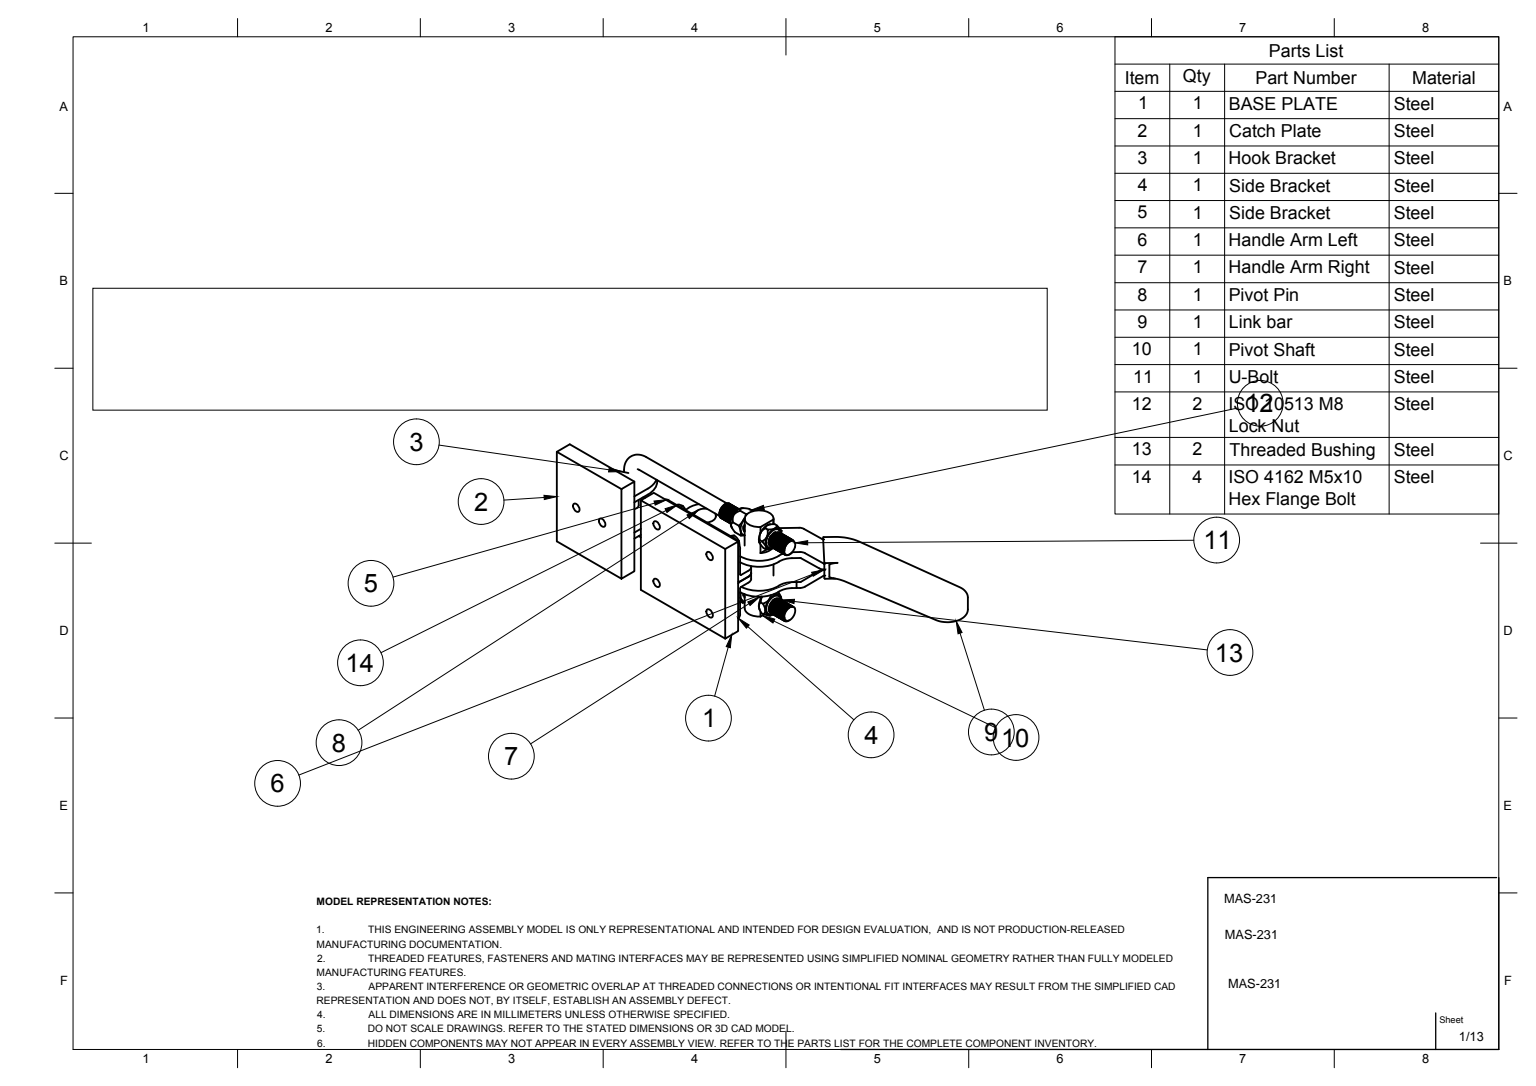
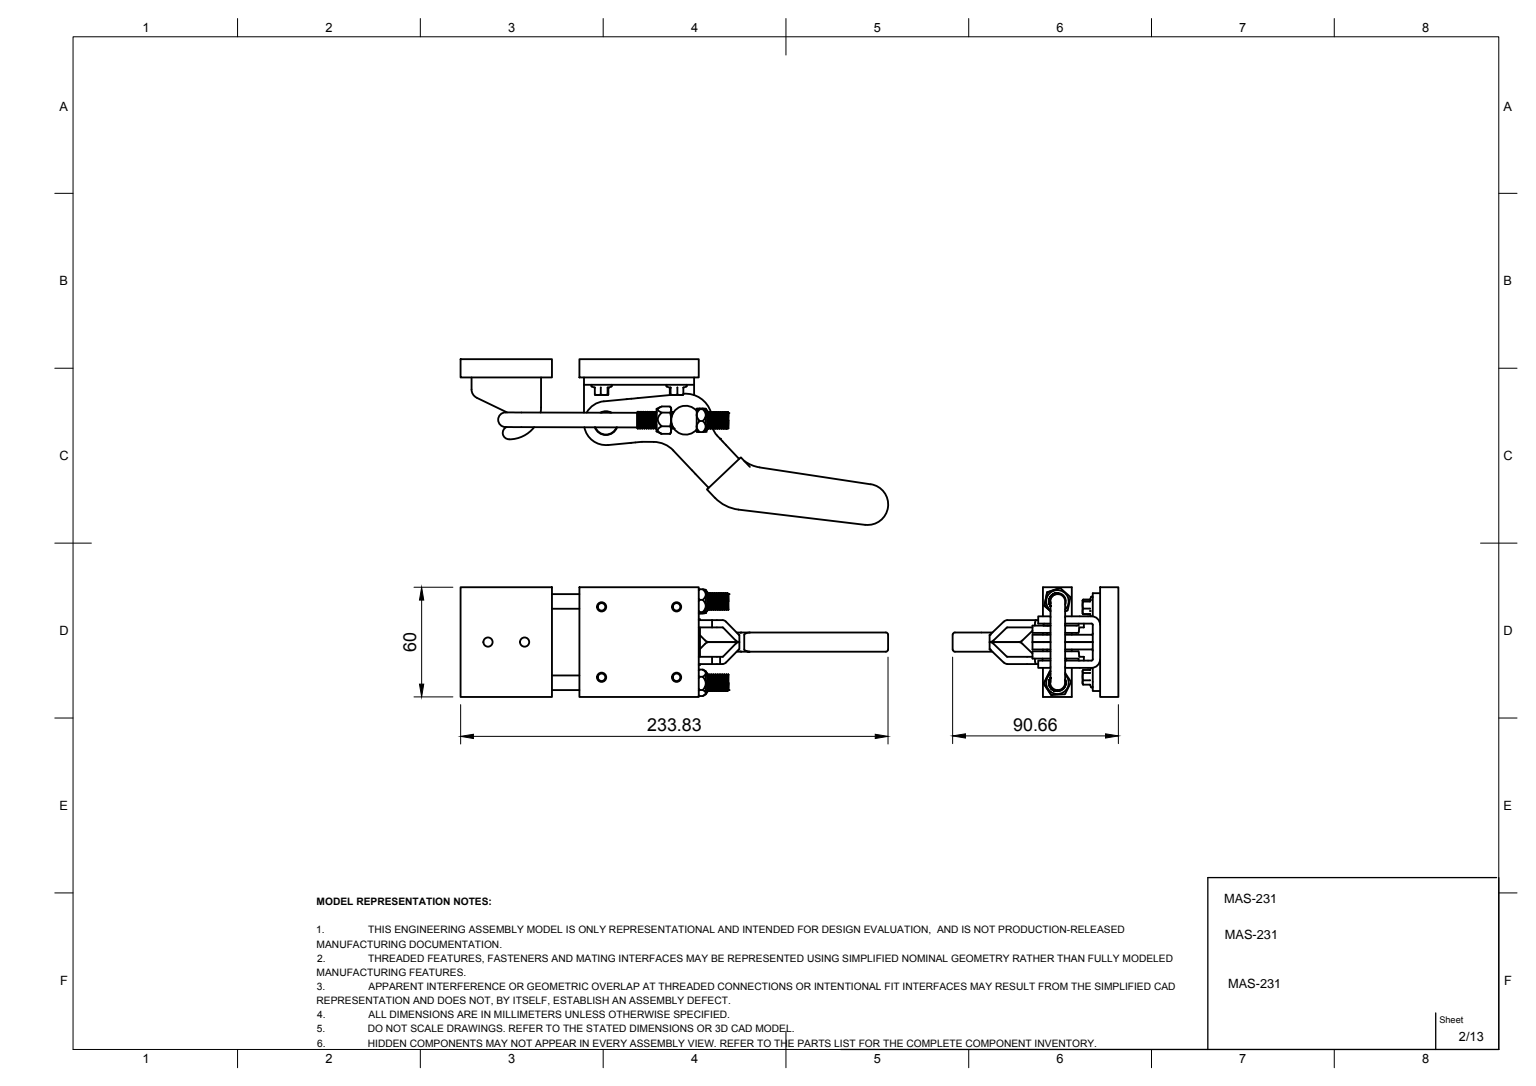
ISO-10303-21;
HEADER;
FILE_DESCRIPTION (('STEP AP214'),
    '1' );
FILE_NAME ( 'MAS-231', '2026-10-04T02:08:54', ( '' ), ( '' ), 'STEP AP214', 'Unspecified', '' );
FILE_SCHEMA (( 'AUTOMOTIVE_DESIGN' ));
ENDSEC;
DATA;
#1 = ORIENTED_EDGE ( 'NONE', *, *, #31259, .T. ) ;
#2 = VERTEX_POINT ( 'NONE', #9971 ) ;
#3 = CARTESIAN_POINT ( 'NONE',  ( -0.7646288533564489232, -0.1113553986120547346, 1.136811023622047223 ) ) ;
#4 = CARTESIAN_POINT ( 'NONE',  ( 0.07405724077823318263, -0.4114173227808823330, -0.1787899950787401604 ) ) ;
#5 = CARTESIAN_POINT ( 'NONE',  ( -1.094772975963752103E-17, -0.9552165353793071745, -0.1787899950787401882 ) ) ;
#6 = CONICAL_SURFACE ( 'NONE', #32970, 0.2471922904502826812, 0.5235987755982992597 ) ;
#7 = CARTESIAN_POINT ( 'NONE',  ( -0.2471922332845153669, -0.07944658092495102131, -0.07441910580874835923 ) ) ;
#8 = FACE_OUTER_BOUND ( 'NONE', #9994, .T. ) ;
#9 = CARTESIAN_POINT ( 'NONE',  ( 0.8019270111902717657, 0.1787899950787401604, 1.727362204670645385 ) ) ;
#10 = CARTESIAN_POINT ( 'NONE',  ( 0.7495606340400177148, 0.1264236179284866091, 0.3518700786863940833 ) ) ;
#11 = CARTESIAN_POINT ( 'NONE',  ( 0.7185039370078746268, -0.06523048226347956391, 0.3075787401574804347 ) ) ;
#12 = CARTESIAN_POINT ( 'NONE',  ( -0.07444174185955065859, -0.2446304237562738071, -0.1797182628040039087 ) ) ;
#13 = CARTESIAN_POINT ( 'NONE',  ( -1.094772975963752103E-17, -0.1049468028749080684, -0.1787899950787401882 ) ) ;
#14 = CARTESIAN_POINT ( 'NONE',  ( -1.094772975963752103E-17, -0.2465551180564728440, -0.1787899950787401882 ) ) ;
#15 = CARTESIAN_POINT ( 'NONE',  ( 0.1787899950787401604, -0.1013779527021420185, -0.07405724077823318263 ) ) ;
#16 = CARTESIAN_POINT ( 'NONE',  ( 0.2471913174570561644, -0.07307272215611475275, -0.08638584879597815958 ) ) ;
#17 = CARTESIAN_POINT ( 'NONE',  ( 0.8019270111902717657, -0.1787899950787401604, 0.6791338582139527791 ) ) ;
#18 = AXIS2_PLACEMENT_3D ( 'NONE', #45673, #23902, #16014 ) ;
#19 = DIRECTION ( 'NONE',  ( 0.000000000000000000, 0.000000000000000000, -1.000000000000000000 ) ) ;
#20 = DIRECTION ( 'NONE',  ( 0.000000000000000000, 0.000000000000000000, 1.000000000000000000 ) ) ;
#21 = CARTESIAN_POINT ( 'NONE',  ( 0.1264236179284866091, -0.4581692912848189247, 0.1264236179284866091 ) ) ;
#22 = EDGE_CURVE ( 'NONE', #36685, #42555, #8791, .T. ) ;
#23 = CARTESIAN_POINT ( 'NONE',  ( -0.8759842519685039353, 0.1574803149606299191, 1.309055118002708573 ) ) ;
#24 = CARTESIAN_POINT ( 'NONE',  ( 0.6971942568897637749, 2.189545951927499583E-17, 1.739665354276945131 ) ) ;
#26 = DIRECTION ( 'NONE',  ( 0.000000000000000000, 0.000000000000000000, -1.000000000000000000 ) ) ;
#25 = CARTESIAN_POINT ( 'NONE',  ( -0.1632645169450111788, -0.09126532511120305502, 0.1911722030494052427 ) ) ;
#27 = CARTESIAN_POINT ( 'NONE',  ( 0.8759842519685039353, 0.1787899950787401882, 0.5044291338045039375 ) ) ;
#28 = CARTESIAN_POINT ( 'NONE',  ( 0.000000000000000000, 0.09842519685039370636, 0.000000000000000000 ) ) ;
#29 = CARTESIAN_POINT ( 'NONE',  ( 0.1527640389977631963, -0.1337207259432456607, 0.04397945982240732826 ) ) ;
#31 = CARTESIAN_POINT ( 'NONE',  ( 0.1787899950787401604, -0.3425196849856064762, 0.07405724077823318263 ) ) ;
#30 = CARTESIAN_POINT ( 'NONE',  ( -0.06523048226347956391, -0.9306102361129453548, -0.1574803149606300301 ) ) ;
#33 = CARTESIAN_POINT ( 'NONE',  ( 0.1619907858920772714, 0.1553500912766716535, 0.01195870310704324514 ) ) ;
#32 = CARTESIAN_POINT ( 'NONE',  ( -0.8759842519685039353, 0.1787899950787401882, 0.4699803149068661479 ) ) ;
#34 = CARTESIAN_POINT ( 'NONE',  ( -0.07405724077823318263, -1.016732283410803905, 0.1787899950787401604 ) ) ;
#35 = FACE_OUTER_BOUND ( 'NONE', #16706, .T. ) ;
#36 = ADVANCED_FACE ( 'NONE', ( #44420 ), #33931, .T. ) ;
#37 = CARTESIAN_POINT ( 'NONE',  ( 0.1602931993194442739, 0.07955613945526338049, -0.1377952755905511861 ) ) ;
#38 = CARTESIAN_POINT ( 'NONE',  ( -0.8759842519685039353, -0.1787899950787401882, 1.587106299158834721 ) ) ;
#39 = VERTEX_POINT ( 'NONE', #1053 ) ;
#40 = CARTESIAN_POINT ( 'NONE',  ( -0.6971942568897648851, 0.07405724077823318263, 1.186023621993481658 ) ) ;
#41 = CYLINDRICAL_SURFACE ( 'NONE', #813, 0.1574803149606299191 ) ;
#42 = CARTESIAN_POINT ( 'NONE',  ( 0.6971942568897648851, -0.07405724077823297447, 1.112204724355684959 ) ) ;
#43 = CARTESIAN_POINT ( 'NONE',  ( 0.1574803149606299191, -1.139763779420031486, -1.928577636452523993E-17 ) ) ;
#44 = CARTESIAN_POINT ( 'NONE',  ( 0.6971942568897637749, 2.189545951927499583E-17, 1.813484251914740053 ) ) ;
#45 = CARTESIAN_POINT ( 'NONE',  ( -1.033464566929133799, 0.000000000000000000, 0.5610236220472440971 ) ) ;
#46 = CARTESIAN_POINT ( 'NONE',  ( -0.8019270111902717657, -0.1787899950787401604, 0.9940944881352130613 ) ) ;
#47 = EDGE_CURVE ( 'NONE', #46518, #3252, #13426, .T. ) ;
#48 = CARTESIAN_POINT ( 'NONE',  ( 0.1588779435336318824, 0.09971251034084034626, -0.1082054717952101869 ) ) ;
#49 = DIRECTION ( 'NONE',  ( 1.822029033848725028E-16, 0.000000000000000000, 1.000000000000000000 ) ) ;
#50 = CARTESIAN_POINT ( 'NONE',  ( 1.002407869896990045, 0.1264236179284866091, 0.3469488188438744070 ) ) ;
#51 = CARTESIAN_POINT ( 'NONE',  ( -0.6971942568897637749, 2.189545951927499583E-17, 0.2780511810485988278 ) ) ;
#52 = CARTESIAN_POINT ( 'NONE',  ( 0.7646288533564489232, -0.1113553986120547346, 1.678149606191684962 ) ) ;
#53 = ORIENTED_EDGE ( 'NONE', *, *, #45978, .F. ) ;
#54 = VECTOR ( 'NONE', #41568, 39.37007874015748143 ) ;
#55 = CARTESIAN_POINT ( 'NONE',  ( 0.1787899950787401604, 0.01181102367581077228, 0.07405724077823318263 ) ) ;
#56 = CARTESIAN_POINT ( 'NONE',  ( 0.7495606340400177148, 0.1264236179284866091, 0.7898622046706456068 ) ) ;
#57 = CARTESIAN_POINT ( 'NONE',  ( 0.8759842519685039353, -0.1787899950787401882, 1.040846456639149764 ) ) ;
#58 = CARTESIAN_POINT ( 'NONE',  ( -0.9500414927467377701, -0.1787899950787401604, 1.825787401521040243 ) ) ;
#59 = ORIENTED_EDGE ( 'NONE', *, *, #22403, .F. ) ;
#60 = VECTOR ( 'NONE', #5427, 39.37007874015748143 ) ;
#61 = AXIS2_PLACEMENT_3D ( 'NONE', #5298, #38366, #19916 ) ;
#62 = ( BOUNDED_CURVE ( )  B_SPLINE_CURVE ( 2, ( #7459, #22081, #47251, #3868, #22310, #18713, #36940, #14196, #13878 ),
 .UNSPECIFIED., .F., .F. ) 
 B_SPLINE_CURVE_WITH_KNOTS ( ( 3, 2, 2, 2, 3 ),
 ( 0.05000000000000000278, 0.05249999999999999806, 0.05500000000000000028, 0.05750000000000000250, 0.05999999999999999778 ),
 .UNSPECIFIED. ) 
 CURVE ( )  GEOMETRIC_REPRESENTATION_ITEM ( )  RATIONAL_B_SPLINE_CURVE ( ( 1.000000000000000000, 0.9238795325112869605, 1.000000000000000000, 0.9238795325112869605, 1.000000000000000000, 0.9238795325112869605, 1.000000000000000000, 0.9238795325112869605, 1.000000000000000000 ) ) 
 REPRESENTATION_ITEM ( '' )  ) ;
#63 = DIRECTION ( 'NONE',  ( 1.822029033848725028E-16, 0.000000000000000000, 1.000000000000000000 ) ) ;
#64 = CARTESIAN_POINT ( 'NONE',  ( 0.1264236179284866091, -1.340183023347348623, 0.1264236179284866091 ) ) ;
#65 = VERTEX_POINT ( 'NONE', #33456 ) ;
#66 = CARTESIAN_POINT ( 'NONE',  ( 0.1264236179284866091, -0.3006889763241893943, 0.1264236179284866091 ) ) ;
#67 = ORIENTED_EDGE ( 'NONE', *, *, #18348, .F. ) ;
#68 = CARTESIAN_POINT ( 'NONE',  ( 1.002407869896990045, 0.1264236179284866091, 1.208169291284818980 ) ) ;
#69 = LINE ( 'NONE', #40323, #2616 ) ;
#70 = EDGE_CURVE ( 'NONE', #32405, #30831, #8652, .T. ) ;
#71 = CARTESIAN_POINT ( 'NONE',  ( -0.7646288533564489232, 0.1113553986120547346, 0.9990157479239685223 ) ) ;
#72 = CARTESIAN_POINT ( 'NONE',  ( 0.8759842519685039353, 0.1787899950787401882, 1.488681102308440751 ) ) ;
#73 = CARTESIAN_POINT ( 'NONE',  ( 0.7646288533564489232, 0.1113553986120547346, 1.914370078740157632 ) ) ;
#74 = CARTESIAN_POINT ( 'NONE',  ( -0.1264236179284866091, -1.693405511757259951, 0.1264236179284866091 ) ) ;
#75 = CIRCLE ( 'NONE', #20007, 0.1787899950787401049 ) ;
#76 = CARTESIAN_POINT ( 'NONE',  ( -0.6971942568897637749, 2.189545951927499583E-17, 0.4404527558517480901 ) ) ;
#77 = CARTESIAN_POINT ( 'NONE',  ( -0.1540809957184832990, -0.09842519685039370636, 0.06850209239233011338 ) ) ;
#79 = CARTESIAN_POINT ( 'NONE',  ( -0.7240989362502219251, -0.07281704346119359517, 1.984672674023657102 ) ) ;
#78 = CARTESIAN_POINT ( 'NONE',  ( 0.1797182628040039087, -1.440496565488557978, 0.07444174185955046430 ) ) ;
#80 = DIRECTION ( 'NONE',  ( 0.000000000000000000, 0.000000000000000000, 1.000000000000000000 ) ) ;
#81 = CARTESIAN_POINT ( 'NONE',  ( 1.054774247047244540, 0.07405724077823318263, 1.249999999946235896 ) ) ;
#82 = CARTESIAN_POINT ( 'NONE',  ( 1.054774247047244540, -0.07405724077823318263, 1.712598425143087466 ) ) ;
#83 = AXIS2_PLACEMENT_3D ( 'NONE', #20865, #3610, #25184 ) ;
#84 = CARTESIAN_POINT ( 'NONE',  ( 0.7646288533564489232, 0.1113553986120547346, 1.510826771546015523 ) ) ;
#85 = CARTESIAN_POINT ( 'NONE',  ( 0.1574803149606300023, 0.3648440108500937140, -3.619166627704267558 ) ) ;
#86 = CIRCLE ( 'NONE', #1647, 0.09842519685039370636 ) ;
#87 = CARTESIAN_POINT ( 'NONE',  ( -0.1574803149606299191, 0.7443365962042343131, -3.964450923140766303 ) ) ;
#89 = CARTESIAN_POINT ( 'NONE',  ( 3.284318927891251994E-17, 0.1225393701325037388, 0.1787899950787401882 ) ) ;
#88 = CARTESIAN_POINT ( 'NONE',  ( -0.1574803149606297803, -0.7632874014672766938, 0.06523048226347956391 ) ) ;
#90 = CARTESIAN_POINT ( 'NONE',  ( 0.7646288533564489232, 0.1113553986120547346, 0.7627952754830236159 ) ) ;
#91 = CARTESIAN_POINT ( 'NONE',  ( 0.7013496418058506876, 0.02137559083948704225, 0.03937007727944009938 ) ) ;
#92 = EDGE_CURVE ( 'NONE', #27712, #6075, #1837, .T. ) ;
#94 = LINE ( 'NONE', #8474, #24641 ) ;
#93 = CARTESIAN_POINT ( 'NONE',  ( 0.8019270111902716547, -0.1787899950787401604, 1.269685039316314601 ) ) ;
#95 = DIRECTION ( 'NONE',  ( 1.000000000000000000, -0.000000000000000000, -1.144917494144692682E-16 ) ) ;
#96 = CARTESIAN_POINT ( 'NONE',  ( 0.3108999017613323090, 0.9251089822459528378, -1.060267534067256046 ) ) ;
#97 = CARTESIAN_POINT ( 'NONE',  ( 0.9412147342319837628, -0.1574803149606297803, 0.5831692912310553201 ) ) ;
#98 = ORIENTED_EDGE ( 'NONE', *, *, #40284, .T. ) ;
#99 = DIRECTION ( 'NONE',  ( 1.822029033848725028E-16, 0.000000000000000000, 1.000000000000000000 ) ) ;
#100 = CARTESIAN_POINT ( 'NONE',  ( 0.9656857656210602325, 0.1425117190157106917, 0.03937007042889534292 ) ) ;
#101 = CARTESIAN_POINT ( 'NONE',  ( -1.033464566929134687, -0.06523048226347956391, 0.3124999998924728462 ) ) ;
#102 = CARTESIAN_POINT ( 'NONE',  ( -0.7185039370078746268, -0.06523048226347956391, 0.4158464565853862704 ) ) ;
#103 = CARTESIAN_POINT ( 'NONE',  ( 0.005425426062181716927, 0.05318853600681028998, 0.1377950977353498141 ) ) ;
#104 = CARTESIAN_POINT ( 'NONE',  ( 0.9500414927467378812, -0.1787899950787401604, 1.432086614119464141 ) ) ;
#105 = CARTESIAN_POINT ( 'NONE',  ( -0.8107537697050253289, 0.1574803149606300301, 1.163877952755904666 ) ) ;
#106 = EDGE_CURVE ( 'NONE', #13083, #24265, #27060, .T. ) ;
#108 = CARTESIAN_POINT ( 'NONE',  ( 0.7185039370078739607, 1.928577636452523993E-17, 1.683070866141732402 ) ) ;
#107 = CARTESIAN_POINT ( 'NONE',  ( -1.033464566929133355, 0.06523048226348168721, 1.626476377952755570 ) ) ;
#109 = CARTESIAN_POINT ( 'NONE',  ( 0.1264236179284866091, -0.1038385826234017734, 0.1264236179284866091 ) ) ;
#110 = VERTEX_POINT ( 'NONE', #36790 ) ;
#111 = CARTESIAN_POINT ( 'NONE',  ( 0.7185039370078746268, -0.06523048226347956391, 0.6520669290263312323 ) ) ;
#112 = DIRECTION ( 'NONE',  ( 1.822029033848725028E-16, 0.000000000000000000, 1.000000000000000000 ) ) ;
#113 = CARTESIAN_POINT ( 'NONE',  ( -0.6195511811023656223, 0.6102362204724407491, 1.186023622047243986 ) ) ;
#114 = CARTESIAN_POINT ( 'NONE',  ( 0.6971942568897626646, 0.07405724077823318263, 0.5954724408911187261 ) ) ;
#115 = ORIENTED_EDGE ( 'NONE', *, *, #9426, .T. ) ;
#116 = CARTESIAN_POINT ( 'NONE',  ( -0.8019270111902716547, 0.1787899950787401604, 1.451771653489543290 ) ) ;
#117 = CARTESIAN_POINT ( 'NONE',  ( 0.1113553986120547346, 0.1250000001075269596, -0.1113553986120547346 ) ) ;
#118 = CARTESIAN_POINT ( 'NONE',  ( -1.002407869896990045, -0.1264236179284866091, 1.163877952702141672 ) ) ;
#119 = EDGE_LOOP ( 'NONE', ( #9384, #25327, #26730, #11644 ) ) ;
#120 = CARTESIAN_POINT ( 'NONE',  ( -0.2559055118110235560, -0.04581480775486102691, -0.03611822492271276469 ) ) ;
#121 = CARTESIAN_POINT ( 'NONE',  ( -0.8019270111902717657, 0.1787899950787401604, 0.8661417322297003674 ) ) ;
#122 = AXIS2_PLACEMENT_3D ( 'NONE', #43059, #39470, #7131 ) ;
#123 = CARTESIAN_POINT ( 'NONE',  ( 0.8107537697050254399, -0.1574803149606297803, 0.6668307086614162493 ) ) ;
#124 = DIRECTION ( 'NONE',  ( -1.000000000000000000, -6.679788269418529283E-17, 0.000000000000000000 ) ) ;
#125 = CARTESIAN_POINT ( 'NONE',  ( -0.1787899950787401604, -0.7668562516938051132, -0.07405724077823318263 ) ) ;
#126 = EDGE_LOOP ( 'NONE', ( #4193, #39037, #39203, #47364, #17831, #33692, #29299, #33986, #26594 ) ) ;
#127 = ORIENTED_EDGE ( 'NONE', *, *, #14895, .F. ) ;
#128 = VECTOR ( 'NONE', #18538, 39.37007874015748143 ) ;
#129 = CARTESIAN_POINT ( 'NONE',  ( 0.7185039370078739607, 1.928577636452523993E-17, 0.9645669290263307882 ) ) ;
#130 = ADVANCED_FACE ( 'NONE', ( #15231 ), #18799, .T. ) ;
#131 = CARTESIAN_POINT ( 'NONE',  ( -0.9500414927467378812, -0.1787899950787401604, 0.8021653542769460188 ) ) ;
#132 = FACE_OUTER_BOUND ( 'NONE', #21236, .T. ) ;
#133 = ORIENTED_EDGE ( 'NONE', *, *, #14771, .F. ) ;
#134 = CARTESIAN_POINT ( 'NONE',  ( -0.8019270111902716547, -0.1787899950787401604, 1.865157480261198097 ) ) ;
#135 = CARTESIAN_POINT ( 'NONE',  ( 0.07405724077823318263, -0.4901574802611972093, -0.1787899950787401604 ) ) ;
#136 = DIRECTION ( 'NONE',  ( -1.000000000000000000, 0.000000000000000000, 0.000000000000000000 ) ) ;
#137 = CARTESIAN_POINT ( 'NONE',  ( 0.7185039370078746268, -0.06523048226347956391, 0.6225393700787401619 ) ) ;
#138 = CARTESIAN_POINT ( 'NONE',  ( 3.301370929368692659E-17, -0.8573272741499744498, 0.1797182628040039365 ) ) ;
#139 = FACE_OUTER_BOUND ( 'NONE', #32124, .T. ) ;
#140 = CARTESIAN_POINT ( 'NONE',  ( -0.8759842519685039353, 0.1574803149606299191, 1.466535432963338437 ) ) ;
#141 = EDGE_CURVE ( 'NONE', #480, #43073, #20129, .T. ) ;
#142 = CARTESIAN_POINT ( 'NONE',  ( 0.9500414927467378812, -0.1787899950787401604, 0.7283464566391493200 ) ) ;
#143 = DIRECTION ( 'NONE',  ( -0.000000000000000000, -0.000000000000000000, 1.000000000000000000 ) ) ;
#144 = CARTESIAN_POINT ( 'NONE',  ( 0.9873396505805591694, -0.1113553986120547346, 1.343503937007874072 ) ) ;
#145 = DIRECTION ( 'NONE',  ( 0.000000000000000000, -0.6156614753256641759, -0.7880107536067173513 ) ) ;
#147 = FACE_OUTER_BOUND ( 'NONE', #21139, .T. ) ;
#146 = CARTESIAN_POINT ( 'NONE',  ( 0.9356431618536311667, -0.1660064224309732994, 1.989266148032244885 ) ) ;
#148 = DIRECTION ( 'NONE',  ( -1.000000000000000000, 0.000000000000000000, 0.000000000000000000 ) ) ;
#149 = CARTESIAN_POINT ( 'NONE',  ( 0.1113553986120547346, -0.6328740156405040507, 0.1113553986120547346 ) ) ;
#150 = ORIENTED_EDGE ( 'NONE', *, *, #2837, .F. ) ;
#151 = CIRCLE ( 'NONE', #10128, 0.1787899950787401049 ) ;
#152 = EDGE_CURVE ( 'NONE', #35410, #47206, #15470, .T. ) ;
#154 = DIRECTION ( 'NONE',  ( -1.000000000000000000, -1.802250327717385127E-14, 1.473544972410982106E-14 ) ) ;
#153 = CARTESIAN_POINT ( 'NONE',  ( 0.7495606340400177148, -0.1264236179284866091, 0.8341535432533228045 ) ) ;
#155 = CARTESIAN_POINT ( 'NONE',  ( 0.1787899950787401882, -0.7288385826234015097, -2.189545951927503898E-17 ) ) ;
#156 = DIRECTION ( 'NONE',  ( 0.000000000000000000, 0.6156614753256598460, 0.7880107536067207930 ) ) ;
#157 = VERTEX_POINT ( 'NONE', #7543 ) ;
#158 = CARTESIAN_POINT ( 'NONE',  ( -0.7646288533564489232, 0.1113553986120547346, 1.166338582677165281 ) ) ;
#159 = TOROIDAL_SURFACE ( 'NONE', #46862, 0.3814023619577306956, 0.009842519685039369942 ) ;
#160 = DIRECTION ( 'NONE',  ( 0.8191520442889949072, -0.4519843998600416302, 0.3531289150159167556 ) ) ;
#161 = CARTESIAN_POINT ( 'NONE',  ( 0.6971942568897637749, 2.189545951927499583E-17, 0.9867125983714331028 ) ) ;
#162 = EDGE_CURVE ( 'NONE', #28497, #15222, #36387, .T. ) ;
#163 = CARTESIAN_POINT ( 'NONE',  ( 0.000000000000000000, 0.000000000000000000, 1.181102362204724310 ) ) ;
#164 = CARTESIAN_POINT ( 'NONE',  ( 0.1113553986120547346, -1.617125984251968518, -0.1113553986120547346 ) ) ;
#165 = CARTESIAN_POINT ( 'NONE',  ( -0.8107537697050254399, -0.1574803149606297803, 0.5093503937007877180 ) ) ;
#166 = ORIENTED_EDGE ( 'NONE', *, *, #15392, .T. ) ;
#167 = FACE_BOUND ( 'NONE', #12224, .T. ) ;
#168 = CARTESIAN_POINT ( 'NONE',  ( -0.8019270111902717657, 0.1787899950787401604, 0.1131889763241894359 ) ) ;
#169 = ORIENTED_EDGE ( 'NONE', *, *, #21607, .F. ) ;
#170 = CARTESIAN_POINT ( 'NONE',  ( -0.9873396505805591694, -0.1113553986120547346, 0.7135826771653542844 ) ) ;
#171 = CARTESIAN_POINT ( 'NONE',  ( 0.07405724077823318263, -1.435039370024976391, -0.1787899950787401604 ) ) ;
#172 = CARTESIAN_POINT ( 'NONE',  ( -0.9873396505805591694, -0.1113553986120547346, 1.855314960629921295 ) ) ;
#173 = CARTESIAN_POINT ( 'NONE',  ( -1.002407869896990045, -0.1264236179284866091, 1.631397637741511808 ) ) ;
#174 = CARTESIAN_POINT ( 'NONE',  ( -1.033464566929133799, 0.000000000000000000, 0.1181102361129454797 ) ) ;
#175 = CARTESIAN_POINT ( 'NONE',  ( 0.1619971594100712287, 0.06735705997075436269, 0.1405166210180776309 ) ) ;
#176 = CARTESIAN_POINT ( 'NONE',  ( 0.9500414927467378812, 0.1787899950787401604, 0.02952755900135462311 ) ) ;
#177 = CYLINDRICAL_SURFACE ( 'NONE', #43516, 0.1574803149606299191 ) ;
#178 = CARTESIAN_POINT ( 'NONE',  ( -1.094772975963752103E-17, -0.3411672753158531690, -0.1787899950787401882 ) ) ;
#179 = CARTESIAN_POINT ( 'NONE',  ( 0.8759842519685039353, 0.000000000000000000, 4.498031496062992574 ) ) ;
#180 = DIRECTION ( 'NONE',  ( 1.822029033848725028E-16, 0.000000000000000000, 1.000000000000000000 ) ) ;
#181 = CARTESIAN_POINT ( 'NONE',  ( -0.9500414927467378812, 0.1787899950787401604, 0.3051181101824569919 ) ) ;
#182 = CIRCLE ( 'NONE', #27018, 0.1574803149606299191 ) ;
#183 = VERTEX_POINT ( 'NONE', #42256 ) ;
#184 = ORIENTED_EDGE ( 'NONE', *, *, #3239, .T. ) ;
#185 = CARTESIAN_POINT ( 'NONE',  ( -0.8019270111902716547, -0.1787899950787401604, 1.313976377898992132 ) ) ;
#186 = ORIENTED_EDGE ( 'NONE', *, *, #26981, .F. ) ;
#187 = ( GEOMETRIC_REPRESENTATION_CONTEXT ( 3 ) GLOBAL_UNCERTAINTY_ASSIGNED_CONTEXT ( ( #19281 ) ) GLOBAL_UNIT_ASSIGNED_CONTEXT ( ( #14903, #26165, #18708 ) ) REPRESENTATION_CONTEXT ( 'NONE', 'WORKASPACE' ) ) ;
#188 = VECTOR ( 'NONE', #38666, 39.37007874015748143 ) ;
#189 = ADVANCED_FACE ( 'NONE', ( #38682 ), #13369, .T. ) ;
#190 = CARTESIAN_POINT ( 'NONE',  ( -0.1787899950787401604, -1.262795275536788386, 0.07405724077823318263 ) ) ;
#191 = CARTESIAN_POINT ( 'NONE',  ( 0.1264236179284866091, -1.403051181048598384, 0.1264236179284866091 ) ) ;
#192 = CARTESIAN_POINT ( 'NONE',  ( 0.000000000000000000, 0.000000000000000000, 0.000000000000000000 ) ) ;
#193 = ADVANCED_FACE ( 'NONE', ( #1523 ), #30571, .F. ) ;
#194 = CARTESIAN_POINT ( 'NONE',  ( 0.8759842519685039353, 0.1574803149606299191, 0.3346456692913385988 ) ) ;
#195 = CARTESIAN_POINT ( 'NONE',  ( -1.181102362204724310, 0.000000000000000000, 0.9842519685039370358 ) ) ;
#196 = CARTESIAN_POINT ( 'NONE',  ( -0.8107537697050253289, -0.1574803149606297803, 1.011318897530268712 ) ) ;
#197 = VECTOR ( 'NONE', #24397, 39.37007874015748143 ) ;
#198 = ADVANCED_FACE ( 'NONE', ( #20458 ), #16639, .T. ) ;
#199 = CARTESIAN_POINT ( 'NONE',  ( 0.6971942568897637749, 2.189545951927499583E-17, 0.4010826771115905687 ) ) ;
#200 = CARTESIAN_POINT ( 'NONE',  ( 0.1113553986120547346, -0.3277559055118110520, 0.1113553986120547346 ) ) ;
#201 = CARTESIAN_POINT ( 'NONE',  ( 0.7185039370078746268, 0.06523048226347956391, 1.906988188868851797 ) ) ;
#202 = EDGE_LOOP ( 'NONE', ( #15956, #3484, #38224, #16323 ) ) ;
#203 = DIRECTION ( 'NONE',  ( 0.000000000000000000, 0.000000000000000000, -1.000000000000000000 ) ) ;
#204 = CARTESIAN_POINT ( 'NONE',  ( 0.7185039370078746268, -0.06523048226347956391, 0.9374999999999991118 ) ) ;
#205 = CARTESIAN_POINT ( 'NONE',  ( -1.033464566929133799, 0.000000000000000000, 0.6692913384751496553 ) ) ;
#206 = CARTESIAN_POINT ( 'NONE',  ( -0.1113553986120547346, -0.4950787400499527813, -0.1113553986120547346 ) ) ;
#208 = CARTESIAN_POINT ( 'NONE',  ( 0.7185039370078746268, -0.06523048226347956391, 0.7406496062992133922 ) ) ;
#207 = CARTESIAN_POINT ( 'NONE',  ( 0.8759842519685039353, 0.000000000000000000, 4.498031496062992574 ) ) ;
#209 = CARTESIAN_POINT ( 'NONE',  ( -0.7185039370078739607, 1.928577636452523993E-17, 0.7677165353255432922 ) ) ;
#210 = EDGE_LOOP ( 'NONE', ( #1234, #31218, #6999, #28687 ) ) ;
#211 = CARTESIAN_POINT ( 'NONE',  ( -0.1574803149606297803, 0.1028543308161884995, 0.06523048226347956391 ) ) ;
#212 = CARTESIAN_POINT ( 'NONE',  ( 0.4330708661417322913, 0.08090551181102362266, 0.000000000000000000 ) ) ;
#213 = CARTESIAN_POINT ( 'NONE',  ( 0.07405724077823318263, -1.508858267662772867, -0.1787899950787401604 ) ) ;
#214 = CARTESIAN_POINT ( 'NONE',  ( -0.1574803149606297803, -1.511318897530268712, 0.06523048226347956391 ) ) ;
#215 = CARTESIAN_POINT ( 'NONE',  ( 0.1264236179284866091, -0.7780511810485984947, 0.1264236179284866091 ) ) ;
#216 = CARTESIAN_POINT ( 'NONE',  ( -0.06523048226347956391, -1.097933070866141225, -0.1574803149606300301 ) ) ;
#217 = CARTESIAN_POINT ( 'NONE',  ( 1.033464566929134687, -0.06523048226347956391, 0.9424212597349932441 ) ) ;
#218 = CARTESIAN_POINT ( 'NONE',  ( 0.7185039370078746268, 0.06523048226347956391, 0.5388779527559055538 ) ) ;
#219 = VECTOR ( 'NONE', #41742, 39.37007874015748143 ) ;
#220 = EDGE_CURVE ( 'NONE', #8537, #45765, #3616, .T. ) ;
#221 = ORIENTED_EDGE ( 'NONE', *, *, #44499, .F. ) ;
#222 = ORIENTED_EDGE ( 'NONE', *, *, #18590, .F. ) ;
#223 = EDGE_LOOP ( 'NONE', ( #32593, #34812, #29678, #45510 ) ) ;
#224 = CARTESIAN_POINT ( 'NONE',  ( -1.054774247047244096, 0.000000000000000000, 1.562499999946236118 ) ) ;
#225 = CARTESIAN_POINT ( 'NONE',  ( 0.6971942568897648851, 0.07405724077823318263, 1.697834645615527771 ) ) ;
#226 = CARTESIAN_POINT ( 'NONE',  ( 0.1574803149606300301, -1.339074803042078932, 0.06523048226347956391 ) ) ;
#227 = CARTESIAN_POINT ( 'NONE',  ( -0.9500414927467378812, -0.1787899950787401604, 0.7283464566391493200 ) ) ;
#228 = AXIS2_PLACEMENT_3D ( 'NONE', #14600, #36183, #18649 ) ;
#230 = FACE_OUTER_BOUND ( 'NONE', #13816, .T. ) ;
#229 = AXIS2_PLACEMENT_3D ( 'NONE', #33997, #1125, #15784 ) ;
#231 = CARTESIAN_POINT ( 'NONE',  ( 1.054774247047244096, 0.000000000000000000, 0.3420275590013546751 ) ) ;
#232 = CARTESIAN_POINT ( 'NONE',  ( 0.3161444924769701292, 2.177585298233984279, -3.731703755406948986 ) ) ;
#233 = CARTESIAN_POINT ( 'NONE',  ( -0.6971942568897648851, 0.07405724077823318263, 1.220472440891118504 ) ) ;
#234 = CARTESIAN_POINT ( 'NONE',  ( -0.7495606340400177148, -0.1264236179284866091, 0.6373031495525354195 ) ) ;
#235 = DIRECTION ( 'NONE',  ( 1.000000000000000000, 0.000000000000000000, -1.822029033848725275E-16 ) ) ;
#236 = ( BOUNDED_CURVE ( )  B_SPLINE_CURVE ( 2, ( #18764, #29842, #25754, #33895, #32949, #1015, #4363, #41246, #25970 ),
 .UNSPECIFIED., .F., .T. ) 
 B_SPLINE_CURVE_WITH_KNOTS ( ( 3, 2, 2, 2, 3 ),
 ( 0.4000000000000000222, 0.4025000000000000244, 0.4050000000000000266, 0.4074999999999999734, 0.4099999999999999756 ),
 .UNSPECIFIED. ) 
 CURVE ( )  GEOMETRIC_REPRESENTATION_ITEM ( )  RATIONAL_B_SPLINE_CURVE ( ( 1.000000000000000000, 0.9238795325112869605, 1.000000000000000000, 0.9238795325112869605, 1.000000000000000000, 0.9238795325112869605, 1.000000000000000000, 0.9238795325112849621, 1.000000000000000000 ) ) 
 REPRESENTATION_ITEM ( '' )  ) ;
#237 = AXIS2_PLACEMENT_3D ( 'NONE', #26256, #7319, #29176 ) ;
#238 = DIRECTION ( 'NONE',  ( -1.000000000000000000, 0.000000000000000000, 0.000000000000000000 ) ) ;
#239 = CARTESIAN_POINT ( 'NONE',  ( -0.8759842519685039353, 0.1787899950787401882, 1.572342519631275692 ) ) ;
#240 = CARTESIAN_POINT ( 'NONE',  ( -0.7185039370078739607, 1.928577636452523993E-17, 1.948818897530267602 ) ) ;
#241 = ORIENTED_EDGE ( 'NONE', *, *, #39973, .T. ) ;
#243 = ( BOUNDED_CURVE ( )  B_SPLINE_CURVE ( 2, ( #38368, #35271, #35028, #17505, #31910, #27861, #39299, #28309, #42180 ),
 .UNSPECIFIED., .F., .F. ) 
 B_SPLINE_CURVE_WITH_KNOTS ( ( 3, 2, 2, 2, 3 ),
 ( 0.4500000000000000111, 0.4525000000000000133, 0.4550000000000000155, 0.4575000000000000178, 0.4600000000000000200 ),
 .UNSPECIFIED. ) 
 CURVE ( )  GEOMETRIC_REPRESENTATION_ITEM ( )  RATIONAL_B_SPLINE_CURVE ( ( 1.000000000000000000, 0.9238795325112869605, 1.000000000000000000, 0.9238795325112869605, 1.000000000000000000, 0.9238795325112869605, 1.000000000000000000, 0.9238795325112869605, 1.000000000000000000 ) ) 
 REPRESENTATION_ITEM ( '' )  ) ;
#242 = CARTESIAN_POINT ( 'NONE',  ( -0.9412147342319837628, -0.1574803149606297803, 1.656003937007873406 ) ) ;
#244 = DIRECTION ( 'NONE',  ( 0.000000000000000000, 0.000000000000000000, 1.000000000000000000 ) ) ;
#245 = CARTESIAN_POINT ( 'NONE',  ( 0.8019270111902716547, -0.1787899950787401604, 1.471456692859622217 ) ) ;
#246 = CARTESIAN_POINT ( 'NONE',  ( 0.2698848154395015464, -3.032960542342102697E-32, 0.09842519685039370636 ) ) ;
#247 = ORIENTED_EDGE ( 'NONE', *, *, #10180, .F. ) ;
#248 = CARTESIAN_POINT ( 'NONE',  ( -0.3161444924769509779, 1.495705267341512767, -0.3569552279982057819 ) ) ;
#249 = ORIENTED_EDGE ( 'NONE', *, *, #21041, .T. ) ;
#250 = ORIENTED_EDGE ( 'NONE', *, *, #34224, .F. ) ;
#251 = EDGE_CURVE ( 'NONE', #13767, #23712, #510, .T. ) ;
#252 = CARTESIAN_POINT ( 'NONE',  ( -0.4338976377952755703, 0.1574803149606299191, 1.928577636452523993E-17 ) ) ;
#253 = CARTESIAN_POINT ( 'NONE',  ( -0.1787899950787401604, -0.4360236219934807145, 0.07405724077823318263 ) ) ;
#254 = EDGE_CURVE ( 'NONE', #18975, #21109, #11079, .T. ) ;
#255 = CARTESIAN_POINT ( 'NONE',  ( 0.1787899950787401604, -0.8494094487651332459, 0.07405724077823318263 ) ) ;
#256 = CARTESIAN_POINT ( 'NONE',  ( 0.7185039370078739607, 0.000000000000000000, 4.498031496062992574 ) ) ;
#257 = CARTESIAN_POINT ( 'NONE',  ( 0.7495606340400177148, 0.1264236179284866091, 1.729822834591905556 ) ) ;
#258 = CARTESIAN_POINT ( 'NONE',  ( -0.1797182628040039087, -0.2003390851735964984, -0.07444174185955065859 ) ) ;
#259 = EDGE_CURVE ( 'NONE', #25443, #30394, #12521, .T. ) ;
#260 = VECTOR ( 'NONE', #32837, 39.37007874015748143 ) ;
#261 = CARTESIAN_POINT ( 'NONE',  ( 0.1787899950787401604, -0.1172499524812071620, 0.07405724077823318263 ) ) ;
#262 = CARTESIAN_POINT ( 'NONE',  ( -0.1264236179284866091, -0.1186023621509608300, 0.1264236179284866091 ) ) ;
#263 = CARTESIAN_POINT ( 'NONE',  ( 0.2471920270787851259, -0.07566776403336712697, -0.08167830084036972749 ) ) ;
#264 = EDGE_CURVE ( 'NONE', #24192, #11278, #27216, .T. ) ;
#265 = CARTESIAN_POINT ( 'NONE',  ( 1.054774247047244540, -0.07405724077823318263, 0.7283464566391493200 ) ) ;
#266 = CARTESIAN_POINT ( 'NONE',  ( 0.1673228346456693549, 0.05639690512153990726, -0.1570009270184611616 ) ) ;
#267 = VECTOR ( 'NONE', #18707, 39.37007874015748143 ) ;
#268 = CARTESIAN_POINT ( 'NONE',  ( -0.1787899950787401604, -0.4311023621509605386, 0.07405724077823318263 ) ) ;
#269 = LINE ( 'NONE', #3642, #3920 ) ;
#270 = CARTESIAN_POINT ( 'NONE',  ( 0.8019270111902717657, -0.1787899950787401604, 1.786417322780882388 ) ) ;
#271 = CYLINDRICAL_SURFACE ( 'NONE', #38342, 0.1574803149606299191 ) ;
#272 = CARTESIAN_POINT ( 'NONE',  ( 0.6971942568897637749, 2.189545951927499583E-17, 0.5142716534895434011 ) ) ;
#273 = ORIENTED_EDGE ( 'NONE', *, *, #35074, .F. ) ;
#274 = CARTESIAN_POINT ( 'NONE',  ( 1.033464566929134687, -0.06523048226347956391, 0.08612204724409450174 ) ) ;
#276 = CARTESIAN_POINT ( 'NONE',  ( 0.1264236179284866091, -0.2170275590013547307, -0.1264236179284866091 ) ) ;
#275 = CARTESIAN_POINT ( 'NONE',  ( 0.1574803149606299191, -0.9429133857192442125, -1.928577636452523993E-17 ) ) ;
#278 = CARTESIAN_POINT ( 'NONE',  ( 0.1571385178022428053, 0.1097099440836636214, 0.09077329659527381966 ) ) ;
#277 = CARTESIAN_POINT ( 'NONE',  ( -0.8759842519685039353, -0.1787899950787401882, 0.4502952755367874427 ) ) ;
#279 = CARTESIAN_POINT ( 'NONE',  ( 0.1787899950787401604, -1.041338582623402287, -0.07405724077823318263 ) ) ;
#280 = CARTESIAN_POINT ( 'NONE',  ( 0.6971942568897626646, -0.07405724077823297447, 0.2460629920722207375 ) ) ;
#281 = CARTESIAN_POINT ( 'NONE',  ( 0.1640397255812384159, 0.08076041531236369253, -0.1398787134456308257 ) ) ;
#282 = CARTESIAN_POINT ( 'NONE',  ( -0.6971942568897648851, 0.07405724077823318263, 1.535433070812378675 ) ) ;
#283 = ORIENTED_EDGE ( 'NONE', *, *, #46313, .T. ) ;
#284 = CARTESIAN_POINT ( 'NONE',  ( -0.8759842519685039353, 0.1787899950787401882, 1.218011810969858111 ) ) ;
#285 = CARTESIAN_POINT ( 'NONE',  ( -0.8107537697050254399, 0.1574803149606300301, 0.3371062992125987146 ) ) ;
#286 = CARTESIAN_POINT ( 'NONE',  ( 0.9500414927467378812, 0.1787899950787401604, 1.254921259788757348 ) ) ;
#287 = CARTESIAN_POINT ( 'NONE',  ( -0.06523048226347956391, -1.206200787294047228, -0.1574803149606300301 ) ) ;
#288 = CARTESIAN_POINT ( 'NONE',  ( 1.054774247047244096, 0.000000000000000000, 1.951279527505291433 ) ) ;
#289 = CARTESIAN_POINT ( 'NONE',  ( -0.8759842519685039353, 0.1574803149606299191, 0.6496062992125984925 ) ) ;
#290 = CARTESIAN_POINT ( 'NONE',  ( -0.6971942568897648851, -0.07405724077823297447, 1.028543307032851795 ) ) ;
#291 = CARTESIAN_POINT ( 'NONE',  ( -0.7185039370078739607, 1.928577636452523993E-17, 1.604330708661417360 ) ) ;
#292 = CARTESIAN_POINT ( 'NONE',  ( -0.1706040688522822979, -0.1969959271856973060, -0.03730110279448183019 ) ) ;
#293 = CARTESIAN_POINT ( 'NONE',  ( 0.8759842519685039353, -0.1787899950787401882, 0.3715551180564728440 ) ) ;
#294 = CARTESIAN_POINT ( 'NONE',  ( -1.002407869896990045, -0.1264236179284866091, 0.1747047243556852092 ) ) ;
#295 = CARTESIAN_POINT ( 'NONE',  ( 0.7185039370078746268, 0.06523048226347956391, 1.670767716427906002 ) ) ;
#296 = ORIENTED_EDGE ( 'NONE', *, *, #20298, .F. ) ;
#297 = CARTESIAN_POINT ( 'NONE',  ( -0.1787899950787401604, 0.03149606304588949135, -0.07405724077823318263 ) ) ;
#298 = ORIENTED_EDGE ( 'NONE', *, *, #27985, .F. ) ;
#299 = CARTESIAN_POINT ( 'NONE',  ( 1.002407869896990045, 0.1264236179284866091, 0.8981299212060788184 ) ) ;
#300 = CARTESIAN_POINT ( 'NONE',  ( 0.9500414927467377701, -0.1787899950787401604, 1.082677165300567346 ) ) ;
#301 = CARTESIAN_POINT ( 'NONE',  ( -0.8759842519685039353, -0.1787899950787401882, 1.823326771599779406 ) ) ;
#302 = AXIS2_PLACEMENT_3D ( 'NONE', #11967, #8576, #23214 ) ;
#303 = EDGE_LOOP ( 'NONE', ( #910, #27362, #9795, #24309 ) ) ;
#304 = CARTESIAN_POINT ( 'NONE',  ( 1.054774247047244540, 0.07405724077823318263, 1.953740157426552715 ) ) ;
#305 = CARTESIAN_POINT ( 'NONE',  ( 0.1574803149606299191, 0.5360961046428496246, -0.7563373642699310340 ) ) ;
#306 = CARTESIAN_POINT ( 'NONE',  ( 0.1787899950787401604, -1.258982235945774075, 0.07405724077823318263 ) ) ;
#307 = AXIS2_PLACEMENT_3D ( 'NONE', #8881, #45755, #23738 ) ;
#308 = ORIENTED_EDGE ( 'NONE', *, *, #11008, .T. ) ;
#309 = CARTESIAN_POINT ( 'NONE',  ( -0.07405724077823318263, -0.2047244093950554844, -0.1787899950787401604 ) ) ;
#310 = DIRECTION ( 'NONE',  ( 0.000000000000000000, 0.000000000000000000, 1.000000000000000000 ) ) ;
#311 = ORIENTED_EDGE ( 'NONE', *, *, #11167, .T. ) ;
#312 = CARTESIAN_POINT ( 'NONE',  ( 0.8019270111902717657, 0.1787899950787401604, 1.136811023568283119 ) ) ;
#313 = CARTESIAN_POINT ( 'NONE',  ( 0.000000000000000000, -0.09842519685039370636, 0.000000000000000000 ) ) ;
#314 = CARTESIAN_POINT ( 'NONE',  ( -0.8759842519685039353, 0.1574803149606299191, 0.9940944880814488460 ) ) ;
#315 = EDGE_CURVE ( 'NONE', #5716, #5360, #10980, .T. ) ;
#316 = CARTESIAN_POINT ( 'NONE',  ( 0.9500414927467378812, 0.1787899950787401604, 0.1870078739619845387 ) ) ;
#317 = CARTESIAN_POINT ( 'NONE',  ( -0.1787899950787401604, -1.656496062938362268, 0.07405724077823318263 ) ) ;
#318 = CARTESIAN_POINT ( 'NONE',  ( 0.1787899950787401604, -1.715551181048599716, 0.07405724077823318263 ) ) ;
#319 = APPLICATION_PROTOCOL_DEFINITION ( 'draft international standard', 'automotive_design', 1998, #20485 ) ;
#320 = APPLICATION_CONTEXT ( 'automotive_design' ) ;
#321 = EDGE_CURVE ( 'NONE', #8150, #39441, #13683, .T. ) ;
#322 = CARTESIAN_POINT ( 'NONE',  ( -0.8759842519685039353, -0.1787899950787401882, 0.5290354330171024300 ) ) ;
#323 = DIRECTION ( 'NONE',  ( -2.602085213965207486E-14, -0.6156614753256566264, -0.7880107536067233465 ) ) ;
#324 = CARTESIAN_POINT ( 'NONE',  ( 3.301370929368692659E-17, -1.369138297772021673, 0.1797182628040039365 ) ) ;
#325 = CARTESIAN_POINT ( 'NONE',  ( 1.033464566929134687, 0.06523048226347956391, 1.429625984251967852 ) ) ;
#326 = AXIS2_PLACEMENT_3D ( 'NONE', #47306, #10657, #25265 ) ;
#327 = CARTESIAN_POINT ( 'NONE',  ( 1.002407869896990045, 0.1264236179284866091, 1.409940944828126153 ) ) ;
#328 = CARTESIAN_POINT ( 'NONE',  ( 0.6971942568897648851, 0.07405724077823318263, 1.732283464513166615 ) ) ;
#329 = B_SPLINE_CURVE_WITH_KNOTS ( 'NONE', 3,
 ( #40653, #8085, #22708, #37314, #20055, #46161, #9758, #34449, #45674, #2308, #13357, #45919, #24148, #16938, #24370, #42328, #41837, #20757 ),
 .UNSPECIFIED., .F., .F.,
 ( 4, 2, 2, 2, 1, 1, 2, 2, 2, 4 ),
 ( 0.000000000000000000, 0.2499999999999993894, 0.3749999999999990008, 0.4374999999999987788, 0.4687499999999986122, 0.4843749999999986122, 0.4921874999999985567, 0.4999999999999985567, 0.7499999999999992228, 1.000000000000000000 ),
 .UNSPECIFIED. ) ;
#330 = AXIS2_PLACEMENT_3D ( 'NONE', #15898, #1005, #37686 ) ;
#331 = CIRCLE ( 'NONE', #19461, 0.1870078740157480324 ) ;
#332 = CARTESIAN_POINT ( 'NONE',  ( 0.7185039370078714072, 0.06523048226347728795, 1.513287401467276583 ) ) ;
#333 = DIRECTION ( 'NONE',  ( 1.000000000000000000, 2.891205793294678326E-16, 0.000000000000000000 ) ) ;
#334 = CARTESIAN_POINT ( 'NONE',  ( 0.7185039370078746268, -0.06523048226347956391, 0.8095472439869610959 ) ) ;
#336 = CARTESIAN_POINT ( 'NONE',  ( 0.5358894627757212481, 4.766607801171850497E-17, 0.000000000000000000 ) ) ;
#335 = CARTESIAN_POINT ( 'NONE',  ( 0.1113553986120547346, -0.8198818896562519720, -0.1113553986120547346 ) ) ;
#337 = CARTESIAN_POINT ( 'NONE',  ( 0.7185039370078739607, 1.928577636452523993E-17, 0.7677165353255432922 ) ) ;
#339 = DIRECTION ( 'NONE',  ( 0.000000000000000000, 1.000000000000000000, 0.000000000000000000 ) ) ;
#338 = CARTESIAN_POINT ( 'NONE',  ( 1.002407869896990045, 0.1264236179284866091, 1.286909448765133801 ) ) ;
#340 = DIRECTION ( 'NONE',  ( 1.000000000000000000, 0.000000000000000000, 0.000000000000000000 ) ) ;
#341 = CARTESIAN_POINT ( 'NONE',  ( 0.7185039370078739607, 0.000000000000000000, 4.498031496062992574 ) ) ;
#342 = CARTESIAN_POINT ( 'NONE',  ( -0.7495606340400177148, -0.1264236179284866091, 1.267224409395055096 ) ) ;
#343 = CARTESIAN_POINT ( 'NONE',  ( 0.7646288533564489232, -0.1113553986120547346, 0.6545275589475906264 ) ) ;
#344 = ORIENTED_EDGE ( 'NONE', *, *, #39545, .F. ) ;
#345 = CARTESIAN_POINT ( 'NONE',  ( -0.7185039370078739607, 1.928577636452523993E-17, 1.761811023622047223 ) ) ;
#346 = CARTESIAN_POINT ( 'NONE',  ( -0.1992661408232795639, -0.3637244504922588773, -1.027838479691305595 ) ) ;
#347 = EDGE_LOOP ( 'NONE', ( #1174, #678, #18238, #19385 ) ) ;
#348 = CARTESIAN_POINT ( 'NONE',  ( 0.9412147342319837628, -0.1574803149606297803, 0.2780511811023620439 ) ) ;
#349 = CARTESIAN_POINT ( 'NONE',  ( -0.1270800023317771588, 0.1515309935665608287, -0.1270800023317771588 ) ) ;
#350 = CARTESIAN_POINT ( 'NONE',  ( 0.1574803149606300301, -1.063484251860977059, 0.06523048226347956391 ) ) ;
#351 = DIRECTION ( 'NONE',  ( 0.000000000000000000, -0.6220299971367094782, 0.7829934116339071215 ) ) ;
#352 = CARTESIAN_POINT ( 'NONE',  ( 0.9500414927467378812, 0.1787899950787401604, 1.643700787347811998 ) ) ;
#354 = CARTESIAN_POINT ( 'NONE',  ( -0.7185039370078732945, -0.06523048226347920309, 0.1107283464566930498 ) ) ;
#353 = CARTESIAN_POINT ( 'NONE',  ( -0.8759842519685039353, 0.1574803149606299191, 0.9251968503937008093 ) ) ;
#355 = CARTESIAN_POINT ( 'NONE',  ( 0.7646288533564489232, -0.1113553986120547346, 1.176181102362204633 ) ) ;
#356 = CARTESIAN_POINT ( 'NONE',  ( 0.07405724077823318263, -0.2244094487651340231, 0.1787899950787401604 ) ) ;
#357 = ORIENTED_EDGE ( 'NONE', *, *, #35134, .F. ) ;
#358 = ( BOUNDED_CURVE ( )  B_SPLINE_CURVE ( 2, ( #11263, #3350, #25876, #28789, #17960, #43354, #17490, #32615, #32121 ),
 .UNSPECIFIED., .F., .T. ) 
 B_SPLINE_CURVE_WITH_KNOTS ( ( 3, 2, 2, 2, 3 ),
 ( 0.2300000000000000100, 0.2325000000000000122, 0.2349999999999999867, 0.2374999999999999889, 0.2399999999999999911 ),
 .UNSPECIFIED. ) 
 CURVE ( )  GEOMETRIC_REPRESENTATION_ITEM ( )  RATIONAL_B_SPLINE_CURVE ( ( 1.000000000000000000, 0.9238795325112869605, 1.000000000000000000, 0.9238795325112869605, 1.000000000000000000, 0.9238795325112869605, 1.000000000000000000, 0.9238795325112869605, 1.000000000000000000 ) ) 
 REPRESENTATION_ITEM ( '' )  ) ;
#359 = DIRECTION ( 'NONE',  ( 1.822029033848725028E-16, 0.000000000000000000, 1.000000000000000000 ) ) ;
#360 = CARTESIAN_POINT ( 'NONE',  ( -0.009745153983727199848, -0.04193537623276894638, 0.2798067035903421540 ) ) ;
#361 = CARTESIAN_POINT ( 'NONE',  ( 1.054774247047244540, -0.07405724077823318263, 0.6545275590013545086 ) ) ;
#362 = ORIENTED_EDGE ( 'NONE', *, *, #11409, .F. ) ;
#363 = CARTESIAN_POINT ( 'NONE',  ( 0.8759842519685039353, 0.1787899950787401882, 0.8243110235682834519 ) ) ;
#364 = CARTESIAN_POINT ( 'NONE',  ( -9.642888182262618425E-18, 0.09055118120988918384, -0.1574803149606299191 ) ) ;
#365 = CARTESIAN_POINT ( 'NONE',  ( -0.8759842519685039353, -0.1787899950787401882, 1.277066929080094448 ) ) ;
#366 = CARTESIAN_POINT ( 'NONE',  ( -0.7495606340400177148, 0.1264236179284866091, 0.1599409448281264023 ) ) ;
#367 = LINE ( 'NONE', #8269, #13455 ) ;
#368 = VECTOR ( 'NONE', #12553, 39.37007874015748143 ) ;
#369 = CARTESIAN_POINT ( 'NONE',  ( 0.1787899950787401882, -0.9021908973630964335, -2.189545951927503898E-17 ) ) ;
#370 = VERTEX_POINT ( 'NONE', #31969 ) ;
#371 = DIRECTION ( 'NONE',  ( 0.000000000000000000, 0.000000000000000000, 1.000000000000000000 ) ) ;
#372 = AXIS2_PLACEMENT_3D ( 'NONE', #5692, #17413, #32052 ) ;
#373 = ORIENTED_EDGE ( 'NONE', *, *, #26554, .F. ) ;
#374 = CARTESIAN_POINT ( 'NONE',  ( 1.054774247047244096, 0.000000000000000000, 1.006397637741511808 ) ) ;
#375 = CARTESIAN_POINT ( 'NONE',  ( 0.003837171311379782533, -0.04331820873536343375, 0.1377949924024825246 ) ) ;
#376 = ( BOUNDED_CURVE ( )  B_SPLINE_CURVE ( 2, ( #44031, #36857, #22706, #4461, #11233, #44728, #15066, #25618, #15540 ),
 .UNSPECIFIED., .F., .T. ) 
 B_SPLINE_CURVE_WITH_KNOTS ( ( 3, 2, 2, 2, 3 ),
 ( 0.07000000000000000666, 0.07249999999999999500, 0.07499999999999999722, 0.07749999999999999944, 0.08000000000000000167 ),
 .UNSPECIFIED. ) 
 CURVE ( )  GEOMETRIC_REPRESENTATION_ITEM ( )  RATIONAL_B_SPLINE_CURVE ( ( 1.000000000000000000, 0.9238795325112859613, 1.000000000000000000, 0.9238795325112869605, 1.000000000000000000, 0.9238795325112869605, 1.000000000000000000, 0.9238795325112869605, 1.000000000000000000 ) ) 
 REPRESENTATION_ITEM ( '' )  ) ;
#377 = CARTESIAN_POINT ( 'NONE',  ( -1.054774247047244540, -0.07405724077823318263, 0.7283464566391493200 ) ) ;
#378 = EDGE_CURVE ( 'NONE', #9213, #13081, #13737, .T. ) ;
#379 = CARTESIAN_POINT ( 'NONE',  ( -0.1787899950787401604, -0.4753937007336378473, 0.07405724077823318263 ) ) ;
#380 = EDGE_CURVE ( 'NONE', #22666, #46167, #21394, .T. ) ;
#381 = CARTESIAN_POINT ( 'NONE',  ( -1.002407869896990045, 0.1264236179284866091, 0.07135826766277185429 ) ) ;
#382 = CARTESIAN_POINT ( 'NONE',  ( -0.8759842519685039353, 0.1574803149606299191, 0.9251968503937008093 ) ) ;
#383 = CARTESIAN_POINT ( 'NONE',  ( -0.1270800023317771588, -1.059098927693281622, 0.1270800023317771588 ) ) ;
#384 = CARTESIAN_POINT ( 'NONE',  ( 0.6195511811023588500, -5.463695987328330208E-16, -1.186023622047243986 ) ) ;
#385 = CARTESIAN_POINT ( 'NONE',  ( -0.7185039370078739607, 1.928577636452523993E-17, 1.594488188868850242 ) ) ;
#386 = CARTESIAN_POINT ( 'NONE',  ( 0.8019270111902717657, -0.1787899950787401604, 0.7234251967966300878 ) ) ;
#387 = CARTESIAN_POINT ( 'NONE',  ( 0.7495606340400177148, -0.1264236179284866091, 1.345964566875370139 ) ) ;
#388 = B_SPLINE_CURVE_WITH_KNOTS ( 'NONE', 3,
 ( #34639, #1791, #24318, #31755 ),
 .UNSPECIFIED., .F., .F.,
 ( 4, 4 ),
 ( 0.000000000000000000, 1.000000000000000000 ),
 .UNSPECIFIED. ) ;
#389 = CARTESIAN_POINT ( 'NONE',  ( -0.1673228346456692994, -0.4812165006432425063, -0.8611016091043821596 ) ) ;
#391 = FACE_OUTER_BOUND ( 'NONE', #347, .T. ) ;
#390 = CARTESIAN_POINT ( 'NONE',  ( 0.7125413026092556334, -0.03488858553940781676, 1.983914878791770864 ) ) ;
#392 = CARTESIAN_POINT ( 'NONE',  ( -0.1235961452251413406, -0.09842519685039370636, 0.2140748031496062798 ) ) ;
#394 = CARTESIAN_POINT ( 'NONE',  ( 0.1637325577037128943, 0.07820587237429499350, 0.1401340067785760701 ) ) ;
#393 = CARTESIAN_POINT ( 'NONE',  ( 1.054774247047244096, 0.000000000000000000, 0.8095472440407244230 ) ) ;
#395 = AXIS2_PLACEMENT_3D ( 'NONE', #5918, #35170, #24842 ) ;
#396 = CARTESIAN_POINT ( 'NONE',  ( -0.1787899950787401604, -0.8248031495525351975, 0.07405724077823318263 ) ) ;
#397 = CARTESIAN_POINT ( 'NONE',  ( -0.5555748031496061667, 0.1864803149606364951, -0.7480314960629921295 ) ) ;
#398 = VERTEX_POINT ( 'NONE', #6064 ) ;
#399 = FACE_OUTER_BOUND ( 'NONE', #15103, .T. ) ;
#400 = CONICAL_SURFACE ( 'NONE', #29553, 0.09842519685039310962, 0.7853981633972314524 ) ;
#401 = DIRECTION ( 'NONE',  ( 1.822029033848725028E-16, 0.000000000000000000, 1.000000000000000000 ) ) ;
#402 = CARTESIAN_POINT ( 'NONE',  ( 0.8019270111902717657, 0.1787899950787401604, 0.9399606298674970661 ) ) ;
#403 = DIRECTION ( 'NONE',  ( 1.000000000000000000, 0.000000000000000000, -1.822029033848725275E-16 ) ) ;
#404 = CARTESIAN_POINT ( 'NONE',  ( -0.06523048226347956391, -1.727854330708660902, -0.1574803149606300301 ) ) ;
#405 = EDGE_CURVE ( 'NONE', #45750, #40086, #43961, .T. ) ;
#406 = DIRECTION ( 'NONE',  ( 0.000000000000000000, -0.2126700594527834443, 0.9771240687918547607 ) ) ;
#407 = ORIENTED_EDGE ( 'NONE', *, *, #24032, .F. ) ;
#408 = DIRECTION ( 'NONE',  ( -1.000000000000000000, 0.000000000000000000, 0.000000000000000000 ) ) ;
#409 = CARTESIAN_POINT ( 'NONE',  ( -0.8019270111902717657, 0.1787899950787401604, 0.2706692912848194243 ) ) ;
#410 = CARTESIAN_POINT ( 'NONE',  ( 0.9873396505805591694, 0.1113553986120547346, 0.3297244094488189226 ) ) ;
#411 = CARTESIAN_POINT ( 'NONE',  ( -0.7495606340400177148, 0.1264236179284866091, 1.611712598371433103 ) ) ;
#412 = CARTESIAN_POINT ( 'NONE',  ( -0.6971942568897648851, 0.07405724077823318263, 0.9055118109698584439 ) ) ;
#413 = CARTESIAN_POINT ( 'NONE',  ( -0.9500414927467378812, -0.1787899950787401604, 0.3346456692375748831 ) ) ;
#414 = CARTESIAN_POINT ( 'NONE',  ( -0.4330708661417322913, 0.1574803149606299191, 1.186023622047243986 ) ) ;
#415 = FACE_OUTER_BOUND ( 'NONE', #12654, .T. ) ;
#416 = CARTESIAN_POINT ( 'NONE',  ( 0.6971942568897626646, 0.07405724077823318263, 0.03937007868639404856 ) ) ;
#417 = DIRECTION ( 'NONE',  ( -1.000000000000000000, 0.000000000000000000, 0.000000000000000000 ) ) ;
#418 = CARTESIAN_POINT ( 'NONE',  ( 0.07405724077823318263, -0.3436279052371127296, -0.1787899950787401604 ) ) ;
#419 = CARTESIAN_POINT ( 'NONE',  ( 0.08603670706143877467, -0.09842519685039370636, 0.1221131442762555253 ) ) ;
#420 = CARTESIAN_POINT ( 'NONE',  ( -0.8107537697050254399, 0.1574803149606300301, 1.902066929026330566 ) ) ;
#421 = PLANE ( 'NONE',  #8031 ) ;
#422 = VECTOR ( 'NONE', #8785, 39.37007874015748143 ) ;
#423 = CARTESIAN_POINT ( 'NONE',  ( -0.8019270111902717657, 0.1787899950787401604, 0.3100393700249766682 ) ) ;
#424 = EDGE_CURVE ( 'NONE', #18854, #1825, #37750, .T. ) ;
#425 = CARTESIAN_POINT ( 'NONE',  ( -1.054774247047244540, -0.07405724077823318263, 1.323818897584032594 ) ) ;
#426 = VERTEX_POINT ( 'NONE', #25002 ) ;
#427 = AXIS2_PLACEMENT_3D ( 'NONE', #21003, #3022, #14070 ) ;
#428 = AXIS2_PLACEMENT_3D ( 'NONE', #42726, #2726, #24548 ) ;
#429 = EDGE_CURVE ( 'NONE', #8074, #10105, #18584, .T. ) ;
#430 = CARTESIAN_POINT ( 'NONE',  ( 0.1787899950787401882, -1.284940944828125930, -2.189545951927503898E-17 ) ) ;
#431 = CARTESIAN_POINT ( 'NONE',  ( 0.1264236179284866091, -1.481791338528913426, 0.1264236179284866091 ) ) ;
#432 = FILL_AREA_STYLE_COLOUR ( '', #44690 ) ;
#433 = DIRECTION ( 'NONE',  ( 0.000000000000000000, 0.000000000000000000, 1.000000000000000000 ) ) ;
#434 = CARTESIAN_POINT ( 'NONE',  ( 0.9412147342319837628, -0.1574803149606297803, 0.3567913385826772532 ) ) ;
#435 = LINE ( 'NONE', #44275, #37021 ) ;
#436 = CARTESIAN_POINT ( 'NONE',  ( -0.7646288533564489232, -0.1113553986120547346, 1.048228346349165507 ) ) ;
#437 = CARTESIAN_POINT ( 'NONE',  ( 0.7495606340400177148, -0.1264236179284866091, 0.4453740156942677664 ) ) ;
#438 = CARTESIAN_POINT ( 'NONE',  ( -0.1113553986120547346, -0.2194881889763779514, 0.1113553986120547346 ) ) ;
#439 = DIRECTION ( 'NONE',  ( 0.000000000000000000, 0.000000000000000000, -1.000000000000000000 ) ) ;
#440 = ORIENTED_EDGE ( 'NONE', *, *, #40777, .T. ) ;
#441 = CARTESIAN_POINT ( 'NONE',  ( -0.1787899950787401604, -0.2047244093950554844, -0.07405724077823318263 ) ) ;
#442 = DIRECTION ( 'NONE',  ( 0.000000000000000000, -0.6156614753256597350, -0.7880107536067206819 ) ) ;
#443 = CARTESIAN_POINT ( 'NONE',  ( 0.8759842519685039353, 0.1574803149606299191, 0.9645669291338583307 ) ) ;
#444 = CARTESIAN_POINT ( 'NONE',  ( 1.033464566929133799, 0.000000000000000000, 1.348425196850393748 ) ) ;
#445 = LINE ( 'NONE', #14857, #29310 ) ;
#446 = CARTESIAN_POINT ( 'NONE',  ( 0.01230737760510395781, 0.07955613945526338049, -0.1377952755905511861 ) ) ;
#447 = CARTESIAN_POINT ( 'NONE',  ( 0.1645760670519675339, 0.08210188079435769282, -0.1405695449895551230 ) ) ;
#448 = CARTESIAN_POINT ( 'NONE',  ( -0.3100393700787401619, -2.714815113292586694E-26, 1.043307086614172707 ) ) ;
#449 = CIRCLE ( 'NONE', #39490, 0.02900000000000001882 ) ;
#450 = ORIENTED_EDGE ( 'NONE', *, *, #1798, .T. ) ;
#451 = CARTESIAN_POINT ( 'NONE',  ( 0.000000000000000000, 0.000000000000000000, -0.1574803149606298636 ) ) ;
#452 = DIRECTION ( 'NONE',  ( 0.000000000000000000, -1.000000000000000000, 0.000000000000000000 ) ) ;
#453 = CARTESIAN_POINT ( 'NONE',  ( -0.1264236179284866091, -1.531003936954110189, 0.1264236179284866091 ) ) ;
#454 = CARTESIAN_POINT ( 'NONE',  ( 0.07405724077823318263, -0.8198818897100156322, 0.1787899950787401604 ) ) ;
#455 = CARTESIAN_POINT ( 'NONE',  ( -0.06523048226347956391, -1.240649606299213614, 0.1574803149606297803 ) ) ;
#456 = CARTESIAN_POINT ( 'NONE',  ( 0.7646288533564489232, -0.1113553986120547346, 0.9301181101286929431 ) ) ;
#457 = CARTESIAN_POINT ( 'NONE',  ( 0.2759478392031653460, -0.09842519685039370636, 2.185526306663015728 ) ) ;
#458 = UNCERTAINTY_MEASURE_WITH_UNIT (LENGTH_MEASURE( 1.000000000000000082E-05 ), #21946, 'distance_accuracy_value', 'NONE') ;
#459 = ORIENTED_EDGE ( 'NONE', *, *, #45696, .T. ) ;
#460 = VERTEX_POINT ( 'NONE', #6542 ) ;
#461 = VERTEX_POINT ( 'NONE', #43426 ) ;
#462 = CARTESIAN_POINT ( 'NONE',  ( -1.002407869896990045, -0.1264236179284866091, 1.557578740103716441 ) ) ;
#463 = CARTESIAN_POINT ( 'NONE',  ( 1.054774247047244540, -0.07405724077823318263, 1.638779527505292988 ) ) ;
#464 = CARTESIAN_POINT ( 'NONE',  ( -1.002407869896990045, -0.1264236179284866091, 0.8095472440407244230 ) ) ;
#465 = DIRECTION ( 'NONE',  ( 0.000000000000000000, -1.000000000000000000, -0.000000000000000000 ) ) ;
#466 = CARTESIAN_POINT ( 'NONE',  ( 0.8759842519685039353, 0.1787899950787401882, 0.2731299212060791515 ) ) ;
#467 = CARTESIAN_POINT ( 'NONE',  ( -0.07874015748031489015, -0.5708661417322835607, 0.9783464566929127582 ) ) ;
#468 = CARTESIAN_POINT ( 'NONE',  ( -0.7495606340400177148, 0.1264236179284866091, 1.296751968450173154 ) ) ;
#469 = DIRECTION ( 'NONE',  ( 1.822029033848725028E-16, 0.000000000000000000, 1.000000000000000000 ) ) ;
#470 = CARTESIAN_POINT ( 'NONE',  ( 0.3604359965418638123, 4.466152701071653354E-17, 0.000000000000000000 ) ) ;
#471 = CARTESIAN_POINT ( 'NONE',  ( -0.7495606340400177148, -0.1264236179284866091, 1.626476377898992132 ) ) ;
#472 = CARTESIAN_POINT ( 'NONE',  ( -0.9873396505805591694, -0.1113553986120547346, 1.884842519577511810 ) ) ;
#473 = ORIENTED_EDGE ( 'NONE', *, *, #10794, .F. ) ;
#474 = CARTESIAN_POINT ( 'NONE',  ( -1.033464566929133799, 0.000000000000000000, 1.663385826771653697 ) ) ;
#475 = DIRECTION ( 'NONE',  ( 0.5735764363510417185, 0.6455006197386566891, -0.5043203561029927506 ) ) ;
#476 = EDGE_CURVE ( 'NONE', #44070, #30751, #10635, .T. ) ;
#477 = CARTESIAN_POINT ( 'NONE',  ( 0.7495606340400177148, -0.1264236179284866091, 1.468996062938362046 ) ) ;
#478 = CARTESIAN_POINT ( 'NONE',  ( -0.2009290272083082973, -0.09842519685039370636, 0.1224581209280712624 ) ) ;
#479 = CARTESIAN_POINT ( 'NONE',  ( 1.033464566929133799, 1.928577636452524610E-17, 4.498031496062992574 ) ) ;
#480 = VERTEX_POINT ( 'NONE', #32205 ) ;
#481 = ORIENTED_EDGE ( 'NONE', *, *, #44567, .F. ) ;
#482 = EDGE_LOOP ( 'NONE', ( #14896, #4355, #6135, #13847 ) ) ;
#483 = EDGE_CURVE ( 'NONE', #12524, #45117, #9920, .T. ) ;
#484 = CARTESIAN_POINT ( 'NONE',  ( 0.1787899950787401604, -0.8937007873478103326, 0.07405724077823318263 ) ) ;
#485 = CARTESIAN_POINT ( 'NONE',  ( -0.1264236179284866091, -0.9010826771115905132, 0.1264236179284866091 ) ) ;
#486 = LINE ( 'NONE', #44113, #7940 ) ;
#487 = CARTESIAN_POINT ( 'NONE',  ( 0.6971942568897648851, 0.07405724077823318263, 1.732283464513166615 ) ) ;
#488 = CARTESIAN_POINT ( 'NONE',  ( 0.1797182628040039087, -0.2544729434413131597, -0.07444174185955065859 ) ) ;
#489 = FACE_OUTER_BOUND ( 'NONE', #28194, .T. ) ;
#490 = CARTESIAN_POINT ( 'NONE',  ( 0.07405724077823318263, -0.03248031490686641154, 0.1787899950787401604 ) ) ;
#491 = CARTESIAN_POINT ( 'NONE',  ( -0.9873396505805591694, -0.1113553986120547346, 0.9005905510735748853 ) ) ;
#492 = CARTESIAN_POINT ( 'NONE',  ( 0.6971942568897626646, -0.07405724077823297447, 0.7923228345919055560 ) ) ;
#493 = CARTESIAN_POINT ( 'NONE',  ( 0.3849708276051176936, 1.205361022782824954E-17, -0.09842519685039370636 ) ) ;
#495 = FACE_OUTER_BOUND ( 'NONE', #27170, .T. ) ;
#494 = LINE ( 'NONE', #33851, #14264 ) ;
#496 = CARTESIAN_POINT ( 'NONE',  ( 0.6195511811023624027, 0.9842519685039370358, -0.8759842519685050455 ) ) ;
#497 = CARTESIAN_POINT ( 'NONE',  ( 1.054774247047244540, -0.07405724077823318263, 1.874999999946236784 ) ) ;
#498 = CARTESIAN_POINT ( 'NONE',  ( 0.5555748031496077211, 2.215965818540671970E-15, 0.7480314960629921295 ) ) ;
#499 = CARTESIAN_POINT ( 'NONE',  ( 1.033464566929134687, 0.06523048226347956391, 0.05167322834645668439 ) ) ;
#500 = CARTESIAN_POINT ( 'NONE',  ( 0.4330708661417322913, 4.616380251121755931E-17, 0.000000000000000000 ) ) ;
#501 = CARTESIAN_POINT ( 'NONE',  ( -0.1787899950787401882, -0.3203740156942680994, 0.000000000000000000 ) ) ;
#502 = DIRECTION ( 'NONE',  ( 0.000000000000000000, -1.000000000000000000, 0.000000000000000000 ) ) ;
#504 = CIRCLE ( 'NONE', #41823, 0.1003937007874011050 ) ;
#503 = CARTESIAN_POINT ( 'NONE',  ( 0.1787899950787401604, -1.164370078686393306, 0.07405724077823318263 ) ) ;
#505 = ( BOUNDED_CURVE ( )  B_SPLINE_CURVE ( 2, ( #37995, #45404, #8993, #34647, #17355, #14004, #10901, #46347, #35584 ),
 .UNSPECIFIED., .F., .F. ) 
 B_SPLINE_CURVE_WITH_KNOTS ( ( 3, 2, 2, 2, 3 ),
 ( 0.5899999999999999689, 0.5925000000000000266, 0.5949999999999999734, 0.5975000000000000311, 0.5999999999999999778 ),
 .UNSPECIFIED. ) 
 CURVE ( )  GEOMETRIC_REPRESENTATION_ITEM ( )  RATIONAL_B_SPLINE_CURVE ( ( 1.000000000000000000, 0.9238795325112869605, 1.000000000000000000, 0.9238795325112869605, 1.000000000000000000, 0.9238795325112869605, 1.000000000000000000, 0.9238795325112869605, 1.000000000000000000 ) ) 
 REPRESENTATION_ITEM ( '' )  ) ;
#506 = CARTESIAN_POINT ( 'NONE',  ( 0.6971942568897626646, 0.07405724077823318263, 0.2017716534895435399 ) ) ;
#507 = CARTESIAN_POINT ( 'NONE',  ( 0.1574803149606300023, -1.308580299410598613, -1.920078980116132872 ) ) ;
#508 = CARTESIAN_POINT ( 'NONE',  ( -0.6971942568897637749, 2.189545951927499583E-17, 1.577263779473795369 ) ) ;
#509 = ORIENTED_EDGE ( 'NONE', *, *, #3081, .F. ) ;
#510 = ( BOUNDED_CURVE ( )  B_SPLINE_CURVE ( 2, ( #44895, #41286, #45377, #26733, #8969, #4890, #8486, #9205, #45132 ),
 .UNSPECIFIED., .F., .T. ) 
 B_SPLINE_CURVE_WITH_KNOTS ( ( 3, 2, 2, 2, 3 ),
 ( 0.6099999999999999867, 0.6125000000000000444, 0.6149999999999999911, 0.6175000000000000488, 0.6199999999999999956 ),
 .UNSPECIFIED. ) 
 CURVE ( )  GEOMETRIC_REPRESENTATION_ITEM ( )  RATIONAL_B_SPLINE_CURVE ( ( 1.000000000000000000, 0.9238795325112869605, 1.000000000000000000, 0.9238795325112869605, 1.000000000000000000, 0.9238795325112869605, 1.000000000000000000, 0.9238795325112869605, 1.000000000000000000 ) ) 
 REPRESENTATION_ITEM ( '' )  ) ;
#511 = CARTESIAN_POINT ( 'NONE',  ( -0.9500414927467378812, 0.1787899950787401604, 1.176181102308441417 ) ) ;
#512 = CARTESIAN_POINT ( 'NONE',  ( 0.1377952755905511861, -1.365923996832131609E-16, 0.9074803149606294195 ) ) ;
#513 = CARTESIAN_POINT ( 'NONE',  ( 0.6971942568897648851, 0.07405724077823318263, 1.304133858213953667 ) ) ;
#514 = CARTESIAN_POINT ( 'NONE',  ( 0.8759842519685039353, -0.1787899950787401882, 1.980807086560409491 ) ) ;
#515 = CARTESIAN_POINT ( 'NONE',  ( -0.6971942568897648851, 0.07405724077823318263, 1.102362204670646495 ) ) ;
#516 = ADVANCED_FACE ( 'NONE', ( #27279 ), #1832, .T. ) ;
#517 = CARTESIAN_POINT ( 'NONE',  ( 0.1577586585109271855, 0.1377137394884521138, -0.04231661445875282285 ) ) ;
#518 = CYLINDRICAL_SURFACE ( 'NONE', #9417, 0.5708661417322833387 ) ;
#519 = CARTESIAN_POINT ( 'NONE',  ( 1.054774247047244540, -0.07405724077823318263, 0.4183070865604096578 ) ) ;
#520 = CARTESIAN_POINT ( 'NONE',  ( -0.7495606340400177148, 0.1264236179284866091, 0.1550196849856066983 ) ) ;
#521 = CARTESIAN_POINT ( 'NONE',  ( -0.9500414927467378812, -0.1787899950787401604, 0.7234251967966300878 ) ) ;
#522 = ORIENTED_EDGE ( 'NONE', *, *, #12247, .F. ) ;
#523 = ADVANCED_FACE ( 'NONE', ( #24362 ), #19359, .F. ) ;
#524 = CARTESIAN_POINT ( 'NONE',  ( -0.1264236179284866091, -0.08907480309584270284, -0.1264236179284866091 ) ) ;
#525 = ORIENTED_EDGE ( 'NONE', *, *, #11840, .F. ) ;
#526 = CARTESIAN_POINT ( 'NONE',  ( -0.9412147342319837628, -0.1574803149606297803, 0.1205708661417322497 ) ) ;
#527 = ADVANCED_FACE ( 'NONE', ( #9030 ), #27517, .T. ) ;
#528 = CARTESIAN_POINT ( 'NONE',  ( -0.1750152858685271595, -0.09851385417196180383, -0.1786646369836015769 ) ) ;
#529 = VERTEX_POINT ( 'NONE', #25560 ) ;
#530 = CARTESIAN_POINT ( 'NONE',  ( 0.8759842519685039353, 0.1787899950787401882, 1.921751968450173376 ) ) ;
#531 = CARTESIAN_POINT ( 'NONE',  ( -1.002407869896990045, -0.1264236179284866091, 0.05659448813521283234 ) ) ;
#532 = CARTESIAN_POINT ( 'NONE',  ( 0.1787899950787401604, -1.455832629646562015, 0.07405724077823318263 ) ) ;
#533 = EDGE_LOOP ( 'NONE', ( #23473, #14540, #33151, #19710 ) ) ;
#534 = CARTESIAN_POINT ( 'NONE',  ( 0.07405724077823318263, -0.4212598424659216856, 0.1787899950787401604 ) ) ;
#535 = DIRECTION ( 'NONE',  ( 1.000000000000000000, -0.000000000000000000, -0.000000000000000000 ) ) ;
#536 = ORIENTED_EDGE ( 'NONE', *, *, #44389, .T. ) ;
#537 = CARTESIAN_POINT ( 'NONE',  ( 0.8759842519685039353, -0.1787899950787401882, 1.232775590497417362 ) ) ;
#538 = CARTESIAN_POINT ( 'NONE',  ( -0.5555748031496058337, 0.2597269656108975311, 0.7480314960629921295 ) ) ;
#539 = CARTESIAN_POINT ( 'NONE',  ( -0.1586641775163213364, 1.209494567139720367, -1.479906699140297599 ) ) ;
#540 = CARTESIAN_POINT ( 'NONE',  ( -0.9873396505805591694, 0.1113553986120547346, 1.432086614173228245 ) ) ;
#541 = CARTESIAN_POINT ( 'NONE',  ( 1.002407869896990045, 0.1264236179284866091, 0.2239173227808822775 ) ) ;
#542 = CARTESIAN_POINT ( 'NONE',  ( 0.07405724077823318263, -1.646653543253324026, 0.1787899950787401604 ) ) ;
#543 = CARTESIAN_POINT ( 'NONE',  ( -0.1787899950787401604, -1.651574803095843258, 0.07405724077823318263 ) ) ;
#544 = APPLICATION_PROTOCOL_DEFINITION ( 'draft international standard', 'automotive_design', 1998, #320 ) ;
#545 = DIRECTION ( 'NONE',  ( 0.000000000000000000, -8.673617379884043361E-16, 1.000000000000000000 ) ) ;
#546 = ORIENTED_EDGE ( 'NONE', *, *, #8764, .F. ) ;
#547 = CARTESIAN_POINT ( 'NONE',  ( -0.6971942568897648851, 0.07405724077823318263, 0.7135826771115916234 ) ) ;
#548 = CARTESIAN_POINT ( 'NONE',  ( -1.100456976456230270E-17, -1.349453258401942746, -0.1797182628040039365 ) ) ;
#549 = CARTESIAN_POINT ( 'NONE',  ( 0.6195511811023604043, 0.4133858267716528090, 0.9891732283464566011 ) ) ;
#550 = CARTESIAN_POINT ( 'NONE',  ( 1.054774247047244540, -0.07405724077823318263, 1.323818897584032817 ) ) ;
#551 = CARTESIAN_POINT ( 'NONE',  ( 1.054774247047244540, -0.07405724077823318263, 1.633858267662771091 ) ) ;
#552 = CARTESIAN_POINT ( 'NONE',  ( 0.8759842519685039353, -0.1787899950787401882, 0.2485236219934806867 ) ) ;
#553 = DIRECTION ( 'NONE',  ( 1.000000000000000000, 0.000000000000000000, -1.822029033848725275E-16 ) ) ;
#554 = EDGE_CURVE ( 'NONE', #37817, #25198, #47100, .T. ) ;
#555 = DIRECTION ( 'NONE',  ( 1.000000000000000000, 0.000000000000000000, 0.000000000000000000 ) ) ;
#556 = DIRECTION ( 'NONE',  ( 0.000000000000000000, 0.9699617890481115889, 0.2432573283306930789 ) ) ;
#557 = CARTESIAN_POINT ( 'NONE',  ( -1.094772975963752103E-17, 0.1422244095025824717, -0.1787899950787401882 ) ) ;
#558 = CARTESIAN_POINT ( 'NONE',  ( -0.1586641775163213364, 1.205832402325951680, -1.129708666049261900 ) ) ;
#559 = CARTESIAN_POINT ( 'NONE',  ( 0.6971942568897637749, 2.189545951927499583E-17, 0.2780511810485988278 ) ) ;
#560 = CARTESIAN_POINT ( 'NONE',  ( -0.9412147342319837628, 0.1574803149606300301, 1.710137795275591843 ) ) ;
#561 = DIRECTION ( 'NONE',  ( 1.144917494144692682E-16, -3.972230510298676574E-31, 1.000000000000000000 ) ) ;
#562 = AXIS2_PLACEMENT_3D ( 'NONE', #23103, #45118, #555 ) ;
#563 = CARTESIAN_POINT ( 'NONE',  ( 0.2759478392031586291, -3.539702385322740129E-16, 1.224299699984019663 ) ) ;
#564 = CARTESIAN_POINT ( 'NONE',  ( -0.8019270111902717657, 0.1787899950787401604, 1.215551181048599272 ) ) ;
#565 = CARTESIAN_POINT ( 'NONE',  ( 0.8107537697050253289, -0.1574803149606297803, 0.6963582676090082080 ) ) ;
#566 = ORIENTED_EDGE ( 'NONE', *, *, #42957, .T. ) ;
#567 = CARTESIAN_POINT ( 'NONE',  ( 0.7185039370078746268, 0.06523048226347956391, 1.405019685039369914 ) ) ;
#568 = CARTESIAN_POINT ( 'NONE',  ( -0.2066929133858267931, -0.3022687907404924545, -1.075852903322848331 ) ) ;
#569 = ORIENTED_EDGE ( 'NONE', *, *, #21974, .T. ) ;
#570 = CARTESIAN_POINT ( 'NONE',  ( 0.1797182628040039365, -0.06008317966178563369, -2.200913952912460540E-17 ) ) ;
#571 = CARTESIAN_POINT ( 'NONE',  ( -0.7185039370078746268, -0.06523048226347956391, 0.2977362203649139283 ) ) ;
#572 = CARTESIAN_POINT ( 'NONE',  ( -0.1787899950787401604, -1.188976377898991688, -0.07405724077823318263 ) ) ;
#573 = CARTESIAN_POINT ( 'NONE',  ( 3.334775382890951728E-20, 0.003375231709989810237, 0.1377952755905512139 ) ) ;
#574 = CARTESIAN_POINT ( 'NONE',  ( 0.8759842519685039353, -0.1787899950787401882, 1.626476377898992132 ) ) ;
#575 = EDGE_CURVE ( 'NONE', #3281, #35903, #38693, .T. ) ;
#576 = FACE_OUTER_BOUND ( 'NONE', #27675, .T. ) ;
#577 = CARTESIAN_POINT ( 'NONE',  ( -1.033464566929134687, 0.06523048226347956391, 0.9178149606299221830 ) ) ;
#578 = CARTESIAN_POINT ( 'NONE',  ( 0.7646288533564489232, -0.1113553986120547346, 1.914370078632629868 ) ) ;
#579 = CARTESIAN_POINT ( 'NONE',  ( 3.284318927891251994E-17, -0.2268700786863941110, 0.1787899950787401882 ) ) ;
#580 = VERTEX_POINT ( 'NONE', #5172 ) ;
#581 = AXIS2_PLACEMENT_3D ( 'NONE', #37868, #23494, #19160 ) ;
#582 = EDGE_CURVE ( 'NONE', #35894, #1072, #33031, .T. ) ;
#583 = CARTESIAN_POINT ( 'NONE',  ( -0.06523048226347935574, 0.09793307086614168322, 0.1574803149606300301 ) ) ;
#584 = CARTESIAN_POINT ( 'NONE',  ( 0.000000000000000000, 0.000000000000000000, -0.3149606299212598381 ) ) ;
#585 = ORIENTED_EDGE ( 'NONE', *, *, #39318, .F. ) ;
#586 = EDGE_CURVE ( 'NONE', #31109, #36213, #45187, .T. ) ;
#587 = CARTESIAN_POINT ( 'NONE',  ( -0.7495606340400177148, -0.1264236179284866091, 1.464074803095842370 ) ) ;
#588 = CARTESIAN_POINT ( 'NONE',  ( -0.1113553986120547346, 0.1348425197925665342, -0.1113553986120547346 ) ) ;
#589 = CARTESIAN_POINT ( 'NONE',  ( -0.7495606340400177148, -0.1264236179284866091, 1.311515747977732405 ) ) ;
#590 = ADVANCED_FACE ( 'NONE', ( #4944 ), #41819, .T. ) ;
#591 = CARTESIAN_POINT ( 'NONE',  ( -0.8019270111902717657, -0.1787899950787401604, 0.3690944881352128393 ) ) ;
#592 = CARTESIAN_POINT ( 'NONE',  ( 0.004734662961546367427, 0.1434636420620040986, -0.02711672434608614068 ) ) ;
#593 = CARTESIAN_POINT ( 'NONE',  ( -0.4620708661417322616, 0.6102362204724408601, 0.5854071585544579071 ) ) ;
#594 = CARTESIAN_POINT ( 'NONE',  ( 0.07405724077823318263, -0.9883129446071914348, 0.1787899950787401604 ) ) ;
#595 = ORIENTED_EDGE ( 'NONE', *, *, #3073, .T. ) ;
#596 = CARTESIAN_POINT ( 'NONE',  ( 0.1787899950787401604, 0.1348425197388028463, 0.07405724077823318263 ) ) ;
#597 = EDGE_LOOP ( 'NONE', ( #36228, #9549, #2235, #27768 ) ) ;
#598 = CARTESIAN_POINT ( 'NONE',  ( 0.6971942568897648851, -0.07405724077823297447, 1.028543307032851795 ) ) ;
#599 = CARTESIAN_POINT ( 'NONE',  ( 0.7185039370078739607, 1.928577636452523993E-17, 1.200787401467275695 ) ) ;
#600 = CARTESIAN_POINT ( 'NONE',  ( -0.8759842519685039353, -0.1574803149606299191, 0.5807086613097960370 ) ) ;
#601 = VECTOR ( 'NONE', #24176, 39.37007874015748143 ) ;
#602 = AXIS2_PLACEMENT_3D ( 'NONE', #9099, #23721, #38801 ) ;
#603 = CARTESIAN_POINT ( 'NONE',  ( -0.7646288533564489232, 0.1113553986120547346, 0.8907480314960629642 ) ) ;
#604 = CYLINDRICAL_SURFACE ( 'NONE', #44721, 0.1574803149606299191 ) ;
#605 = CARTESIAN_POINT ( 'NONE',  ( -0.07444174185955065859, -1.071402077299582034, -0.1797182628040039087 ) ) ;
#606 = CARTESIAN_POINT ( 'NONE',  ( 0.1574803149606299191, 0.6241017553149685870, 0.3240160679609070948 ) ) ;
#607 = CARTESIAN_POINT ( 'NONE',  ( -0.7185039370078746268, -0.06523048226347956391, 1.518208661309795149 ) ) ;
#608 = CARTESIAN_POINT ( 'NONE',  ( 1.054774247047244540, 0.07405724077823318263, 0.9350393700249758355 ) ) ;
#609 = CARTESIAN_POINT ( 'NONE',  ( 0.7495606340400177148, 0.1264236179284866091, 1.375492125930488196 ) ) ;
#610 = CARTESIAN_POINT ( 'NONE',  ( -0.9412147342319837628, 0.1574803149606300301, 0.4502952755905510474 ) ) ;
#611 = CARTESIAN_POINT ( 'NONE',  ( 0.8759842519685039353, -0.1574803149606299191, 1.456692913385826849 ) ) ;
#612 = CARTESIAN_POINT ( 'NONE',  ( 0.000000000000000000, -0.09842519685039370636, 0.000000000000000000 ) ) ;
#613 = ( BOUNDED_CURVE ( )  B_SPLINE_CURVE ( 2, ( #7881, #44290, #26361, #32849, #7413, #29979, #15326, #47443, #39990 ),
 .UNSPECIFIED., .F., .T. ) 
 B_SPLINE_CURVE_WITH_KNOTS ( ( 3, 2, 2, 2, 3 ),
 ( 0.4099999999999999756, 0.4124999999999999778, 0.4149999999999999800, 0.4174999999999999822, 0.4199999999999999845 ),
 .UNSPECIFIED. ) 
 CURVE ( )  GEOMETRIC_REPRESENTATION_ITEM ( )  RATIONAL_B_SPLINE_CURVE ( ( 1.000000000000000000, 0.9238795325112879597, 1.000000000000000000, 0.9238795325112869605, 1.000000000000000000, 0.9238795325112869605, 1.000000000000000000, 0.9238795325112869605, 1.000000000000000000 ) ) 
 REPRESENTATION_ITEM ( '' )  ) ;
#614 = CARTESIAN_POINT ( 'NONE',  ( 0.8019270111902716547, 0.1787899950787401604, 0.8218503936470251681 ) ) ;
#615 = CARTESIAN_POINT ( 'NONE',  ( -0.07405724077823318263, -0.7411417322297018107, 0.1787899950787401604 ) ) ;
#616 = ORIENTED_EDGE ( 'NONE', *, *, #20566, .T. ) ;
#617 = CARTESIAN_POINT ( 'NONE',  ( 0.7646288533564489232, -0.1113553986120547346, 0.4183070865066456645 ) ) ;
#618 = DIRECTION ( 'NONE',  ( -0.000000000000000000, 0.7880107536067184615, -0.6156614753256628436 ) ) ;
#619 = CARTESIAN_POINT ( 'NONE',  ( 0.7495606340400177148, -0.1264236179284866091, 1.070374015694267600 ) ) ;
#620 = LINE ( 'NONE', #7837, #8860 ) ;
#621 = CARTESIAN_POINT ( 'NONE',  ( -0.1574803149606300301, -1.644192913385826404, -0.06523048226347956391 ) ) ;
#622 = CYLINDRICAL_SURFACE ( 'NONE', #2285, 0.1574803149606297803 ) ;
#623 = EDGE_CURVE ( 'NONE', #39641, #16593, #45079, .T. ) ;
#624 = AXIS2_PLACEMENT_3D ( 'NONE', #17137, #13103, #2740 ) ;
#625 = ORIENTED_EDGE ( 'NONE', *, *, #36161, .F. ) ;
#626 = PLANE ( 'NONE',  #7602 ) ;
#627 = CARTESIAN_POINT ( 'NONE',  ( -0.6971942568897637749, 2.189545951927499583E-17, 0.2386811023084413619 ) ) ;
#628 = ORIENTED_EDGE ( 'NONE', *, *, #34521, .T. ) ;
#629 = CARTESIAN_POINT ( 'NONE',  ( -0.06523048226347956391, 0.05364173239099160467, -0.1574803149606300301 ) ) ;
#630 = CARTESIAN_POINT ( 'NONE',  ( -0.9500414927467378812, 0.1787899950787401604, 1.643700787347811998 ) ) ;
#631 = CARTESIAN_POINT ( 'NONE',  ( -1.054774247047244540, -0.07405724077823318263, 0.8858267715997791836 ) ) ;
#632 = ADVANCED_FACE ( 'NONE', ( #9505 ), #7574, .F. ) ;
#633 = CARTESIAN_POINT ( 'NONE',  ( -1.054774247047244096, 0.000000000000000000, 1.124507873961984261 ) ) ;
#634 = CONICAL_SURFACE ( 'NONE', #29824, 0.09842519685039370636, 0.9599310885968824758 ) ;
#635 = CARTESIAN_POINT ( 'NONE',  ( -0.6971942568897637749, 2.189545951927499583E-17, 0.4798228345919055560 ) ) ;
#636 = ( BOUNDED_CURVE ( )  B_SPLINE_CURVE ( 2, ( #787, #43949, #8233, #4159, #30330, #26237, #30102, #40335, #15451 ),
 .UNSPECIFIED., .F., .T. ) 
 B_SPLINE_CURVE_WITH_KNOTS ( ( 3, 2, 2, 2, 3 ),
 ( 0.8100000000000000533, 0.8125000000000000000, 0.8149999999999999467, 0.8175000000000000044, 0.8199999999999999512 ),
 .UNSPECIFIED. ) 
 CURVE ( )  GEOMETRIC_REPRESENTATION_ITEM ( )  RATIONAL_B_SPLINE_CURVE ( ( 1.000000000000000000, 0.9238795325112899581, 1.000000000000000000, 0.9238795325112869605, 1.000000000000000000, 0.9238795325112869605, 1.000000000000000000, 0.9238795325112829637, 1.000000000000000000 ) ) 
 REPRESENTATION_ITEM ( '' )  ) ;
#637 = CARTESIAN_POINT ( 'NONE',  ( 0.1377952755905511861, 0.1574803149606299191, -0.7057086614173228023 ) ) ;
#638 = CARTESIAN_POINT ( 'NONE',  ( -0.6971942568897648851, -0.07405724077823297447, 1.978346456639149320 ) ) ;
#639 = CARTESIAN_POINT ( 'NONE',  ( 0.8759842519685039353, 0.000000000000000000, 4.498031496062992574 ) ) ;
#640 = CARTESIAN_POINT ( 'NONE',  ( 1.054774247047244540, 0.07405724077823318263, 0.06397637789899228433 ) ) ;
#641 = CARTESIAN_POINT ( 'NONE',  ( -0.3094175599200251203, 0.02245875686878780197, -0.7098059324661201153 ) ) ;
#642 = CARTESIAN_POINT ( 'NONE',  ( -0.07405724077823318263, -0.5995334170481365632, 0.1787899950787401604 ) ) ;
#643 = FACE_OUTER_BOUND ( 'NONE', #21090, .T. ) ;
#644 = CARTESIAN_POINT ( 'NONE',  ( -1.033464566929133799, 0.000000000000000000, 1.781496062992125928 ) ) ;
#645 = DIRECTION ( 'NONE',  ( 0.000000000000000000, 1.000000000000000000, 0.000000000000000000 ) ) ;
#646 = CARTESIAN_POINT ( 'NONE',  ( -0.6971942568897626646, 0.07405724077823318263, 0.3149606298674962890 ) ) ;
#647 = CARTESIAN_POINT ( 'NONE',  ( -0.1264236179284866091, -1.743726330433962524, 0.1264236179284866091 ) ) ;
#648 = ORIENTED_EDGE ( 'NONE', *, *, #45925, .T. ) ;
#649 = VERTEX_POINT ( 'NONE', #2063 ) ;
#650 = CARTESIAN_POINT ( 'NONE',  ( -0.8759842519685039353, 0.1787899950787401882, 1.375492125930488196 ) ) ;
#651 = ORIENTED_EDGE ( 'NONE', *, *, #28716, .F. ) ;
#652 = CARTESIAN_POINT ( 'NONE',  ( 0.1264236179284866091, -1.289862204670645607, 0.1264236179284866091 ) ) ;
#653 = ADVANCED_FACE ( 'NONE', ( #8542 ), #25959, .T. ) ;
#654 = CARTESIAN_POINT ( 'NONE',  ( 0.07405724077823318263, -1.587598425143086800, -0.1787899950787401604 ) ) ;
#655 = AXIS2_PLACEMENT_3D ( 'NONE', #20910, #35078, #2226 ) ;
#656 = DIRECTION ( 'NONE',  ( -1.000000000000000000, 0.000000000000000000, 7.051687499798870116E-15 ) ) ;
#657 = DIRECTION ( 'NONE',  ( 0.000000000000000000, 0.000000000000000000, -1.000000000000000000 ) ) ;
#658 = CARTESIAN_POINT ( 'NONE',  ( 1.033464566929133799, 0.000000000000000000, 0.4330708660342047489 ) ) ;
#659 = CARTESIAN_POINT ( 'NONE',  ( -0.7646288533564489232, 0.1113553986120547346, 1.038385826664126155 ) ) ;
#660 = AXIS2_PLACEMENT_3D ( 'NONE', #17202, #46421, #20086 ) ;
#661 = CARTESIAN_POINT ( 'NONE',  ( 1.054774247047244540, 0.07405724077823318263, 0.6200787401037165525 ) ) ;
#662 = CARTESIAN_POINT ( 'NONE',  ( -0.8107537697050254399, -0.1574803149606297803, 1.483759842412158747 ) ) ;
#663 = CARTESIAN_POINT ( 'NONE',  ( -0.1113553986120547346, -0.2293307086614173318, -0.1113553986120547346 ) ) ;
#664 = DIRECTION ( 'NONE',  ( 0.000000000000000000, 0.000000000000000000, 1.000000000000000000 ) ) ;
#665 = ORIENTED_EDGE ( 'NONE', *, *, #6692, .F. ) ;
#666 = CARTESIAN_POINT ( 'NONE',  ( -0.1427036564498907201, -0.09517011092317628762, -0.1080556551396093801 ) ) ;
#667 = CARTESIAN_POINT ( 'NONE',  ( -0.6971942568897637749, 2.189545951927499583E-17, 0.9522637794737952577 ) ) ;
#668 = CARTESIAN_POINT ( 'NONE',  ( 0.7185039370078746268, 0.06523048226347956391, 0.9325787401574799906 ) ) ;
#669 = VECTOR ( 'NONE', #5870, 39.37007874015748143 ) ;
#670 = DIRECTION ( 'NONE',  ( 1.000000000000000000, 0.000000000000000000, -0.000000000000000000 ) ) ;
#671 = CARTESIAN_POINT ( 'NONE',  ( 0.3425196850393700809, 4.616380251121755931E-17, 0.000000000000000000 ) ) ;
#672 = CARTESIAN_POINT ( 'NONE',  ( -0.1690815567638284667, -0.08955967048287666321, -0.02567216645670302583 ) ) ;
#673 = ORIENTED_EDGE ( 'NONE', *, *, #33785, .F. ) ;
#674 = AXIS2_PLACEMENT_3D ( 'NONE', #44945, #41576, #5660 ) ;
#675 = DIRECTION ( 'NONE',  ( 0.000000000000000000, 1.000000000000000000, 0.000000000000000000 ) ) ;
#676 = CARTESIAN_POINT ( 'NONE',  ( -0.2802144182493691016, 0.1328525842424023995, 0.9782784368059546098 ) ) ;
#677 = CARTESIAN_POINT ( 'NONE',  ( 1.002407869896990045, 0.1264236179284866091, 0.6963582676627716461 ) ) ;
#678 = ORIENTED_EDGE ( 'NONE', *, *, #20325, .T. ) ;
#679 = FACE_OUTER_BOUND ( 'NONE', #47350, .T. ) ;
#680 = CARTESIAN_POINT ( 'NONE',  ( 1.033464566929136907, -0.06523048226347749612, 1.385334645669292541 ) ) ;
#681 = CARTESIAN_POINT ( 'NONE',  ( -0.07405724077823318263, -1.607283464513165949, 0.1787899950787401604 ) ) ;
#682 = CARTESIAN_POINT ( 'NONE',  ( -0.1787899950787401604, -0.7952755904974174728, -0.07405724077823318263 ) ) ;
#683 = CARTESIAN_POINT ( 'NONE',  ( -0.1113553986120547346, -1.252952755905511806, -0.1113553986120547346 ) ) ;
#684 = CARTESIAN_POINT ( 'NONE',  ( 0.8759842519685039353, -0.1574803149606299191, 1.131889763672000004 ) ) ;
#685 = CARTESIAN_POINT ( 'NONE',  ( 0.2395294000716133853, 0.1968503937007874127, -1.181102362204724310 ) ) ;
#686 = EDGE_CURVE ( 'NONE', #23816, #39475, #34433, .T. ) ;
#687 = CARTESIAN_POINT ( 'NONE',  ( -0.9500414927467378812, -0.1787899950787401604, 0.4872047243556847929 ) ) ;
#688 = ORIENTED_EDGE ( 'NONE', *, *, #3021, .T. ) ;
#689 = ORIENTED_EDGE ( 'NONE', *, *, #1840, .T. ) ;
#690 = CARTESIAN_POINT ( 'NONE',  ( -0.8019270111902717657, -0.1787899950787401604, 1.825787401521040243 ) ) ;
#691 = CARTESIAN_POINT ( 'NONE',  ( 0.9500414927467378812, -0.1787899950787401604, 1.673228346402929834 ) ) ;
#692 = CARTESIAN_POINT ( 'NONE',  ( 0.8759842519685039353, 0.000000000000000000, 4.498031496062992574 ) ) ;
#693 = CARTESIAN_POINT ( 'NONE',  ( 0.8019270111902717657, 0.1787899950787401604, 0.2362204723871814960 ) ) ;
#694 = CARTESIAN_POINT ( 'NONE',  ( -1.054774247047244540, -0.07405724077823318263, 1.200787401521039355 ) ) ;
#695 = CARTESIAN_POINT ( 'NONE',  ( -0.9500414927467378812, -0.1787899950787401604, 0.05905511805647267048 ) ) ;
#696 = AXIS2_PLACEMENT_3D ( 'NONE', #10327, #39534, #28800 ) ;
#697 = CARTESIAN_POINT ( 'NONE',  ( 0.1377952755905511861, 0.000000000000000000, -0.1712639279175142137 ) ) ;
#698 = CARTESIAN_POINT ( 'NONE',  ( -1.054774247047244540, 0.07405724077823318263, 1.604330708607653921 ) ) ;
#699 = CARTESIAN_POINT ( 'NONE',  ( -0.9412147342319837628, -0.1574803149606297803, 1.843011810916095561 ) ) ;
#700 = ORIENTED_EDGE ( 'NONE', *, *, #15382, .F. ) ;
#701 = CARTESIAN_POINT ( 'NONE',  ( -0.7646288533564489232, -0.1113553986120547346, 1.609251968503937036 ) ) ;
#702 = CARTESIAN_POINT ( 'NONE',  ( 0.1925235483212767162, -0.3878655561654137385, -1.008977380820889946 ) ) ;
#703 = CARTESIAN_POINT ( 'NONE',  ( 0.6971942568897648851, 0.07405724077823318263, 1.579724409395055318 ) ) ;
#704 = CARTESIAN_POINT ( 'NONE',  ( -0.1919739359782932919, -0.09842519685039370636, 0.1351110688617698785 ) ) ;
#705 = DIRECTION ( 'NONE',  ( 0.000000000000000000, -1.000000000000000000, 0.000000000000000000 ) ) ;
#706 = CARTESIAN_POINT ( 'NONE',  ( 1.033464566929134687, 0.06523048226347956391, 0.2780511809948353341 ) ) ;
#707 = EDGE_LOOP ( 'NONE', ( #31570, #13137, #36634, #7165 ) ) ;
#708 = B_SPLINE_CURVE_WITH_KNOTS ( 'NONE', 3,
 ( #28141, #32202, #2466, #28627, #9914, #21640, #28865, #17093, #7013, #18040, #32685, #28374, #6538, #32454, #24524, #2926, #25235, #7260, #47275, #6296, #31966, #42943, #39824, #46788, #14454, #29112, #43665, #35327, #13976, #46551, #21152, #25494, #20919, #10153, #47031, #17804, #35559, #10873 ),
 .UNSPECIFIED., .F., .F.,
 ( 4, 2, 2, 2, 2, 2, 2, 2, 2, 2, 2, 2, 2, 2, 2, 2, 2, 2, 4 ),
 ( 0.000000000000000000, 0.0008476847199669468704, 0.001695369439933893741, 0.002543054159900840286, 0.003390738879867787482, 0.004238423599834733810, 0.005086108319801680572, 0.005933793039768628201, 0.006781477759735574963, 0.007205320119719049211, 0.007629162479702521725, 0.008476847199669457211, 0.009324531919636393565, 0.01017221663960332992, 0.01101990135957026627, 0.01186758607953720263, 0.01229142843952067167, 0.01271527079950414071, 0.01356295551947107707 ),
 .UNSPECIFIED. ) ;
#709 = CIRCLE ( 'NONE', #12248, 0.1968503937007874127 ) ;
#710 = ORIENTED_EDGE ( 'NONE', *, *, #12023, .T. ) ;
#711 = AXIS2_PLACEMENT_3D ( 'NONE', #7841, #43130, #8307 ) ;
#712 = VERTEX_POINT ( 'NONE', #45900 ) ;
#713 = B_SPLINE_CURVE_WITH_KNOTS ( 'NONE', 3,
 ( #38757, #41598, #38277, #27534 ),
 .UNSPECIFIED., .F., .F.,
 ( 4, 4 ),
 ( 0.000000000000000000, 1.000000000000000000 ),
 .UNSPECIFIED. ) ;
#714 = CARTESIAN_POINT ( 'NONE',  ( 0.1264236179284866091, -0.9256889763241890057, -0.1264236179284866091 ) ) ;
#715 = CARTESIAN_POINT ( 'NONE',  ( -0.07405724077823318263, -0.9921259841982054128, -0.1787899950787401604 ) ) ;
#716 = DIRECTION ( 'NONE',  ( 1.000000000000000000, -3.469446951953614978E-15, -1.144917494144692929E-16 ) ) ;
#717 = CARTESIAN_POINT ( 'NONE',  ( 0.8759842519685039353, 0.1787899950787401882, 1.803641732229700700 ) ) ;
#718 = CARTESIAN_POINT ( 'NONE',  ( 0.07444174185955065859, -0.3824256993468252430, 0.1797182628040039087 ) ) ;
#719 = CARTESIAN_POINT ( 'NONE',  ( -0.1574803149606297803, 0.09301181102362203468, 0.06523048226347956391 ) ) ;
#720 = CARTESIAN_POINT ( 'NONE',  ( 0.1787899950787401604, -0.02755905506434671789, 0.07405724077823318263 ) ) ;
#721 = CARTESIAN_POINT ( 'NONE',  ( -1.033464566929133799, 0.000000000000000000, 1.062992125876724314 ) ) ;
#722 = CARTESIAN_POINT ( 'NONE',  ( 0.6971942568897637749, 2.189545951927499583E-17, 0.7898622046706456068 ) ) ;
#723 = AXIS2_PLACEMENT_3D ( 'NONE', #34044, #1169, #31627 ) ;
#725 = CARTESIAN_POINT ( 'NONE',  ( 0.4934383202099732468, 0.08090551181102362266, 9.908067607274841931E-18 ) ) ;
#724 = DIRECTION ( 'NONE',  ( 0.000000000000000000, -1.000000000000000000, 0.000000000000000000 ) ) ;
#726 = CARTESIAN_POINT ( 'NONE',  ( 1.033464566929133799, 1.928577636452524610E-17, 4.498031496062992574 ) ) ;
#727 = CARTESIAN_POINT ( 'NONE',  ( 0.6971942568897648851, 0.07405724077823318263, 1.815944881835999558 ) ) ;
#728 = CARTESIAN_POINT ( 'NONE',  ( 0.8759842519685039353, -0.1574803149606299191, 1.879921259734992134 ) ) ;
#729 = EDGE_CURVE ( 'NONE', #7655, #31223, #13710, .T. ) ;
#730 = ADVANCED_FACE ( 'NONE', ( #7834 ), #25829, .F. ) ;
#731 = CARTESIAN_POINT ( 'NONE',  ( 0.8759842519685039353, -0.1574803149606299191, 0.1181102362204724532 ) ) ;
#732 = DIRECTION ( 'NONE',  ( 0.000000000000000000, -0.7880107536067199048, 0.6156614753256609562 ) ) ;
#733 = CARTESIAN_POINT ( 'NONE',  ( -0.07405724077823318263, -0.2342519684501733479, 0.1787899950787401604 ) ) ;
#734 = AXIS2_PLACEMENT_3D ( 'NONE', #37549, #13067, #42266 ) ;
#735 = CARTESIAN_POINT ( 'NONE',  ( -1.094772975963752103E-17, -1.270177165300566902, -0.1787899950787401882 ) ) ;
#736 = CARTESIAN_POINT ( 'NONE',  ( 1.002407869896990045, -0.1264236179284866091, 0.1796259841982051075 ) ) ;
#737 = CARTESIAN_POINT ( 'NONE',  ( 0.1642211665453957858, 0.08093770371294724264, -0.1401839329144623780 ) ) ;
#738 = ADVANCED_FACE ( 'NONE', ( #36391 ), #37067, .F. ) ;
#739 = CARTESIAN_POINT ( 'NONE',  ( -0.8759842519685039353, 0.1787899950787401882, 1.724901574749385880 ) ) ;
#740 = VERTEX_POINT ( 'NONE', #18615 ) ;
#741 = CARTESIAN_POINT ( 'NONE',  ( -0.9500414927467378812, 0.1787899950787401604, 1.333661417269071059 ) ) ;
#742 = FACE_OUTER_BOUND ( 'NONE', #45156, .T. ) ;
#743 = CARTESIAN_POINT ( 'NONE',  ( 1.054774247047244540, -0.07405724077823318263, 1.284448818843874740 ) ) ;
#744 = CARTESIAN_POINT ( 'NONE',  ( 0.1574803149606299191, -1.218503936900346529, -1.928577636452523993E-17 ) ) ;
#745 = CARTESIAN_POINT ( 'NONE',  ( -0.6971942568897648851, 0.07405724077823318263, 1.023622047190330342 ) ) ;
#746 = CARTESIAN_POINT ( 'NONE',  ( 0.01529509707327361516, -0.09839281432029055308, -0.1781982434423184380 ) ) ;
#747 = CARTESIAN_POINT ( 'NONE',  ( -1.181162989532618060E-16, -0.0009842519685041700977, -0.3937007874015748254 ) ) ;
#748 = CARTESIAN_POINT ( 'NONE',  ( 0.6971942568897637749, 2.189545951927499583E-17, 0.4010826771115905687 ) ) ;
#749 = CARTESIAN_POINT ( 'NONE',  ( -0.9500414927467377701, -0.1787899950787401604, 0.3690944881352128393 ) ) ;
#750 = CARTESIAN_POINT ( 'NONE',  ( -1.054774247047244540, -0.07405724077823318263, 0.8464566928596233275 ) ) ;
#751 = ORIENTED_EDGE ( 'NONE', *, *, #17520, .F. ) ;
#752 = VERTEX_POINT ( 'NONE', #29469 ) ;
#753 = EDGE_CURVE ( 'NONE', #41392, #4833, #15522, .T. ) ;
#754 = PRODUCT_DEFINITION ( 'UNKNOWN', '', #15557, #11115 ) ;
#755 = ORIENTED_EDGE ( 'NONE', *, *, #13172, .T. ) ;
#756 = CARTESIAN_POINT ( 'NONE',  ( -0.7646288533564489232, 0.1113553986120547346, 0.1033464566929133965 ) ) ;
#757 = FACE_OUTER_BOUND ( 'NONE', #34050, .T. ) ;
#758 = VERTEX_POINT ( 'NONE', #19081 ) ;
#759 = CARTESIAN_POINT ( 'NONE',  ( -0.9500414927467378812, -0.1787899950787401604, 0.8858267715997791836 ) ) ;
#760 = CARTESIAN_POINT ( 'NONE',  ( 0.5962569168439626477, -3.032960542342102697E-32, 0.09842519685039370636 ) ) ;
#761 = CARTESIAN_POINT ( 'NONE',  ( 1.033464566929133799, 0.000000000000000000, 0.3248031496062992463 ) ) ;
#762 = CARTESIAN_POINT ( 'NONE',  ( 0.1264236179284866091, -1.379553102087506256, 0.1264236179284866091 ) ) ;
#763 = VERTEX_POINT ( 'NONE', #18849 ) ;
#764 = PLANE ( 'NONE',  #10375 ) ;
#765 = CARTESIAN_POINT ( 'NONE',  ( -0.07405724077823318263, -0.4655511810485986057, 0.1787899950787401604 ) ) ;
#766 = DIRECTION ( 'NONE',  ( -1.000000000000000000, -0.000000000000000000, 0.000000000000000000 ) ) ;
#767 = ORIENTED_EDGE ( 'NONE', *, *, #22825, .T. ) ;
#768 = CARTESIAN_POINT ( 'NONE',  ( 0.8019270111902717657, -0.1787899950787401604, 1.269685039316314601 ) ) ;
#769 = AXIS2_PLACEMENT_3D ( 'NONE', #1035, #36541, #36769 ) ;
#770 = CARTESIAN_POINT ( 'NONE',  ( 1.033464566929134687, 0.06523048226347956391, 1.587106299212598604 ) ) ;
#771 = AXIS2_PLACEMENT_3D ( 'NONE', #44550, #8619, #18463 ) ;
#772 = CARTESIAN_POINT ( 'NONE',  ( -0.1574803149606299191, 1.928577636452524610E-17, -0.1966003937007873570 ) ) ;
#773 = CARTESIAN_POINT ( 'NONE',  ( 0.6971942568897626646, -0.07405724077823297447, 0.1230314960092287191 ) ) ;
#774 = CARTESIAN_POINT ( 'NONE',  ( -0.1787899950787401604, -1.740157480261197875, -0.07405724077823318263 ) ) ;
#775 = CARTESIAN_POINT ( 'NONE',  ( 0.1787899950787401604, -1.710629921206078041, -0.07405724077823318263 ) ) ;
#776 = DIRECTION ( 'NONE',  ( -0.5506710774114468299, 0.000000000000000000, 0.8347223277848248024 ) ) ;
#777 = EDGE_CURVE ( 'NONE', #24545, #4083, #7595, .T. ) ;
#778 = CARTESIAN_POINT ( 'NONE',  ( -0.1476377952755905387, -0.2274162997038010614, -0.9219983537151217323 ) ) ;
#779 = CARTESIAN_POINT ( 'NONE',  ( -1.054774247047244096, 0.000000000000000000, 0.6176181101824566033 ) ) ;
#780 = CARTESIAN_POINT ( 'NONE',  ( 0.7185039370078746268, -0.06523048226347956391, 0.2977362203649139283 ) ) ;
#781 = CARTESIAN_POINT ( 'NONE',  ( 3.301370929368692659E-17, -1.447878455252336716, 0.1797182628040039365 ) ) ;
#782 = CARTESIAN_POINT ( 'NONE',  ( -0.3551574803149606385, -0.2559055118110236116, 0.000000000000000000 ) ) ;
#783 = CARTESIAN_POINT ( 'NONE',  ( 0.5839895013123354017, 4.616380251121755931E-17, 0.000000000000000000 ) ) ;
#784 = CARTESIAN_POINT ( 'NONE',  ( 0.6971942568897648851, 0.07405724077823318263, 1.422244094434426120 ) ) ;
#785 = CARTESIAN_POINT ( 'NONE',  ( 0.9500414927467377701, 0.1787899950787401604, 1.761811023568284229 ) ) ;
#786 = EDGE_CURVE ( 'NONE', #42479, #21227, #41230, .T. ) ;
#787 = CARTESIAN_POINT ( 'NONE',  ( -0.7185039370078739607, 1.928577636452523993E-17, 1.633858267609007875 ) ) ;
#788 = CARTESIAN_POINT ( 'NONE',  ( -0.8107537697050254399, 0.1574803149606300301, 1.518208661417322913 ) ) ;
#789 = DIRECTION ( 'NONE',  ( -0.000000000000000000, 1.000000000000000000, -0.000000000000000000 ) ) ;
#791 = CARTESIAN_POINT ( 'NONE',  ( 0.1264236179284866091, 0.1274606299750234428, 0.1264236179284866091 ) ) ;
#790 = CARTESIAN_POINT ( 'NONE',  ( -0.1574803149606297803, -0.8026574802074324388, 0.06523048226347956391 ) ) ;
#792 = CARTESIAN_POINT ( 'NONE',  ( -1.033464566929133799, 0.000000000000000000, 1.220472440837354400 ) ) ;
#793 = CARTESIAN_POINT ( 'NONE',  ( 0.7495606340400177148, 0.1264236179284866091, 0.3518700786863940833 ) ) ;
#794 = CARTESIAN_POINT ( 'NONE',  ( -0.8107537697050254399, -0.1574803149606297803, 1.719980314853102321 ) ) ;
#795 = LINE ( 'NONE', #37964, #37288 ) ;
#796 = CARTESIAN_POINT ( 'NONE',  ( -0.8107537697050254399, 0.1574803149606300301, 0.7701771653543307838 ) ) ;
#797 = CARTESIAN_POINT ( 'NONE',  ( -0.8019270111902717657, 0.1787899950787401604, 1.373031496009229135 ) ) ;
#798 = CARTESIAN_POINT ( 'NONE',  ( 1.033464566929134687, 0.06523048226347956391, 0.7111220471365681250 ) ) ;
#799 = VERTEX_POINT ( 'NONE', #25603 ) ;
#800 = CARTESIAN_POINT ( 'NONE',  ( -0.7646288533564489232, 0.1113553986120547346, 1.756889763779527547 ) ) ;
#801 = CARTESIAN_POINT ( 'NONE',  ( 0.1627249056762492263, 1.099487083487564965, -0.04739565599252298922 ) ) ;
#802 = VERTEX_POINT ( 'NONE', #40870 ) ;
#803 = CARTESIAN_POINT ( 'NONE',  ( 0.1797182628040039365, -0.02071310092162823024, -2.200913952912460540E-17 ) ) ;
#804 = CARTESIAN_POINT ( 'NONE',  ( 0.1264236179284866091, -1.289862204670645607, 0.1264236179284866091 ) ) ;
#805 = AXIS2_PLACEMENT_3D ( 'NONE', #34915, #9017, #31319 ) ;
#806 = CARTESIAN_POINT ( 'NONE',  ( -1.033464566929134687, 0.06523048226347956391, 1.104822834538142340 ) ) ;
#807 = CARTESIAN_POINT ( 'NONE',  ( 0.8019270111902717657, 0.1787899950787401604, 1.530511810969859443 ) ) ;
#808 = FACE_OUTER_BOUND ( 'NONE', #31107, .T. ) ;
#810 = CARTESIAN_POINT ( 'NONE',  ( 0.9873396505805591694, 0.1113553986120547346, 1.904527559055118280 ) ) ;
#809 = CARTESIAN_POINT ( 'NONE',  ( 0.1574803149606300023, 0.06415291647593675262, -0.1630605872086743346 ) ) ;
#811 = CARTESIAN_POINT ( 'NONE',  ( -1.033464566929134687, -0.06523048226347956391, 0.5093503935932608417 ) ) ;
#813 = AXIS2_PLACEMENT_3D ( 'NONE', #15403, #44359, #29363 ) ;
#812 = CARTESIAN_POINT ( 'NONE',  ( -1.094772975963752103E-17, -0.1678149605761578844, -0.1787899950787401882 ) ) ;
#814 = CARTESIAN_POINT ( 'NONE',  ( 0.8759842519685039353, 0.1574803149606299191, 1.309055118002708573 ) ) ;
#815 = VERTEX_POINT ( 'NONE', #4446 ) ;
#816 = CARTESIAN_POINT ( 'NONE',  ( -0.1574803149606299191, 0.06415291647593700242, -0.1630605872086743624 ) ) ;
#817 = CIRCLE ( 'NONE', #6954, 0.1624015748031501782 ) ;
#818 = CARTESIAN_POINT ( 'NONE',  ( 0.9500414927467377701, -0.1787899950787401604, 0.9251968503399373711 ) ) ;
#819 = CARTESIAN_POINT ( 'NONE',  ( -0.8759842519685039353, 0.1787899950787401882, 1.528051181048598384 ) ) ;
#820 = CARTESIAN_POINT ( 'NONE',  ( -0.06523048226347956391, -0.08907480304207930633, 0.1574803149606297803 ) ) ;
#821 = CARTESIAN_POINT ( 'NONE',  ( -0.8759842519685039353, -0.1787899950787401882, 1.237696850339937038 ) ) ;
#822 = ORIENTED_EDGE ( 'NONE', *, *, #16650, .T. ) ;
#823 = CARTESIAN_POINT ( 'NONE',  ( -1.054774247047244540, 0.07405724077823318263, 0.3444881889226146243 ) ) ;
#824 = CARTESIAN_POINT ( 'NONE',  ( 1.033464566929133799, 1.928577636452524610E-17, 4.498031496062992574 ) ) ;
#825 = DIRECTION ( 'NONE',  ( 1.822029033848725028E-16, 0.000000000000000000, 1.000000000000000000 ) ) ;
#826 = CARTESIAN_POINT ( 'NONE',  ( -0.1264236179284866091, -0.9267971965756948149, -0.1264236179284866091 ) ) ;
#827 = VERTEX_POINT ( 'NONE', #3995 ) ;
#828 = CARTESIAN_POINT ( 'NONE',  ( -0.07405724077823318263, 0.08562992131360593062, 0.1787899950787401604 ) ) ;
#829 = VERTEX_POINT ( 'NONE', #7135 ) ;
#830 = ORIENTED_EDGE ( 'NONE', *, *, #34012, .T. ) ;
#831 = DIRECTION ( 'NONE',  ( 1.000000000000000000, 0.000000000000000000, -1.822029033848725275E-16 ) ) ;
#832 = CYLINDRICAL_SURFACE ( 'NONE', #40644, 0.09842519685039370636 ) ;
#833 = CARTESIAN_POINT ( 'NONE',  ( 0.7185039370078714072, 0.06523048226347728795, 1.828248031388537198 ) ) ;
#834 = VECTOR ( 'NONE', #5877, 39.37007874015748143 ) ;
#835 = AXIS2_PLACEMENT_3D ( 'NONE', #29189, #20976, #40131 ) ;
#836 = CARTESIAN_POINT ( 'NONE',  ( 0.07405724077823318263, -0.5442913385289138706, 0.1787899950787401604 ) ) ;
#837 = EDGE_CURVE ( 'NONE', #23661, #38468, #18158, .T. ) ;
#838 = CIRCLE ( 'NONE', #29214, 0.09842519685039370636 ) ;
#839 = ADVANCED_FACE ( 'NONE', ( #47393 ), #6059, .T. ) ;
#840 = CARTESIAN_POINT ( 'NONE',  ( -0.7495606340400177148, 0.1264236179284866091, 0.1993110235682838682 ) ) ;
#841 = CARTESIAN_POINT ( 'NONE',  ( -1.033464566929134687, 0.06523048226347956391, 0.9571850393700783721 ) ) ;
#842 = DIRECTION ( 'NONE',  ( 0.7986355100472960489, 0.000000000000000000, -0.6018150231520441595 ) ) ;
#843 = CARTESIAN_POINT ( 'NONE',  ( 0.1270800023317771588, -1.039413888323202695, -0.1270800023317771588 ) ) ;
#844 = CARTESIAN_POINT ( 'NONE',  ( 0.1731942250296887864, 0.1299212598425197318, 0.03910837931845940335 ) ) ;
#845 = CARTESIAN_POINT ( 'NONE',  ( -1.033464566929134687, 0.06523048226347956391, 1.459153543199560144 ) ) ;
#846 = CARTESIAN_POINT ( 'NONE',  ( 0.9500414927467378812, -0.1787899950787401604, 0.8858267715997791836 ) ) ;
#847 = EDGE_CURVE ( 'NONE', #7195, #1272, #43787, .T. ) ;
#848 = ADVANCED_FACE ( 'NONE', ( #29928 ), #26313, .T. ) ;
#849 = CARTESIAN_POINT ( 'NONE',  ( 0.7185039370078737386, 0.06523048226348011902, 0.5290354329633389918 ) ) ;
#850 = CARTESIAN_POINT ( 'NONE',  ( 1.033464566929134687, 0.06523048226347956391, 1.350885826771654363 ) ) ;
#852 = DIRECTION ( 'NONE',  ( 1.822029033848725028E-16, 0.000000000000000000, 1.000000000000000000 ) ) ;
#851 = CARTESIAN_POINT ( 'NONE',  ( 0.7154772363482215791, 0.03734124201450598340, 1.982562885371508488 ) ) ;
#853 = CYLINDRICAL_SURFACE ( 'NONE', #4451, 0.1574803149606299191 ) ;
#854 = CARTESIAN_POINT ( 'NONE',  ( 0.1113553986120547346, -0.7017716534357795188, -0.1113553986120547346 ) ) ;
#856 = CARTESIAN_POINT ( 'NONE',  ( 0.1608809465420318885, 0.1607368455565694743, -0.002813831971227472289 ) ) ;
#855 = CARTESIAN_POINT ( 'NONE',  ( 0.8019270111902716547, -0.1787899950787401604, 0.8366141731745828647 ) ) ;
#857 = CARTESIAN_POINT ( 'NONE',  ( 1.054774247047244540, -0.07405724077823318263, 1.756889763725764553 ) ) ;
#858 = CARTESIAN_POINT ( 'NONE',  ( -0.1787899950787401882, -0.7091535432533228045, 0.000000000000000000 ) ) ;
#859 = CARTESIAN_POINT ( 'NONE',  ( -0.1673228346456692994, -0.9654866319674424435, -1.480939111413832610 ) ) ;
#860 = VERTEX_POINT ( 'NONE', #44704 ) ;
#861 = CARTESIAN_POINT ( 'NONE',  ( 1.033464566929134687, 0.06523048226347956391, 1.075295275590550048 ) ) ;
#862 = CARTESIAN_POINT ( 'NONE',  ( 0.2395294000716133853, 0.000000000000000000, 0.8759842519685039353 ) ) ;
#863 = CARTESIAN_POINT ( 'NONE',  ( -0.7185039370078746268, -0.06523048226347956391, 0.1008858266641264878 ) ) ;
#864 = CARTESIAN_POINT ( 'NONE',  ( 0.8019270111902717657, -0.1787899950787401604, 1.112204724355684959 ) ) ;
#865 = CARTESIAN_POINT ( 'NONE',  ( -0.1377952755905511861, 0.1574803149606320007, -0.8070866141732283561 ) ) ;
#866 = CARTESIAN_POINT ( 'NONE',  ( -0.06523048226347956391, -1.634350393700787496, 0.1574803149606297803 ) ) ;
#867 = CARTESIAN_POINT ( 'NONE',  ( 0.5555748031496089423, 0.3833307086614172743, 0.7480314960629921295 ) ) ;
#868 = CONICAL_SURFACE ( 'NONE', #23889, 0.08090551181102362266, 0.9599310885968742602 ) ;
#869 = EDGE_LOOP ( 'NONE', ( #32440, #31673, #26613, #9439 ) ) ;
#870 = DIRECTION ( 'NONE',  ( 1.000000000000000000, 0.000000000000000000, 0.000000000000000000 ) ) ;
#871 = CARTESIAN_POINT ( 'NONE',  ( -0.8759842519685039353, -0.1787899950787401882, 0.2485236219934806867 ) ) ;
#872 = CARTESIAN_POINT ( 'NONE',  ( -0.7185039370078739607, 1.928577636452523993E-17, 0.6200787401574803237 ) ) ;
#873 = VERTEX_POINT ( 'NONE', #29699 ) ;
#874 = CARTESIAN_POINT ( 'NONE',  ( -1.094772975963752103E-17, -1.471948818843874074, -0.1787899950787401882 ) ) ;
#875 = AXIS2_PLACEMENT_3D ( 'NONE', #18309, #25267, #40324 ) ;
#876 = VECTOR ( 'NONE', #10922, 39.37007874015748143 ) ;
#877 = CARTESIAN_POINT ( 'NONE',  ( -0.6971942568897637749, 2.189545951927499583E-17, 0.9473425196312755814 ) ) ;
#878 = CARTESIAN_POINT ( 'NONE',  ( -0.7495606340400177148, -0.1264236179284866091, 0.4847440944344252323 ) ) ;
#879 = DIRECTION ( 'NONE',  ( 1.822029033848725028E-16, 0.000000000000000000, 1.000000000000000000 ) ) ;
#880 = CARTESIAN_POINT ( 'NONE',  ( 0.1594617487093260011, 0.04893254358519821129, 0.1404675734346356175 ) ) ;
#881 = CARTESIAN_POINT ( 'NONE',  ( 0.1574803149606299746, 0.6241017553149654784, 0.3240160679609099259 ) ) ;
#882 = CARTESIAN_POINT ( 'NONE',  ( 0.5057057357416000487, 4.766607801171850497E-17, 0.000000000000000000 ) ) ;
#883 = CARTESIAN_POINT ( 'NONE',  ( 0.07405724077823318263, -0.5798483776780570809, -0.1787899950787401604 ) ) ;
#884 = CARTESIAN_POINT ( 'NONE',  ( 0.02785187604205846545, -0.08955996554169548540, 0.2176922158899677329 ) ) ;
#885 = CARTESIAN_POINT ( 'NONE',  ( 0.8759842519685039353, 0.000000000000000000, 4.498031496062992574 ) ) ;
#886 = CYLINDRICAL_SURFACE ( 'NONE', #39424, 0.1574803149606299191 ) ;
#887 = CARTESIAN_POINT ( 'NONE',  ( 0.2559052507921502073, -0.04868370062670082654, -0.03721911624063468926 ) ) ;
#888 = CARTESIAN_POINT ( 'NONE',  ( -0.6971942568897626646, -0.07405724077823297447, 0.3198818897100162983 ) ) ;
#889 = CARTESIAN_POINT ( 'NONE',  ( 0.8070866141732283561, -0.0009842519685049383633, 0.8559055118110230342 ) ) ;
#890 = ORIENTED_EDGE ( 'NONE', *, *, #19656, .T. ) ;
#891 = CARTESIAN_POINT ( 'NONE',  ( 0.2471922904502826812, -0.03219022224904106305, 0.1427165354330708902 ) ) ;
#892 = ORIENTED_EDGE ( 'NONE', *, *, #28438, .F. ) ;
#893 = CARTESIAN_POINT ( 'NONE',  ( -0.6971942568897637749, 2.189545951927499583E-17, 1.464074803095842370 ) ) ;
#894 = VERTEX_POINT ( 'NONE', #40177 ) ;
#895 = CIRCLE ( 'NONE', #27749, 0.4724409448818896462 ) ;
#896 = CARTESIAN_POINT ( 'NONE',  ( 0.1264236179284866091, -1.358759842465921297, -0.1264236179284866091 ) ) ;
#897 = CARTESIAN_POINT ( 'NONE',  ( 0.07405724077823318263, -1.523622047190330564, 0.1787899950787401604 ) ) ;
#898 = ( BOUNDED_CURVE ( )  B_SPLINE_CURVE ( 2, ( #25785, #18803, #810, #11640, #18103, #40125, #10697, #22157, #37254 ),
 .UNSPECIFIED., .F., .T. ) 
 B_SPLINE_CURVE_WITH_KNOTS ( ( 3, 2, 2, 2, 3 ),
 ( 0.9599999999999999645, 0.9625000000000000222, 0.9649999999999999689, 0.9675000000000000266, 0.9699999999999999734 ),
 .UNSPECIFIED. ) 
 CURVE ( )  GEOMETRIC_REPRESENTATION_ITEM ( )  RATIONAL_B_SPLINE_CURVE ( ( 1.000000000000000000, 0.9238795325112869605, 1.000000000000000000, 0.9238795325112869605, 1.000000000000000000, 0.9238795325112869605, 1.000000000000000000, 0.9238795325112869605, 1.000000000000000000 ) ) 
 REPRESENTATION_ITEM ( '' )  ) ;
#899 = EDGE_CURVE ( 'NONE', #2549, #11279, #11446, .T. ) ;
#900 = AXIS2_PLACEMENT_3D ( 'NONE', #38784, #2573, #27326 ) ;
#901 = CARTESIAN_POINT ( 'NONE',  ( 1.033464566929133799, 0.000000000000000000, 0.2066929133858267931 ) ) ;
#902 = CARTESIAN_POINT ( 'NONE',  ( 0.1555687797274980522, 0.09281549603114055969, 0.1148293963254592570 ) ) ;
#903 = DIRECTION ( 'NONE',  ( 1.822029033848725028E-16, 0.000000000000000000, 1.000000000000000000 ) ) ;
#904 = CARTESIAN_POINT ( 'NONE',  ( -0.9873396505805591694, 0.1113553986120547346, 1.107283464459401623 ) ) ;
#905 = CARTESIAN_POINT ( 'NONE',  ( 0.7495606340400177148, 0.1264236179284866091, 0.5142716534895434011 ) ) ;
#907 = DIRECTION ( 'NONE',  ( 0.8191520442889899112, -0.4519843998600478474, 0.3531289150159199197 ) ) ;
#906 = CARTESIAN_POINT ( 'NONE',  ( 0.1574803149606300301, -0.2416338582677168279, -0.06523048226347956391 ) ) ;
#908 = VECTOR ( 'NONE', #12308, 39.37007874015748143 ) ;
#909 = CARTESIAN_POINT ( 'NONE',  ( 0.7646288533564489232, -0.1113553986120547346, 1.953740157372787500 ) ) ;
#910 = ORIENTED_EDGE ( 'NONE', *, *, #13077, .T. ) ;
#911 = EDGE_CURVE ( 'NONE', #13663, #9851, #36610, .T. ) ;
#912 = CARTESIAN_POINT ( 'NONE',  ( 0.7185039370078739607, 1.928577636452523993E-17, 0.9744094488188976833 ) ) ;
#913 = CARTESIAN_POINT ( 'NONE',  ( -0.8759842519685039353, -0.1787899950787401882, 1.040846456639149764 ) ) ;
#914 = CARTESIAN_POINT ( 'NONE',  ( 0.9873396505805591694, 0.1113553986120547346, 0.9596456692913386544 ) ) ;
#915 = CARTESIAN_POINT ( 'NONE',  ( 0.1641609177537618758, -0.08086997970899940935, -0.1400748931816458154 ) ) ;
#916 = CARTESIAN_POINT ( 'NONE',  ( 0.5839895013123354017, 0.08090551181102362266, 9.908067607274841931E-18 ) ) ;
#917 = CARTESIAN_POINT ( 'NONE',  ( 0.1113553986120547346, -0.5442913384751496553, -0.1113553986120547346 ) ) ;
#918 = CARTESIAN_POINT ( 'NONE',  ( 1.351300519334104211E-16, 0.000000000000000000, 0.2942913385826777528 ) ) ;
#919 = CARTESIAN_POINT ( 'NONE',  ( -0.1547363509471673670, -0.08956143428533665241, 0.05872201630027999719 ) ) ;
#920 = ORIENTED_EDGE ( 'NONE', *, *, #33954, .T. ) ;
#921 = AXIS2_PLACEMENT_3D ( 'NONE', #33497, #29461, #21978 ) ;
#922 = CARTESIAN_POINT ( 'NONE',  ( 0.1645805171892397445, -0.08212597262126515585, -0.1405696315964612142 ) ) ;
#923 = ORIENTED_EDGE ( 'NONE', *, *, #43493, .T. ) ;
#924 = DIRECTION ( 'NONE',  ( 0.000000000000000000, -0.7880107536067184615, 0.6156614753256628436 ) ) ;
#925 = CARTESIAN_POINT ( 'NONE',  ( 2.892866454678787531E-17, -0.01771653543307086590, 0.1574803149606299191 ) ) ;
#926 = CARTESIAN_POINT ( 'NONE',  ( 0.1787899950787401604, -1.558070866087969630, 0.07405724077823318263 ) ) ;
#927 = CARTESIAN_POINT ( 'NONE',  ( -0.07405724077823318263, -0.9576771653005667906, -0.1787899950787401604 ) ) ;
#928 = CARTESIAN_POINT ( 'NONE',  ( 0.06523048226347956391, -1.142224409448818534, -0.1574803149606300301 ) ) ;
#930 = ( BOUNDED_CURVE ( )  B_SPLINE_CURVE ( 2, ( #28913, #10684, #25292, #39880, #29164, #18090, #14741, #32736, #25546 ),
 .UNSPECIFIED., .F., .T. ) 
 B_SPLINE_CURVE_WITH_KNOTS ( ( 3, 2, 2, 2, 3 ),
 ( 0.6099999999999999867, 0.6125000000000000444, 0.6149999999999999911, 0.6175000000000000488, 0.6199999999999999956 ),
 .UNSPECIFIED. ) 
 CURVE ( )  GEOMETRIC_REPRESENTATION_ITEM ( )  RATIONAL_B_SPLINE_CURVE ( ( 1.000000000000000000, 0.9238795325112869605, 1.000000000000000000, 0.9238795325112869605, 1.000000000000000000, 0.9238795325112869605, 1.000000000000000000, 0.9238795325112869605, 1.000000000000000000 ) ) 
 REPRESENTATION_ITEM ( '' )  ) ;
#929 = CARTESIAN_POINT ( 'NONE',  ( 1.033464566929134687, -0.06523048226347956391, 1.099901574695622886 ) ) ;
#931 = ORIENTED_EDGE ( 'NONE', *, *, #9551, .T. ) ;
#932 = ORIENTED_EDGE ( 'NONE', *, *, #10243, .T. ) ;
#933 = CARTESIAN_POINT ( 'NONE',  ( -0.6971942568897648851, 0.07405724077823318263, 1.815944881835999558 ) ) ;
#934 = CARTESIAN_POINT ( 'NONE',  ( 0.8759842519685039353, -0.1787899950787401882, 1.710137795221826851 ) ) ;
#935 = CARTESIAN_POINT ( 'NONE',  ( -0.7495606340400177148, -0.1264236179284866091, 0.9178149605761574126 ) ) ;
#936 = CARTESIAN_POINT ( 'NONE',  ( -0.05425864391566919548, -0.2641663005107283690, -0.3070225280280975411 ) ) ;
#937 = CARTESIAN_POINT ( 'NONE',  ( 0.7495606340400177148, 0.1264236179284866091, 0.2780511810485988278 ) ) ;
#938 = CARTESIAN_POINT ( 'NONE',  ( -1.054774247047244540, -0.07405724077823318263, 1.437007873961985371 ) ) ;
#939 = CARTESIAN_POINT ( 'NONE',  ( 1.229559056033039366E-16, -0.3937007874015746034, 0.3937007874015748254 ) ) ;
#940 = CARTESIAN_POINT ( 'NONE',  ( -0.8759842519685039353, -0.1787899950787401882, 1.311515747977732405 ) ) ;
#941 = CARTESIAN_POINT ( 'NONE',  ( -0.7495606340400177148, 0.1264236179284866091, 0.7849409448281259305 ) ) ;
#942 = CARTESIAN_POINT ( 'NONE',  ( -0.8019270111902717657, -0.1787899950787401604, 0.1328740156942679607 ) ) ;
#943 = DIRECTION ( 'NONE',  ( -0.8191520442889950182, 0.4519843998600410750, -0.3531289150159169776 ) ) ;
#944 = CARTESIAN_POINT ( 'NONE',  ( -0.6971942568897648851, -0.07405724077823297447, 1.624015747977732849 ) ) ;
#945 = CARTESIAN_POINT ( 'NONE',  ( -1.054774247047244540, 0.07405724077823318263, 0.06889763774151215492 ) ) ;
#946 = CARTESIAN_POINT ( 'NONE',  ( -1.033464566929134687, -0.06523048226347956391, 1.582185039370078927 ) ) ;
#947 = CARTESIAN_POINT ( 'NONE',  ( 1.033464566929133799, 0.000000000000000000, 0.7185039370078739607 ) ) ;
#948 = CARTESIAN_POINT ( 'NONE',  ( 0.8019270111902716547, 0.1787899950787401604, 1.574803149552536530 ) ) ;
#949 = CARTESIAN_POINT ( 'NONE',  ( -0.1522652282534474322, -0.09842519685039370636, -0.2000201865208625918 ) ) ;
#950 = LINE ( 'NONE', #23504, #21058 ) ;
#951 = CARTESIAN_POINT ( 'NONE',  ( -0.2559127773736598055, 0.03449262457614915567, -0.3136310232799333630 ) ) ;
#952 = ORIENTED_EDGE ( 'NONE', *, *, #13535, .F. ) ;
#953 = CIRCLE ( 'NONE', #27790, 0.1377952755905511861 ) ;
#954 = VERTEX_POINT ( 'NONE', #1342 ) ;
#955 = VERTEX_POINT ( 'NONE', #12405 ) ;
#956 = CARTESIAN_POINT ( 'NONE',  ( -1.054774247047244096, 0.000000000000000000, 1.168799212544661348 ) ) ;
#957 = ORIENTED_EDGE ( 'NONE', *, *, #27196, .F. ) ;
#958 = CARTESIAN_POINT ( 'NONE',  ( 0.1264236179284866091, -0.8174212597887557941, 0.1264236179284866091 ) ) ;
#959 = CARTESIAN_POINT ( 'NONE',  ( -0.1787899950787401882, -1.063484251914740275, 0.000000000000000000 ) ) ;
#960 = EDGE_CURVE ( 'NONE', #2888, #5683, #38491, .T. ) ;
#961 = CARTESIAN_POINT ( 'NONE',  ( 0.000000000000000000, 0.000000000000000000, 0.000000000000000000 ) ) ;
#962 = CARTESIAN_POINT ( 'NONE',  ( 0.7646288533564489232, -0.1113553986120547346, 0.3100393700787401619 ) ) ;
#963 = CARTESIAN_POINT ( 'NONE',  ( -0.1797182628040039087, -0.3922682190318645401, 0.07444174185955065859 ) ) ;
#964 = DIRECTION ( 'NONE',  ( -1.000000000000000000, 0.000000000000000000, 0.000000000000000000 ) ) ;
#965 = CARTESIAN_POINT ( 'NONE',  ( 0.1264236179284866091, -0.1382874015210397711, -0.1264236179284866091 ) ) ;
#966 = EDGE_CURVE ( 'NONE', #3817, #13566, #5414, .T. ) ;
#967 = CARTESIAN_POINT ( 'NONE',  ( 0.8019270111902717657, 0.1787899950787401604, 0.7824803149068669805 ) ) ;
#969 = CARTESIAN_POINT ( 'NONE',  ( 1.033464566929134687, -0.06523048226347956391, 1.139271653435781184 ) ) ;
#968 = CARTESIAN_POINT ( 'NONE',  ( 0.4632545931758527691, -0.08090551181102362266, 0.000000000000000000 ) ) ;
#970 = LINE ( 'NONE', #33143, #21182 ) ;
#971 = DIRECTION ( 'NONE',  ( -1.000000000000000000, 0.000000000000000000, 0.000000000000000000 ) ) ;
#972 = CARTESIAN_POINT ( 'NONE',  ( 0.6971942568897637749, 2.189545951927499583E-17, 1.818405511757259729 ) ) ;
#973 = AXIS2_PLACEMENT_3D ( 'NONE', #44511, #22847, #34131 ) ;
#974 = CIRCLE ( 'NONE', #3327, 0.5708661417322835607 ) ;
#975 = CARTESIAN_POINT ( 'NONE',  ( 0.7646288533564489232, -0.1113553986120547346, 0.1525590551181102428 ) ) ;
#976 = LINE ( 'NONE', #7946, #6077 ) ;
#977 = CARTESIAN_POINT ( 'NONE',  ( 0.1787899950787401604, -0.4557086613635593086, -0.07405724077823318263 ) ) ;
#978 = PLANE ( 'NONE',  #26301 ) ;
#979 = CARTESIAN_POINT ( 'NONE',  ( -0.1787899950787401882, -1.299704724355684959, 0.000000000000000000 ) ) ;
#980 = CARTESIAN_POINT ( 'NONE',  ( 0.6971942568897637749, 2.189545951927499583E-17, 0.2042322834108035723 ) ) ;
#981 = DIRECTION ( 'NONE',  ( 1.000000000000000000, 0.000000000000000000, -1.822029033848725275E-16 ) ) ;
#982 = CARTESIAN_POINT ( 'NONE',  ( -0.6971942568897648851, 0.07405724077823318263, 1.692913385773008539 ) ) ;
#983 = ORIENTED_EDGE ( 'NONE', *, *, #25046, .T. ) ;
#984 = CARTESIAN_POINT ( 'NONE',  ( -0.8019270111902717657, -0.1787899950787401604, 1.313976377898992132 ) ) ;
#985 = CARTESIAN_POINT ( 'NONE',  ( -0.9412147342319837628, 0.1574803149606300301, 0.3321850393700786497 ) ) ;
#986 = CARTESIAN_POINT ( 'NONE',  ( 1.002407869896990045, 0.1264236179284866091, 1.291830708607653477 ) ) ;
#987 = CARTESIAN_POINT ( 'NONE',  ( -0.06523048226347956391, -1.166830708553891371, -0.1574803149606300301 ) ) ;
#988 = CARTESIAN_POINT ( 'NONE',  ( -1.002407869896990045, -0.1264236179284866091, 0.5339566928596221063 ) ) ;
#989 = CARTESIAN_POINT ( 'NONE',  ( 1.054774247047244540, -0.07405724077823318263, 1.909448818843873186 ) ) ;
#990 = CARTESIAN_POINT ( 'NONE',  ( -1.002407869896990045, -0.1264236179284866091, 1.001476377898992132 ) ) ;
#991 = DIRECTION ( 'NONE',  ( 0.000000000000000000, 1.000000000000000000, 0.000000000000000000 ) ) ;
#992 = CARTESIAN_POINT ( 'NONE',  ( -0.05462378473120000494, -0.09842519705081047288, -0.1712222294880737516 ) ) ;
#993 = CARTESIAN_POINT ( 'NONE',  ( 0.7646288533564489232, 0.1113553986120547346, 1.205708661417322913 ) ) ;
#994 = CARTESIAN_POINT ( 'NONE',  ( 1.054774247047244096, 0.000000000000000000, 0.4995078739619842612 ) ) ;
#995 = CARTESIAN_POINT ( 'NONE',  ( -1.054774247047244540, 0.07405724077823318263, 0.3395669290800949480 ) ) ;
#996 = CARTESIAN_POINT ( 'NONE',  ( -0.9500414927467378812, -0.1787899950787401604, 0.8415354330171019859 ) ) ;
#997 = ORIENTED_EDGE ( 'NONE', *, *, #17149, .F. ) ;
#998 = EDGE_CURVE ( 'NONE', #41311, #3412, #6808, .T. ) ;
#999 = CYLINDRICAL_SURFACE ( 'NONE', #43573, 0.1574803149606299191 ) ;
#1000 = VERTEX_POINT ( 'NONE', #42057 ) ;
#1001 = CARTESIAN_POINT ( 'NONE',  ( 0.8759842519685039353, -0.1787899950787401882, 0.9227362204186770889 ) ) ;
#1002 = CARTESIAN_POINT ( 'NONE',  ( -0.9873396505805591694, -0.1113553986120547346, 0.1230314960629921295 ) ) ;
#1003 = DIRECTION ( 'NONE',  ( 1.000000000000000000, 0.000000000000000000, 0.000000000000000000 ) ) ;
#1004 = VERTEX_POINT ( 'NONE', #1577 ) ;
#1005 = DIRECTION ( 'NONE',  ( 0.000000000000000000, 1.000000000000000000, 0.000000000000000000 ) ) ;
#1006 = CARTESIAN_POINT ( 'NONE',  ( -0.9500414927467378812, 0.1787899950787401604, 0.9005905511273389896 ) ) ;
#1007 = CARTESIAN_POINT ( 'NONE',  ( 0.1637370714319413278, -0.1604746447930043285, 0.002359686926949007297 ) ) ;
#1008 = DIRECTION ( 'NONE',  ( 0.000000000000000000, 0.000000000000000000, -1.000000000000000000 ) ) ;
#1009 = CARTESIAN_POINT ( 'NONE',  ( -0.1787899950787401882, -1.473057039095379883, 0.000000000000000000 ) ) ;
#1010 = ORIENTED_EDGE ( 'NONE', *, *, #106, .T. ) ;
#1011 = CARTESIAN_POINT ( 'NONE',  ( 0.1264236179284866091, -0.3695866141194649179, -0.1264236179284866091 ) ) ;
#1012 = EDGE_CURVE ( 'NONE', #35936, #46714, #2060, .T. ) ;
#1013 = CYLINDRICAL_SURFACE ( 'NONE', #11687, 0.1574803149606297803 ) ;
#1014 = ORIENTED_EDGE ( 'NONE', *, *, #13181, .F. ) ;
#1015 = CARTESIAN_POINT ( 'NONE',  ( -0.8107537697050254399, 0.1574803149606300301, 0.8390748030420788206 ) ) ;
#1016 = CARTESIAN_POINT ( 'NONE',  ( 0.3161444924769291065, 1.914733266569315084, -0.6843357808987579061 ) ) ;
#1017 = EDGE_CURVE ( 'NONE', #32743, #28431, #42763, .T. ) ;
#1018 = CARTESIAN_POINT ( 'NONE',  ( 1.054774247047244540, 0.07405724077823318263, 1.638779527505292988 ) ) ;
#1019 = CARTESIAN_POINT ( 'NONE',  ( 0.9500414927467378812, 0.1787899950787401604, 0.2263779527021421711 ) ) ;
#1020 = AXIS2_PLACEMENT_3D ( 'NONE', #961, #29788, #33603 ) ;
#1021 = CARTESIAN_POINT ( 'NONE',  ( 0.1264236179284866091, -1.722933070812378009, 0.1264236179284866091 ) ) ;
#1022 = CARTESIAN_POINT ( 'NONE',  ( -0.1787899950787401882, -1.772145669237574994, 0.000000000000000000 ) ) ;
#1023 = CARTESIAN_POINT ( 'NONE',  ( -0.7185039370078714072, 0.06523048226347728795, 1.749507873908221045 ) ) ;
#1024 = ORIENTED_EDGE ( 'NONE', *, *, #5865, .T. ) ;
#1025 = ADVANCED_FACE ( 'NONE', ( #22928 ), #19568, .F. ) ;
#1026 = EDGE_CURVE ( 'NONE', #14442, #15222, #38252, .T. ) ;
#1027 = CARTESIAN_POINT ( 'NONE',  ( -1.002407869896990045, -0.1264236179284866091, 0.6520669290800944484 ) ) ;
#1029 = LENGTH_MEASURE_WITH_UNIT ( LENGTH_MEASURE( 0.02539999999999999897 ), #18778 ) ;
#1028 = CARTESIAN_POINT ( 'NONE',  ( -0.1113553986120547346, -0.7312992125984252301, 0.1113553986120547346 ) ) ;
#1030 = CARTESIAN_POINT ( 'NONE',  ( -0.1797182628040039087, -1.342071368638164675, -0.07444174185955065859 ) ) ;
#1031 = DIRECTION ( 'NONE',  ( 0.000000000000000000, -1.000000000000000000, 0.000000000000000000 ) ) ;
#1032 = CARTESIAN_POINT ( 'NONE',  ( 0.8759842519685039353, 0.1787899950787401882, 1.296751968450173154 ) ) ;
#1033 = CARTESIAN_POINT ( 'NONE',  ( 0.6971942568897648851, -0.07405724077823297447, 1.894685039316315489 ) ) ;
#1034 = CARTESIAN_POINT ( 'NONE',  ( 0.9500414927467377701, 0.1787899950787401604, 0.2657480314422993595 ) ) ;
#1035 = CARTESIAN_POINT ( 'NONE',  ( -0.8759842519685039353, 0.000000000000000000, 0.000000000000000000 ) ) ;
#1036 = AXIS2_PLACEMENT_3D ( 'NONE', #44067, #21807, #46957 ) ;
#1037 = CARTESIAN_POINT ( 'NONE',  ( -0.1184675242425147629, -0.09842519685039370636, 1.713085361781126803 ) ) ;
#1038 = CARTESIAN_POINT ( 'NONE',  ( 0.2362204724409448509, 0.000000000000000000, 0.9891732283464566011 ) ) ;
#1039 = CARTESIAN_POINT ( 'NONE',  ( -0.07405724077823318263, 0.1200787402112438867, 0.1787899950787401604 ) ) ;
#1040 = CARTESIAN_POINT ( 'NONE',  ( -0.8107537697050254399, 0.1574803149606300301, 1.232775590443654812 ) ) ;
#1041 = CARTESIAN_POINT ( 'NONE',  ( 0.8759842519685039353, -0.1787899950787401882, 0.3666338582139531677 ) ) ;
#1042 = SHAPE_REPRESENTATION ( 'ISO 10513 M8 Lock Nut', ( #20860 ), #17833 ) ;
#1043 = CARTESIAN_POINT ( 'NONE',  ( -0.7185039370078739607, 1.928577636452523993E-17, 1.250000000000000000 ) ) ;
#1044 = CARTESIAN_POINT ( 'NONE',  ( 1.739107093083948175E-16, 0.1574803149606340824, 0.2923228346456709370 ) ) ;
#1045 = CYLINDRICAL_SURFACE ( 'NONE', #11555, 0.009842519685039274532 ) ;
#1046 = CARTESIAN_POINT ( 'NONE',  ( -0.9500414927467378812, -0.1787899950787401604, 1.313976377898992132 ) ) ;
#1047 = CARTESIAN_POINT ( 'NONE',  ( 0.8759842519685039353, 0.1574803149606299191, 0.6791338581601890079 ) ) ;
#1048 = ORIENTED_EDGE ( 'NONE', *, *, #37438, .T. ) ;
#1049 = CARTESIAN_POINT ( 'NONE',  ( 0.4208034506101054895, 1.205361022782824954E-17, -0.09842519685039370636 ) ) ;
#1050 = ORIENTED_EDGE ( 'NONE', *, *, #18714, .T. ) ;
#1051 = CARTESIAN_POINT ( 'NONE',  ( 0.1797182628040039365, -0.09945325840194331468, -2.200913952912460540E-17 ) ) ;
#1052 = CARTESIAN_POINT ( 'NONE',  ( -0.1787899950787401604, -1.267716535379307619, -0.07405724077823318263 ) ) ;
#1053 = CARTESIAN_POINT ( 'NONE',  ( -1.181162989532618060E-16, 0.000000000000000000, -0.2942913385826778083 ) ) ;
#1054 = CARTESIAN_POINT ( 'NONE',  ( 0.9500414927467378812, 0.1787899950787401604, 1.604330708607653921 ) ) ;
#1055 = CARTESIAN_POINT ( 'NONE',  ( -1.033464566929133799, 0.000000000000000000, 1.190944881889763884 ) ) ;
#1056 = CARTESIAN_POINT ( 'NONE',  ( -0.7646288533564489232, 0.1113553986120547346, 1.156496062884598608 ) ) ;
#1058 = CARTESIAN_POINT ( 'NONE',  ( 0.8759842519685039353, 0.1574803149606299191, 1.948818897637795367 ) ) ;
#1057 = CARTESIAN_POINT ( 'NONE',  ( -0.9412147342319837628, 0.1574803149606300301, 0.9227362204724415262 ) ) ;
#1059 = CARTESIAN_POINT ( 'NONE',  ( 0.7185039370078760701, 0.06523048226348075740, 0.3715551180027094613 ) ) ;
#1060 = ORIENTED_EDGE ( 'NONE', *, *, #16668, .T. ) ;
#1061 = CARTESIAN_POINT ( 'NONE',  ( -0.06648378651140092466, -0.08350519546677943883, -0.2470477387548498660 ) ) ;
#1062 = CIRCLE ( 'NONE', #4901, 0.2471922904502826812 ) ;
#1063 = CARTESIAN_POINT ( 'NONE',  ( 0.7495606340400177148, -0.1264236179284866091, 0.6815944881352126172 ) ) ;
#1064 = CARTESIAN_POINT ( 'NONE',  ( -1.002407869896990045, 0.1264236179284866091, 1.523129921206078707 ) ) ;
#1065 = CARTESIAN_POINT ( 'NONE',  ( -0.06523048226347956391, 0.01427165365083412490, -0.1574803149606300301 ) ) ;
#1066 = CARTESIAN_POINT ( 'NONE',  ( -1.054774247047244540, -0.07405724077823318263, 1.323818897584032817 ) ) ;
#1067 = VERTEX_POINT ( 'NONE', #37789 ) ;
#1068 = DIRECTION ( 'NONE',  ( 1.541976423090495042E-15, 0.4344452574044150306, -0.9006982393225888561 ) ) ;
#1069 = CARTESIAN_POINT ( 'NONE',  ( -0.8019270111902717657, -0.1787899950787401604, 0.3297244093950552069 ) ) ;
#1070 = DIRECTION ( 'NONE',  ( 0.000000000000000000, 0.000000000000000000, -1.000000000000000000 ) ) ;
#1071 = CARTESIAN_POINT ( 'NONE',  ( -1.094772975963752103E-17, -0.9317184564182144912, -0.1787899950787401882 ) ) ;
#1072 = VERTEX_POINT ( 'NONE', #4941 ) ;
#1073 = CARTESIAN_POINT ( 'NONE',  ( -0.07405724077823318263, 0.006889763833291078637, 0.1787899950787401604 ) ) ;
#1074 = EDGE_LOOP ( 'NONE', ( #27931, #18471, #35975, #5562 ) ) ;
#1075 = EDGE_CURVE ( 'NONE', #17962, #28784, #34674, .T. ) ;
#1076 = ORIENTED_EDGE ( 'NONE', *, *, #45990, .T. ) ;
#1077 = CARTESIAN_POINT ( 'NONE',  ( 0.3649999999999999911, -0.1870078740157480324, 0.000000000000000000 ) ) ;
#1078 = DIRECTION ( 'NONE',  ( 0.000000000000000000, 0.000000000000000000, 1.000000000000000000 ) ) ;
#1079 = DIRECTION ( 'NONE',  ( 3.469446951953613794E-15, 1.000000000000000000, 1.020425574103997713E-16 ) ) ;
#1080 = CONICAL_SURFACE ( 'NONE', #330, 0.09842519685039310962, 0.7853981633972314524 ) ;
#1081 = CARTESIAN_POINT ( 'NONE',  ( 3.284318927891251994E-17, -0.5467519684501732646, 0.1787899950787401882 ) ) ;
#1082 = EDGE_CURVE ( 'NONE', #21217, #8391, #23509, .T. ) ;
#1083 = CARTESIAN_POINT ( 'NONE',  ( -1.033464566929134687, 0.06523048226347956391, 0.8390748031496061410 ) ) ;
#1084 = DIRECTION ( 'NONE',  ( 1.822029033848725028E-16, 0.000000000000000000, 1.000000000000000000 ) ) ;
#1085 = CARTESIAN_POINT ( 'NONE',  ( 0.1377952755905511861, 0.000000000000000000, -0.2886241641379866385 ) ) ;
#1086 = CARTESIAN_POINT ( 'NONE',  ( 3.301370929368692659E-17, -0.9360674316302894926, 0.1797182628040039365 ) ) ;
#1087 = CARTESIAN_POINT ( 'NONE',  ( 0.2397010884053811242, 4.466152701071653354E-17, 0.000000000000000000 ) ) ;
#1088 = CARTESIAN_POINT ( 'NONE',  ( -0.8759842519685039353, -0.1574803149606299191, 1.564960629813732185 ) ) ;
#1089 = AXIS2_PLACEMENT_3D ( 'NONE', #19982, #5124, #34384 ) ;
#1090 = CARTESIAN_POINT ( 'NONE',  ( 1.002407869896990045, 0.1264236179284866091, 0.8587598424659212970 ) ) ;
#1091 = CARTESIAN_POINT ( 'NONE',  ( 1.002407869896990045, 0.1264236179284866091, 1.405019684985606476 ) ) ;
#1092 = CARTESIAN_POINT ( 'NONE',  ( -0.7185039370078739607, 1.928577636452523993E-17, 0.4625984251968504046 ) ) ;
#1093 = CARTESIAN_POINT ( 'NONE',  ( 0.8107537697050253289, 0.1574803149606300301, 1.636318897637794700 ) ) ;
#1095 = CARTESIAN_POINT ( 'NONE',  ( -0.2341188618557034362, -0.1603256443476437643, -0.2993662881635553719 ) ) ;
#1094 = CARTESIAN_POINT ( 'NONE',  ( 0.7117081823007622710, -0.03022371456366571355, 1.983825291605011643 ) ) ;
#1096 = CARTESIAN_POINT ( 'NONE',  ( 0.1574803149606300023, -0.4008464425712924273, -0.9238935802775078976 ) ) ;
#1097 = CARTESIAN_POINT ( 'NONE',  ( -0.1787899950787401604, 0.08070866147108628208, 0.07405724077823318263 ) ) ;
#1098 = DIRECTION ( 'NONE',  ( 0.000000000000000000, -1.000000000000000000, 0.000000000000000000 ) ) ;
#1100 = CARTESIAN_POINT ( 'NONE',  ( -0.9873396505805591694, -0.1113553986120547346, 1.422244094488188892 ) ) ;
#1099 = CARTESIAN_POINT ( 'NONE',  ( 0.8759842519685039353, 0.1787899950787401882, 0.8981299212060788184 ) ) ;
#1101 = CARTESIAN_POINT ( 'NONE',  ( 1.054774247047244096, 0.000000000000000000, 1.838090551127338657 ) ) ;
#1102 = CARTESIAN_POINT ( 'NONE',  ( 3.284318927891251994E-17, -0.7780511810485984947, 0.1787899950787401882 ) ) ;
#1103 = DIRECTION ( 'NONE',  ( -0.8191520442889914655, 0.000000000000000000, -0.5735764363510464925 ) ) ;
#1104 = ORIENTED_EDGE ( 'NONE', *, *, #45815, .T. ) ;
#1105 = CARTESIAN_POINT ( 'NONE',  ( 0.7646288533564489232, 0.1113553986120547346, 1.087598425196850460 ) ) ;
#1106 = CARTESIAN_POINT ( 'NONE',  ( -0.1113553986120547346, -1.715551180994834723, -0.1113553986120547346 ) ) ;
#1107 = CARTESIAN_POINT ( 'NONE',  ( -0.9873396505805591694, -0.1113553986120547346, 0.07381889753026830980 ) ) ;
#1108 = CARTESIAN_POINT ( 'NONE',  ( 0.6971942568897637749, 2.189545951927499583E-17, 1.065452755851747924 ) ) ;
#1109 = CARTESIAN_POINT ( 'NONE',  ( 0.06523048226347956391, -1.654035433070866423, -0.1574803149606300301 ) ) ;
#1110 = DIRECTION ( 'NONE',  ( -1.144917494144692682E-16, -2.347476851301873745E-33, -1.000000000000000000 ) ) ;
#1111 = ORIENTED_EDGE ( 'NONE', *, *, #15990, .F. ) ;
#1113 = CYLINDRICAL_SURFACE ( 'NONE', #14538, 0.1574803149606299191 ) ;
#1112 = AXIS2_PLACEMENT_3D ( 'NONE', #692, #36914, #11285 ) ;
#1114 = CARTESIAN_POINT ( 'NONE',  ( -1.054774247047244096, 0.000000000000000000, 0.2977362204186775885 ) ) ;
#1115 = CARTESIAN_POINT ( 'NONE',  ( 0.1787899950787401604, 0.09547244099864542199, -0.07405724077823318263 ) ) ;
#1116 = CARTESIAN_POINT ( 'NONE',  ( -1.094772975963752103E-17, -1.511318897584031484, -0.1787899950787401882 ) ) ;
#1117 = AXIS2_PLACEMENT_3D ( 'NONE', #18428, #1630, #34961 ) ;
#1118 = AXIS2_PLACEMENT_3D ( 'NONE', #47069, #18320, #21680 ) ;
#1119 = CARTESIAN_POINT ( 'NONE',  ( -0.9500414927467378812, -0.1787899950787401604, 1.865157480261195877 ) ) ;
#1120 = ADVANCED_FACE ( 'NONE', ( #44191 ), #22642, .F. ) ;
#1121 = CARTESIAN_POINT ( 'NONE',  ( -0.9500414927467378812, 0.1787899950787401604, 1.131889763725763665 ) ) ;
#1122 = CARTESIAN_POINT ( 'NONE',  ( -0.9500414927467378812, 0.1787899950787401604, 0.5856299212060785964 ) ) ;
#1123 = EDGE_CURVE ( 'NONE', #29994, #13605, #35169, .T. ) ;
#1124 = CARTESIAN_POINT ( 'NONE',  ( -0.8107537697050234415, -0.1574803149606297803, 0.1058070865066461363 ) ) ;
#1125 = DIRECTION ( 'NONE',  ( -1.000000000000000000, 0.000000000000000000, 0.000000000000000000 ) ) ;
#1126 = CARTESIAN_POINT ( 'NONE',  ( -1.033464566929134687, 0.06523048226347956391, 0.3174212597349925224 ) ) ;
#1127 = DIRECTION ( 'NONE',  ( 0.000000000000000000, -0.2126700594527834443, 0.9771240687918547607 ) ) ;
#1128 = CARTESIAN_POINT ( 'NONE',  ( -0.07405724077823318263, -0.5601633383079792639, 0.1787899950787401604 ) ) ;
#1129 = CARTESIAN_POINT ( 'NONE',  ( -0.2359654055811763462, -0.08955966323838543408, 0.02109953285558708452 ) ) ;
#1130 = FACE_OUTER_BOUND ( 'NONE', #21280, .T. ) ;
#1131 = CARTESIAN_POINT ( 'NONE',  ( 1.033464566929133799, 0.000000000000000000, 1.938976377952756014 ) ) ;
#1132 = EDGE_CURVE ( 'NONE', #37374, #5152, #28405, .T. ) ;
#1133 = CARTESIAN_POINT ( 'NONE',  ( 0.000000000000000000, 0.09842519685039370636, 0.000000000000000000 ) ) ;
#1134 = CARTESIAN_POINT ( 'NONE',  ( -0.6971942568897626646, -0.07405724077823297447, 0.5167322834108034613 ) ) ;
#1135 = CARTESIAN_POINT ( 'NONE',  ( 3.284318927891251994E-17, -1.778175149331602256, 0.1787899950787401882 ) ) ;
#1136 = CARTESIAN_POINT ( 'NONE',  ( 0.5415383587465882886, 4.466152701071653354E-17, 0.000000000000000000 ) ) ;
#1137 = CARTESIAN_POINT ( 'NONE',  ( -0.6971942568897648851, -0.07405724077823297447, 1.505905511757261062 ) ) ;
#1138 = CARTESIAN_POINT ( 'NONE',  ( -0.1787899950787401604, -1.341535433017102541, 0.07405724077823318263 ) ) ;
#1139 = CARTESIAN_POINT ( 'NONE',  ( 3.284318927891251994E-17, -1.486712598371433103, 0.1787899950787401882 ) ) ;
#1140 = CARTESIAN_POINT ( 'NONE',  ( -0.3161444924769509779, 1.205832402325951680, -1.129708666049261900 ) ) ;
#1141 = CARTESIAN_POINT ( 'NONE',  ( 0.9873396505805591694, 0.1113553986120547346, 0.4478346456692913202 ) ) ;
#1142 = AXIS2_PLACEMENT_3D ( 'NONE', #179, #21291, #43334 ) ;
#1143 = DIRECTION ( 'NONE',  ( 0.000000000000000000, -1.000000000000000000, 0.000000000000000000 ) ) ;
#1144 = CARTESIAN_POINT ( 'NONE',  ( -0.7185039370078739607, 1.928577636452523993E-17, 1.082677165246803241 ) ) ;
#1145 = CARTESIAN_POINT ( 'NONE',  ( 0.6971942568897637749, 2.189545951927499583E-17, 0.5585629920722204877 ) ) ;
#1147 = CARTESIAN_POINT ( 'NONE',  ( 0.7646288533564489232, -0.1113553986120547346, 1.756889763671999782 ) ) ;
#1146 = CARTESIAN_POINT ( 'NONE',  ( -0.06523048226347956391, -0.2317913385826771144, -0.1574803149606300301 ) ) ;
#1148 = VECTOR ( 'NONE', #44501, 39.37007874015748143 ) ;
#1149 = PRESENTATION_LAYER_ASSIGNMENT (  '', '', ( #25641 ) ) ;
#1150 = CARTESIAN_POINT ( 'NONE',  ( 0.7646288533564489232, 0.1113553986120547346, 1.983267716427905558 ) ) ;
#1151 = EDGE_LOOP ( 'NONE', ( #21562, #26634, #30176, #184 ) ) ;
#1152 = CARTESIAN_POINT ( 'NONE',  ( -0.1545411696117860445, -0.09842519685039370636, -0.08990488994085453489 ) ) ;
#1153 = CARTESIAN_POINT ( 'NONE',  ( -0.8759842519685039353, 0.1787899950787401882, 1.099901574749385880 ) ) ;
#1154 = CARTESIAN_POINT ( 'NONE',  ( 0.7185039370078739607, 1.928577636452523993E-17, 0.9744094488188976833 ) ) ;
#1155 = CYLINDRICAL_SURFACE ( 'NONE', #17449, 0.1574803149606299191 ) ;
#1156 = CARTESIAN_POINT ( 'NONE',  ( -0.06523048226347956391, -0.5369094487113711400, -0.1574803149606300301 ) ) ;
#1157 = CARTESIAN_POINT ( 'NONE',  ( -0.1807077244524717130, -0.08350519546717886932, 0.1811005174367878168 ) ) ;
#1158 = CARTESIAN_POINT ( 'NONE',  ( 1.033464566929133799, 0.000000000000000000, 0.5905511809948347235 ) ) ;
#1159 = CARTESIAN_POINT ( 'NONE',  ( -0.1009669065382620273, -0.08956173115452045752, 0.1239132365318445506 ) ) ;
#1160 = ORIENTED_EDGE ( 'NONE', *, *, #40875, .T. ) ;
#1161 = FACE_OUTER_BOUND ( 'NONE', #10540, .T. ) ;
#1162 = CARTESIAN_POINT ( 'NONE',  ( -0.8759842519685039353, 0.000000000000000000, 0.000000000000000000 ) ) ;
#1163 = CARTESIAN_POINT ( 'NONE',  ( 0.8759842519685039353, 0.1574803149606299191, 1.279527559055118280 ) ) ;
#1164 = CARTESIAN_POINT ( 'NONE',  ( -0.9412147342319837628, 0.1574803149606300301, 0.4404527557979849850 ) ) ;
#1165 = CARTESIAN_POINT ( 'NONE',  ( 0.07405724077823318263, -1.681102362150960650, 0.1787899950787401604 ) ) ;
#1166 = CARTESIAN_POINT ( 'NONE',  ( 0.1264236179284866091, -0.9256889763241890057, -0.1264236179284866091 ) ) ;
#1167 = CARTESIAN_POINT ( 'NONE',  ( 0.06523048226347956391, -1.220964566929134687, -0.1574803149606300301 ) ) ;
#1168 = CARTESIAN_POINT ( 'NONE',  ( 0.8107537697050253289, 0.1574803149606300301, 1.114665354223180804 ) ) ;
#1169 = DIRECTION ( 'NONE',  ( 0.000000000000000000, 0.000000000000000000, 1.000000000000000000 ) ) ;
#1170 = VERTEX_POINT ( 'NONE', #7542 ) ;
#1171 = ORIENTED_EDGE ( 'NONE', *, *, #34714, .F. ) ;
#1172 = CARTESIAN_POINT ( 'NONE',  ( -0.7495606340400177148, 0.1264236179284866091, 1.734744094434425232 ) ) ;
#1173 = CARTESIAN_POINT ( 'NONE',  ( 0.8759842519685039353, 0.1787899950787401882, 1.887303149552535420 ) ) ;
#1174 = ORIENTED_EDGE ( 'NONE', *, *, #26040, .T. ) ;
#1175 = CARTESIAN_POINT ( 'NONE',  ( 0.1113553986120547346, -1.371062992018456717, -0.1113553986120547346 ) ) ;
#1176 = LINE ( 'NONE', #15837, #24099 ) ;
#1177 = CARTESIAN_POINT ( 'NONE',  ( 1.054774247047244540, 0.07405724077823318263, 0.4625984251430869665 ) ) ;
#1178 = CARTESIAN_POINT ( 'NONE',  ( -1.002407869896990045, -0.1264236179284866091, 1.316437007820252081 ) ) ;
#1179 = CARTESIAN_POINT ( 'NONE',  ( 4.268512490100409430E-16, 0.2954942322624074524, -0.2921040715117803055 ) ) ;
#1180 = CARTESIAN_POINT ( 'NONE',  ( -0.9500414927467377701, -0.1787899950787401604, 1.235236220418678199 ) ) ;
#1181 = CARTESIAN_POINT ( 'NONE',  ( -0.8019270111902716547, 0.1787899950787401604, 0.7824803149068668695 ) ) ;
#1182 = CARTESIAN_POINT ( 'NONE',  ( -0.8759842519685039353, 0.1787899950787401882, 0.8981299212060788184 ) ) ;
#1183 = CARTESIAN_POINT ( 'NONE',  ( -1.054774247047244096, 0.000000000000000000, 0.1058070865604096300 ) ) ;
#1184 = ADVANCED_FACE ( 'NONE', ( #13915 ), #38972, .F. ) ;
#1185 = CARTESIAN_POINT ( 'NONE',  ( 0.05837987205262076124, 0.07899857248962811884, 0.2517274360213053175 ) ) ;
#1186 = CARTESIAN_POINT ( 'NONE',  ( -1.002407869896990045, -0.1264236179284866091, 1.715059055064346527 ) ) ;
#1187 = CARTESIAN_POINT ( 'NONE',  ( -0.9873396505805591694, -0.1113553986120547346, 2.002952755797984263 ) ) ;
#1188 = CARTESIAN_POINT ( 'NONE',  ( -0.8107537697050253289, 0.1574803149606300301, 1.557578740157481212 ) ) ;
#1189 = FACE_OUTER_BOUND ( 'NONE', #29440, .T. ) ;
#1190 = CARTESIAN_POINT ( 'NONE',  ( 1.002407869896990045, -0.1264236179284866091, 1.557578740103716441 ) ) ;
#1191 = CARTESIAN_POINT ( 'NONE',  ( 0.01579849016993808974, -0.09851382911741830839, 0.1545074369619750254 ) ) ;
#1192 = LINE ( 'NONE', #30474, #15730 ) ;
#1193 = EDGE_CURVE ( 'NONE', #46578, #5859, #11421, .T. ) ;
#1194 = CARTESIAN_POINT ( 'NONE',  ( -0.2559055118110236116, 0.000000000000000000, -0.3149606299212598381 ) ) ;
#1195 = AXIS2_PLACEMENT_3D ( 'NONE', #12675, #24382, #42094 ) ;
#1196 = AXIS2_PLACEMENT_3D ( 'NONE', #37509, #40374, #15249 ) ;
#1197 = ORIENTED_EDGE ( 'NONE', *, *, #33083, .F. ) ;
#1198 = EDGE_CURVE ( 'NONE', #23361, #25294, #34801, .T. ) ;
#1199 = ( BOUNDED_CURVE ( )  B_SPLINE_CURVE ( 2, ( #19737, #45366, #23812, #12580, #27208, #38431, #31258, #13505, #13971 ),
 .UNSPECIFIED., .F., .T. ) 
 B_SPLINE_CURVE_WITH_KNOTS ( ( 3, 2, 2, 2, 3 ),
 ( 0.9699999999999999734, 0.9725000000000000311, 0.9749999999999999778, 0.9775000000000000355, 0.9799999999999999822 ),
 .UNSPECIFIED. ) 
 CURVE ( )  GEOMETRIC_REPRESENTATION_ITEM ( )  RATIONAL_B_SPLINE_CURVE ( ( 1.000000000000000000, 0.9238795325112939549, 1.000000000000000000, 0.9238795325112869605, 1.000000000000000000, 0.9238795325112869605, 1.000000000000000000, 0.9238795325112869605, 1.000000000000000000 ) ) 
 REPRESENTATION_ITEM ( '' )  ) ;
#1200 = EDGE_LOOP ( 'NONE', ( #32073, #12303, #19442, #7739 ) ) ;
#1201 = CARTESIAN_POINT ( 'NONE',  ( 0.1787899950787401604, -0.8887795275052913224, -0.07405724077823318263 ) ) ;
#1202 = CARTESIAN_POINT ( 'NONE',  ( -0.1787899950787401604, -1.100393700733639069, 0.07405724077823318263 ) ) ;
#1203 = CARTESIAN_POINT ( 'NONE',  ( -0.8759842519685039353, 0.000000000000000000, 0.000000000000000000 ) ) ;
#1204 = CARTESIAN_POINT ( 'NONE',  ( 1.054774247047244096, 0.000000000000000000, 1.833169291284818758 ) ) ;
#1205 = CARTESIAN_POINT ( 'NONE',  ( 0.07444174185955046430, -0.4070319985594234580, -0.1797182628040039087 ) ) ;
#1206 = CARTESIAN_POINT ( 'NONE',  ( -0.1574803149606300301, -1.791830708553890261, -0.06523048226347956391 ) ) ;
#1207 = CARTESIAN_POINT ( 'NONE',  ( -0.1113553986120547346, 0.1643700787401574936, -0.1113553986120547346 ) ) ;
#1208 = CIRCLE ( 'NONE', #21080, 0.09842519685039370636 ) ;
#1209 = CARTESIAN_POINT ( 'NONE',  ( 0.7495606340400177148, 0.1264236179284866091, 0.8243110235682834519 ) ) ;
#1210 = ( BOUNDED_CURVE ( )  B_SPLINE_CURVE ( 2, ( #33886, #41720, #19230, #37208, #26923, #30523, #30070, #19702, #12061 ),
 .UNSPECIFIED., .F., .F. ) 
 B_SPLINE_CURVE_WITH_KNOTS ( ( 3, 2, 2, 2, 3 ),
 ( 0.1499999999999999944, 0.1524999999999999967, 0.1549999999999999989, 0.1575000000000000011, 0.1600000000000000033 ),
 .UNSPECIFIED. ) 
 CURVE ( )  GEOMETRIC_REPRESENTATION_ITEM ( )  RATIONAL_B_SPLINE_CURVE ( ( 1.000000000000000000, 0.9238795325112869605, 1.000000000000000000, 0.9238795325112869605, 1.000000000000000000, 0.9238795325112869605, 1.000000000000000000, 0.9238795325112869605, 1.000000000000000000 ) ) 
 REPRESENTATION_ITEM ( '' )  ) ;
#1212 = CARTESIAN_POINT ( 'NONE',  ( -0.7185039370078739607, 1.928577636452523993E-17, 1.525590551181102317 ) ) ;
#1211 = CARTESIAN_POINT ( 'NONE',  ( 0.05275478416826926559, 0.2650362434218154761, -0.05809220732314351876 ) ) ;
#1213 = CARTESIAN_POINT ( 'NONE',  ( 0.1574803149606299191, 0.4668427075568346574, -0.7022306805398661478 ) ) ;
#1214 = CARTESIAN_POINT ( 'NONE',  ( 1.002407869896990045, -0.1264236179284866091, 1.872539370024976391 ) ) ;
#1215 = CARTESIAN_POINT ( 'NONE',  ( 1.033464566929134687, -0.06523048226347956391, 0.1648622047244094890 ) ) ;
#1216 = LINE ( 'NONE', #15633, #39726 ) ;
#1217 = CARTESIAN_POINT ( 'NONE',  ( 3.284318927891251994E-17, -0.3892716534895436786, 0.1787899950787401882 ) ) ;
#1218 = CARTESIAN_POINT ( 'NONE',  ( 0.000000000000000000, 0.000000000000000000, -0.1712639279175142137 ) ) ;
#1219 = CARTESIAN_POINT ( 'NONE',  ( -0.07405724077823318263, -1.292322834591905778, 0.1787899950787401604 ) ) ;
#1220 = CARTESIAN_POINT ( 'NONE',  ( 1.054774247047244540, 0.07405724077823318263, 0.1870078739619845387 ) ) ;
#1221 = CARTESIAN_POINT ( 'NONE',  ( -0.8019270111902717657, 0.1787899950787401604, 1.806102362150961316 ) ) ;
#1222 = ORIENTED_EDGE ( 'NONE', *, *, #15124, .F. ) ;
#1223 = CARTESIAN_POINT ( 'NONE',  ( -0.6971942568897637749, 2.189545951927499583E-17, 1.227854330654897685 ) ) ;
#1224 = CARTESIAN_POINT ( 'NONE',  ( -0.7185039370078739607, 1.928577636452523993E-17, 1.328740157480315043 ) ) ;
#1225 = CARTESIAN_POINT ( 'NONE',  ( 0.8019270111902717657, 0.1787899950787401604, 1.299212598371432215 ) ) ;
#1226 = CARTESIAN_POINT ( 'NONE',  ( -0.6971942568897626646, 0.07405724077823318263, 0.5561023621509617598 ) ) ;
#1227 = CARTESIAN_POINT ( 'NONE',  ( 0.6971942568897648851, -0.07405724077823297447, 1.973425196796630088 ) ) ;
#1228 = CARTESIAN_POINT ( 'NONE',  ( -0.6971942568897648851, -0.07405724077823297447, 1.225393700733637514 ) ) ;
#1229 = APPLICATION_CONTEXT ( 'automotive_design' ) ;
#1230 = CARTESIAN_POINT ( 'NONE',  ( 0.04979026054520423183, -0.09842589400172224723, -0.1717333828277539942 ) ) ;
#1231 = CARTESIAN_POINT ( 'NONE',  ( 0.9873396505805591694, 0.1113553986120547346, 1.195866141732283561 ) ) ;
#1232 = CARTESIAN_POINT ( 'NONE',  ( 1.054774247047244540, 0.07405724077823318263, 0.4625984251430869665 ) ) ;
#1233 = CARTESIAN_POINT ( 'NONE',  ( -0.8019270111902716547, 0.1787899950787401604, 0.3887795275052913224 ) ) ;
#1234 = ORIENTED_EDGE ( 'NONE', *, *, #7462, .F. ) ;
#1235 = ADVANCED_FACE ( 'NONE', ( #12987 ), #46257, .F. ) ;
#1236 = FACE_OUTER_BOUND ( 'NONE', #37991, .T. ) ;
#1237 = ORIENTED_EDGE ( 'NONE', *, *, #25095, .T. ) ;
#1238 = CARTESIAN_POINT ( 'NONE',  ( 1.054774247047244540, -0.07405724077823318263, 0.8907480314422986378 ) ) ;
#1239 = CARTESIAN_POINT ( 'NONE',  ( -0.7185039370078746268, -0.06523048226347956391, 0.2682086614173231909 ) ) ;
#1240 = CARTESIAN_POINT ( 'NONE',  ( -0.1947286603072740374, -0.09851385302161634605, -0.1548760358685606353 ) ) ;
#1241 = CARTESIAN_POINT ( 'NONE',  ( -0.7646288533564489232, 0.1113553986120547346, 0.4872047243019220208 ) ) ;
#1242 = VERTEX_POINT ( 'NONE', #23759 ) ;
#1243 = AXIS2_PLACEMENT_3D ( 'NONE', #9459, #1527, #38204 ) ;
#1244 = ADVANCED_FACE ( 'NONE', ( #13229 ), #27628, .F. ) ;
#1245 = CARTESIAN_POINT ( 'NONE',  ( 0.1645760587280559184, -0.08068587895603188120, -0.1413870478498926997 ) ) ;
#1246 = CARTESIAN_POINT ( 'NONE',  ( -0.8759842519685039353, -0.1574803149606299191, 0.1968503937007874127 ) ) ;
#1247 = CARTESIAN_POINT ( 'NONE',  ( -0.1264236179284866091, -1.399238141457584739, -0.1264236179284866091 ) ) ;
#1248 = ORIENTED_EDGE ( 'NONE', *, *, #7894, .F. ) ;
#1249 = CARTESIAN_POINT ( 'NONE',  ( 0.1574803149606299191, 0.5288907983920094757, -0.7507079620615707549 ) ) ;
#1250 = CARTESIAN_POINT ( 'NONE',  ( 0.1264236179284866091, -0.4581692912848189247, 0.1264236179284866091 ) ) ;
#1251 = CARTESIAN_POINT ( 'NONE',  ( -0.8759842519685039353, -0.1574803149606299191, 0.07874015748031495954 ) ) ;
#1252 = EDGE_LOOP ( 'NONE', ( #11130, #15694, #34141, #24810 ) ) ;
#1253 = CARTESIAN_POINT ( 'NONE',  ( -0.06594017991609162077, 0.2574235754682526744, -0.3092881115733063790 ) ) ;
#1254 = CARTESIAN_POINT ( 'NONE',  ( -0.2471922904502826812, -0.09842519685039370636, 5.914624404477007554E-17 ) ) ;
#1255 = CARTESIAN_POINT ( 'NONE',  ( -1.033464566929133799, 0.000000000000000000, 1.545275590551181244 ) ) ;
#1256 = CARTESIAN_POINT ( 'NONE',  ( 0.8759842519685039353, -0.1787899950787401882, 0.1697834645131655606 ) ) ;
#1257 = CARTESIAN_POINT ( 'NONE',  ( -0.07405724077823318263, -1.730314960576156968, 0.1787899950787401604 ) ) ;
#1258 = CARTESIAN_POINT ( 'NONE',  ( -0.07405724077823318263, -1.804133858213953889, 0.1787899950787401604 ) ) ;
#1259 = DIRECTION ( 'NONE',  ( -1.000000000000000078E-15, -1.000000000000000000, -1.000000000000000078E-15 ) ) ;
#1260 = CARTESIAN_POINT ( 'NONE',  ( 0.5314960629921260393, 0.000000000000000000, 4.498031496062992574 ) ) ;
#1261 = ORIENTED_EDGE ( 'NONE', *, *, #13253, .T. ) ;
#1262 = EDGE_CURVE ( 'NONE', #3955, #45154, #243, .T. ) ;
#1263 = CARTESIAN_POINT ( 'NONE',  ( -0.8759842519685039353, -0.1787899950787401882, 0.6077755904974173617 ) ) ;
#1265 = PLANE ( 'NONE',  #18594 ) ;
#1264 = CARTESIAN_POINT ( 'NONE',  ( 0.1113553986120547346, -0.7608267716535432879, 0.1113553986120547346 ) ) ;
#1266 = CARTESIAN_POINT ( 'NONE',  ( -0.1797182628040039087, -1.573370581236589683, 0.07444174185955065859 ) ) ;
#1267 = FACE_OUTER_BOUND ( 'NONE', #22288, .T. ) ;
#1268 = DIRECTION ( 'NONE',  ( 1.822029033848725028E-16, 0.000000000000000000, 1.000000000000000000 ) ) ;
#1269 = CARTESIAN_POINT ( 'NONE',  ( 0.6971942568897648851, 0.07405724077823318263, 1.304133858213953667 ) ) ;
#1270 = CARTESIAN_POINT ( 'NONE',  ( 1.054774247047244540, -0.07405724077823318263, 1.870078740103715331 ) ) ;
#1271 = CARTESIAN_POINT ( 'NONE',  ( 0.9500414927467377701, -0.1787899950787401604, 0.2903543306548980185 ) ) ;
#1272 = VERTEX_POINT ( 'NONE', #1946 ) ;
#1273 = CARTESIAN_POINT ( 'NONE',  ( -0.7185039370078739607, 0.000000000000000000, -2.869337061179095023E-17 ) ) ;
#1274 = CARTESIAN_POINT ( 'NONE',  ( -0.8759842519685039353, -0.1574803149606299191, 1.446850393593259732 ) ) ;
#1275 = CARTESIAN_POINT ( 'NONE',  ( -0.1787899950787401604, -0.007874015694267972806, -0.07405724077823318263 ) ) ;
#1276 = CARTESIAN_POINT ( 'NONE',  ( 0.8759842519685039353, -0.1787899950787401882, 0.4847440944344252323 ) ) ;
#1278 = CARTESIAN_POINT ( 'NONE',  ( -1.033464566929134687, -0.06523048226347956391, 0.7554133858267708668 ) ) ;
#1277 = CARTESIAN_POINT ( 'NONE',  ( 0.7495606340400177148, -0.1264236179284866091, 1.306594488135212728 ) ) ;
#1279 = CARTESIAN_POINT ( 'NONE',  ( -0.8759842519685039353, 0.000000000000000000, 0.000000000000000000 ) ) ;
#1280 = CARTESIAN_POINT ( 'NONE',  ( 0.1574803149606300023, -0.9875035750853327077, -1.463737590216208861 ) ) ;
#1281 = CARTESIAN_POINT ( 'NONE',  ( -0.6971942568897648851, 0.07405724077823318263, 1.338582677111590069 ) ) ;
#1282 = CARTESIAN_POINT ( 'NONE',  ( 0.7646288533564489232, 0.1113553986120547346, 0.8809055117034961802 ) ) ;
#1283 = VERTEX_POINT ( 'NONE', #42877 ) ;
#1284 = CARTESIAN_POINT ( 'NONE',  ( -0.8107537697050254399, 0.1574803149606300301, 0.7997047243019207441 ) ) ;
#1285 = CARTESIAN_POINT ( 'NONE',  ( -0.1646842833814627927, -0.4387826116600692661, -0.9691966172188706263 ) ) ;
#1286 = ORIENTED_EDGE ( 'NONE', *, *, #30075, .F. ) ;
#1287 = EDGE_CURVE ( 'NONE', #34753, #1625, #41935, .T. ) ;
#1288 = CARTESIAN_POINT ( 'NONE',  ( -0.07444174185955065859, -0.08715010879564398516, -0.1797182628040039087 ) ) ;
#1289 = CARTESIAN_POINT ( 'NONE',  ( 0.1787899950787401604, -1.366141732229700478, 0.07405724077823318263 ) ) ;
#1290 = CARTESIAN_POINT ( 'NONE',  ( -0.8107537697050253289, -0.1574803149606297803, 0.5782480313885360879 ) ) ;
#1291 = CARTESIAN_POINT ( 'NONE',  ( 1.054774247047244096, 0.000000000000000000, 1.557578740103716441 ) ) ;
#1292 = CARTESIAN_POINT ( 'NONE',  ( -0.8759842519685039353, 0.1574803149606299191, 1.279527559055118280 ) ) ;
#1293 = CARTESIAN_POINT ( 'NONE',  ( 1.033464566929133799, 0.000000000000000000, 0.2066929133858267931 ) ) ;
#1295 = CARTESIAN_POINT ( 'NONE',  ( 0.9412147342319837628, 0.1574803149606300301, 1.946358267716537638 ) ) ;
#1294 = CARTESIAN_POINT ( 'NONE',  ( 0.1587072800412973328, -0.1005018865549618251, 0.1068311739851083991 ) ) ;
#1296 = DIRECTION ( 'NONE',  ( -0.000000000000000000, -0.2432573283306819767, 0.9699617890481142535 ) ) ;
#1297 = EDGE_CURVE ( 'NONE', #10382, #802, #31438, .T. ) ;
#1298 = ORIENTED_EDGE ( 'NONE', *, *, #37653, .F. ) ;
#1299 = EDGE_LOOP ( 'NONE', ( #44521, #27760, #38088 ) ) ;
#1300 = EDGE_CURVE ( 'NONE', #29883, #25085, #16051, .T. ) ;
#1301 = CARTESIAN_POINT ( 'NONE',  ( 0.7646288533564489232, -0.1113553986120547346, 0.5856299212598424786 ) ) ;
#1302 = ORIENTED_EDGE ( 'NONE', *, *, #20125, .F. ) ;
#1303 = CARTESIAN_POINT ( 'NONE',  ( 0.8759842519685039353, 0.1787899950787401882, 0.6668307086076534773 ) ) ;
#1304 = CARTESIAN_POINT ( 'NONE',  ( 0.9500414927467377701, 0.1787899950787401604, 0.9793307086076531442 ) ) ;
#1305 = CARTESIAN_POINT ( 'NONE',  ( -0.8019270111902716547, -0.1787899950787401604, 1.505905511757261062 ) ) ;
#1306 = CARTESIAN_POINT ( 'NONE',  ( -9.642888182262618425E-18, 0.01181102372957427288, -0.1574803149606299191 ) ) ;
#1307 = CARTESIAN_POINT ( 'NONE',  ( -0.6971942568897648851, 0.07405724077823318263, 1.264763779473795813 ) ) ;
#1308 = EDGE_CURVE ( 'NONE', #46256, #9934, #25199, .T. ) ;
#1309 = VECTOR ( 'NONE', #45246, 39.37007874015748143 ) ;
#1310 = DIRECTION ( 'NONE',  ( -1.000000000000000000, 3.469446951953613794E-15, 0.000000000000000000 ) ) ;
#1311 = CARTESIAN_POINT ( 'NONE',  ( 0.1787899950787401604, -1.017840503662311047, -0.07405724077823318263 ) ) ;
#1312 = ORIENTED_EDGE ( 'NONE', *, *, #24514, .F. ) ;
#1313 = CARTESIAN_POINT ( 'NONE',  ( 0.07405724077823318263, 0.09055118115612580121, 0.1787899950787401604 ) ) ;
#1314 = ORIENTED_EDGE ( 'NONE', *, *, #8215, .T. ) ;
#1315 = CARTESIAN_POINT ( 'NONE',  ( 0.8107537697050254399, -0.1574803149606297803, 1.208169291231056430 ) ) ;
#1316 = DIRECTION ( 'NONE',  ( 0.000000000000000000, 0.000000000000000000, 1.000000000000000000 ) ) ;
#1317 = CARTESIAN_POINT ( 'NONE',  ( 0.4620708661417356478, 0.9842519685039370358, -0.8759842519685050455 ) ) ;
#1318 = CARTESIAN_POINT ( 'NONE',  ( 0.07405724077823318263, -0.7017716534895438452, 0.1787899950787401604 ) ) ;
#1319 = ( BOUNDED_CURVE ( )  B_SPLINE_CURVE ( 2, ( #8751, #5155, #41080, #19776, #19540, #34409, #4427, #23616, #16201 ),
 .UNSPECIFIED., .F., .T. ) 
 B_SPLINE_CURVE_WITH_KNOTS ( ( 3, 2, 2, 2, 3 ),
 ( 0.02999999999999999889, 0.03250000000000000111, 0.03500000000000000333, 0.03749999999999999861, 0.04000000000000000083 ),
 .UNSPECIFIED. ) 
 CURVE ( )  GEOMETRIC_REPRESENTATION_ITEM ( )  RATIONAL_B_SPLINE_CURVE ( ( 1.000000000000000000, 0.9238795325112869605, 1.000000000000000000, 0.9238795325112869605, 1.000000000000000000, 0.9238795325112869605, 1.000000000000000000, 0.9238795325112869605, 1.000000000000000000 ) ) 
 REPRESENTATION_ITEM ( '' )  ) ;
#1320 = CARTESIAN_POINT ( 'NONE',  ( -0.7495606340400177148, -0.1264236179284866091, 0.2091535432533232486 ) ) ;
#1321 = CARTESIAN_POINT ( 'NONE',  ( -0.9873396505805591694, -0.1113553986120547346, 0.9104330708661417804 ) ) ;
#1322 = FACE_OUTER_BOUND ( 'NONE', #41297, .T. ) ;
#1323 = CARTESIAN_POINT ( 'NONE',  ( 0.1797182628040039087, -1.041874518244462422, -0.07444174185955065859 ) ) ;
#1324 = CARTESIAN_POINT ( 'NONE',  ( 0.7495606340400177148, 0.1264236179284866091, 0.8686023621509606496 ) ) ;
#1325 = CARTESIAN_POINT ( 'NONE',  ( 0.7495606340400177148, -0.1264236179284866091, 1.424704724355685181 ) ) ;
#1326 = CARTESIAN_POINT ( 'NONE',  ( -0.7185039370078739607, 1.928577636452523993E-17, 0.8562992125984251190 ) ) ;
#1327 = CARTESIAN_POINT ( 'NONE',  ( 0.9412147342319837628, -0.1574803149606297803, 1.537893700787401841 ) ) ;
#1329 = DIRECTION ( 'NONE',  ( -1.000000000000000000, 0.000000000000000000, 0.000000000000000000 ) ) ;
#1328 = CARTESIAN_POINT ( 'NONE',  ( 0.7301145607164034601, -0.08514804839641164358, 1.984932717043631056 ) ) ;
#1330 = LINE ( 'NONE', #2050, #12163 ) ;
#1331 = CARTESIAN_POINT ( 'NONE',  ( 0.06523048226347956391, -0.6993110235145204578, -0.1574803149606300301 ) ) ;
#1332 = CARTESIAN_POINT ( 'NONE',  ( -0.9873396505805591694, 0.1113553986120547346, 1.619094488081448846 ) ) ;
#1333 = VECTOR ( 'NONE', #26259, 39.37007874015748143 ) ;
#1334 = CARTESIAN_POINT ( 'NONE',  ( 1.033464566929133799, 0.000000000000000000, 1.427165354330708569 ) ) ;
#1335 = CARTESIAN_POINT ( 'NONE',  ( 0.6971942568897637749, 2.189545951927499583E-17, 0.9867125983714331028 ) ) ;
#1336 = CARTESIAN_POINT ( 'NONE',  ( 1.054774247047244540, -0.07405724077823318263, 1.874999999946236784 ) ) ;
#1337 = CARTESIAN_POINT ( 'NONE',  ( -0.07405724077823318263, -0.8592519684501739308, 0.1787899950787401604 ) ) ;
#1338 = CARTESIAN_POINT ( 'NONE',  ( 0.8107537697050253289, 0.1574803149606300301, 0.4060039369003469734 ) ) ;
#1339 = VERTEX_POINT ( 'NONE', #16576 ) ;
#1340 = ADVANCED_FACE ( 'NONE', ( #5541, #31206 ), #42645, .T. ) ;
#1341 = LINE ( 'NONE', #8065, #13865 ) ;
#1342 = CARTESIAN_POINT ( 'NONE',  ( 0.1377952755905510196, 0.000000000000000000, -0.1828167807439035619 ) ) ;
#1343 = CARTESIAN_POINT ( 'NONE',  ( -0.1574803149606297803, -1.668799212490898576, 0.06523048226347956391 ) ) ;
#1344 = CARTESIAN_POINT ( 'NONE',  ( -0.9873396505805591694, -0.1113553986120547346, 0.1131889762704257896 ) ) ;
#1345 = CARTESIAN_POINT ( 'NONE',  ( 0.8759842519685039353, -0.1787899950787401882, 1.075295275536787276 ) ) ;
#1346 = DIRECTION ( 'NONE',  ( -0.000000000000000000, 0.7880107536067203489, -0.6156614753256604011 ) ) ;
#1347 = CARTESIAN_POINT ( 'NONE',  ( 2.892866454678787531E-17, -1.789370078740157410, 0.1574803149606299191 ) ) ;
#1348 = DIRECTION ( 'NONE',  ( 1.000000000000000000, -3.469446951953613794E-15, -0.000000000000000000 ) ) ;
#1349 = EDGE_CURVE ( 'NONE', #33650, #35903, #5146, .T. ) ;
#1350 = CARTESIAN_POINT ( 'NONE',  ( -0.9500414927467378812, 0.1787899950787401604, 0.1870078739619845387 ) ) ;
#1351 = ORIENTED_EDGE ( 'NONE', *, *, #3191, .T. ) ;
#1353 = CARTESIAN_POINT ( 'NONE',  ( 0.1787899950787401882, -1.599901574749385880, -2.189545951927503898E-17 ) ) ;
#1352 = CARTESIAN_POINT ( 'NONE',  ( -0.06523048226347956391, -0.3400590550105831444, -0.1574803149606300301 ) ) ;
#1354 = CARTESIAN_POINT ( 'NONE',  ( -0.6971942568897648851, 0.07405724077823318263, 1.889763779473794258 ) ) ;
#1355 = CARTESIAN_POINT ( 'NONE',  ( -1.002407869896990045, 0.1264236179284866091, 0.8932086613635591421 ) ) ;
#1356 = ADVANCED_FACE ( 'NONE', ( #19336 ), #22697, .T. ) ;
#1357 = CARTESIAN_POINT ( 'NONE',  ( -0.6971942568897637749, 2.189545951927499583E-17, 0.5585629920722204877 ) ) ;
#1358 = FACE_OUTER_BOUND ( 'NONE', #15642, .T. ) ;
#1360 = CIRCLE ( 'NONE', #22783, 0.2362204724409449064 ) ;
#1359 = PRODUCT_DEFINITION ( 'UNKNOWN', '', #8646, #32694 ) ;
#1361 = CARTESIAN_POINT ( 'NONE',  ( 0.2204724409448818867, 0.000000000000000000, 0.000000000000000000 ) ) ;
#1362 = LINE ( 'NONE', #9042, #21868 ) ;
#1363 = CARTESIAN_POINT ( 'NONE',  ( -0.2066929133858267931, 1.174718201258053041, -3.430321324600322797 ) ) ;
#1364 = CARTESIAN_POINT ( 'NONE',  ( -0.07405724077823318263, -0.4961869603552226948, -0.1787899950787401604 ) ) ;
#1365 = CARTESIAN_POINT ( 'NONE',  ( 0.1120789836339634027, -0.08956013912318722126, 0.1830409950616023740 ) ) ;
#1366 = CARTESIAN_POINT ( 'NONE',  ( 0.1476377952755906220, 0.06415291647593697466, -0.1630605872086746122 ) ) ;
#1367 = CARTESIAN_POINT ( 'NONE',  ( -0.1377952755905511861, 0.1574803149606320007, -0.8070866141732283561 ) ) ;
#1368 = CARTESIAN_POINT ( 'NONE',  ( -1.054774247047244540, -0.07405724077823318263, 0.4527559054580477249 ) ) ;
#1369 = DIRECTION ( 'NONE',  ( 0.000000000000000000, -1.000000000000000000, 0.000000000000000000 ) ) ;
#1370 = CARTESIAN_POINT ( 'NONE',  ( -0.8759842519685039353, -0.1787899950787401882, 1.552657480261196765 ) ) ;
#1371 = CARTESIAN_POINT ( 'NONE',  ( 0.1787899950787401604, -1.558070866087969630, -0.07405724077823318263 ) ) ;
#1372 = CARTESIAN_POINT ( 'NONE',  ( 0.1264236179284866091, -1.590059055064346305, -0.1264236179284866091 ) ) ;
#1373 = ( CONVERSION_BASED_UNIT ( 'INCH', #8573 ) LENGTH_UNIT ( ) NAMED_UNIT ( #37463 ) ) ;
#1374 = DIRECTION ( 'NONE',  ( -1.000000000000000000, 0.000000000000000000, 0.000000000000000000 ) ) ;
#1375 = CARTESIAN_POINT ( 'NONE',  ( 1.033464566929133799, 1.928577636452524610E-17, 4.498031496062992574 ) ) ;
#1376 = CARTESIAN_POINT ( 'NONE',  ( -0.8759842519685039353, -0.1574803149606299191, 1.289370078632629868 ) ) ;
#1377 = CARTESIAN_POINT ( 'NONE',  ( 0.7495606340400177148, -0.1264236179284866091, 0.5241141731745827537 ) ) ;
#1379 = CARTESIAN_POINT ( 'NONE',  ( 0.8107537697050254399, -0.1574803149606297803, 0.3518700787401575769 ) ) ;
#1378 = CARTESIAN_POINT ( 'NONE',  ( -0.1113553986120547346, -0.4261811023622047445, -0.1113553986120547346 ) ) ;
#1380 = CARTESIAN_POINT ( 'NONE',  ( -1.033464566929134687, 0.06523048226347956391, 0.4060039370078741827 ) ) ;
#1381 = ORIENTED_EDGE ( 'NONE', *, *, #11607, .T. ) ;
#1382 = ADVANCED_FACE ( 'NONE', ( #15057 ), #26068, .T. ) ;
#1383 = CARTESIAN_POINT ( 'NONE',  ( -0.1574803149606299191, -0.4872761608334555961, -0.8688576204587789009 ) ) ;
#1384 = CARTESIAN_POINT ( 'NONE',  ( -1.054774247047244096, 0.000000000000000000, 1.050688976324189117 ) ) ;
#1385 = CARTESIAN_POINT ( 'NONE',  ( 0.7185039370078746268, 0.06523048226347956391, 1.168799212598425896 ) ) ;
#1386 = CARTESIAN_POINT ( 'NONE',  ( 0.1184675242425283492, -0.5708661417322835607, 1.214596435718460654 ) ) ;
#1387 = CARTESIAN_POINT ( 'NONE',  ( 1.033464566929133355, -0.06523048226348075740, 0.5880905510735754405 ) ) ;
#1388 = CARTESIAN_POINT ( 'NONE',  ( -0.8759842519685039353, 0.000000000000000000, 1.990649606245448844 ) ) ;
#1389 = CARTESIAN_POINT ( 'NONE',  ( -0.1154458135679224812, -0.08956175409534371246, 0.1128118131157532372 ) ) ;
#1390 = CARTESIAN_POINT ( 'NONE',  ( 0.1787899950787401604, -0.4901574802611972093, -0.07405724077823318263 ) ) ;
#1391 = ORIENTED_EDGE ( 'NONE', *, *, #22168, .T. ) ;
#1392 = ADVANCED_FACE ( 'NONE', ( #33283 ), #26320, .T. ) ;
#1393 = DIRECTION ( 'NONE',  ( 0.000000000000000000, -1.000000000000000000, 0.000000000000000000 ) ) ;
#1394 = EDGE_LOOP ( 'NONE', ( #19452, #2996, #3138, #1298 ) ) ;
#1395 = CARTESIAN_POINT ( 'NONE',  ( 0.7646288533564489232, 0.1113553986120547346, 1.284448818897637956 ) ) ;
#1396 = CARTESIAN_POINT ( 'NONE',  ( -0.06523048226347956391, -0.03494094488188976416, -0.1574803149606300301 ) ) ;
#1397 = CARTESIAN_POINT ( 'NONE',  ( 0.1787899950787401882, -1.713090551127338657, -2.189545951927503898E-17 ) ) ;
#1398 = CARTESIAN_POINT ( 'NONE',  ( 0.07405724077823318263, -0.9379921259304876413, 0.1787899950787401604 ) ) ;
#1400 = VECTOR ( 'NONE', #475, 39.37007874015748143 ) ;
#1399 = CARTESIAN_POINT ( 'NONE',  ( -0.1113553986120547346, -1.282480314960629864, 0.1113553986120547346 ) ) ;
#1401 = CARTESIAN_POINT ( 'NONE',  ( 0.7646288533564489232, 0.1113553986120547346, 1.077755905404283565 ) ) ;
#1402 = DIRECTION ( 'NONE',  ( -1.000000000000000000, 0.000000000000000000, 0.000000000000000000 ) ) ;
#1403 = ORIENTED_EDGE ( 'NONE', *, *, #27999, .T. ) ;
#1404 = ORIENTED_EDGE ( 'NONE', *, *, #13116, .F. ) ;
#1405 = CARTESIAN_POINT ( 'NONE',  ( -0.7495606340400177148, 0.1264236179284866091, 1.695374015694267822 ) ) ;
#1406 = CARTESIAN_POINT ( 'NONE',  ( 1.054774247047244540, -0.07405724077823318263, 1.796259842465923073 ) ) ;
#1407 = ORIENTED_EDGE ( 'NONE', *, *, #14186, .F. ) ;
#1408 = CARTESIAN_POINT ( 'NONE',  ( 0.1574803149606300301, -0.0004921258767249256719, 0.06523048226347956391 ) ) ;
#1409 = CARTESIAN_POINT ( 'NONE',  ( 1.002407869896990045, 0.1264236179284866091, 0.4256889763241890057 ) ) ;
#1410 = CARTESIAN_POINT ( 'NONE',  ( -0.6971942568897637749, 2.189545951927499583E-17, 1.380413385773007873 ) ) ;
#1411 = CYLINDRICAL_SURFACE ( 'NONE', #33531, 0.1574803149606299191 ) ;
#1412 = CARTESIAN_POINT ( 'NONE',  ( -0.9500414927467377701, 0.1787899950787401604, 1.407480314906865981 ) ) ;
#1413 = CARTESIAN_POINT ( 'NONE',  ( -1.002407869896990045, -0.1264236179284866091, 0.8046259841982047467 ) ) ;
#1414 = CARTESIAN_POINT ( 'NONE',  ( -0.6971942568897626646, -0.07405724077823297447, 0.8710629920722218200 ) ) ;
#1415 = CARTESIAN_POINT ( 'NONE',  ( -1.054774247047244540, 0.07405724077823318263, 0.1476377952218269618 ) ) ;
#1416 = DIRECTION ( 'NONE',  ( 0.000000000000000000, 0.000000000000000000, -1.000000000000000000 ) ) ;
#1417 = CARTESIAN_POINT ( 'NONE',  ( -0.9500414927467378812, -0.1787899950787401604, 1.712598425143087688 ) ) ;
#1418 = CARTESIAN_POINT ( 'NONE',  ( -1.054774247047244540, -0.07405724077823318263, 0.1033464566391498751 ) ) ;
#1419 = CARTESIAN_POINT ( 'NONE',  ( -0.9412147342319837628, -0.1574803149606297803, 1.695374015748031482 ) ) ;
#1420 = CARTESIAN_POINT ( 'NONE',  ( -0.8107537697050254399, 0.1574803149606300301, 0.2977362204724410821 ) ) ;
#1421 = CARTESIAN_POINT ( 'NONE',  ( 0.7495606340400177148, -0.1264236179284866091, 1.587106299158834721 ) ) ;
#1422 = CARTESIAN_POINT ( 'NONE',  ( -0.2092218244630917323, -0.09842519685039370636, 0.1092665889510173183 ) ) ;
#1423 = CARTESIAN_POINT ( 'NONE',  ( -0.8759842519685039353, 0.000000000000000000, 0.000000000000000000 ) ) ;
#1424 = CIRCLE ( 'NONE', #38924, 0.2471922904502826812 ) ;
#1425 = EDGE_LOOP ( 'NONE', ( #24710, #12215, #7861, #39524, #40146 ) ) ;
#1426 = CARTESIAN_POINT ( 'NONE',  ( -0.8019270111902716547, 0.1787899950787401604, 1.181102362150960428 ) ) ;
#1427 = CARTESIAN_POINT ( 'NONE',  ( -0.1264236179284866091, -0.9158464566391496531, -0.1264236179284866091 ) ) ;
#1428 = CIRCLE ( 'NONE', #47370, 0.09842519685039370636 ) ;
#1429 = CARTESIAN_POINT ( 'NONE',  ( -0.07405724077823318263, -1.110236220418677533, -0.1787899950787401604 ) ) ;
#1430 = DIRECTION ( 'NONE',  ( -0.000000000000000000, 1.000000000000000000, -0.000000000000000000 ) ) ;
#1431 = ( LENGTH_UNIT ( ) NAMED_UNIT ( * ) SI_UNIT ( $, .METRE. ) ) ;
#1432 = CARTESIAN_POINT ( 'NONE',  ( 0.7495606340400177148, 0.1264236179284866091, 1.847933070812378009 ) ) ;
#1433 = CARTESIAN_POINT ( 'NONE',  ( -1.100456976456230270E-17, -0.2864611324176913332, -0.1797182628040039365 ) ) ;
#1434 = CARTESIAN_POINT ( 'NONE',  ( -0.06523048226347956391, -1.821358267609009651, 0.1574803149606297803 ) ) ;
#1435 = AXIS2_PLACEMENT_3D ( 'NONE', #9624, #2406, #9388 ) ;
#1436 = FACE_OUTER_BOUND ( 'NONE', #45627, .T. ) ;
#1437 = CARTESIAN_POINT ( 'NONE',  ( 0.1264236179284866091, -0.1481299212060789294, 0.1264236179284866091 ) ) ;
#1438 = EDGE_CURVE ( 'NONE', #4911, #23956, #39418, .T. ) ;
#1439 = CARTESIAN_POINT ( 'NONE',  ( 0.6971942568897626646, 0.07405724077823318263, 0.9055118109698585549 ) ) ;
#1440 = ADVANCED_FACE ( 'NONE', ( #26557 ), #44714, .F. ) ;
#1441 = DIRECTION ( 'NONE',  ( 0.000000000000000000, 0.000000000000000000, -1.000000000000000000 ) ) ;
#1442 = CARTESIAN_POINT ( 'NONE',  ( -0.3100393700787401619, -2.714815113292586694E-26, 1.043307086614172707 ) ) ;
#1443 = CARTESIAN_POINT ( 'NONE',  ( 0.9500414927467378812, -0.1787899950787401604, 1.988188976324187562 ) ) ;
#1444 = EDGE_CURVE ( 'NONE', #18796, #17177, #32922, .T. ) ;
#1445 = ADVANCED_FACE ( 'NONE', ( #167, #29705 ), #40878, .F. ) ;
#1446 = DIRECTION ( 'NONE',  ( -1.000000000000000000, 0.000000000000000000, 0.000000000000000000 ) ) ;
#1448 = CARTESIAN_POINT ( 'NONE',  ( 0.1264236179284866091, -0.3843503936470239468, 0.1264236179284866091 ) ) ;
#1447 = CARTESIAN_POINT ( 'NONE',  ( -0.06523048226347956391, -0.9945866140657014798, 0.1574803149606297803 ) ) ;
#1449 = CARTESIAN_POINT ( 'NONE',  ( -0.7185039370078739607, 0.000000000000000000, -2.869337061179095023E-17 ) ) ;
#1450 = CARTESIAN_POINT ( 'NONE',  ( 0.1787899950787401604, -1.203740157426551383, 0.07405724077823318263 ) ) ;
#1451 = AXIS2_PLACEMENT_3D ( 'NONE', #15454, #4626, #8236 ) ;
#1452 = CARTESIAN_POINT ( 'NONE',  ( -1.054774247047244540, -0.07405724077823318263, 1.751968503883245765 ) ) ;
#1453 = ORIENTED_EDGE ( 'NONE', *, *, #37947, .T. ) ;
#1454 = CARTESIAN_POINT ( 'NONE',  ( -0.8759842519685039353, 0.1787899950787401882, 1.375492125930488196 ) ) ;
#1455 = CARTESIAN_POINT ( 'NONE',  ( 0.8019270111902717657, 0.1787899950787401604, 1.456692913332062744 ) ) ;
#1456 = CARTESIAN_POINT ( 'NONE',  ( -0.1113553986120547346, -1.233267716427905336, 0.1113553986120547346 ) ) ;
#1457 = CARTESIAN_POINT ( 'NONE',  ( -0.7495606340400177148, -0.1264236179284866091, 0.5241141731745827537 ) ) ;
#1458 = CARTESIAN_POINT ( 'NONE',  ( -1.002407869896990045, -0.1264236179284866091, 1.158956692859621995 ) ) ;
#1459 = FACE_OUTER_BOUND ( 'NONE', #19089, .T. ) ;
#1460 = CARTESIAN_POINT ( 'NONE',  ( -0.1209429854940891474, -0.09842561477428417305, -0.1316810161538188584 ) ) ;
#1461 = CARTESIAN_POINT ( 'NONE',  ( 1.054774247047244540, -0.07405724077823318263, 0.4576771653005669016 ) ) ;
#1462 = CARTESIAN_POINT ( 'NONE',  ( -0.7495606340400177148, 0.1264236179284866091, 0.3912401574265515491 ) ) ;
#1463 = ( NAMED_UNIT ( * ) PLANE_ANGLE_UNIT ( ) SI_UNIT ( $, .RADIAN. ) ) ;
#1464 = ( BOUNDED_CURVE ( )  B_SPLINE_CURVE ( 2, ( #11705, #33769, #32816, #14821, #25384, #29256, #36626, #26330, #29487 ),
 .UNSPECIFIED., .F., .T. ) 
 B_SPLINE_CURVE_WITH_KNOTS ( ( 3, 2, 2, 2, 3 ),
 ( 0.1799999999999999933, 0.1824999999999999956, 0.1849999999999999978, 0.1875000000000000000, 0.1900000000000000022 ),
 .UNSPECIFIED. ) 
 CURVE ( )  GEOMETRIC_REPRESENTATION_ITEM ( )  RATIONAL_B_SPLINE_CURVE ( ( 1.000000000000000000, 0.9238795325112869605, 1.000000000000000000, 0.9238795325112869605, 1.000000000000000000, 0.9238795325112869605, 1.000000000000000000, 0.9238795325112869605, 1.000000000000000000 ) ) 
 REPRESENTATION_ITEM ( '' )  ) ;
#1465 = CARTESIAN_POINT ( 'NONE',  ( -0.1158283541424031532, -0.08956345598586890056, -0.1361971163587911426 ) ) ;
#1466 = ORIENTED_EDGE ( 'NONE', *, *, #25772, .F. ) ;
#1467 = VERTEX_POINT ( 'NONE', #10334 ) ;
#1468 = CARTESIAN_POINT ( 'NONE',  ( -0.7185039370078739607, 1.928577636452523993E-17, 0.2657480314960630197 ) ) ;
#1469 = AXIS2_PLACEMENT_3D ( 'NONE', #15050, #30164, #26063 ) ;
#1470 = CARTESIAN_POINT ( 'NONE',  ( -1.002407869896990045, -0.1264236179284866091, 1.946358267662771757 ) ) ;
#1471 = CARTESIAN_POINT ( 'NONE',  ( -0.7185039370078746268, -0.06523048226347956391, 1.961122047244095778 ) ) ;
#1472 = ORIENTED_EDGE ( 'NONE', *, *, #29449, .F. ) ;
#1473 = CARTESIAN_POINT ( 'NONE',  ( 0.000000000000000000, 0.000000000000000000, -0.2219368594840610276 ) ) ;
#1474 = CARTESIAN_POINT ( 'NONE',  ( -0.6971942568897648851, 0.07405724077823318263, 1.028543307032851795 ) ) ;
#1475 = CARTESIAN_POINT ( 'NONE',  ( 0.1596650774283281671, -0.09389790430994664205, -0.1183119828674929208 ) ) ;
#1476 = CARTESIAN_POINT ( 'NONE',  ( -0.6971942568897626646, 0.07405724077823318263, 0.03937007868639404856 ) ) ;
#1477 = CARTESIAN_POINT ( 'NONE',  ( 0.1787899950787401882, -1.571482235945773853, -2.189545951927503898E-17 ) ) ;
#1478 = ORIENTED_EDGE ( 'NONE', *, *, #45701, .T. ) ;
#1479 = CARTESIAN_POINT ( 'NONE',  ( -0.9412147342319837628, 0.1574803149606300301, 0.1648622046168823629 ) ) ;
#1480 = CARTESIAN_POINT ( 'NONE',  ( 3.284318927891251994E-17, -0.4630905511273386010, 0.1787899950787401882 ) ) ;
#1481 = CARTESIAN_POINT ( 'NONE',  ( 1.033464566929133799, 0.000000000000000000, 1.692913385719244213 ) ) ;
#1482 = EDGE_LOOP ( 'NONE', ( #18220, #20705 ) ) ;
#1483 = B_SPLINE_CURVE_WITH_KNOTS ( 'NONE', 3,
 ( #27986, #3010, #17175, #24600, #42774, #24838, #16708, #5916, #39439, #2776, #31337, #5681, #42553, #35166, #27769, #2081 ),
 .UNSPECIFIED., .F., .F.,
 ( 4, 2, 2, 2, 2, 2, 2, 4 ),
 ( 0.000000000000000000, 0.2499999999999998335, 0.3749999999999996669, 0.4374999999999997224, 0.4999999999999997780, 0.6249999999999997780, 0.7499999999999998890, 1.000000000000000000 ),
 .UNSPECIFIED. ) ;
#1484 = CARTESIAN_POINT ( 'NONE',  ( 0.8759842519685039353, 0.1574803149606299191, 1.466535432963338437 ) ) ;
#1485 = DIRECTION ( 'NONE',  ( 1.822029033848725028E-16, 0.000000000000000000, 1.000000000000000000 ) ) ;
#1486 = ( BOUNDED_CURVE ( )  B_SPLINE_CURVE ( 2, ( #17218, #9568, #24880, #43066, #31853, #38789, #17678, #5946, #39240 ),
 .UNSPECIFIED., .F., .T. ) 
 B_SPLINE_CURVE_WITH_KNOTS ( ( 3, 2, 2, 2, 3 ),
 ( 0.3300000000000000155, 0.3325000000000000178, 0.3350000000000000200, 0.3375000000000000222, 0.3400000000000000244 ),
 .UNSPECIFIED. ) 
 CURVE ( )  GEOMETRIC_REPRESENTATION_ITEM ( )  RATIONAL_B_SPLINE_CURVE ( ( 1.000000000000000000, 0.9238795325112869605, 1.000000000000000000, 0.9238795325112869605, 1.000000000000000000, 0.9238795325112869605, 1.000000000000000000, 0.9238795325112869605, 1.000000000000000000 ) ) 
 REPRESENTATION_ITEM ( '' )  ) ;
#1487 = CARTESIAN_POINT ( 'NONE',  ( -1.094772975963752103E-17, -0.2121062991588350544, -0.1787899950787401882 ) ) ;
#1488 = AXIS2_PLACEMENT_3D ( 'NONE', #8603, #23243, #19630 ) ;
#1489 = CARTESIAN_POINT ( 'NONE',  ( 0.006378642920537238789, -0.09116121678392095917, -0.1176987636585394986 ) ) ;
#1490 = CARTESIAN_POINT ( 'NONE',  ( 0.1787899950787401604, -1.715551181048599716, -0.07405724077823318263 ) ) ;
#1491 = APPLICATION_PROTOCOL_DEFINITION ( 'draft international standard', 'automotive_design', 1998, #3971 ) ;
#1492 = LINE ( 'NONE', #22848, #24213 ) ;
#1493 = VECTOR ( 'NONE', #28318, 39.37007874015748143 ) ;
#1494 = EDGE_CURVE ( 'NONE', #3991, #16648, #40415, .T. ) ;
#1495 = CARTESIAN_POINT ( 'NONE',  ( -0.8759842519685039353, 0.1787899950787401882, 0.6274606298674959559 ) ) ;
#1497 = CARTESIAN_POINT ( 'NONE',  ( 0.000000000000000000, 0.000000000000000000, -0.4921259842519685179 ) ) ;
#1496 = CARTESIAN_POINT ( 'NONE',  ( 0.06523048226347956391, -0.8026574803149603143, 0.1574803149606297803 ) ) ;
#1498 = CARTESIAN_POINT ( 'NONE',  ( 3.301370929368692659E-17, -1.644728848953123990, 0.1797182628040039365 ) ) ;
#1499 = CARTESIAN_POINT ( 'NONE',  ( -0.3980944881889741382, 0.7681739484881660029, -0.04983111751016756213 ) ) ;
#1500 = DIRECTION ( 'NONE',  ( 0.000000000000000000, 0.000000000000000000, 1.000000000000000000 ) ) ;
#1501 = CARTESIAN_POINT ( 'NONE',  ( 0.6971942568897648851, 0.07405724077823318263, 1.579724409395055318 ) ) ;
#1502 = CONICAL_SURFACE ( 'NONE', #6088, 0.1377952755905510751, 0.9599310885968951323 ) ;
#1503 = CARTESIAN_POINT ( 'NONE',  ( 0.6971942568897637749, 2.189545951927499583E-17, 1.892224409395055096 ) ) ;
#1504 = APPLICATION_CONTEXT ( 'automotive_design' ) ;
#1505 = CARTESIAN_POINT ( 'NONE',  ( 0.000000000000000000, 0.09842519685039370636, 0.000000000000000000 ) ) ;
#1506 = ADVANCED_FACE ( 'NONE', ( #36617 ), #1113, .T. ) ;
#1507 = CARTESIAN_POINT ( 'NONE',  ( 0.03901279071809810040, -0.09842519685039370636, 1.870565676741754668 ) ) ;
#1508 = CARTESIAN_POINT ( 'NONE',  ( 0.2185580477451977144, -0.1693028889592579356, -0.3031249188859761468 ) ) ;
#1509 = CARTESIAN_POINT ( 'NONE',  ( 0.1264236179284866091, 0.01919291343959031448, -0.1264236179284866091 ) ) ;
#1510 = CARTESIAN_POINT ( 'NONE',  ( 1.033464566929133799, 0.000000000000000000, 0.5118110235145204578 ) ) ;
#1511 = CARTESIAN_POINT ( 'NONE',  ( 1.054774247047244096, 0.000000000000000000, 0.4552165353793071745 ) ) ;
#1512 = CARTESIAN_POINT ( 'NONE',  ( -0.7185039370078739607, 1.928577636452523993E-17, 1.722440944881889813 ) ) ;
#1513 = DIRECTION ( 'NONE',  ( -1.144917494144692682E-16, 5.091027988365947196E-31, -1.000000000000000000 ) ) ;
#1514 = FACE_OUTER_BOUND ( 'NONE', #43262, .T. ) ;
#1515 = CARTESIAN_POINT ( 'NONE',  ( -0.7495606340400177148, -0.1264236179284866091, 1.306594488135212728 ) ) ;
#1516 = CARTESIAN_POINT ( 'NONE',  ( 0.7646288533564489232, 0.1113553986120547346, 0.8021653542231811373 ) ) ;
#1517 = ORIENTED_EDGE ( 'NONE', *, *, #16320, .F. ) ;
#1518 = CARTESIAN_POINT ( 'NONE',  ( -0.1574803149606299191, 0.3648440108500937140, -3.619166627704267114 ) ) ;
#1519 = CARTESIAN_POINT ( 'NONE',  ( 0.8019270111902717657, 0.1787899950787401604, 0.9842519684501742638 ) ) ;
#1520 = VERTEX_POINT ( 'NONE', #24946 ) ;
#1521 = CARTESIAN_POINT ( 'NONE',  ( -0.1787899950787401604, -1.341535433017102541, 0.07405724077823318263 ) ) ;
#1522 = CARTESIAN_POINT ( 'NONE',  ( -0.9412147342319837628, -0.1574803149606297803, 0.5437992124908979097 ) ) ;
#1523 = FACE_OUTER_BOUND ( 'NONE', #20708, .T. ) ;
#1524 = CARTESIAN_POINT ( 'NONE',  ( 0.9500414927467378812, 0.1787899950787401604, 1.722440944828125930 ) ) ;
#1525 = CARTESIAN_POINT ( 'NONE',  ( -1.033464566929134687, -0.06523048226347956391, 1.306594488188977055 ) ) ;
#1526 = CARTESIAN_POINT ( 'NONE',  ( 0.000000000000000000, 0.6305768042517894134, -0.4926605935704669315 ) ) ;
#1528 = DIRECTION ( 'NONE',  ( -1.000000000000000000, 0.000000000000000000, 0.000000000000000000 ) ) ;
#1527 = DIRECTION ( 'NONE',  ( -1.000000000000000000, 0.000000000000000000, 0.000000000000000000 ) ) ;
#1529 = CARTESIAN_POINT ( 'NONE',  ( 1.002407869896990045, -0.1264236179284866091, 0.06151574797773248782 ) ) ;
#1530 = CARTESIAN_POINT ( 'NONE',  ( 0.7185039370078746268, -0.06523048226347956391, 1.360728346349165285 ) ) ;
#1531 = VERTEX_POINT ( 'NONE', #22453 ) ;
#1532 = EDGE_LOOP ( 'NONE', ( #26230, #3600, #16284, #44821 ) ) ;
#1533 = AXIS2_PLACEMENT_3D ( 'NONE', #32083, #18396, #33038 ) ;
#1534 = DIRECTION ( 'NONE',  ( -1.000000000000000000, 0.000000000000000000, 0.000000000000000000 ) ) ;
#1535 = VERTEX_POINT ( 'NONE', #39542 ) ;
#1536 = CARTESIAN_POINT ( 'NONE',  ( -1.002407869896990045, 0.1264236179284866091, 1.601870078686393750 ) ) ;
#1537 = CARTESIAN_POINT ( 'NONE',  ( -0.06523048226347956391, -0.02509842508932335833, -0.1574803149606300301 ) ) ;
#1538 = CARTESIAN_POINT ( 'NONE',  ( -1.002407869896990045, -0.1264236179284866091, 1.478838582623401399 ) ) ;
#1539 = ORIENTED_EDGE ( 'NONE', *, *, #45161, .T. ) ;
#1540 = AXIS2_PLACEMENT_3D ( 'NONE', #15602, #11522, #41421 ) ;
#1541 = EDGE_CURVE ( 'NONE', #34889, #31112, #8075, .T. ) ;
#1542 = LINE ( 'NONE', #23135, #39059 ) ;
#1543 = CARTESIAN_POINT ( 'NONE',  ( 0.5538057742782149795, -0.08090551181102362266, 1.098083891755157578E-17 ) ) ;
#1544 = CARTESIAN_POINT ( 'NONE',  ( -0.6195511811023656223, 1.354170115732555191, -0.4197102375732078561 ) ) ;
#1545 = CARTESIAN_POINT ( 'NONE',  ( -0.1787899950787401882, -1.039986172953647481, 0.000000000000000000 ) ) ;
#1546 = EDGE_LOOP ( 'NONE', ( #9201, #4846, #43494, #46692 ) ) ;
#1547 = AXIS2_PLACEMENT_3D ( 'NONE', #38721, #20498, #26603 ) ;
#1548 = CARTESIAN_POINT ( 'NONE',  ( -0.07405724077823318263, 0.04625984257344856188, 0.1787899950787401604 ) ) ;
#1549 = EDGE_LOOP ( 'NONE', ( #2403, #29375, #9278, #18291, #6691, #19468 ) ) ;
#1550 = ORIENTED_EDGE ( 'NONE', *, *, #36171, .F. ) ;
#1551 = CARTESIAN_POINT ( 'NONE',  ( 0.7185039370078739607, 1.928577636452523993E-17, 1.751968503829480106 ) ) ;
#1552 = CARTESIAN_POINT ( 'NONE',  ( -0.4338976377952755703, -2.656856766417909227E-17, 0.000000000000000000 ) ) ;
#1553 = CARTESIAN_POINT ( 'NONE',  ( 0.1787899950787401882, -0.5762795275052914334, -2.189545951927503898E-17 ) ) ;
#1554 = EDGE_CURVE ( 'NONE', #14871, #42574, #29477, .T. ) ;
#1555 = CARTESIAN_POINT ( 'NONE',  ( -0.9500414927467377701, 0.1787899950787401604, 0.1525590550643468324 ) ) ;
#1556 = CARTESIAN_POINT ( 'NONE',  ( -1.033464566929134687, 0.06523048226347956391, 0.9965551181102363376 ) ) ;
#1557 = DIRECTION ( 'NONE',  ( 1.000000000000000000, -3.469446951953613794E-15, -0.000000000000000000 ) ) ;
#1558 = CARTESIAN_POINT ( 'NONE',  ( 0.1797182628040039087, -1.159984754464934653, -0.07444174185955065859 ) ) ;
#1559 = CARTESIAN_POINT ( 'NONE',  ( 0.1540151740152538029, 0.1299212598425197041, -0.07158477921181821690 ) ) ;
#1560 = CARTESIAN_POINT ( 'NONE',  ( 0.8019270111902717657, -0.1787899950787401604, 0.8809055117572599514 ) ) ;
#1561 = CARTESIAN_POINT ( 'NONE',  ( 1.002407869896990045, -0.1264236179284866091, 1.434547244040724534 ) ) ;
#1562 = AXIS2_PLACEMENT_3D ( 'NONE', #44292, #23233, #41393 ) ;
#1563 = CARTESIAN_POINT ( 'NONE',  ( 0.000000000000000000, 0.000000000000000000, 0.000000000000000000 ) ) ;
#1564 = ADVANCED_FACE ( 'NONE', ( #4001, #18623 ), #626, .T. ) ;
#1565 = CARTESIAN_POINT ( 'NONE',  ( 0.8107537697050253289, -0.1574803149606297803, 1.532972440944882608 ) ) ;
#1567 = CARTESIAN_POINT ( 'NONE',  ( 0.7185039370078739607, 0.000000000000000000, 4.498031496062992574 ) ) ;
#1566 = CARTESIAN_POINT ( 'NONE',  ( 0.8184489996385461152, 0.1487827445626105083, 1.979498570521418532 ) ) ;
#1568 = AXIS2_PLACEMENT_3D ( 'NONE', #36016, #3175, #19208 ) ;
#1569 = DIRECTION ( 'NONE',  ( 1.822029033848725028E-16, 0.000000000000000000, 1.000000000000000000 ) ) ;
#1570 = CARTESIAN_POINT ( 'NONE',  ( -0.1787899950787401604, 0.07578740162856664742, -0.07405724077823318263 ) ) ;
#1571 = FACE_BOUND ( 'NONE', #4322, .T. ) ;
#1572 = CARTESIAN_POINT ( 'NONE',  ( 1.054774247047244540, -0.07405724077823318263, 1.003937007820253413 ) ) ;
#1573 = CARTESIAN_POINT ( 'NONE',  ( 0.9500414927467377701, -0.1787899950787401604, 1.791338582623401177 ) ) ;
#1574 = CARTESIAN_POINT ( 'NONE',  ( 0.8759842519685039353, -0.1574803149606299191, 0.3051181101286932762 ) ) ;
#1575 = ORIENTED_EDGE ( 'NONE', *, *, #29905, .T. ) ;
#1576 = DIRECTION ( 'NONE',  ( 1.822029033848725028E-16, 0.000000000000000000, 1.000000000000000000 ) ) ;
#1577 = CARTESIAN_POINT ( 'NONE',  ( 1.614954907737318939E-16, 0.1574803149606340824, 0.4950787401574787139 ) ) ;
#1578 = CARTESIAN_POINT ( 'NONE',  ( 0.06523048226347956391, -1.658956692805858557, 0.1574803149606297803 ) ) ;
#1579 = CARTESIAN_POINT ( 'NONE',  ( -0.8107537697050253289, 0.1574803149606300301, 0.2485236219397170265 ) ) ;
#1580 = DIRECTION ( 'NONE',  ( -1.000000000000000000, 0.000000000000000000, 0.000000000000000000 ) ) ;
#1581 = CARTESIAN_POINT ( 'NONE',  ( 0.6971942568897637749, 2.189545951927499583E-17, 1.301673228292692830 ) ) ;
#1582 = CARTESIAN_POINT ( 'NONE',  ( 0.05769093565149619601, -0.07859528327913710422, 0.2521251929553415816 ) ) ;
#1583 = CARTESIAN_POINT ( 'NONE',  ( -0.1574803149606297803, -1.796751968503936814, 0.06523048226347956391 ) ) ;
#1584 = LINE ( 'NONE', #16237, #3828 ) ;
#1585 = CARTESIAN_POINT ( 'NONE',  ( -0.9500414927467378812, -0.1787899950787401604, 0.6053149605761579677 ) ) ;
#1586 = CARTESIAN_POINT ( 'NONE',  ( 0.000000000000000000, -0.09842519685039370636, 0.000000000000000000 ) ) ;
#1587 = DIRECTION ( 'NONE',  ( 0.000000000000000000, -1.000000000000000000, 0.000000000000000000 ) ) ;
#1588 = ORIENTED_EDGE ( 'NONE', *, *, #46677, .T. ) ;
#1590 = CARTESIAN_POINT ( 'NONE',  ( 0.1787899950787401604, -1.518700787347811554, -0.07405724077823318263 ) ) ;
#1589 = CARTESIAN_POINT ( 'NONE',  ( -0.1574803149606297803, -0.3695866140657014243, 0.06523048226347956391 ) ) ;
#1591 = CARTESIAN_POINT ( 'NONE',  ( -0.6971942568897648851, -0.07405724077823297447, 1.776574803095843924 ) ) ;
#1592 = EDGE_LOOP ( 'NONE', ( #42543, #7954, #19874, #27330 ) ) ;
#1593 = CARTESIAN_POINT ( 'NONE',  ( -0.6971942568897637749, 2.189545951927499583E-17, 0.5979330708123780092 ) ) ;
#1594 = ORIENTED_EDGE ( 'NONE', *, *, #10024, .F. ) ;
#1595 = FACE_OUTER_BOUND ( 'NONE', #26190, .T. ) ;
#1596 = CARTESIAN_POINT ( 'NONE',  ( -0.1377952755905511861, 0.1564960629921283985, -0.8070866141732283561 ) ) ;
#1597 = CARTESIAN_POINT ( 'NONE',  ( -0.07405724077823318263, -0.5749271178355379597, -0.1787899950787401604 ) ) ;
#1598 = CARTESIAN_POINT ( 'NONE',  ( 0.2035752408203165831, -0.08956008440634705137, -0.0002272480696794984621 ) ) ;
#1599 = DIRECTION ( 'NONE',  ( -1.000000000000000000, 0.000000000000000000, 0.000000000000000000 ) ) ;
#1600 = CIRCLE ( 'NONE', #42131, 0.1968503937007874127 ) ;
#1602 = CARTESIAN_POINT ( 'NONE',  ( -1.033464566929133799, 0.000000000000000000, 1.771653543199558811 ) ) ;
#1601 = AXIS2_PLACEMENT_3D ( 'NONE', #34251, #4042, #22736 ) ;
#1603 = CARTESIAN_POINT ( 'NONE',  ( -0.6971942568897626646, 0.07405724077823318263, 0.5118110235682844511 ) ) ;
#1604 = ( BOUNDED_SURFACE ( )  B_SPLINE_SURFACE ( 3, 2, ( 
 ( #21922, #6580, #35599 ),
 ( #46830, #47074, #47320 ),
 ( #24800, #2738, #2973 ),
 ( #32962, #20953, #28666 ),
 ( #32492, #39871, #25283 ),
 ( #32251, #36542, #10194 ) ),
 .UNSPECIFIED., .F., .F., .T. ) 
 B_SPLINE_SURFACE_WITH_KNOTS ( ( 4, 2, 4 ),
 ( 3, 3 ),
 ( 0.01651732063679904952, 0.01857756227444015001, 0.02063780391208129908 ),
 ( 0.000000000000000000, 1.000000000000000000 ),
 .UNSPECIFIED. ) 
 GEOMETRIC_REPRESENTATION_ITEM ( )  RATIONAL_B_SPLINE_SURFACE ( (
 ( 1.000000000000000000, 0.8047781231227479903, 1.000000000000000000),
 ( 1.000000000000000000, 0.8123782108661420365, 1.000000000000000000),
 ( 1.000000000000000000, 0.8190665102138239284, 1.000000000000000000),
 ( 1.000000000000000000, 0.8192358432839229598, 1.000000000000000000),
 ( 1.000000000000000000, 0.8126132624438909824, 1.000000000000000000),
 ( 1.000000000000000000, 0.8047712436238880773, 1.000000000000000000) ) ) 
 REPRESENTATION_ITEM ( '' )  SURFACE ( )  ) ;
#1605 = CARTESIAN_POINT ( 'NONE',  ( 0.07405724077823318263, -1.815084598150499273, 0.1787899950787401604 ) ) ;
#1606 = ORIENTED_EDGE ( 'NONE', *, *, #27421, .T. ) ;
#1607 = CARTESIAN_POINT ( 'NONE',  ( 0.1574803149606300023, 0.2512968553230416346, -0.3092734567177706229 ) ) ;
#1608 = CIRCLE ( 'NONE', #19992, 0.7972440944881888925 ) ;
#1609 = ADVANCED_FACE ( 'NONE', ( #15284, #29934 ), #13123, .F. ) ;
#1610 = CARTESIAN_POINT ( 'NONE',  ( -0.6971942568897637749, 2.189545951927499583E-17, 1.503444881836000002 ) ) ;
#1611 = EDGE_CURVE ( 'NONE', #8914, #32474, #33311, .T. ) ;
#1612 = CARTESIAN_POINT ( 'NONE',  ( 3.284318927891251994E-17, -1.491633858213953001, 0.1787899950787401882 ) ) ;
#1613 = DIRECTION ( 'NONE',  ( 1.000000000000000000, -0.000000000000000000, -0.000000000000000000 ) ) ;
#1614 = EDGE_CURVE ( 'NONE', #44803, #21841, #30633, .T. ) ;
#1615 = CARTESIAN_POINT ( 'NONE',  ( 0.8107537697050234415, -0.1574803149606297803, 0.1943897637795276023 ) ) ;
#1616 = CARTESIAN_POINT ( 'NONE',  ( 0.7185039370078739607, 1.928577636452523993E-17, 0.4625984251968504046 ) ) ;
#1617 = CARTESIAN_POINT ( 'NONE',  ( -0.1270800023317771588, -0.6653981402917066301, 0.1270800023317771588 ) ) ;
#1618 = CARTESIAN_POINT ( 'NONE',  ( -7.957671378281915615E-17, 0.1574803149606340824, -0.2923228346456709370 ) ) ;
#1619 = CARTESIAN_POINT ( 'NONE',  ( -0.7646288533564489232, -0.1113553986120547346, 1.245078740049952559 ) ) ;
#1620 = CARTESIAN_POINT ( 'NONE',  ( 0.7495606340400177148, -0.1264236179284866091, 0.5634842519147401640 ) ) ;
#1621 = CARTESIAN_POINT ( 'NONE',  ( 0.7495606340400177148, -0.1264236179284866091, 0.04675196845017354913 ) ) ;
#1623 = DIRECTION ( 'NONE',  ( -1.000000000000000000, -0.000000000000000000, 0.000000000000000000 ) ) ;
#1622 = CARTESIAN_POINT ( 'NONE',  ( -0.1574803149606299191, -0.3818897637795276023, 0.000000000000000000 ) ) ;
#1624 = CARTESIAN_POINT ( 'NONE',  ( 0.000000000000000000, 1.205361022782826802E-17, -0.09842519685039370636 ) ) ;
#1625 = VERTEX_POINT ( 'NONE', #45907 ) ;
#1626 = DIRECTION ( 'NONE',  ( 8.439683963172029406E-16, 0.2432573283306645739, -0.9699617890481188054 ) ) ;
#1627 = ADVANCED_FACE ( 'NONE', ( #42320 ), #19809, .T. ) ;
#1628 = CARTESIAN_POINT ( 'NONE',  ( -0.8759842519685039353, 0.1787899950787401882, 1.139271653489543290 ) ) ;
#1629 = CARTESIAN_POINT ( 'NONE',  ( 0.8107537697050253289, -0.1574803149606297803, 1.178641732283464583 ) ) ;
#1630 = DIRECTION ( 'NONE',  ( -1.000000000000000000, 0.000000000000000000, 0.000000000000000000 ) ) ;
#1631 = CARTESIAN_POINT ( 'NONE',  ( -1.002407869896990045, -0.1264236179284866091, 1.990649606245448844 ) ) ;
#1632 = DIRECTION ( 'NONE',  ( 1.000000000000000000, 0.000000000000000000, 0.000000000000000000 ) ) ;
#1633 = CIRCLE ( 'NONE', #30748, 0.1377952755905510751 ) ;
#1635 = DIRECTION ( 'NONE',  ( 1.000000000000000000, 0.000000000000000000, 0.000000000000000000 ) ) ;
#1634 = DIRECTION ( 'NONE',  ( 0.000000000000000000, 0.000000000000000000, 1.000000000000000000 ) ) ;
#1636 = DIRECTION ( 'NONE',  ( -0.000000000000000000, 1.000000000000000000, 0.000000000000000000 ) ) ;
#1637 = CARTESIAN_POINT ( 'NONE',  ( 0.1787899950787401604, -0.6131889763241887836, 0.07405724077823318263 ) ) ;
#1638 = VERTEX_POINT ( 'NONE', #30404 ) ;
#1639 = CONICAL_SURFACE ( 'NONE', #35330, 0.09842519685039370636, 0.9599310885968824758 ) ;
#1641 = CARTESIAN_POINT ( 'NONE',  ( -0.07117121207836790697, -0.08956324299011318713, 0.1404802767937309016 ) ) ;
#1640 = PRESENTATION_LAYER_ASSIGNMENT (  '', '', ( #28463 ) ) ;
#1642 = VERTEX_POINT ( 'NONE', #12881 ) ;
#1643 = DIRECTION ( 'NONE',  ( 0.000000000000000000, -1.000000000000000000, 0.000000000000000000 ) ) ;
#1644 = DIRECTION ( 'NONE',  ( 0.000000000000000000, 0.000000000000000000, -1.000000000000000000 ) ) ;
#1645 = CARTESIAN_POINT ( 'NONE',  ( -0.1264236179284866091, -1.777066929080094670, -0.1264236179284866091 ) ) ;
#1646 = CARTESIAN_POINT ( 'NONE',  ( -0.1787899950787401604, -0.8346456692375755493, -0.07405724077823318263 ) ) ;
#1647 = AXIS2_PLACEMENT_3D ( 'NONE', #13097, #20494, #12627 ) ;
#1648 = CARTESIAN_POINT ( 'NONE',  ( 0.1113553986120547346, -1.380905511811023834, -0.1113553986120547346 ) ) ;
#1649 = CARTESIAN_POINT ( 'NONE',  ( 0.9873396505805591694, -0.1113553986120547346, 1.294291338475149544 ) ) ;
#1650 = CARTESIAN_POINT ( 'NONE',  ( -0.7185039370078714072, 0.06523048226347728795, 1.867618110128693720 ) ) ;
#1651 = VERTEX_POINT ( 'NONE', #38262 ) ;
#1652 = EDGE_LOOP ( 'NONE', ( #44997, #42200, #22401, #33638 ) ) ;
#1653 = CARTESIAN_POINT ( 'NONE',  ( -0.8759842519685039353, 0.1787899950787401882, 1.690452755851748146 ) ) ;
#1654 = CARTESIAN_POINT ( 'NONE',  ( 0.8759842519685039353, -0.1787899950787401882, 1.828248031442299082 ) ) ;
#1655 = ORIENTED_EDGE ( 'NONE', *, *, #10241, .T. ) ;
#1656 = CARTESIAN_POINT ( 'NONE',  ( 1.033464566929134687, -0.06523048226347956391, 0.5585629921259840369 ) ) ;
#1657 = CARTESIAN_POINT ( 'NONE',  ( 1.002407869896990045, -0.1264236179284866091, 0.3764763778989925203 ) ) ;
#1658 = CARTESIAN_POINT ( 'NONE',  ( -0.6971942568897637749, 2.189545951927499583E-17, 1.341043307032850462 ) ) ;
#1659 = CARTESIAN_POINT ( 'NONE',  ( 0.7185039370078739607, 1.928577636452523993E-17, 0.6988188976377952555 ) ) ;
#1660 = CARTESIAN_POINT ( 'NONE',  ( -0.6971942568897626646, 0.07405724077823318263, 0.8661417322297003674 ) ) ;
#1661 = CARTESIAN_POINT ( 'NONE',  ( -1.054774247047244096, 0.000000000000000000, 0.1451771653005673179 ) ) ;
#1662 = CARTESIAN_POINT ( 'NONE',  ( 0.7185039370078746268, -0.06523048226347956391, 1.567421259842519454 ) ) ;
#1663 = CARTESIAN_POINT ( 'NONE',  ( -0.8019270111902717657, -0.1787899950787401604, 1.786417322780882388 ) ) ;
#1664 = CARTESIAN_POINT ( 'NONE',  ( -1.054774247047244540, -0.07405724077823318263, 0.06397637789899228433 ) ) ;
#1665 = CARTESIAN_POINT ( 'NONE',  ( -0.1572451146043662151, 0.09317026862874178139, 0.1946475616205573522 ) ) ;
#1666 = CARTESIAN_POINT ( 'NONE',  ( -0.7646288533564489232, -0.1113553986120547346, 1.766732283464566899 ) ) ;
#1667 = CARTESIAN_POINT ( 'NONE',  ( 1.002407869896990045, -0.1264236179284866091, 1.675688976324189117 ) ) ;
#1668 = CARTESIAN_POINT ( 'NONE',  ( 0.2033597642235094594, -0.09842519685039370636, -0.03144620579497787310 ) ) ;
#1669 = DIRECTION ( 'NONE',  ( 0.000000000000000000, 0.000000000000000000, 1.000000000000000000 ) ) ;
#1670 = ADVANCED_FACE ( 'NONE', ( #44953 ), #16006, .F. ) ;
#1671 = VECTOR ( 'NONE', #1986, 39.37007874015748854 ) ;
#1672 = AXIS2_PLACEMENT_3D ( 'NONE', #671, #18207, #43831 ) ;
#1673 = ORIENTED_EDGE ( 'NONE', *, *, #12185, .T. ) ;
#1674 = ADVANCED_FACE ( 'NONE', ( #4949 ), #46634, .T. ) ;
#1675 = ORIENTED_EDGE ( 'NONE', *, *, #35776, .T. ) ;
#1676 = AXIS2_PLACEMENT_3D ( 'NONE', #22841, #34127, #40789 ) ;
#1677 = VECTOR ( 'NONE', #22205, 39.37007874015748143 ) ;
#1678 = CARTESIAN_POINT ( 'NONE',  ( 0.07405724077823318263, -0.9773622046706458288, 0.1787899950787401604 ) ) ;
#1679 = CARTESIAN_POINT ( 'NONE',  ( -0.07405724077823318263, -1.228346456639149542, -0.1787899950787401604 ) ) ;
#1680 = CARTESIAN_POINT ( 'NONE',  ( -0.9412147342319837628, -0.1574803149606297803, 0.5930118110236221041 ) ) ;
#1681 = ( CONVERSION_BASED_UNIT ( 'INCH', #5279 ) LENGTH_UNIT ( ) NAMED_UNIT ( #38110 ) ) ;
#1682 = CARTESIAN_POINT ( 'NONE',  ( -0.1797182628040039087, -0.3528981402917069077, 0.07444174185955065859 ) ) ;
#1683 = CARTESIAN_POINT ( 'NONE',  ( -0.06523048226347956391, -1.781988188868851575, 0.1574803149606297803 ) ) ;
#1684 = CARTESIAN_POINT ( 'NONE',  ( -0.9412147342319837628, -0.1574803149606297803, 0.8587598424121576368 ) ) ;
#1685 = CARTESIAN_POINT ( 'NONE',  ( 0.1113553986120547346, 0.07578740157480315376, -0.1113553986120547346 ) ) ;
#1686 = CARTESIAN_POINT ( 'NONE',  ( 0.7495606340400177148, 0.1264236179284866091, 0.9424212597887559051 ) ) ;
#1688 = CARTESIAN_POINT ( 'NONE',  ( 0.1583744855326524870, -0.03901141430315739622, 0.1404421906569240930 ) ) ;
#1687 = CARTESIAN_POINT ( 'NONE',  ( 0.2360031691063811943, 0.1592377390492322742, -0.08759220388355022646 ) ) ;
#1689 = CARTESIAN_POINT ( 'NONE',  ( 0.7495606340400177148, 0.1264236179284866091, 1.970964566875370139 ) ) ;
#1690 = CARTESIAN_POINT ( 'NONE',  ( 0.7185039370078739607, 1.928577636452523993E-17, 0.2263779527559055260 ) ) ;
#1691 = CARTESIAN_POINT ( 'NONE',  ( 0.8759842519685039353, 0.000000000000000000, 4.498031496062992574 ) ) ;
#1692 = CARTESIAN_POINT ( 'NONE',  ( 0.07405724077823318263, -0.4114173227808823330, -0.1787899950787401604 ) ) ;
#1693 = CARTESIAN_POINT ( 'NONE',  ( 1.033464566929133799, 1.928577636452524610E-17, 4.498031496062992574 ) ) ;
#1694 = CARTESIAN_POINT ( 'NONE',  ( 0.1787899950787401604, -1.439960629867495401, 0.07405724077823318263 ) ) ;
#1695 = CIRCLE ( 'NONE', #17780, 0.09842519685039370636 ) ;
#1696 = CARTESIAN_POINT ( 'NONE',  ( -0.8019270111902717657, -0.1787899950787401604, 1.742125984198204858 ) ) ;
#1697 = VERTEX_POINT ( 'NONE', #27757 ) ;
#1698 = FACE_OUTER_BOUND ( 'NONE', #16346, .T. ) ;
#1699 = CARTESIAN_POINT ( 'NONE',  ( 0.8759842519685039353, -0.1787899950787401882, 1.434547244040724534 ) ) ;
#1700 = CARTESIAN_POINT ( 'NONE',  ( -0.6971942568897637749, 2.189545951927499583E-17, 0.5191929133320630774 ) ) ;
#1701 = AXIS2_PLACEMENT_3D ( 'NONE', #24854, #9540, #24162 ) ;
#1702 = AXIS2_PLACEMENT_3D ( 'NONE', #14220, #14450, #28368 ) ;
#1703 = CARTESIAN_POINT ( 'NONE',  ( -0.9500414927467378812, -0.1787899950787401604, 1.274606299158834277 ) ) ;
#1704 = CARTESIAN_POINT ( 'NONE',  ( 0.1583858528204731275, 0.1411902173418021211, -0.03633609477026231160 ) ) ;
#1705 = DIRECTION ( 'NONE',  ( -0.000000000000000000, 0.7880107536067207930, -0.6156614753256598460 ) ) ;
#1706 = CARTESIAN_POINT ( 'NONE',  ( 0.8759842519685039353, 0.1787899950787401882, 0.5487204723871811352 ) ) ;
#1707 = CARTESIAN_POINT ( 'NONE',  ( -0.9500414927467377701, 0.1787899950787401604, 0.5019685038832443214 ) ) ;
#1708 = CARTESIAN_POINT ( 'NONE',  ( -1.002407869896990045, 0.1264236179284866091, 0.8144685038832440993 ) ) ;
#1709 = FACE_OUTER_BOUND ( 'NONE', #29645, .T. ) ;
#1710 = ORIENTED_EDGE ( 'NONE', *, *, #13280, .T. ) ;
#1711 = PRODUCT ( 'ISO 4162 M5x10 Hex Flange Bolt', 'ISO 4162 M5x10 Hex Flange Bolt', '', ( #36993 ) ) ;
#1712 = FACE_OUTER_BOUND ( 'NONE', #19526, .T. ) ;
#1713 = AXIS2_PLACEMENT_3D ( 'NONE', #24114, #35138, #35369 ) ;
#1714 = CARTESIAN_POINT ( 'NONE',  ( -0.8759842519685039353, -0.1574803149606299191, 0.3543307086614173040 ) ) ;
#1715 = CARTESIAN_POINT ( 'NONE',  ( 0.6971942568897637749, 2.189545951927499583E-17, 1.188484251914740275 ) ) ;
#1716 = CARTESIAN_POINT ( 'NONE',  ( -0.03350987669894700538, -0.09851384946037776424, 0.2233477092115621898 ) ) ;
#1717 = CARTESIAN_POINT ( 'NONE',  ( -0.7185039370078739607, 1.928577636452523993E-17, 0.4921259841444416971 ) ) ;
#1718 = VERTEX_POINT ( 'NONE', #45433 ) ;
#1719 = EDGE_CURVE ( 'NONE', #3727, #47141, #38174, .T. ) ;
#1720 = CARTESIAN_POINT ( 'NONE',  ( -0.9500414927467378812, -0.1787899950787401604, 0.9645669290800953366 ) ) ;
#1721 = EDGE_CURVE ( 'NONE', #24716, #11036, #37626, .T. ) ;
#1722 = CARTESIAN_POINT ( 'NONE',  ( -1.002407869896990045, -0.1264236179284866091, 0.2140748030958428971 ) ) ;
#1723 = CARTESIAN_POINT ( 'NONE',  ( -0.1787899950787401604, -1.632997983977269030, -0.07405724077823318263 ) ) ;
#1724 = ORIENTED_EDGE ( 'NONE', *, *, #18503, .F. ) ;
#1725 = CARTESIAN_POINT ( 'NONE',  ( 0.3980944881889779130, 0.4370297686271517601, 0.6367018223237037589 ) ) ;
#1726 = CARTESIAN_POINT ( 'NONE',  ( 0.07405724077823318263, -0.6181102361667089040, 0.1787899950787401604 ) ) ;
#1727 = EDGE_CURVE ( 'NONE', #7028, #6659, #38498, .T. ) ;
#1728 = CARTESIAN_POINT ( 'NONE',  ( -0.2984771744461587883, -0.08441368980803264088, 1.020863600671442217 ) ) ;
#1729 = CARTESIAN_POINT ( 'NONE',  ( 1.002407869896990045, 0.1264236179284866091, 1.286909448765133801 ) ) ;
#1730 = EDGE_CURVE ( 'NONE', #47099, #3114, #36085, .T. ) ;
#1731 = CARTESIAN_POINT ( 'NONE',  ( 0.01230737760510407577, 0.1591122789105269553, -1.502406898952441074E-18 ) ) ;
#1732 = CARTESIAN_POINT ( 'NONE',  ( 0.2362204724409448509, 0.1574803149606299191, -1.186023622047243986 ) ) ;
#1733 = VECTOR ( 'NONE', #44365, 39.37007874015748143 ) ;
#1734 = DIRECTION ( 'NONE',  ( -1.000000000000000000, 0.000000000000000000, 0.000000000000000000 ) ) ;
#1735 = CARTESIAN_POINT ( 'NONE',  ( 0.6971942568897648851, 0.07405724077823318263, 1.574803149552536530 ) ) ;
#1736 = AXIS2_PLACEMENT_3D ( 'NONE', #14915, #22318, #30036 ) ;
#1737 = CARTESIAN_POINT ( 'NONE',  ( -0.07405724077823318263, 0.1091280002746981559, 0.1787899950787401604 ) ) ;
#1738 = ITEM_DEFINED_TRANSFORMATION ( 'NONE', 'NONE', #4067,  #20860 ) ;
#1739 = CARTESIAN_POINT ( 'NONE',  ( 0.002770643200454896322, -0.03669440867518906219, -0.1377943639823349942 ) ) ;
#1740 = CARTESIAN_POINT ( 'NONE',  ( 0.7495606340400177148, 0.1264236179284866091, 0.4699803149068661479 ) ) ;
#1741 = CARTESIAN_POINT ( 'NONE',  ( -1.054774247047244540, 0.07405724077823318263, 0.7381889763241898939 ) ) ;
#1743 = DIRECTION ( 'NONE',  ( 7.155734338404322954E-15, 0.000000000000000000, 1.000000000000000000 ) ) ;
#1742 = CARTESIAN_POINT ( 'NONE',  ( -0.1574803149606299191, -0.8149606299212598381, 0.000000000000000000 ) ) ;
#1745 = CARTESIAN_POINT ( 'NONE',  ( -0.7919991761111997430, -0.1498786536115133128, 1.986579935406608932 ) ) ;
#1744 = CARTESIAN_POINT ( 'NONE',  ( 0.1797182628040039087, -1.514315463126352901, -0.07444174185955065859 ) ) ;
#1746 = CARTESIAN_POINT ( 'NONE',  ( -9.642888182262618425E-18, -0.06692913375074074911, -0.1574803149606299191 ) ) ;
#1747 = CARTESIAN_POINT ( 'NONE',  ( 0.1113553986120547346, -0.4753937006798740206, 0.1113553986120547346 ) ) ;
#1748 = VECTOR ( 'NONE', #4428, 39.37007874015748143 ) ;
#1749 = CARTESIAN_POINT ( 'NONE',  ( -0.1264236179284866091, -0.3991141731745826982, -0.1264236179284866091 ) ) ;
#1750 = DIRECTION ( 'NONE',  ( 0.000000000000000000, 0.000000000000000000, 1.000000000000000000 ) ) ;
#1751 = CARTESIAN_POINT ( 'NONE',  ( 0.8759842519685039353, -0.1787899950787401882, 1.513287401521039355 ) ) ;
#1752 = CARTESIAN_POINT ( 'NONE',  ( 1.054774247047244540, 0.07405724077823318263, 1.796259842465920853 ) ) ;
#1753 = CARTESIAN_POINT ( 'NONE',  ( 0.9500414927467377701, 0.1787899950787401604, 0.4625984251430869665 ) ) ;
#1755 = ORIENTED_EDGE ( 'NONE', *, *, #21966, .F. ) ;
#1754 = DIRECTION ( 'NONE',  ( 0.000000000000000000, 1.000000000000000000, 0.000000000000000000 ) ) ;
#1756 = DIRECTION ( 'NONE',  ( 0.000000000000000000, 0.000000000000000000, -1.000000000000000000 ) ) ;
#1757 = DIRECTION ( 'NONE',  ( 0.8660254037844389297, 1.060575238724907285E-16, -0.4999999999999994449 ) ) ;
#1758 = CARTESIAN_POINT ( 'NONE',  ( 0.1264236179284866091, -0.02017716530056720692, -0.1264236179284866091 ) ) ;
#1759 = CARTESIAN_POINT ( 'NONE',  ( 1.002407869896990045, 0.1264236179284866091, 0.4207677164816693294 ) ) ;
#1760 = CARTESIAN_POINT ( 'NONE',  ( 0.7791120256548125234, -0.1328245026793817840, 0.03936940671680725506 ) ) ;
#1761 = CARTESIAN_POINT ( 'NONE',  ( -0.8759842519685039353, 0.000000000000000000, 0.000000000000000000 ) ) ;
#1762 = CARTESIAN_POINT ( 'NONE',  ( 0.8759842519685039353, 0.1574803149606299191, 0.8464566929133857665 ) ) ;
#1763 = CARTESIAN_POINT ( 'NONE',  ( -0.8759842519685039353, 0.1787899950787401882, 1.370570866087968520 ) ) ;
#1764 = CARTESIAN_POINT ( 'NONE',  ( 0.9873396505805591694, 0.1113553986120547346, 0.8316929132782993062 ) ) ;
#1765 = ORIENTED_EDGE ( 'NONE', *, *, #13397, .F. ) ;
#1766 = CARTESIAN_POINT ( 'NONE',  ( 0.6971942568897637749, 2.189545951927499583E-17, 1.070374015694267600 ) ) ;
#1767 = VERTEX_POINT ( 'NONE', #2534 ) ;
#1769 = CARTESIAN_POINT ( 'NONE',  ( 0.1787899950787401604, -1.326771653489542402, 0.07405724077823318263 ) ) ;
#1768 = CARTESIAN_POINT ( 'NONE',  ( 0.1574803149606300301, -1.102854330601134913, 0.06523048226347956391 ) ) ;
#1770 = CARTESIAN_POINT ( 'NONE',  ( -0.7185039370078746268, -0.06523048226347956391, 0.6126968502861739330 ) ) ;
#1771 = DIRECTION ( 'NONE',  ( 0.000000000000000000, 0.000000000000000000, 1.000000000000000000 ) ) ;
#1772 = CARTESIAN_POINT ( 'NONE',  ( 0.7495606340400177148, -0.1264236179284866091, 1.700295275536787498 ) ) ;
#1773 = CARTESIAN_POINT ( 'NONE',  ( -0.9412147342319837628, 0.1574803149606300301, 1.316437007874015519 ) ) ;
#1774 = CARTESIAN_POINT ( 'NONE',  ( -0.8107537697050254399, 0.1574803149606300301, 1.154035432963338659 ) ) ;
#1775 = DIRECTION ( 'NONE',  ( 1.822029033848725028E-16, 0.000000000000000000, 1.000000000000000000 ) ) ;
#1776 = CARTESIAN_POINT ( 'NONE',  ( 0.8759842519685039353, -0.1787899950787401882, 0.1353346456155279653 ) ) ;
#1777 = CARTESIAN_POINT ( 'NONE',  ( 0.7185039370078746268, 0.06523048226347956391, 1.395177165246804130 ) ) ;
#1778 = EDGE_LOOP ( 'NONE', ( #39006, #25813, #3590, #30137 ) ) ;
#1779 = ORIENTED_EDGE ( 'NONE', *, *, #33305, .F. ) ;
#1780 = VECTOR ( 'NONE', #20781, 39.37007874015748143 ) ;
#1781 = CARTESIAN_POINT ( 'NONE',  ( -0.07857503534280656232, -0.08918665060152188018, -0.2400663896720299229 ) ) ;
#1782 = CARTESIAN_POINT ( 'NONE',  ( 1.054774247047244540, -0.07405724077823318263, 0.6938976377415123631 ) ) ;
#1783 = CARTESIAN_POINT ( 'NONE',  ( -0.6971942568897648851, -0.07405724077823297447, 1.619094488135213838 ) ) ;
#1784 = CARTESIAN_POINT ( 'NONE',  ( -0.1574803149606299191, -0.1358267715460163283, 0.000000000000000000 ) ) ;
#1785 = CARTESIAN_POINT ( 'NONE',  ( 0.1476377952755906220, -0.4075443641102559078, -0.9311509272141712534 ) ) ;
#1786 = TOROIDAL_SURFACE ( 'NONE', #4809, 0.01968503937007873988, 0.009842519685039369942 ) ;
#1787 = ORIENTED_EDGE ( 'NONE', *, *, #21920, .F. ) ;
#1788 = ( BOUNDED_CURVE ( )  B_SPLINE_CURVE ( 2, ( #25686, #25908, #14180, #33358, #3134, #36463, #35974, #32410, #3620 ),
 .UNSPECIFIED., .F., .F. ) 
 B_SPLINE_CURVE_WITH_KNOTS ( ( 3, 2, 2, 2, 3 ),
 ( 0.1600000000000000033, 0.1625000000000000056, 0.1650000000000000078, 0.1675000000000000100, 0.1700000000000000122 ),
 .UNSPECIFIED. ) 
 CURVE ( )  GEOMETRIC_REPRESENTATION_ITEM ( )  RATIONAL_B_SPLINE_CURVE ( ( 1.000000000000000000, 0.9238795325112869605, 1.000000000000000000, 0.9238795325112869605, 1.000000000000000000, 0.9238795325112869605, 1.000000000000000000, 0.9238795325112869605, 1.000000000000000000 ) ) 
 REPRESENTATION_ITEM ( '' )  ) ;
#1789 = EDGE_CURVE ( 'NONE', #46167, #19219, #12552, .T. ) ;
#1790 = CARTESIAN_POINT ( 'NONE',  ( -1.033464566929133799, 0.000000000000000000, 0.2362204723334177248 ) ) ;
#1791 = CARTESIAN_POINT ( 'NONE',  ( 0.1049868766404236653, 0.4668427075568369333, -0.7022306805398673690 ) ) ;
#1792 = CARTESIAN_POINT ( 'NONE',  ( -0.1264236179284866091, -1.113805070591442847, 0.1264236179284866091 ) ) ;
#1793 = ORIENTED_EDGE ( 'NONE', *, *, #46477, .T. ) ;
#1794 = CARTESIAN_POINT ( 'NONE',  ( -0.1787899950787401604, -0.03740157474938609478, 0.07405724077823318263 ) ) ;
#1795 = EDGE_LOOP ( 'NONE', ( #46640, #41069, #14398, #46541 ) ) ;
#1796 = ADVANCED_FACE ( 'NONE', ( #42541 ), #24822, .T. ) ;
#1797 = ORIENTED_EDGE ( 'NONE', *, *, #45159, .F. ) ;
#1798 = EDGE_CURVE ( 'NONE', #8209, #31760, #18021, .T. ) ;
#1799 = LINE ( 'NONE', #12615, #43945 ) ;
#1800 = CARTESIAN_POINT ( 'NONE',  ( 0.1574803149606299191, 0.000000000000000000, -0.1574803149606298636 ) ) ;
#1801 = CARTESIAN_POINT ( 'NONE',  ( 0.9873396505805591694, -0.1113553986120547346, 1.855314960629921295 ) ) ;
#1802 = CARTESIAN_POINT ( 'NONE',  ( -0.1264236179284866091, -0.5516732282926929409, 0.1264236179284866091 ) ) ;
#1803 = CARTESIAN_POINT ( 'NONE',  ( -0.9500414927467377701, -0.1787899950787401604, 0.1377952755367876370 ) ) ;
#1804 = CARTESIAN_POINT ( 'NONE',  ( -0.9873396505805591694, -0.1113553986120547346, 1.107283464566929165 ) ) ;
#1805 = CARTESIAN_POINT ( 'NONE',  ( -0.1270800023317771588, -1.216579242653911486, 0.1270800023317771588 ) ) ;
#1806 = CARTESIAN_POINT ( 'NONE',  ( 0.1746296719420869226, 0.1299212598425197041, -0.002904701756485846172 ) ) ;
#1807 = CARTESIAN_POINT ( 'NONE',  ( 1.002407869896990045, -0.1264236179284866091, 1.085137795221826629 ) ) ;
#1808 = DIRECTION ( 'NONE',  ( 1.000000000000000000, 0.000000000000000000, -1.822029033848725275E-16 ) ) ;
#1809 = EDGE_CURVE ( 'NONE', #39475, #34571, #39007, .T. ) ;
#1810 = CARTESIAN_POINT ( 'NONE',  ( 0.7646288533564489232, 0.1113553986120547346, 1.560039370078740273 ) ) ;
#1812 = FACE_OUTER_BOUND ( 'NONE', #12611, .T. ) ;
#1811 = CARTESIAN_POINT ( 'NONE',  ( -0.6195511811023656223, 0.6102362204724407491, 0.9891732283464566011 ) ) ;
#1813 = CARTESIAN_POINT ( 'NONE',  ( 0.8107537697050254399, -0.1574803149606297803, 0.4601377951680635792 ) ) ;
#1814 = CARTESIAN_POINT ( 'NONE',  ( -0.7185039370078746268, 0.06523048226347956391, 1.631397637687747926 ) ) ;
#1815 = CARTESIAN_POINT ( 'NONE',  ( -0.9873396505805591694, -0.1113553986120547346, 0.7037401573727875004 ) ) ;
#1816 = CARTESIAN_POINT ( 'NONE',  ( 0.6971942568897637749, 2.189545951927499583E-17, 0.9473425196312755814 ) ) ;
#1817 = CARTESIAN_POINT ( 'NONE',  ( 0.8019270111902716547, 0.1787899950787401604, 1.771653543253322249 ) ) ;
#1818 = CARTESIAN_POINT ( 'NONE',  ( 0.8107537697050234415, -0.1574803149606297803, 0.2632874014672759722 ) ) ;
#1819 = ORIENTED_EDGE ( 'NONE', *, *, #20179, .T. ) ;
#1820 = DIRECTION ( 'NONE',  ( -5.724375810226263558E-16, -0.6156614753256592909, -0.7880107536067213481 ) ) ;
#1821 = CARTESIAN_POINT ( 'NONE',  ( 1.031250533963468774, 0.03915069072625195629, 0.03937005934756545450 ) ) ;
#1822 = CARTESIAN_POINT ( 'NONE',  ( 0.1113553986120547346, -1.764763779420031486, -0.1113553986120547346 ) ) ;
#1823 = CARTESIAN_POINT ( 'NONE',  ( -0.8759842519685039353, -0.1574803149606299191, 0.2657480313885358103 ) ) ;
#1824 = CARTESIAN_POINT ( 'NONE',  ( 0.8019270111902717657, -0.1787899950787401604, 1.269685039316314601 ) ) ;
#1825 = VERTEX_POINT ( 'NONE', #7084 ) ;
#1826 = FACE_OUTER_BOUND ( 'NONE', #11922, .T. ) ;
#1827 = CARTESIAN_POINT ( 'NONE',  ( -0.1787899950787401604, 0.1545275591088816070, -0.07405724077823318263 ) ) ;
#1828 = LINE ( 'NONE', #34439, #32941 ) ;
#1829 = CARTESIAN_POINT ( 'NONE',  ( -0.6971942568897626646, -0.07405724077823297447, 0.5561023621509617598 ) ) ;
#1830 = DIRECTION ( 'NONE',  ( 1.000000000000000000, 0.000000000000000000, 0.000000000000000000 ) ) ;
#1831 = CARTESIAN_POINT ( 'NONE',  ( 0.1574803149606299191, 0.3740157480314960647, 1.004692544842683111 ) ) ;
#1832 = CYLINDRICAL_SURFACE ( 'NONE', #7128, 0.1574803149606299191 ) ;
#1833 = CARTESIAN_POINT ( 'NONE',  ( -0.1264236179284866091, -1.585137795221826629, -0.1264236179284866091 ) ) ;
#1834 = CARTESIAN_POINT ( 'NONE',  ( -0.9500414927467378812, 0.1787899950787401604, 1.058070866087969186 ) ) ;
#1835 = EDGE_LOOP ( 'NONE', ( #32627, #33041, #45588, #11414 ) ) ;
#1836 = CARTESIAN_POINT ( 'NONE',  ( -0.6971942568897648851, 0.07405724077823318263, 0.9842519684501743749 ) ) ;
#1837 = B_SPLINE_CURVE_WITH_KNOTS ( 'NONE', 3,
 ( #37491, #573, #18339, #36558, #40819, #40589, #3718, #43727, #10930, #44651, #25551, #103, #11868, #14749 ),
 .UNSPECIFIED., .F., .F.,
 ( 4, 2, 2, 2, 2, 2, 4 ),
 ( 0.000000000000000000, 0.1250000000000001110, 0.2500000000000002220, 0.3750000000000004441, 0.4375000000000004441, 0.5000000000000004441, 1.000000000000000000 ),
 .UNSPECIFIED. ) ;
#1838 = CARTESIAN_POINT ( 'NONE',  ( -1.054774247047244540, 0.07405724077823318263, 0.6594488188438737408 ) ) ;
#1839 = ORIENTED_EDGE ( 'NONE', *, *, #26366, .T. ) ;
#1840 = EDGE_CURVE ( 'NONE', #13298, #37374, #35390, .T. ) ;
#1841 = CARTESIAN_POINT ( 'NONE',  ( -0.2133366555409255683, 0.1723185650271337466, -0.3044102143376714031 ) ) ;
#1842 = CARTESIAN_POINT ( 'NONE',  ( 0.8107537697050254399, -0.1574803149606297803, 1.808562992125984481 ) ) ;
#1843 = LINE ( 'NONE', #23903, #35866 ) ;
#1844 = CARTESIAN_POINT ( 'NONE',  ( 3.284318927891251994E-17, -0.7151830233473485121, 0.1787899950787401882 ) ) ;
#1845 = CARTESIAN_POINT ( 'NONE',  ( 0.03156423158163212256, -0.08956068939121496209, -0.1858659549881094553 ) ) ;
#1846 = VERTEX_POINT ( 'NONE', #36083 ) ;
#1847 = CARTESIAN_POINT ( 'NONE',  ( 0.7185039370078739607, 1.928577636452523993E-17, 0.8169291338582678197 ) ) ;
#1848 = ADVANCED_FACE ( 'NONE', ( #21708 ), #3242, .F. ) ;
#1849 = DIRECTION ( 'NONE',  ( 0.000000000000000000, -1.000000000000000000, 0.000000000000000000 ) ) ;
#1850 = CARTESIAN_POINT ( 'NONE',  ( -1.054774247047244096, 0.000000000000000000, 0.5339566928596221063 ) ) ;
#1851 = CARTESIAN_POINT ( 'NONE',  ( -0.7185039370078746268, -0.06523048226347956391, 0.3863188976377952000 ) ) ;
#1852 = ORIENTED_EDGE ( 'NONE', *, *, #42070, .T. ) ;
#1853 = TOROIDAL_SURFACE ( 'NONE', #17148, 0.7874015748031496509, 0.04921259842519685318 ) ;
#1854 = CARTESIAN_POINT ( 'NONE',  ( -0.1264236179284866091, -1.496555118056472677, 0.1264236179284866091 ) ) ;
#1855 = CARTESIAN_POINT ( 'NONE',  ( -0.2559055118110236671, 0.1226799225465883270, -0.2993403469937337413 ) ) ;
#1856 = FILL_AREA_STYLE ('',( #14599 ) ) ;
#1857 = DIRECTION ( 'NONE',  ( 0.000000000000000000, 1.000000000000000000, 1.224646799147353947E-16 ) ) ;
#1858 = CARTESIAN_POINT ( 'NONE',  ( 1.033464566929133799, 0.000000000000000000, 0.5610236220472440971 ) ) ;
#1859 = CARTESIAN_POINT ( 'NONE',  ( 0.07444174185955046430, -0.6826225497405251641, -0.1797182628040039087 ) ) ;
#1860 = CARTESIAN_POINT ( 'NONE',  ( 0.7185039370078739607, 1.928577636452523993E-17, 0.9350393700787401619 ) ) ;
#1861 = CARTESIAN_POINT ( 'NONE',  ( -0.8107537697050253289, -0.1574803149606297803, 1.247539369971212508 ) ) ;
#1862 = CARTESIAN_POINT ( 'NONE',  ( 0.000000000000000000, 0.000000000000000000, -0.3149606299212598381 ) ) ;
#1863 = CARTESIAN_POINT ( 'NONE',  ( 0.8019270111902716547, 0.1787899950787401604, 0.07381889758403178958 ) ) ;
#1865 = CARTESIAN_POINT ( 'NONE',  ( 0.7185039370078766252, -0.06523048226348168721, 1.754429133750741832 ) ) ;
#1864 = CARTESIAN_POINT ( 'NONE',  ( 0.1574803149606300301, -0.3646653543307084577, 0.06523048226347956391 ) ) ;
#1866 = CARTESIAN_POINT ( 'NONE',  ( 0.2559055118110236116, -0.1477471161312047254, -0.3149606299212598381 ) ) ;
#1867 = ORIENTED_EDGE ( 'NONE', *, *, #8153, .F. ) ;
#1868 = DIRECTION ( 'NONE',  ( -0.8191520442890007914, -0.4519843998600331925, 0.3531289150159138690 ) ) ;
#1869 = CARTESIAN_POINT ( 'NONE',  ( 1.033464566929134687, 0.06523048226347956391, 1.035925196850394192 ) ) ;
#1871 = CARTESIAN_POINT ( 'NONE',  ( -0.9300548450171354231, -0.1677133419385780366, 1.989159733827547516 ) ) ;
#1870 = CARTESIAN_POINT ( 'NONE',  ( 0.1574803149606299191, 0.4668427075568346574, -0.7022306805398661478 ) ) ;
#1872 = DIRECTION ( 'NONE',  ( 1.000000000000000000, 0.000000000000000000, 0.000000000000000000 ) ) ;
#1873 = EDGE_CURVE ( 'NONE', #12155, #6854, #31803, .T. ) ;
#1875 = CARTESIAN_POINT ( 'NONE',  ( -0.8107537697050254399, -0.1574803149606297803, 1.956200787294048338 ) ) ;
#1874 = CARTESIAN_POINT ( 'NONE',  ( 0.7185039370078746268, -0.06523048226347956391, 0.5733267715460159675 ) ) ;
#1876 = DIRECTION ( 'NONE',  ( -1.000000000000000000, 0.000000000000000000, 0.000000000000000000 ) ) ;
#1877 = ORIENTED_EDGE ( 'NONE', *, *, #5750, .T. ) ;
#1878 = DIRECTION ( 'NONE',  ( 0.000000000000000000, -1.000000000000000000, 0.000000000000000000 ) ) ;
#1879 = CIRCLE ( 'NONE', #1117, 0.09842519685039370636 ) ;
#1880 = AXIS2_PLACEMENT_3D ( 'NONE', #16154, #30324, #19006 ) ;
#1881 = DIRECTION ( 'NONE',  ( 1.822029033848725028E-16, 0.000000000000000000, 1.000000000000000000 ) ) ;
#1882 = CARTESIAN_POINT ( 'NONE',  ( -1.002407869896990045, 0.1264236179284866091, 1.055610236166708793 ) ) ;
#1883 = CARTESIAN_POINT ( 'NONE',  ( 0.6971942568897637749, 2.189545951927499583E-17, 0.8686023621509606496 ) ) ;
#1884 = ORIENTED_EDGE ( 'NONE', *, *, #37161, .F. ) ;
#1885 = CARTESIAN_POINT ( 'NONE',  ( 0.1574803149606299746, 0.7443365962042343131, -3.523993443072799270 ) ) ;
#1886 = CARTESIAN_POINT ( 'NONE',  ( -0.3551574803149606385, -2.130889186148732174E-17, 0.000000000000000000 ) ) ;
#1887 = CARTESIAN_POINT ( 'NONE',  ( 0.07405724077823318263, -1.720472440891118726, 0.1787899950787401604 ) ) ;
#1888 = CARTESIAN_POINT ( 'NONE',  ( 0.1264236179284866091, -0.9749015747493857686, 0.1264236179284866091 ) ) ;
#1889 = CARTESIAN_POINT ( 'NONE',  ( -0.1574803149606297803, -1.442421259842518566, 0.06523048226347956391 ) ) ;
#1890 = CARTESIAN_POINT ( 'NONE',  ( 1.033464566929134687, -0.06523048226347956391, 1.218011810916095117 ) ) ;
#1891 = CARTESIAN_POINT ( 'NONE',  ( -0.7185039370078739607, 1.928577636452523993E-17, 1.870078740049952559 ) ) ;
#1892 = EDGE_LOOP ( 'NONE', ( #25261, #10836, #6956, #14618 ) ) ;
#1893 = VERTEX_POINT ( 'NONE', #8023 ) ;
#1894 = CARTESIAN_POINT ( 'NONE',  ( -0.6971942568897648851, 0.07405724077823318263, 1.894685039316315489 ) ) ;
#1895 = EDGE_LOOP ( 'NONE', ( #12411, #29985, #27803, #34322 ) ) ;
#1896 = CARTESIAN_POINT ( 'NONE',  ( -9.642888182262618425E-18, -1.366141732175937040, -0.1574803149606299191 ) ) ;
#1897 = CARTESIAN_POINT ( 'NONE',  ( 1.002407869896990045, 0.1264236179284866091, 0.5044291338045039375 ) ) ;
#1898 = CARTESIAN_POINT ( 'NONE',  ( -1.054774247047244096, 0.000000000000000000, 1.400098425143086800 ) ) ;
#1899 = CARTESIAN_POINT ( 'NONE',  ( -0.7495606340400177148, -0.1264236179284866091, 0.9916338582139527791 ) ) ;
#1900 = EDGE_CURVE ( 'NONE', #30530, #3057, #37258, .T. ) ;
#1901 = CARTESIAN_POINT ( 'NONE',  ( -0.7495606340400177148, -0.1264236179284866091, 0.1697834645131657827 ) ) ;
#1902 = ( BOUNDED_CURVE ( )  B_SPLINE_CURVE ( 2, ( #11378, #19011, #7762, #8470, #44878, #788, #26953, #37476, #15452 ),
 .UNSPECIFIED., .F., .T. ) 
 B_SPLINE_CURVE_WITH_KNOTS ( ( 3, 2, 2, 2, 3 ),
 ( 0.7600000000000000089, 0.7624999999999999556, 0.7650000000000000133, 0.7674999999999999600, 0.7700000000000000178 ),
 .UNSPECIFIED. ) 
 CURVE ( )  GEOMETRIC_REPRESENTATION_ITEM ( )  RATIONAL_B_SPLINE_CURVE ( ( 1.000000000000000000, 0.9238795325112869605, 1.000000000000000000, 0.9238795325112869605, 1.000000000000000000, 0.9238795325112869605, 1.000000000000000000, 0.9238795325112869605, 1.000000000000000000 ) ) 
 REPRESENTATION_ITEM ( '' )  ) ;
#1903 = ADVANCED_FACE ( 'NONE', ( #8262 ), #36341, .T. ) ;
#1904 = CARTESIAN_POINT ( 'NONE',  ( -1.033464566929133799, 0.000000000000000000, 0.5118110235145196807 ) ) ;
#1905 = CARTESIAN_POINT ( 'NONE',  ( -0.7495606340400177148, -0.1264236179284866091, 1.744586614119464807 ) ) ;
#1906 = CARTESIAN_POINT ( 'NONE',  ( -1.002407869896990045, 0.1264236179284866091, 0.1107283464029293202 ) ) ;
#1907 = CARTESIAN_POINT ( 'NONE',  ( 1.033464566929136907, -0.06523048226347749612, 1.414862204616882835 ) ) ;
#1908 = CARTESIAN_POINT ( 'NONE',  ( -0.7185039370078739607, 1.928577636452523993E-17, 1.761811023622047223 ) ) ;
#1909 = DIRECTION ( 'NONE',  ( 1.000000000000000000, 0.000000000000000000, -1.822029033848725275E-16 ) ) ;
#1910 = CARTESIAN_POINT ( 'NONE',  ( 0.8019270111902716547, -0.1787899950787401604, 1.747047244040724312 ) ) ;
#1911 = CARTESIAN_POINT ( 'NONE',  ( 0.2063724842062263920, -0.09842519685039370636, -0.01079757893850124065 ) ) ;
#1912 = LINE ( 'NONE', #35237, #37906 ) ;
#1913 = EDGE_CURVE ( 'NONE', #45437, #5036, #32752, .T. ) ;
#1914 = VERTEX_POINT ( 'NONE', #37030 ) ;
#1915 = VERTEX_POINT ( 'NONE', #33707 ) ;
#1916 = AXIS2_PLACEMENT_3D ( 'NONE', #43620, #18692, #26145 ) ;
#1917 = CARTESIAN_POINT ( 'NONE',  ( -0.1264236179284866091, -1.033956692859621995, -0.1264236179284866091 ) ) ;
#1918 = CARTESIAN_POINT ( 'NONE',  ( -0.1787899950787401604, -1.262795275536788386, -0.07405724077823318263 ) ) ;
#1919 = CARTESIAN_POINT ( 'NONE',  ( -0.7185039370078739607, 1.928577636452523993E-17, 0.5807086614173228023 ) ) ;
#1920 = CARTESIAN_POINT ( 'NONE',  ( 1.002407869896990045, -0.1264236179284866091, 0.4109251967966299213 ) ) ;
#1921 = CARTESIAN_POINT ( 'NONE',  ( 0.1797182628040039087, -0.4906934158822578995, -0.07444174185955065859 ) ) ;
#1922 = CARTESIAN_POINT ( 'NONE',  ( -9.642888182262618425E-18, -1.799212598317669443, -0.1574803149606299191 ) ) ;
#1923 = CARTESIAN_POINT ( 'NONE',  ( -0.8759842519685039353, 0.1574803149606299191, 0.7578740156405039397 ) ) ;
#1924 = CARTESIAN_POINT ( 'NONE',  ( 0.1113553986120547346, -0.01279527559055118092, 0.1113553986120547346 ) ) ;
#1925 = CARTESIAN_POINT ( 'NONE',  ( -1.094772975963752103E-17, -0.1727362204186775607, -0.1787899950787401882 ) ) ;
#1926 = CARTESIAN_POINT ( 'NONE',  ( 1.002407869896990045, 0.1264236179284866091, 0.9325787401037164415 ) ) ;
#1928 = DIRECTION ( 'NONE',  ( -1.000000000000000000, 0.000000000000000000, 0.000000000000000000 ) ) ;
#1927 = DIRECTION ( 'NONE',  ( -1.000000000000000000, -0.000000000000000000, 0.000000000000000000 ) ) ;
#1929 = CARTESIAN_POINT ( 'NONE',  ( 1.033464566929134687, -0.06523048226347956391, 0.07627952745152805081 ) ) ;
#1930 = CARTESIAN_POINT ( 'NONE',  ( 0.5236220472440944462, 4.616380251121755931E-17, 0.000000000000000000 ) ) ;
#1931 = CARTESIAN_POINT ( 'NONE',  ( -0.1787899950787401604, -0.4015748030958427028, -0.07405724077823318263 ) ) ;
#1932 = DIRECTION ( 'NONE',  ( -1.000000000000000000, 3.469446951953613794E-15, 1.144917494144692682E-16 ) ) ;
#1933 = CARTESIAN_POINT ( 'NONE',  ( 0.1787899950787401604, -1.400590551127339323, 0.07405724077823318263 ) ) ;
#1934 = CARTESIAN_POINT ( 'NONE',  ( 0.7495606340400177148, -0.1264236179284866091, 0.3666338582139531677 ) ) ;
#1935 = CYLINDRICAL_SURFACE ( 'NONE', #4743, 0.1574803149606299191 ) ;
#1936 = CARTESIAN_POINT ( 'NONE',  ( -0.8019270111902717657, -0.1787899950787401604, 1.938976377898990799 ) ) ;
#1937 = ORIENTED_EDGE ( 'NONE', *, *, #42883, .T. ) ;
#1938 = VECTOR ( 'NONE', #4599, 39.37007874015748143 ) ;
#1939 = CARTESIAN_POINT ( 'NONE',  ( -0.9500414927467378812, -0.1787899950787401604, 1.515748031442299526 ) ) ;
#1940 = FACE_OUTER_BOUND ( 'NONE', #45893, .T. ) ;
#1941 = EDGE_CURVE ( 'NONE', #14850, #38506, #16810, .T. ) ;
#1942 = CARTESIAN_POINT ( 'NONE',  ( 0.8759842519685039353, -0.1787899950787401882, 1.395177165300567124 ) ) ;
#1943 = B_SPLINE_CURVE_WITH_KNOTS ( 'NONE', 3,
 ( #19400, #45017, #30232, #8373, #34051, #12230, #936, #26137, #26853, #5019, #40705, #30459, #44544, #4520, #22759, #37613, #44087, #33341, #23001 ),
 .UNSPECIFIED., .F., .F.,
 ( 4, 2, 2, 1, 2, 2, 2, 2, 2, 4 ),
 ( 0.000000000000000000, 0.2500000000000015543, 0.3750000000000021649, 0.4375000000000022760, 0.4687500000000021649, 0.5000000000000021094, 0.6250000000000014433, 0.6875000000000008882, 0.7500000000000004441, 1.000000000000000000 ),
 .UNSPECIFIED. ) ;
#1944 = VECTOR ( 'NONE', #31591, 39.37007874015748143 ) ;
#1946 = CARTESIAN_POINT ( 'NONE',  ( -0.1574803149606299191, -0.4008464425712929824, -0.9238935802775073425 ) ) ;
#1945 = CONICAL_SURFACE ( 'NONE', #26464, 0.09842519685039310962, 0.7853981633972314524 ) ;
#1947 = EDGE_CURVE ( 'NONE', #45939, #23245, #19092, .T. ) ;
#1948 = CARTESIAN_POINT ( 'NONE',  ( -0.7495606340400177148, 0.1264236179284866091, 0.5536417322297008115 ) ) ;
#1949 = CARTESIAN_POINT ( 'NONE',  ( 1.054774247047244540, 0.07405724077823318263, 0.1082677164816695514 ) ) ;
#1950 = CARTESIAN_POINT ( 'NONE',  ( -0.6971942568897648851, -0.07405724077823297447, 1.186023621993481658 ) ) ;
#1951 = CARTESIAN_POINT ( 'NONE',  ( 0.1251454632067010020, -0.09843574689532874622, -0.1277354705666547130 ) ) ;
#1952 = CARTESIAN_POINT ( 'NONE',  ( 0.8019270111902716547, -0.1787899950787401604, 0.5659448818360001132 ) ) ;
#1953 = CARTESIAN_POINT ( 'NONE',  ( -0.7495606340400177148, -0.1264236179284866091, 0.5191929133320630774 ) ) ;
#1954 = EDGE_CURVE ( 'NONE', #35241, #13693, #27859, .T. ) ;
#1955 = CARTESIAN_POINT ( 'NONE',  ( 0.000000000000000000, 0.000000000000000000, 0.000000000000000000 ) ) ;
#1956 = EDGE_LOOP ( 'NONE', ( #15134, #37598, #45628, #21040 ) ) ;
#1957 = CARTESIAN_POINT ( 'NONE',  ( -1.033464566929134687, 0.06523048226347956391, 0.2485236220472441526 ) ) ;
#1958 = CARTESIAN_POINT ( 'NONE',  ( 1.002407869896990045, -0.1264236179284866091, 1.321358267662771757 ) ) ;
#1959 = CARTESIAN_POINT ( 'NONE',  ( -0.2191150658379515670, -0.09851385013792676726, 0.09090310240979053436 ) ) ;
#1960 = ORIENTED_EDGE ( 'NONE', *, *, #29711, .T. ) ;
#1961 = EDGE_CURVE ( 'NONE', #23847, #13064, #10940, .T. ) ;
#1962 = CARTESIAN_POINT ( 'NONE',  ( 0.8759842519685039353, 0.000000000000000000, 4.498031496062992574 ) ) ;
#1963 = CARTESIAN_POINT ( 'NONE',  ( -0.8019270111902717657, -0.1787899950787401604, 0.9990157479777320715 ) ) ;
#1964 = PRODUCT_RELATED_PRODUCT_CATEGORY ( 'part', '', ( #26085 ) ) ;
#1965 = CARTESIAN_POINT ( 'NONE',  ( -0.6971942568897637749, 2.189545951927499583E-17, 0.1993110235682838682 ) ) ;
#1966 = VERTEX_POINT ( 'NONE', #18807 ) ;
#1967 = CARTESIAN_POINT ( 'NONE',  ( -0.8759842519685039353, 0.1574803149606299191, 0.1673228345381423399 ) ) ;
#1968 = CARTESIAN_POINT ( 'NONE',  ( -0.1787899950787401604, -0.6673228345919050009, 0.07405724077823318263 ) ) ;
#1969 = DIRECTION ( 'NONE',  ( 0.000000000000000000, 0.000000000000000000, -1.000000000000000000 ) ) ;
#1970 = ORIENTED_EDGE ( 'NONE', *, *, #42883, .F. ) ;
#1971 = CARTESIAN_POINT ( 'NONE',  ( 1.002407869896990045, 0.1264236179284866091, 1.365649606245448844 ) ) ;
#1972 = AXIS2_PLACEMENT_3D ( 'NONE', #43308, #35675, #44016 ) ;
#1973 = CARTESIAN_POINT ( 'NONE',  ( 0.008396861977782204417, 0.1523390671602133373, 0.01173154688194899542 ) ) ;
#1974 = CARTESIAN_POINT ( 'NONE',  ( -0.1787899950787401604, -0.8248031495525351975, 0.07405724077823318263 ) ) ;
#1975 = CYLINDRICAL_SURFACE ( 'NONE', #2691, 0.1574803149606299191 ) ;
#1976 = CARTESIAN_POINT ( 'NONE',  ( 0.8759842519685039353, -0.1787899950787401882, 1.587106299158834721 ) ) ;
#1977 = VECTOR ( 'NONE', #17777, 39.37007874015748143 ) ;
#1978 = CARTESIAN_POINT ( 'NONE',  ( 0.07405724077823318263, 0.07467918137706039405, 0.1787899950787401604 ) ) ;
#1979 = CARTESIAN_POINT ( 'NONE',  ( 0.1787899950787401604, 0.1348425197388028463, -0.07405724077823318263 ) ) ;
#1980 = ITEM_DEFINED_TRANSFORMATION ( 'NONE', 'NONE', #13260,  #20860 ) ;
#1981 = DIRECTION ( 'NONE',  ( 1.822029033848725028E-16, 0.000000000000000000, 1.000000000000000000 ) ) ;
#1982 = CARTESIAN_POINT ( 'NONE',  ( 1.054774247047244096, 0.000000000000000000, 0.4945866141194645849 ) ) ;
#1983 = DIMENSIONAL_EXPONENTS ( 1.000000000000000000, 0.000000000000000000, 0.000000000000000000, 0.000000000000000000, 0.000000000000000000, 0.000000000000000000, 0.000000000000000000 ) ;
#1984 = CARTESIAN_POINT ( 'NONE',  ( -0.6971942568897637749, 2.189545951927499583E-17, 0.8735236219934803259 ) ) ;
#1986 = DIRECTION ( 'NONE',  ( 0.000000000000000000, 0.7880107536067212370, -0.6156614753256591799 ) ) ;
#1985 = CARTESIAN_POINT ( 'NONE',  ( -0.1113553986120547346, -0.8592519685039370358, -0.1113553986120547346 ) ) ;
#1987 = CARTESIAN_POINT ( 'NONE',  ( -0.07444174185955065859, -1.529079242653912152, 0.1797182628040039087 ) ) ;
#1988 = CARTESIAN_POINT ( 'NONE',  ( -0.9412147342319837628, 0.1574803149606300301, 1.031003936900347639 ) ) ;
#1989 = CARTESIAN_POINT ( 'NONE',  ( 0.8019270111902717657, 0.1787899950787401604, 1.535433070812378675 ) ) ;
#1990 = CARTESIAN_POINT ( 'NONE',  ( 1.054774247047244540, -0.07405724077823318263, 1.791338582623401177 ) ) ;
#1991 = CARTESIAN_POINT ( 'NONE',  ( 0.8759842519685039353, -0.1787899950787401882, 0.3666338582139531677 ) ) ;
#1992 = ORIENTED_EDGE ( 'NONE', *, *, #20083, .T. ) ;
#1994 = EDGE_CURVE ( 'NONE', #30756, #31965, #2268, .T. ) ;
#1993 = CARTESIAN_POINT ( 'NONE',  ( 0.000000000000000000, 0.1299212598425196763, 0.000000000000000000 ) ) ;
#1995 = B_SPLINE_CURVE_WITH_KNOTS ( 'NONE', 3,
 ( #2475, #32211, #28634, #2244, #28147, #28384, #42952, #35792, #16864, #2934, #43191, #10160, #6068, #10403, #13060, #42707, #25005, #9925, #20926, #39132, #6547, #24769 ),
 .UNSPECIFIED., .F., .F.,
 ( 4, 2, 2, 2, 2, 2, 2, 2, 2, 2, 4 ),
 ( 0.000000000000000000, 0.06250000000000008327, 0.1250000000000001665, 0.1875000000000002498, 0.2500000000000003331, 0.3750000000000002776, 0.5000000000000002220, 0.6250000000000001110, 0.7500000000000001110, 0.8750000000000000000, 1.000000000000000000 ),
 .UNSPECIFIED. ) ;
#1996 = DIRECTION ( 'NONE',  ( 0.000000000000000000, 0.000000000000000000, -1.000000000000000000 ) ) ;
#1997 = CARTESIAN_POINT ( 'NONE',  ( 0.4736248074375440931, 1.890321945096787193, -4.194630839571732217 ) ) ;
#1998 = CARTESIAN_POINT ( 'NONE',  ( -0.1264236179284866091, 0.1077755906049446960, -0.1264236179284866091 ) ) ;
#1999 = CARTESIAN_POINT ( 'NONE',  ( -0.9412147342319837628, 0.1574803149606300301, 0.1747047244094490082 ) ) ;
#2000 = CARTESIAN_POINT ( 'NONE',  ( 0.9500414927467378812, -0.1787899950787401604, 0.5265748030958428139 ) ) ;
#2001 = CARTESIAN_POINT ( 'NONE',  ( 0.7185039370078746268, -0.06523048226347956391, 0.07135826771653554224 ) ) ;
#2002 = DIRECTION ( 'NONE',  ( -1.000000000000000000, 0.000000000000000000, 0.000000000000000000 ) ) ;
#2003 = CARTESIAN_POINT ( 'NONE',  ( 0.7185039370078746268, 0.06523048226347956391, 0.2239173228346459099 ) ) ;
#2004 = CARTESIAN_POINT ( 'NONE',  ( -0.8019270111902717657, -0.1787899950787401604, 1.427165354276944687 ) ) ;
#2005 = CARTESIAN_POINT ( 'NONE',  ( 0.9412147342319837628, 0.1574803149606300301, 0.8735236219397174429 ) ) ;
#2006 = ORIENTED_EDGE ( 'NONE', *, *, #33798, .F. ) ;
#2007 = EDGE_CURVE ( 'NONE', #36271, #46609, #4854, .T. ) ;
#2008 = CARTESIAN_POINT ( 'NONE',  ( 0.8759842519685039353, 0.1787899950787401882, 1.021161417269070837 ) ) ;
#2009 = EDGE_LOOP ( 'NONE', ( #35399, #38692, #14943 ) ) ;
#2010 = CARTESIAN_POINT ( 'NONE',  ( 0.1787899950787401604, -1.361220472387181690, -0.07405724077823318263 ) ) ;
#2011 = CARTESIAN_POINT ( 'NONE',  ( -0.8759842519685039353, 0.1574803149606299191, 0.5610236219397165547 ) ) ;
#2012 = DIRECTION ( 'NONE',  ( 0.000000000000000000, 1.000000000000000000, 0.000000000000000000 ) ) ;
#2013 = CARTESIAN_POINT ( 'NONE',  ( -0.8759842519685039353, 0.1574803149606299191, 1.397637795275590511 ) ) ;
#2014 = AXIS2_PLACEMENT_3D ( 'NONE', #36944, #44817, #11317 ) ;
#2015 = DIRECTION ( 'NONE',  ( 0.000000000000000000, 0.000000000000000000, -1.000000000000000000 ) ) ;
#2016 = CARTESIAN_POINT ( 'NONE',  ( 0.1578366172104690157, 0.2043672459940823471, -0.3136338785705632959 ) ) ;
#2017 = CARTESIAN_POINT ( 'NONE',  ( 0.6971942568897626646, 0.07405724077823318263, 0.1624015747493861017 ) ) ;
#2018 = CARTESIAN_POINT ( 'NONE',  ( 0.8107537697050253289, 0.1574803149606300301, 1.429625984144440531 ) ) ;
#2019 = VERTEX_POINT ( 'NONE', #7328 ) ;
#2020 = VERTEX_POINT ( 'NONE', #816 ) ;
#2021 = CARTESIAN_POINT ( 'NONE',  ( -0.8759842519685039353, 0.000000000000000000, 0.000000000000000000 ) ) ;
#2022 = CARTESIAN_POINT ( 'NONE',  ( -0.1235961452251415349, -0.09842519685039370636, -0.2140748031496062798 ) ) ;
#2023 = CARTESIAN_POINT ( 'NONE',  ( 0.6971942568897626646, 0.07405724077823318263, 0.7135826771115916234 ) ) ;
#2024 = CARTESIAN_POINT ( 'NONE',  ( -1.002407869896990045, 0.1264236179284866091, 1.641240157426551161 ) ) ;
#2025 = CARTESIAN_POINT ( 'NONE',  ( -0.1113553986120547346, -0.2588582676090082635, -0.1113553986120547346 ) ) ;
#2026 = EDGE_LOOP ( 'NONE', ( #6463, #36198, #44216, #7732 ) ) ;
#2027 = ORIENTED_EDGE ( 'NONE', *, *, #23171, .T. ) ;
#2028 = DIRECTION ( 'NONE',  ( -1.000000000000000000, 0.000000000000000000, -0.000000000000000000 ) ) ;
#2029 = CARTESIAN_POINT ( 'NONE',  ( 0.07405724077823318263, -1.106423180827663444, 0.1787899950787401604 ) ) ;
#2030 = ORIENTED_EDGE ( 'NONE', *, *, #1727, .T. ) ;
#2031 = CARTESIAN_POINT ( 'NONE',  ( 0.1787899950787401604, -0.1013779527021420185, 0.07405724077823318263 ) ) ;
#2032 = ORIENTED_EDGE ( 'NONE', *, *, #20257, .F. ) ;
#2033 = ORIENTED_EDGE ( 'NONE', *, *, #22550, .F. ) ;
#2034 = CARTESIAN_POINT ( 'NONE',  ( -0.1574803149606299191, -0.4812165006432426173, -0.8611016091043821596 ) ) ;
#2035 = CARTESIAN_POINT ( 'NONE',  ( -0.8759842519685039353, -0.1574803149606299191, 1.456692913385826849 ) ) ;
#2036 = CARTESIAN_POINT ( 'NONE',  ( 1.033464566929134687, -0.06523048226347956391, 1.818405511811023167 ) ) ;
#2037 = CARTESIAN_POINT ( 'NONE',  ( 0.1264236179284866091, -0.5713582676627716461, -0.1264236179284866091 ) ) ;
#2038 = CARTESIAN_POINT ( 'NONE',  ( -0.6971942568897648851, 0.07405724077823318263, 0.3986220471903311746 ) ) ;
#2039 = CARTESIAN_POINT ( 'NONE',  ( -0.7185039370078746268, -0.06523048226347956391, 1.055610236220473341 ) ) ;
#2040 = CARTESIAN_POINT ( 'NONE',  ( -0.07444174185955065859, -1.189512313520053821, -0.1797182628040039087 ) ) ;
#2041 = CARTESIAN_POINT ( 'NONE',  ( -0.2559055118110236116, 0.1477471161312031434, -0.1122047244094468571 ) ) ;
#2042 = CARTESIAN_POINT ( 'NONE',  ( 0.6971942568897648851, -0.07405724077823297447, 1.072834645615528659 ) ) ;
#2043 = CARTESIAN_POINT ( 'NONE',  ( 0.7495606340400177148, -0.1264236179284866091, 0.2042322834108035723 ) ) ;
#2045 = ADVANCED_FACE ( 'NONE', ( #29886 ), #21945, .T. ) ;
#2044 = DIRECTION ( 'NONE',  ( 0.000000000000000000, 0.000000000000000000, -1.000000000000000000 ) ) ;
#2046 = CARTESIAN_POINT ( 'NONE',  ( 0.8759842519685039353, -0.1574803149606299191, 1.535433070866141669 ) ) ;
#2048 = CARTESIAN_POINT ( 'NONE',  ( 0.9412147342319837628, 0.1574803149606300301, 1.710137795275591843 ) ) ;
#2047 = CARTESIAN_POINT ( 'NONE',  ( 0.8483274250313047604, 0.1565762035813350328, 1.978884771285821742 ) ) ;
#2049 = CARTESIAN_POINT ( 'NONE',  ( 1.033464566929133799, 0.000000000000000000, 1.456692913278299084 ) ) ;
#2050 = CARTESIAN_POINT ( 'NONE',  ( -0.3161444924769509779, 0.8918838478058892516, -1.034309214090478823 ) ) ;
#2051 = CARTESIAN_POINT ( 'NONE',  ( -1.033464566929134687, -0.06523048226347956391, 1.651082677057826853 ) ) ;
#2052 = ADVANCED_FACE ( 'NONE', ( #15008 ), #44201, .T. ) ;
#2053 = CARTESIAN_POINT ( 'NONE',  ( 0.000000000000000000, 0.4666052258408008302, -0.7025346432751023995 ) ) ;
#2054 = CARTESIAN_POINT ( 'NONE',  ( 0.6971942568897648851, -0.07405724077823297447, 0.9498031495525356416 ) ) ;
#2055 = CARTESIAN_POINT ( 'NONE',  ( 0.8759842519685039353, -0.1787899950787401882, 1.946358267662771757 ) ) ;
#2056 = CARTESIAN_POINT ( 'NONE',  ( 0.9873396505805591694, -0.1113553986120547346, 0.3887795274515282729 ) ) ;
#2057 = VERTEX_POINT ( 'NONE', #16188 ) ;
#2058 = DIRECTION ( 'NONE',  ( 0.000000000000000000, 0.000000000000000000, 1.000000000000000000 ) ) ;
#2059 = EDGE_CURVE ( 'NONE', #13671, #3164, #7934, .T. ) ;
#2060 = LINE ( 'NONE', #30862, #32086 ) ;
#2061 = CARTESIAN_POINT ( 'NONE',  ( 0.1113553986120547346, -1.695866141624755796, 0.1113553986120547346 ) ) ;
#2062 = CARTESIAN_POINT ( 'NONE',  ( -1.033464566929134687, 0.06523048226347956391, 0.2780511809948349455 ) ) ;
#2063 = CARTESIAN_POINT ( 'NONE',  ( 0.3425196850393700809, -0.08090551181102362266, 1.098083891755157578E-17 ) ) ;
#2064 = CARTESIAN_POINT ( 'NONE',  ( 0.6971942568897648851, -0.07405724077823297447, 1.304133858213953667 ) ) ;
#2065 = ADVANCED_FACE ( 'NONE', ( #27224 ), #1502, .F. ) ;
#2066 = CARTESIAN_POINT ( 'NONE',  ( 0.1178667752584772188, -0.09842519685039369248, 0.2173826564421467711 ) ) ;
#2067 = CARTESIAN_POINT ( 'NONE',  ( 0.1574803149606299191, -1.779527559055118058, -1.928577636452523993E-17 ) ) ;
#2068 = CARTESIAN_POINT ( 'NONE',  ( -1.033464566929133799, 0.000000000000000000, 1.860236220472440971 ) ) ;
#2069 = ( BOUNDED_CURVE ( )  B_SPLINE_CURVE ( 2, ( #25128, #14583, #3562, #46683, #43801, #3789, #24900, #18406, #17931 ),
 .UNSPECIFIED., .F., .T. ) 
 B_SPLINE_CURVE_WITH_KNOTS ( ( 3, 2, 2, 2, 3 ),
 ( 0.1400000000000000133, 0.1424999999999999878, 0.1449999999999999900, 0.1474999999999999922, 0.1499999999999999944 ),
 .UNSPECIFIED. ) 
 CURVE ( )  GEOMETRIC_REPRESENTATION_ITEM ( )  RATIONAL_B_SPLINE_CURVE ( ( 1.000000000000000000, 0.9238795325112869605, 1.000000000000000000, 0.9238795325112869605, 1.000000000000000000, 0.9238795325112869605, 1.000000000000000000, 0.9238795325112869605, 1.000000000000000000 ) ) 
 REPRESENTATION_ITEM ( '' )  ) ;
#2070 = CARTESIAN_POINT ( 'NONE',  ( -1.054774247047244096, 0.000000000000000000, 0.6520669290800944484 ) ) ;
#2071 = CARTESIAN_POINT ( 'NONE',  ( -1.033464566929133799, 0.000000000000000000, 0.2854330708661417804 ) ) ;
#2072 = LINE ( 'NONE', #13565, #23069 ) ;
#2073 = ORIENTED_EDGE ( 'NONE', *, *, #24705, .F. ) ;
#2074 = ORIENTED_EDGE ( 'NONE', *, *, #27847, .F. ) ;
#2075 = CARTESIAN_POINT ( 'NONE',  ( -0.1264236179284866091, -1.703248031442299304, -0.1264236179284866091 ) ) ;
#2076 = CARTESIAN_POINT ( 'NONE',  ( -0.9500414927467378812, -0.1787899950787401604, 1.043307086560409269 ) ) ;
#2077 = CARTESIAN_POINT ( 'NONE',  ( -0.9500414927467378812, -0.1787899950787401604, 1.943897637741510254 ) ) ;
#2078 = ORIENTED_EDGE ( 'NONE', *, *, #29473, .F. ) ;
#2079 = FACE_OUTER_BOUND ( 'NONE', #5846, .T. ) ;
#2080 = CARTESIAN_POINT ( 'NONE',  ( 0.7646288533564489232, -0.1113553986120547346, 1.806102362204724532 ) ) ;
#2081 = CARTESIAN_POINT ( 'NONE',  ( 0.000000000000000000, 0.000000000000000000, -0.1377952755905511861 ) ) ;
#2082 = ORIENTED_EDGE ( 'NONE', *, *, #29973, .F. ) ;
#2083 = CARTESIAN_POINT ( 'NONE',  ( -0.05855107416953937022, -0.08956097176436082774, -0.1736406213399021847 ) ) ;
#2084 = DIRECTION ( 'NONE',  ( -2.392722035830075028E-16, 0.000000000000000000, -1.000000000000000000 ) ) ;
#2085 = ORIENTED_EDGE ( 'NONE', *, *, #38033, .T. ) ;
#2086 = CARTESIAN_POINT ( 'NONE',  ( 0.6195511811023610704, 0.6102362204724403050, 0.5167322834645649010 ) ) ;
#2087 = DIRECTION ( 'NONE',  ( 0.000000000000000000, -1.000000000000000000, 0.000000000000000000 ) ) ;
#2088 = CARTESIAN_POINT ( 'NONE',  ( -0.8019270111902717657, 0.1787899950787401604, 0.5462598424659214080 ) ) ;
#2089 = CARTESIAN_POINT ( 'NONE',  ( 0.8759842519685039353, 0.1574803149606299191, 1.348425196742866206 ) ) ;
#2090 = ORIENTED_EDGE ( 'NONE', *, *, #33751, .T. ) ;
#2091 = CARTESIAN_POINT ( 'NONE',  ( -1.054774247047244540, 0.07405724077823318263, 1.683070866087970074 ) ) ;
#2092 = CARTESIAN_POINT ( 'NONE',  ( -0.1264236179284866091, -1.545767716481669218, -0.1264236179284866091 ) ) ;
#2093 = LINE ( 'NONE', #31355, #18026 ) ;
#2094 = VECTOR ( 'NONE', #47331, 39.37007874015748854 ) ;
#2095 = CARTESIAN_POINT ( 'NONE',  ( 0.1797182628040039087, -0.6924650694255656269, 0.07444174185955046430 ) ) ;
#2096 = CARTESIAN_POINT ( 'NONE',  ( 0.9873396505805591694, -0.1113553986120547346, 0.9498031496062993018 ) ) ;
#2097 = CARTESIAN_POINT ( 'NONE',  ( -0.9412147342319837628, -0.1574803149606297803, 1.173720472333417586 ) ) ;
#2098 = CARTESIAN_POINT ( 'NONE',  ( 0.9500414927467378812, -0.1787899950787401604, 0.6496062991588353874 ) ) ;
#2100 = CARTESIAN_POINT ( 'NONE',  ( -0.06162495753422155692, -0.09842519685039370636, 0.1485290488906215733 ) ) ;
#2099 = CARTESIAN_POINT ( 'NONE',  ( 0.1113553986120547346, -0.4360236220472440971, -0.1113553986120547346 ) ) ;
#2101 = DIRECTION ( 'NONE',  ( 0.000000000000000000, 0.000000000000000000, 1.000000000000000000 ) ) ;
#2102 = ORIENTED_EDGE ( 'NONE', *, *, #35592, .F. ) ;
#2103 = CARTESIAN_POINT ( 'NONE',  ( -9.642888182262618425E-18, 0.04133858267716535029, -0.1574803149606299191 ) ) ;
#2104 = CARTESIAN_POINT ( 'NONE',  ( -0.8759842519685039353, -0.1787899950787401882, 1.080216535379306952 ) ) ;
#2105 = CARTESIAN_POINT ( 'NONE',  ( 0.9873396505805591694, 0.1113553986120547346, 1.038385826771653475 ) ) ;
#2107 = CARTESIAN_POINT ( 'NONE',  ( 0.4620708661417344820, 0.6102362204724408601, 0.5854071585544579071 ) ) ;
#2106 = CARTESIAN_POINT ( 'NONE',  ( 0.1377952755905511861, 0.1574803149606299191, -0.8070866141732283561 ) ) ;
#2108 = DIRECTION ( 'NONE',  ( 0.000000000000000000, 8.673617379884035472E-16, 1.000000000000000000 ) ) ;
#2109 = EDGE_CURVE ( 'NONE', #33977, #31956, #23129, .T. ) ;
#2110 = DIRECTION ( 'NONE',  ( 1.000000000000000000, 0.000000000000000000, -1.822029033848725275E-16 ) ) ;
#2111 = DIRECTION ( 'NONE',  ( 0.000000000000000000, -0.000000000000000000, 1.000000000000000000 ) ) ;
#2112 = CARTESIAN_POINT ( 'NONE',  ( -0.1264236179284866091, -0.5959645668753701386, -0.1264236179284866091 ) ) ;
#2113 = LINE ( 'NONE', #5940, #4706 ) ;
#2114 = ORIENTED_EDGE ( 'NONE', *, *, #26641, .T. ) ;
#2115 = CARTESIAN_POINT ( 'NONE',  ( 0.8759842519685039353, 0.1574803149606299191, 1.161417322834645605 ) ) ;
#2116 = CARTESIAN_POINT ( 'NONE',  ( 0.7495606340400177148, -0.1264236179284866091, 0.7554133857730077617 ) ) ;
#2117 = EDGE_CURVE ( 'NONE', #30877, #31109, #35949, .T. ) ;
#2118 = VERTEX_POINT ( 'NONE', #8978 ) ;
#2119 = CARTESIAN_POINT ( 'NONE',  ( 0.7185039370078739607, 1.928577636452523993E-17, 1.525590551181102317 ) ) ;
#2120 = CARTESIAN_POINT ( 'NONE',  ( -0.7185039370078739607, 1.928577636452523993E-17, 0.5413385826771653919 ) ) ;
#2121 = CARTESIAN_POINT ( 'NONE',  ( 0.1787899950787401604, -1.789370078686394194, -0.07405724077823318263 ) ) ;
#2122 = CARTESIAN_POINT ( 'NONE',  ( -0.1787899950787401882, -1.029035433017102319, 0.000000000000000000 ) ) ;
#2123 = CARTESIAN_POINT ( 'NONE',  ( 0.06523048226347956391, -1.393208661417322469, 0.1574803149606297803 ) ) ;
#2124 = CARTESIAN_POINT ( 'NONE',  ( 1.033464566929134687, -0.06523048226347956391, 1.257381889656253193 ) ) ;
#2125 = CARTESIAN_POINT ( 'NONE',  ( 0.1602931993194444682, 0.1591122789105269553, 0.000000000000000000 ) ) ;
#2126 = VECTOR ( 'NONE', #1756, 39.37007874015748143 ) ;
#2127 = ORIENTED_EDGE ( 'NONE', *, *, #36636, .T. ) ;
#2128 = CARTESIAN_POINT ( 'NONE',  ( -1.054774247047244540, -0.07405724077823318263, 1.874999999946236784 ) ) ;
#2129 = CARTESIAN_POINT ( 'NONE',  ( 0.9500414927467378812, 0.1787899950787401604, 1.845472440891119392 ) ) ;
#2130 = ORIENTED_EDGE ( 'NONE', *, *, #32542, .F. ) ;
#2131 = CYLINDRICAL_SURFACE ( 'NONE', #6486, 0.3912448816427545051 ) ;
#2132 = CARTESIAN_POINT ( 'NONE',  ( -0.8759842519685039353, -0.1787899950787401882, 1.547736220418677089 ) ) ;
#2133 = DIRECTION ( 'NONE',  ( 1.000000000000000000, 0.000000000000000000, -1.822029033848725275E-16 ) ) ;
#2134 = CARTESIAN_POINT ( 'NONE',  ( -0.6971942568897637749, 2.189545951927499583E-17, 0.9867125983714331028 ) ) ;
#2135 = AXIS2_PLACEMENT_3D ( 'NONE', #14937, #21886, #25004 ) ;
#2136 = CARTESIAN_POINT ( 'NONE',  ( -1.054774247047244096, 0.000000000000000000, 0.2239173227808822775 ) ) ;
#2137 = CYLINDRICAL_SURFACE ( 'NONE', #29140, 0.07874015748031498729 ) ;
#2138 = CARTESIAN_POINT ( 'NONE',  ( -1.054774247047244096, 0.000000000000000000, 1.719980314906866203 ) ) ;
#2139 = CARTESIAN_POINT ( 'NONE',  ( 0.1574803149606299191, 1.086379535891623949, -0.03715491745706125948 ) ) ;
#2140 = CARTESIAN_POINT ( 'NONE',  ( -0.8107537697050253289, -0.1574803149606297803, 1.690452755905512916 ) ) ;
#2141 = CARTESIAN_POINT ( 'NONE',  ( -0.8759842519685039353, 0.000000000000000000, 0.000000000000000000 ) ) ;
#2142 = CARTESIAN_POINT ( 'NONE',  ( -0.07405724077823318263, -0.2452027083867192869, 0.1787899950787401604 ) ) ;
#2143 = CARTESIAN_POINT ( 'NONE',  ( 1.054774247047244096, 0.000000000000000000, 1.719980314906866203 ) ) ;
#2144 = CARTESIAN_POINT ( 'NONE',  ( -0.02999430697247586555, -0.09842519685039370636, -0.1860644942534716850 ) ) ;
#2145 = DIRECTION ( 'NONE',  ( 0.000000000000000000, 0.000000000000000000, 1.000000000000000000 ) ) ;
#2146 = EDGE_CURVE ( 'NONE', #36896, #18734, #9944, .T. ) ;
#2147 = ADVANCED_BREP_SHAPE_REPRESENTATION ( 'Pivot Pin', ( #20948, #20860 ), #10178 ) ;
#2148 = ORIENTED_EDGE ( 'NONE', *, *, #3089, .F. ) ;
#2149 = CARTESIAN_POINT ( 'NONE',  ( -0.8759842519685039353, 0.1787899950787401882, 1.296751968450173154 ) ) ;
#2150 = EDGE_LOOP ( 'NONE', ( #36178, #13805, #10108, #5274 ) ) ;
#2151 = CARTESIAN_POINT ( 'NONE',  ( -0.1264236179284866091, -1.102854330654897685, 0.1264236179284866091 ) ) ;
#2152 = CARTESIAN_POINT ( 'NONE',  ( 0.1264236179284866091, -1.284940944828125930, 0.1264236179284866091 ) ) ;
#2153 = CIRCLE ( 'NONE', #15974, 0.1574803149606299191 ) ;
#2154 = CYLINDRICAL_SURFACE ( 'NONE', #8738, 0.1003937007874010356 ) ;
#2155 = CARTESIAN_POINT ( 'NONE',  ( -0.07444174185955065859, -0.5448272741499744498, 0.1797182628040039087 ) ) ;
#2156 = CARTESIAN_POINT ( 'NONE',  ( 0.1574803149606300301, -1.772145669183811334, 0.06523048226347956391 ) ) ;
#2157 = CARTESIAN_POINT ( 'NONE',  ( -0.8107537697050253289, 0.1574803149606300301, 0.8390748030420787096 ) ) ;
#2158 = CARTESIAN_POINT ( 'NONE',  ( -0.7185039370078746268, 0.06523048226347956391, 0.6569881889763781180 ) ) ;
#2159 = CARTESIAN_POINT ( 'NONE',  ( -0.1113553986120547346, 0.04625984251968504046, -0.1113553986120547346 ) ) ;
#2160 = CARTESIAN_POINT ( 'NONE',  ( 0.6971942568897637749, 2.189545951927499583E-17, 0.9867125983714331028 ) ) ;
#2161 = VECTOR ( 'NONE', #24206, 39.37007874015748143 ) ;
#2162 = EDGE_CURVE ( 'NONE', #18566, #33555, #16421, .T. ) ;
#2164 = DIRECTION ( 'NONE',  ( 7.051687499798870116E-15, 0.000000000000000000, 1.000000000000000000 ) ) ;
#2163 = LINE ( 'NONE', #46478, #34704 ) ;
#2165 = CARTESIAN_POINT ( 'NONE',  ( 0.9500414927467378812, -0.1787899950787401604, 1.909448818843873186 ) ) ;
#2166 = CARTESIAN_POINT ( 'NONE',  ( 0.7185039370078739607, 1.928577636452523993E-17, 0.1870078740157480324 ) ) ;
#2167 = CARTESIAN_POINT ( 'NONE',  ( 0.8759842519685039353, 0.000000000000000000, 4.498031496062992574 ) ) ;
#2168 = CARTESIAN_POINT ( 'NONE',  ( 0.1787899950787401604, -0.6131889763241887836, -0.07405724077823318263 ) ) ;
#2169 = CARTESIAN_POINT ( 'NONE',  ( -1.094772975963752103E-17, -1.427657480261196987, -0.1787899950787401882 ) ) ;
#2170 = ( BOUNDED_CURVE ( )  B_SPLINE_CURVE ( 2, ( #31566, #46147, #23887, #5903, #16463, #38259, #41824, #24358, #6121 ),
 .UNSPECIFIED., .F., .T. ) 
 B_SPLINE_CURVE_WITH_KNOTS ( ( 3, 2, 2, 2, 3 ),
 ( 0.4899999999999999911, 0.4924999999999999933, 0.4949999999999999956, 0.4974999999999999978, 0.5000000000000000000 ),
 .UNSPECIFIED. ) 
 CURVE ( )  GEOMETRIC_REPRESENTATION_ITEM ( )  RATIONAL_B_SPLINE_CURVE ( ( 1.000000000000000000, 0.9238795325112869605, 1.000000000000000000, 0.9238795325112869605, 1.000000000000000000, 0.9238795325112869605, 1.000000000000000000, 0.9238795325112869605, 1.000000000000000000 ) ) 
 REPRESENTATION_ITEM ( '' )  ) ;
#2171 = CARTESIAN_POINT ( 'NONE',  ( -0.8759842519685039353, 0.000000000000000000, 0.000000000000000000 ) ) ;
#2172 = CARTESIAN_POINT ( 'NONE',  ( -1.002407869896990045, -0.1264236179284866091, 1.946358267662771757 ) ) ;
#2173 = ORIENTED_EDGE ( 'NONE', *, *, #32989, .F. ) ;
#2174 = CARTESIAN_POINT ( 'NONE',  ( -1.002407869896990045, -0.1264236179284866091, 1.400098425143086800 ) ) ;
#2175 = CARTESIAN_POINT ( 'NONE',  ( 0.6971942568897648851, -0.07405724077823297447, 1.348425196796630976 ) ) ;
#2176 = DIRECTION ( 'NONE',  ( 0.000000000000000000, -1.000000000000000000, 0.000000000000000000 ) ) ;
#2177 = CARTESIAN_POINT ( 'NONE',  ( -1.002407869896990045, 0.1264236179284866091, 0.5831692912848189803 ) ) ;
#2178 = CARTESIAN_POINT ( 'NONE',  ( 1.054774247047244096, 0.000000000000000000, 0.06643700782025216411 ) ) ;
#2179 = CARTESIAN_POINT ( 'NONE',  ( -1.054774247047244096, 0.000000000000000000, 1.163877952702141672 ) ) ;
#2180 = CARTESIAN_POINT ( 'NONE',  ( 0.09061490859345046334, -0.09842521672346266071, -0.1541267623450696400 ) ) ;
#2181 = CARTESIAN_POINT ( 'NONE',  ( 0.9500414927467377701, -0.1787899950787401604, 0.6102362204186774219 ) ) ;
#2182 = CARTESIAN_POINT ( 'NONE',  ( -1.054774247047244540, -0.07405724077823318263, 0.5314960629383620461 ) ) ;
#2183 = LINE ( 'NONE', #28090, #23824 ) ;
#2184 = AXIS2_PLACEMENT_3D ( 'NONE', #36061, #18327, #37237 ) ;
#2185 = DIRECTION ( 'NONE',  ( -1.000000000000000000, 0.000000000000000000, 0.000000000000000000 ) ) ;
#2186 = ORIENTED_EDGE ( 'NONE', *, *, #13562, .F. ) ;
#2187 = CARTESIAN_POINT ( 'NONE',  ( -0.9873396505805591694, -0.1113553986120547346, 0.2411417322834645827 ) ) ;
#2188 = AXIS2_PLACEMENT_3D ( 'NONE', #20786, #27796, #9553 ) ;
#2189 = CARTESIAN_POINT ( 'NONE',  ( 0.8019270111902716547, 0.1787899950787401604, 1.299212598371434435 ) ) ;
#2190 = CARTESIAN_POINT ( 'NONE',  ( -0.1222724946009781516, -0.09851384947599900466, 0.1962728965156417260 ) ) ;
#2191 = EDGE_LOOP ( 'NONE', ( #41545, #6382, #11816, #21573 ) ) ;
#2192 = CARTESIAN_POINT ( 'NONE',  ( 0.000000000000000000, 0.000000000000000000, -0.1436967020037460685 ) ) ;
#2193 = CARTESIAN_POINT ( 'NONE',  ( -0.6971942568897637749, 2.189545951927499583E-17, 1.031003936954110189 ) ) ;
#2194 = CIRCLE ( 'NONE', #36653, 0.2471922904502826812 ) ;
#2195 = ( BOUNDED_CURVE ( )  B_SPLINE_CURVE ( 2, ( #39405, #24575, #2981, #17614, #39174, #43241, #21439, #25545, #17374 ),
 .UNSPECIFIED., .F., .T. ) 
 B_SPLINE_CURVE_WITH_KNOTS ( ( 3, 2, 2, 2, 3 ),
 ( 0.9000000000000000222, 0.9024999999999999689, 0.9050000000000000266, 0.9074999999999999734, 0.9100000000000000311 ),
 .UNSPECIFIED. ) 
 CURVE ( )  GEOMETRIC_REPRESENTATION_ITEM ( )  RATIONAL_B_SPLINE_CURVE ( ( 1.000000000000000000, 0.9238795325112869605, 1.000000000000000000, 0.9238795325112869605, 1.000000000000000000, 0.9238795325112869605, 1.000000000000000000, 0.9238795325112829637, 1.000000000000000000 ) ) 
 REPRESENTATION_ITEM ( '' )  ) ;
#2196 = CARTESIAN_POINT ( 'NONE',  ( -0.1787899950787401604, -1.628076724134750020, 0.07405724077823318263 ) ) ;
#2197 = VERTEX_POINT ( 'NONE', #4657 ) ;
#2198 = CARTESIAN_POINT ( 'NONE',  ( 0.1574803149606300023, 0.2573565155132549465, -0.3015174453633734930 ) ) ;
#2199 = CARTESIAN_POINT ( 'NONE',  ( 0.1787899950787401604, -0.5738188975840317063, 0.07405724077823318263 ) ) ;
#2200 = CARTESIAN_POINT ( 'NONE',  ( 0.7185039370078739607, 1.928577636452523993E-17, 0.3838582677165354173 ) ) ;
#2201 = EDGE_LOOP ( 'NONE', ( #25060, #15373, #39420, #6603 ) ) ;
#2202 = CARTESIAN_POINT ( 'NONE',  ( 1.002407869896990045, 0.1264236179284866091, 1.405019684985606476 ) ) ;
#2203 = DIRECTION ( 'NONE',  ( 0.000000000000000000, -0.6156614753256598460, -0.7880107536067207930 ) ) ;
#2204 = CARTESIAN_POINT ( 'NONE',  ( -0.1787899950787401604, -0.3572834645131658382, 0.07405724077823318263 ) ) ;
#2205 = CARTESIAN_POINT ( 'NONE',  ( -1.094772975963752103E-17, -0.7583661416785196785, -0.1787899950787401882 ) ) ;
#2206 = FACE_OUTER_BOUND ( 'NONE', #4838, .T. ) ;
#2207 = LINE ( 'NONE', #37047, #4035 ) ;
#2208 = ADVANCED_FACE ( 'NONE', ( #12834 ), #42012, .T. ) ;
#2209 = CARTESIAN_POINT ( 'NONE',  ( 0.07405724077823318263, 0.01070280342430459698, -0.1787899950787401604 ) ) ;
#2210 = CARTESIAN_POINT ( 'NONE',  ( -0.1787899950787401604, 0.07086614178604697112, -0.07405724077823318263 ) ) ;
#2211 = APPLICATION_PROTOCOL_DEFINITION ( 'draft international standard', 'automotive_design', 1998, #37634 ) ;
#2212 = DIRECTION ( 'NONE',  ( 0.000000000000000000, 0.000000000000000000, -1.000000000000000000 ) ) ;
#2213 = CARTESIAN_POINT ( 'NONE',  ( 0.6971942568897626646, 0.07405724077823318263, 0.4330708660879683536 ) ) ;
#2214 = CARTESIAN_POINT ( 'NONE',  ( -0.8019270111902716547, 0.1787899950787401604, 0.7874015747493863238 ) ) ;
#2215 = EDGE_CURVE ( 'NONE', #13663, #4590, #3334, .T. ) ;
#2217 = CARTESIAN_POINT ( 'NONE',  ( 0.8759842519685039353, 0.000000000000000000, 1.995570866087968520 ) ) ;
#2216 = CARTESIAN_POINT ( 'NONE',  ( -0.1574803149606300301, -0.9355314960629919074, -0.06523048226347956391 ) ) ;
#2218 = CARTESIAN_POINT ( 'NONE',  ( 0.1270800023317771588, -1.600437510370446681, 0.1270800023317771588 ) ) ;
#2219 = CARTESIAN_POINT ( 'NONE',  ( 0.7495606340400177148, -0.1264236179284866091, 1.587106299158834721 ) ) ;
#2221 = CARTESIAN_POINT ( 'NONE',  ( 0.2559055118110235560, 0.07338436260360474417, -0.3090062946576829783 ) ) ;
#2220 = CARTESIAN_POINT ( 'NONE',  ( 0.6971942568897637749, 2.189545951927499583E-17, 1.970964566875370139 ) ) ;
#2222 = CARTESIAN_POINT ( 'NONE',  ( 0.6971942568897637749, 2.189545951927499583E-17, 0.3961614172690708924 ) ) ;
#2223 = CARTESIAN_POINT ( 'NONE',  ( 0.8070866141732283561, 0.000000000000000000, 0.7574803149606299524 ) ) ;
#2224 = EDGE_CURVE ( 'NONE', #36581, #7779, #22925, .T. ) ;
#2225 = CARTESIAN_POINT ( 'NONE',  ( 1.033464566929133799, 0.000000000000000000, 0.8661417321759370402 ) ) ;
#2226 = DIRECTION ( 'NONE',  ( -1.000000000000000000, 0.000000000000000000, 0.000000000000000000 ) ) ;
#2228 = CARTESIAN_POINT ( 'NONE',  ( -0.1787899950787401882, 0.03395669296714932950, 0.000000000000000000 ) ) ;
#2227 = CARTESIAN_POINT ( 'NONE',  ( 0.1574803149606300301, -0.8666338581601887858, 0.06523048226347956391 ) ) ;
#2229 = CARTESIAN_POINT ( 'NONE',  ( 0.2395294000716134131, 3.423225304703229610E-16, -0.7086614173228350522 ) ) ;
#2230 = AXIS2_PLACEMENT_3D ( 'NONE', #33648, #41237, #4840 ) ;
#2231 = CARTESIAN_POINT ( 'NONE',  ( 1.054774247047244540, -0.07405724077823318263, 0.4527559054580477249 ) ) ;
#2232 = CARTESIAN_POINT ( 'NONE',  ( 0.1264236179284866091, -0.8518700786863936392, 0.1264236179284866091 ) ) ;
#2233 = CARTESIAN_POINT ( 'NONE',  ( 0.7947666225829561615, -0.1415185883302085834, 0.03937007183037401215 ) ) ;
#2234 = DIRECTION ( 'NONE',  ( 1.822029033848725028E-16, 0.000000000000000000, 1.000000000000000000 ) ) ;
#2235 = ORIENTED_EDGE ( 'NONE', *, *, #20610, .T. ) ;
#2236 = VECTOR ( 'NONE', #15764, 39.37007874015748143 ) ;
#2237 = CARTESIAN_POINT ( 'NONE',  ( 1.054774247047244540, 0.07405724077823318263, 1.053149606245450176 ) ) ;
#2238 = ORIENTED_EDGE ( 'NONE', *, *, #13233, .T. ) ;
#2239 = CARTESIAN_POINT ( 'NONE',  ( -0.1787899950787401604, -1.346456692859623550, -0.07405724077823318263 ) ) ;
#2240 = CARTESIAN_POINT ( 'NONE',  ( -1.033464566929133799, 0.000000000000000000, 0.5118110235145204578 ) ) ;
#2241 = CARTESIAN_POINT ( 'NONE',  ( -1.033464566929134687, -0.06523048226347956391, 1.345964566929133133 ) ) ;
#2242 = LINE ( 'NONE', #5611, #32006 ) ;
#2244 = CARTESIAN_POINT ( 'NONE',  ( -0.7037739381401700856, 0.04180313491334981812, 0.03937007874015843040 ) ) ;
#2243 = CARTESIAN_POINT ( 'NONE',  ( 0.1550611416720020230, 0.2059691479692354332, -0.3138705397960873111 ) ) ;
#2245 = CARTESIAN_POINT ( 'NONE',  ( 1.054774247047244096, 0.000000000000000000, 0.1058070865604096300 ) ) ;
#2246 = CARTESIAN_POINT ( 'NONE',  ( -1.054774247047244540, 0.07405724077823318263, 0.1427165353793073133 ) ) ;
#2247 = CARTESIAN_POINT ( 'NONE',  ( 0.9873396505805591694, -0.1113553986120547346, 1.412401574695621997 ) ) ;
#2248 = ORIENTED_EDGE ( 'NONE', *, *, #47327, .F. ) ;
#2249 = ORIENTED_EDGE ( 'NONE', *, *, #23334, .F. ) ;
#2250 = CARTESIAN_POINT ( 'NONE',  ( 0.1264236179284866091, 0.08809055123486594918, 0.1264236179284866091 ) ) ;
#2251 = CARTESIAN_POINT ( 'NONE',  ( 0.1934636958948905971, -0.1837979153590739156, -0.05069326177276377299 ) ) ;
#2252 = ORIENTED_EDGE ( 'NONE', *, *, #6760, .T. ) ;
#2253 = CARTESIAN_POINT ( 'NONE',  ( -0.6971942568897648851, 0.07405724077823318263, 1.771653543253322249 ) ) ;
#2254 = ORIENTED_EDGE ( 'NONE', *, *, #30710, .T. ) ;
#2255 = DIRECTION ( 'NONE',  ( 1.109243974507663983E-29, 1.000000000000000000, 2.355041373848515369E-15 ) ) ;
#2256 = LINE ( 'NONE', #9473, #8825 ) ;
#2257 = CARTESIAN_POINT ( 'NONE',  ( 0.7646288533564489232, -0.1113553986120547346, 1.599409448711369919 ) ) ;
#2258 = CARTESIAN_POINT ( 'NONE',  ( 0.1787899950787401882, -1.177781448544198639, -2.189545951927503898E-17 ) ) ;
#2259 = ORIENTED_EDGE ( 'NONE', *, *, #27251, .F. ) ;
#2260 = CARTESIAN_POINT ( 'NONE',  ( -0.07405724077823318263, -0.1899606298674962612, 0.1787899950787401604 ) ) ;
#2261 = ORIENTED_EDGE ( 'NONE', *, *, #17908, .T. ) ;
#2262 = VERTEX_POINT ( 'NONE', #20698 ) ;
#2263 = CARTESIAN_POINT ( 'NONE',  ( 0.8759842519685039353, 0.1787899950787401882, 1.094980314906866203 ) ) ;
#2264 = EDGE_CURVE ( 'NONE', #33124, #758, #10410, .T. ) ;
#2265 = AXIS2_PLACEMENT_3D ( 'NONE', #23060, #44845, #19691 ) ;
#2266 = LINE ( 'NONE', #20712, #5444 ) ;
#2267 = CARTESIAN_POINT ( 'NONE',  ( 1.033464566929134687, 0.06523048226347956391, 1.823326771653542178 ) ) ;
#2268 = CIRCLE ( 'NONE', #24483, 0.2952755905511806334 ) ;
#2269 = EDGE_CURVE ( 'NONE', #31572, #34936, #15953, .T. ) ;
#2270 = CARTESIAN_POINT ( 'NONE',  ( -1.094772975963752103E-17, -0.6845472440407243120, -0.1787899950787401882 ) ) ;
#2271 = CARTESIAN_POINT ( 'NONE',  ( -0.6971942568897626646, 0.07405724077823318263, 0.2805118109698587214 ) ) ;
#2272 = CARTESIAN_POINT ( 'NONE',  ( -0.9873396505805591694, -0.1113553986120547346, 0.9891732283464568232 ) ) ;
#2273 = CYLINDRICAL_SURFACE ( 'NONE', #20992, 0.1574803149606299191 ) ;
#2274 = CARTESIAN_POINT ( 'NONE',  ( 0.07444174185955065859, -1.169827274149974894, 0.1797182628040039087 ) ) ;
#2275 = CARTESIAN_POINT ( 'NONE',  ( -0.1702179831425296441, 0.1972188338741525382, -0.03726912461314065700 ) ) ;
#2276 = CARTESIAN_POINT ( 'NONE',  ( 1.054774247047244540, 0.07405724077823318263, 1.092519684985605810 ) ) ;
#2277 = CARTESIAN_POINT ( 'NONE',  ( 0.6971942568897648851, -0.07405724077823297447, 1.500984251914741829 ) ) ;
#2278 = CARTESIAN_POINT ( 'NONE',  ( -0.7185039370078739607, 0.000000000000000000, -2.869337061179095023E-17 ) ) ;
#2279 = CARTESIAN_POINT ( 'NONE',  ( 0.9873396505805591694, -0.1113553986120547346, 1.658464566929134021 ) ) ;
#2281 = CARTESIAN_POINT ( 'NONE',  ( -0.9412147342319837628, -0.1574803149606297803, 1.104822834645669882 ) ) ;
#2280 = DIRECTION ( 'NONE',  ( 1.000000000000000000, 0.000000000000000000, 0.000000000000000000 ) ) ;
#2282 = LINE ( 'NONE', #13545, #25142 ) ;
#2283 = CARTESIAN_POINT ( 'NONE',  ( -0.7646288533564489232, 0.1113553986120547346, 1.560039370078740273 ) ) ;
#2284 = CARTESIAN_POINT ( 'NONE',  ( 0.7495606340400177148, 0.1264236179284866091, 1.021161417269070837 ) ) ;
#2285 = AXIS2_PLACEMENT_3D ( 'NONE', #44710, #29474, #29932 ) ;
#2286 = CARTESIAN_POINT ( 'NONE',  ( 0.9412147342319837628, -0.1574803149606297803, 0.2682086613097960370 ) ) ;
#2287 = ORIENTED_EDGE ( 'NONE', *, *, #20440, .F. ) ;
#2288 = DIRECTION ( 'NONE',  ( -0.5735764363510518216, 0.8191520442889876907, 1.003171929053519693E-16 ) ) ;
#2289 = CARTESIAN_POINT ( 'NONE',  ( -0.7185039370078746268, 0.06523048226347956391, 0.2534448817822366751 ) ) ;
#2290 = CARTESIAN_POINT ( 'NONE',  ( 0.7495606340400177148, -0.1264236179284866091, 1.267224409395055096 ) ) ;
#2292 = CARTESIAN_POINT ( 'NONE',  ( -1.033464566929134687, 0.06523048226347956391, 0.2780511809948353341 ) ) ;
#2291 = FACE_OUTER_BOUND ( 'NONE', #37130, .T. ) ;
#2294 = VECTOR ( 'NONE', #5738, 39.37007874015748143 ) ;
#2293 = CARTESIAN_POINT ( 'NONE',  ( -0.1264236179284866091, 0.1520669291876218521, -0.1264236179284866091 ) ) ;
#2295 = CARTESIAN_POINT ( 'NONE',  ( 0.000000000000000000, -0.09842519685039370636, 0.000000000000000000 ) ) ;
#2296 = ORIENTED_EDGE ( 'NONE', *, *, #17744, .F. ) ;
#2297 = CARTESIAN_POINT ( 'NONE',  ( 0.1908328281150623862, 0.07780450164205171548, 0.1752556861836929991 ) ) ;
#2298 = CARTESIAN_POINT ( 'NONE',  ( -0.02442443439252901111, 0.05525422739384169835, 0.2713316170948106287 ) ) ;
#2299 = ORIENTED_EDGE ( 'NONE', *, *, #37947, .F. ) ;
#2300 = ORIENTED_EDGE ( 'NONE', *, *, #18650, .F. ) ;
#2301 = CARTESIAN_POINT ( 'NONE',  ( -0.8759842519685039353, 0.1787899950787401882, 1.409940944828126153 ) ) ;
#2303 = CARTESIAN_POINT ( 'NONE',  ( -0.1264236179284866091, -1.663877952702141672, -0.1264236179284866091 ) ) ;
#2302 = CARTESIAN_POINT ( 'NONE',  ( -0.06523048226347956391, -0.4040354329633388808, 0.1574803149606297803 ) ) ;
#2304 = CARTESIAN_POINT ( 'NONE',  ( -0.6971942568897648851, -0.07405724077823297447, 0.9940944881352130613 ) ) ;
#2305 = CARTESIAN_POINT ( 'NONE',  ( -0.8019270111902717657, 0.1787899950787401604, 1.924212598371433325 ) ) ;
#2306 = ORIENTED_EDGE ( 'NONE', *, *, #31742, .T. ) ;
#2307 = CARTESIAN_POINT ( 'NONE',  ( -0.9500414927467378812, -0.1787899950787401604, 0.6889763778989935750 ) ) ;
#2308 = CARTESIAN_POINT ( 'NONE',  ( 0.1526800167754713278, 0.1252930045944034287, -0.05620926796873287890 ) ) ;
#2309 = CARTESIAN_POINT ( 'NONE',  ( -0.8759842519685039353, 0.000000000000000000, 0.000000000000000000 ) ) ;
#2310 = CARTESIAN_POINT ( 'NONE',  ( 0.1787899950787401604, -0.6635097950008927992, -0.07405724077823318263 ) ) ;
#2311 = ORIENTED_EDGE ( 'NONE', *, *, #16420, .T. ) ;
#2312 = CARTESIAN_POINT ( 'NONE',  ( 0.1998254672493015582, -0.08956033089349921261, -0.03070792776777759789 ) ) ;
#2313 = ORIENTED_EDGE ( 'NONE', *, *, #6559, .F. ) ;
#2314 = DIRECTION ( 'NONE',  ( 1.000000000000000000, 0.000000000000000000, -0.000000000000000000 ) ) ;
#2315 = EDGE_CURVE ( 'NONE', #3713, #30859, #28291, .T. ) ;
#2316 = CARTESIAN_POINT ( 'NONE',  ( -1.002407869896990045, -0.1264236179284866091, 0.6865157479777322935 ) ) ;
#2317 = CARTESIAN_POINT ( 'NONE',  ( 0.1113553986120547346, 0.07578740157480315376, -0.1113553986120547346 ) ) ;
#2318 = ADVANCED_FACE ( 'NONE', ( #29029 ), #46707, .T. ) ;
#2319 = AXIS2_PLACEMENT_3D ( 'NONE', #15882, #43971, #29427 ) ;
#2320 = EDGE_CURVE ( 'NONE', #11282, #39413, #6695, .T. ) ;
#2321 = CARTESIAN_POINT ( 'NONE',  ( -0.6971942568897648851, -0.07405724077823297447, 1.702755905458047003 ) ) ;
#2322 = VECTOR ( 'NONE', #39942, 39.37007874015748143 ) ;
#2323 = EDGE_CURVE ( 'NONE', #7079, #3732, #45911, .T. ) ;
#2324 = AXIS2_PLACEMENT_3D ( 'NONE', #9453, #24067, #35088 ) ;
#2325 = CARTESIAN_POINT ( 'NONE',  ( -0.2066929133858267931, -0.5175744617845221551, -0.9076376772307637175 ) ) ;
#2326 = CARTESIAN_POINT ( 'NONE',  ( -0.7646288533564489232, -0.1113553986120547346, 0.1820866140657015630 ) ) ;
#2327 = CARTESIAN_POINT ( 'NONE',  ( 0.7185039370078746268, 0.06523048226347956391, 0.6569881889763780070 ) ) ;
#2328 = VERTEX_POINT ( 'NONE', #25156 ) ;
#2329 = CARTESIAN_POINT ( 'NONE',  ( -0.1270800023317771588, -0.7146107387169036151, -0.1270800023317771588 ) ) ;
#2330 = DIRECTION ( 'NONE',  ( -6.679788269418529283E-17, 1.000000000000000000, 0.000000000000000000 ) ) ;
#2331 = CARTESIAN_POINT ( 'NONE',  ( -1.033464566929134687, -0.06523048226347956391, 1.218011810916095117 ) ) ;
#2332 = CARTESIAN_POINT ( 'NONE',  ( 0.8019270111902717657, -0.1787899950787401604, 0.6446850393163160442 ) ) ;
#2334 = CARTESIAN_POINT ( 'NONE',  ( -0.1650166048207457326, -0.09842519685039370636, -0.06577345936140498173 ) ) ;
#2333 = CARTESIAN_POINT ( 'NONE',  ( 0.1574803149606299191, -0.4015748031496063630, -1.928577636452523993E-17 ) ) ;
#2335 = CARTESIAN_POINT ( 'NONE',  ( 1.033464566929133799, 0.000000000000000000, 0.9940944881889764995 ) ) ;
#2336 = ORIENTED_EDGE ( 'NONE', *, *, #44618, .F. ) ;
#2337 = DIRECTION ( 'NONE',  ( 1.000000000000000000, 0.000000000000000000, -0.000000000000000000 ) ) ;
#2338 = CARTESIAN_POINT ( 'NONE',  ( 0.7646288533564489232, -0.1113553986120547346, 1.097440944881889813 ) ) ;
#2339 = CARTESIAN_POINT ( 'NONE',  ( -0.1586641775163213364, 1.975221432870719385, -0.9622519263226601005 ) ) ;
#2341 = DIRECTION ( 'NONE',  ( 0.000000000000000000, 0.7880107536067206819, -0.6156614753256597350 ) ) ;
#2340 = DIRECTION ( 'NONE',  ( 1.000000000000000000, -0.000000000000000000, -0.000000000000000000 ) ) ;
#2342 = CARTESIAN_POINT ( 'NONE',  ( 0.1555687797274980522, 0.05303742630350897352, 0.1377952755905511861 ) ) ;
#2343 = CARTESIAN_POINT ( 'NONE',  ( -1.094772975963752103E-17, -0.5615157479777322935, -0.1787899950787401882 ) ) ;
#2344 = ORIENTED_EDGE ( 'NONE', *, *, #21534, .F. ) ;
#2345 = CARTESIAN_POINT ( 'NONE',  ( -0.3161444924769509779, 0.1169123912647635627, -2.121729632260043186 ) ) ;
#2346 = CARTESIAN_POINT ( 'NONE',  ( 0.6971942568897626646, 0.07405724077823318263, 0.8661417322297003674 ) ) ;
#2347 = DIRECTION ( 'NONE',  ( -1.000000000000000000, 0.000000000000000000, 0.000000000000000000 ) ) ;
#2348 = DIRECTION ( 'NONE',  ( 1.822029033848725028E-16, 0.000000000000000000, 1.000000000000000000 ) ) ;
#2349 = CARTESIAN_POINT ( 'NONE',  ( -0.1787899950787401604, -1.809055118056471123, 0.07405724077823318263 ) ) ;
#2350 = CARTESIAN_POINT ( 'NONE',  ( 0.07405724077823318263, -1.134842519631275914, 0.1787899950787401604 ) ) ;
#2351 = CARTESIAN_POINT ( 'NONE',  ( -0.1574803149606297803, -1.324311023622046779, 0.06523048226347956391 ) ) ;
#2352 = CARTESIAN_POINT ( 'NONE',  ( -1.033464566929134687, 0.06523048226347956391, 1.852854330601134469 ) ) ;
#2353 = ORIENTED_EDGE ( 'NONE', *, *, #25974, .F. ) ;
#2354 = CARTESIAN_POINT ( 'NONE',  ( -0.7495606340400177148, 0.1264236179284866091, 1.931594488135212728 ) ) ;
#2355 = DIRECTION ( 'NONE',  ( -0.000000000000000000, -0.000000000000000000, -1.000000000000000000 ) ) ;
#2356 = VERTEX_POINT ( 'NONE', #39746 ) ;
#2357 = DIRECTION ( 'NONE',  ( -0.000000000000000000, 1.000000000000000000, -0.000000000000000000 ) ) ;
#2358 = AXIS2_PLACEMENT_3D ( 'NONE', #3227, #47084, #17858 ) ;
#2359 = CARTESIAN_POINT ( 'NONE',  ( -0.6971942568897648851, 0.07405724077823318263, 1.535433070812378675 ) ) ;
#2360 = CARTESIAN_POINT ( 'NONE',  ( 0.1476377952755906220, 0.5419727308409664213, -0.7545416139885205986 ) ) ;
#2361 = CARTESIAN_POINT ( 'NONE',  ( -0.8019270111902717657, 0.1787899950787401604, 1.018700787347811110 ) ) ;
#2362 = LINE ( 'NONE', #45498, #19120 ) ;
#2363 = CARTESIAN_POINT ( 'NONE',  ( -0.7495606340400177148, 0.1264236179284866091, 1.852854330654897685 ) ) ;
#2364 = CARTESIAN_POINT ( 'NONE',  ( -0.1898978525284567009, 0.07836113345104847583, 0.1757954945903054400 ) ) ;
#2365 = CARTESIAN_POINT ( 'NONE',  ( -1.033464566929134687, -0.06523048226347956391, 1.700295275590550936 ) ) ;
#2366 = LINE ( 'NONE', #17236, #2940 ) ;
#2367 = CARTESIAN_POINT ( 'NONE',  ( 0.1787899950787401882, -0.1935294800402626025, -2.189545951927503898E-17 ) ) ;
#2368 = VECTOR ( 'NONE', #43957, 39.37007874015748854 ) ;
#2369 = B_SPLINE_CURVE_WITH_KNOTS ( 'NONE', 3,
 ( #35071, #9669, #27672, #2450, #46306, #9435, #6043, #38657, #17549, #28125, #42232, #17315, #32187, #13036, #46773, #42684, #13720, #17789, #24511 ),
 .UNSPECIFIED., .F., .F.,
 ( 4, 1, 1, 1, 2, 2, 1, 1, 1, 1, 2, 2, 4 ),
 ( 0.000000000000000000, 0.1250000000000002498, 0.1875000000000002498, 0.2187500000000004163, 0.2343750000000003608, 0.2500000000000002776, 0.3750000000000021094, 0.4375000000000029976, 0.4687500000000034417, 0.4843750000000036082, 0.4921875000000036082, 0.5000000000000035527, 1.000000000000000000 ),
 .UNSPECIFIED. ) ;
#2370 = CARTESIAN_POINT ( 'NONE',  ( -0.08392896972913758968, -0.09842519685039370636, 0.2125180856786228201 ) ) ;
#2371 = DIRECTION ( 'NONE',  ( 0.000000000000000000, -0.7880107536067207930, 0.6156614753256597350 ) ) ;
#2372 = CARTESIAN_POINT ( 'NONE',  ( -0.8759842519685039353, 0.1574803149606299191, 0.04921259831766984505 ) ) ;
#2373 = EDGE_CURVE ( 'NONE', #42760, #4911, #43923, .T. ) ;
#2374 = ORIENTED_EDGE ( 'NONE', *, *, #36808, .F. ) ;
#2375 = ORIENTED_EDGE ( 'NONE', *, *, #9641, .T. ) ;
#2376 = EDGE_CURVE ( 'NONE', #19774, #31278, #9778, .T. ) ;
#2377 = CARTESIAN_POINT ( 'NONE',  ( -0.1787899950787401604, -0.9921259841982054128, -0.07405724077823318263 ) ) ;
#2378 = CARTESIAN_POINT ( 'NONE',  ( -0.1264236179284866091, -1.147145669237574772, -0.1264236179284866091 ) ) ;
#2379 = CIRCLE ( 'NONE', #29242, 0.1574803149606299191 ) ;
#2380 = CARTESIAN_POINT ( 'NONE',  ( -1.033464566929134687, 0.06523048226347956391, 1.537893700679874076 ) ) ;
#2381 = ( NAMED_UNIT ( * ) SI_UNIT ( $, .STERADIAN. ) SOLID_ANGLE_UNIT ( ) ) ;
#2382 = CARTESIAN_POINT ( 'NONE',  ( -0.1270800023317771588, -0.4783902662759590974, -0.1270800023317771588 ) ) ;
#2383 = DIRECTION ( 'NONE',  ( 1.000000000000000000, 0.000000000000000000, 0.000000000000000000 ) ) ;
#2384 = CARTESIAN_POINT ( 'NONE',  ( -0.9412147342319837628, -0.1574803149606297803, 0.7406496061916858498 ) ) ;
#2385 = CARTESIAN_POINT ( 'NONE',  ( -0.7185039370078746268, 0.06523048226347956391, 0.6963582677165359724 ) ) ;
#2386 = CARTESIAN_POINT ( 'NONE',  ( -0.06523048226347956391, 0.04379921259842517456, -0.1574803149606300301 ) ) ;
#2387 = VECTOR ( 'NONE', #36112, 39.37007874015748143 ) ;
#2388 = CONICAL_SURFACE ( 'NONE', #29250, 0.08090551181102362266, 0.9599310885968742602 ) ;
#2389 = CARTESIAN_POINT ( 'NONE',  ( 0.9500414927467378812, -0.1787899950787401604, 0.9202755904974182499 ) ) ;
#2390 = AXIS2_PLACEMENT_3D ( 'NONE', #23864, #42522, #1808 ) ;
#2392 = DIRECTION ( 'NONE',  ( 1.000000000000000000, 0.000000000000000000, 0.000000000000000000 ) ) ;
#2391 = CARTESIAN_POINT ( 'NONE',  ( 0.1339681929923581538, 0.2181476599754205714, -0.02739586109244947915 ) ) ;
#2393 = CARTESIAN_POINT ( 'NONE',  ( 0.7495606340400177148, -0.1264236179284866091, 1.941437007820252081 ) ) ;
#2394 = VERTEX_POINT ( 'NONE', #24115 ) ;
#2395 = ORIENTED_EDGE ( 'NONE', *, *, #29884, .F. ) ;
#2396 = CARTESIAN_POINT ( 'NONE',  ( -0.8759842519685039353, -0.1574803149606299191, 0.7775590550105826448 ) ) ;
#2397 = DIRECTION ( 'NONE',  ( 0.000000000000000000, -1.000000000000000000, 0.000000000000000000 ) ) ;
#2399 = CARTESIAN_POINT ( 'NONE',  ( 0.07405724077823318263, -0.5295275590013543976, -0.1787899950787401604 ) ) ;
#2398 = CARTESIAN_POINT ( 'NONE',  ( -0.1113553986120547346, -0.9970472439869606518, 0.1113553986120547346 ) ) ;
#2400 = CARTESIAN_POINT ( 'NONE',  ( 0.1787899950787401604, -1.321850393647023392, 0.07405724077823318263 ) ) ;
#2401 = CARTESIAN_POINT ( 'NONE',  ( 0.8019270111902717657, -0.1787899950787401604, 0.3297244093950552069 ) ) ;
#2402 = CARTESIAN_POINT ( 'NONE',  ( -0.8019270111902717657, 0.1787899950787401604, 1.963582677111591401 ) ) ;
#2403 = ORIENTED_EDGE ( 'NONE', *, *, #44041, .F. ) ;
#2404 = CARTESIAN_POINT ( 'NONE',  ( -0.6971942568897648851, 0.07405724077823318263, 1.500984251914741607 ) ) ;
#2405 = CARTESIAN_POINT ( 'NONE',  ( 0.9500414927467378812, -0.1787899950787401604, 1.437007873961985371 ) ) ;
#2406 = DIRECTION ( 'NONE',  ( 1.000000000000000000, 0.000000000000000000, 0.000000000000000000 ) ) ;
#2407 = CARTESIAN_POINT ( 'NONE',  ( 0.1574803149606299191, -1.257874015640503718, -1.928577636452523993E-17 ) ) ;
#2408 = CARTESIAN_POINT ( 'NONE',  ( -0.6971942568897626646, -0.07405724077823297447, 0.6791338582139527791 ) ) ;
#2409 = LINE ( 'NONE', #17041, #30487 ) ;
#2410 = CARTESIAN_POINT ( 'NONE',  ( -0.9412147342319837628, 0.1574803149606300301, 1.621555118002709683 ) ) ;
#2411 = CARTESIAN_POINT ( 'NONE',  ( 0.9500414927467377701, 0.1787899950787401604, 0.5856299212060785964 ) ) ;
#2412 = CARTESIAN_POINT ( 'NONE',  ( -0.9500414927467377701, -0.1787899950787401604, 0.5659448818360001132 ) ) ;
#2413 = CARTESIAN_POINT ( 'NONE',  ( 0.2374471364661455419, -0.04193537623317827867, 0.1483429027091067720 ) ) ;
#2414 = AXIS2_PLACEMENT_3D ( 'NONE', #20561, #20331, #35436 ) ;
#2415 = CARTESIAN_POINT ( 'NONE',  ( -0.1574803149606299191, 0.000000000000000000, -0.07924015748031493223 ) ) ;
#2416 = ORIENTED_EDGE ( 'NONE', *, *, #22181, .F. ) ;
#2417 = CARTESIAN_POINT ( 'NONE',  ( -1.054774247047244096, 0.000000000000000000, 1.483759842465921075 ) ) ;
#2418 = DIRECTION ( 'NONE',  ( -1.000000000000000000, -0.000000000000000000, -0.000000000000000000 ) ) ;
#2419 = CARTESIAN_POINT ( 'NONE',  ( -0.9873396505805591694, -0.1113553986120547346, 0.5167322834645668994 ) ) ;
#2420 = CARTESIAN_POINT ( 'NONE',  ( 1.054774247047244096, 0.000000000000000000, 1.286909448765133801 ) ) ;
#2421 = CARTESIAN_POINT ( 'NONE',  ( 0.1947686307480071266, -0.09851384395597342913, -0.06118066026927814621 ) ) ;
#2422 = ( REPRESENTATION_RELATIONSHIP ('NONE','NONE', #9609, #20643 ) REPRESENTATION_RELATIONSHIP_WITH_TRANSFORMATION ( #3323 )SHAPE_REPRESENTATION_RELATIONSHIP( ) ) ;
#2423 = VECTOR ( 'NONE', #41247, 39.37007874015748143 ) ;
#2424 = ORIENTED_EDGE ( 'NONE', *, *, #32883, .T. ) ;
#2425 = CIRCLE ( 'NONE', #46038, 0.1377952755905511861 ) ;
#2426 = DIRECTION ( 'NONE',  ( 5.724375810226264544E-16, 0.6156614753256587358, 0.7880107536067215701 ) ) ;
#2427 = CARTESIAN_POINT ( 'NONE',  ( -0.7495606340400177148, -0.1264236179284866091, 1.035925196796629866 ) ) ;
#2428 = EDGE_CURVE ( 'NONE', #9934, #46256, #25269, .T. ) ;
#2429 = CARTESIAN_POINT ( 'NONE',  ( -0.1264236179284866091, -1.556718456418214602, -0.1264236179284866091 ) ) ;
#2430 = VERTEX_POINT ( 'NONE', #44529 ) ;
#2431 = CARTESIAN_POINT ( 'NONE',  ( 0.1787899950787401604, -0.5344488188438744070, 0.07405724077823318263 ) ) ;
#2432 = CARTESIAN_POINT ( 'NONE',  ( 0.8759842519685039353, -0.1787899950787401882, 1.390255905458047447 ) ) ;
#2433 = EDGE_CURVE ( 'NONE', #33511, #19692, #3856, .T. ) ;
#2434 = CARTESIAN_POINT ( 'NONE',  ( 3.284318927891251994E-17, -0.3105314960092286913, 0.1787899950787401882 ) ) ;
#2435 = CARTESIAN_POINT ( 'NONE',  ( 0.1787899950787401604, -0.7706692912848194243, 0.07405724077823318263 ) ) ;
#2436 = DIRECTION ( 'NONE',  ( 0.000000000000000000, 0.000000000000000000, -1.000000000000000000 ) ) ;
#2437 = CARTESIAN_POINT ( 'NONE',  ( -1.033464566929134687, -0.06523048226347956391, 0.9817913384751512096 ) ) ;
#2438 = CARTESIAN_POINT ( 'NONE',  ( 0.1264236179284866091, -0.001600346181994637780, 0.1264236179284866091 ) ) ;
#2439 = CONTEXT_DEPENDENT_SHAPE_REPRESENTATION ( #15316, #39411 ) ;
#2440 = CARTESIAN_POINT ( 'NONE',  ( 0.06828144477518423294, -0.09842519685039377575, 0.1509156562122493384 ) ) ;
#2441 = CARTESIAN_POINT ( 'NONE',  ( 0.7495606340400177148, 0.1264236179284866091, 0.4306102361667086820 ) ) ;
#2442 = ( BOUNDED_SURFACE ( )  B_SPLINE_SURFACE ( 1, 2, ( 
 ( #7254, #10389, #28367, #21634, #21876, #31961, #25488, #6770, #7007, #7475, #17799, #29105, #2923, #14449, #43660, #28620, #40054, #36268, #36496, #47024, #18035, #14684, #22094, #24994, #32681, #17558, #3652, #39589, #18273, #3169, #39351, #32196, #10627, #42936, #32916, #25721, #13970, #40290, #14219, #36721, #43180, #32446, #21146, #3883, #28860, #46546, #24755, #43419, #21387, #10146, #6532, #36012, #25230, #47270, #39818, #18730, #23043, #33621, #22326, #34090, #4328, #26186, #736, #37410, #44354, #1220, #15398, #23289, #37184, #8415, #33390, #506, #980, #15163, #29807, #30042, #36954, #37903, #18502, #37661, #18961, #15872, #4817, #4111, #33159, #22802, #11562, #44587, #44827, #280, #40754, #14925, #7950, #11329, #19202, #15638, #8651, #11804, #26423, #30275, #25941, #40991, #22569, #12040, #19440, #30499, #26662, #41210, #8177, #45059, #4568, #33861, #12273, #7711, #26894, #41451, #29590, #44131, #40521, #19678, #46249, #16344, #35022, #2401, #13448, #9381, #5998, #16793, #20618, #12755, #41929, #5060, #30734, #23752, #34794, #16568, #9135, #28077, #1934, #42639, #13220, #9849, #31200, #45771, #27620, #10551, #21798, #32607, #17718, #29274, #15089, #25865, #199, #25150, #22249, #29022, #32368, #25639, #4036, #3093, #44056, #39982, #11021, #11481, #36423, #33072, #39740, #14845, #33313, #47195, #437, #22021, #29736, #44278, #3581, #43822, #21550, #26103, #3807, #40675, #7873, #14138, #6927, #18199, #47434, #36188, #17949, #40911, #33789, #19607, #4987, #26351, #8821, #23456, #45222, #22970, #11732, #4255, #905, #22488, #19842, #30206, #1377, #27066, #29968, #8344, #37107, #12195, #37578, #16035, #12444, #4739, #15314, #19365, #34020, #22731, #1145, #5214, #1620, #37337, #15803, #37830, #8578, #38059, #4487, #34471, #16270, #30662, #15567, #30902, #27309, #30431, #45459, #44984, #41378, #26821, #12684, #33545, #19125, #41859, #18890, #661, #44515, #23216, #38532, #23925, #5462, #20314, #31828, #20077, #10009, #2332, #6157, #2098, #28476, #34723, #20779, #38292, #2559, #31364, #42793, #46414, #28230, #9063, #39222, #21009, #17423, #32060, #46648, #24858, #10739, #33019, #15038, #11204, #32310, #25817, #28967, #3277, #25347, #14550, #21490, #40393, #39930, #386, #14322, #142, #10494, #25092, #25589, #39683, #43294, #7117, #14078, #43045, #10253, #14794, #43524, #7582, #29456, #28725, #39458, #47378, #36122, #21741, #21972, #6634, #46889, #21254, #6869, #35878, #43767, #40161, #33262, #36372, #3527, #7360, #3031, #18140, #17901, #36597, #44002, #22195, #3754, #18377, #32784, #36832, #29222, #10970, #32549, #47137, #3982, #18601, #17662, #19550, #41090, #44229, #41554, #33492, #1090, #27010, #8763, #19313, #1324, #33965, #34197, #22679, #26299, #1560, #29687, #846, #44691, #8287, #26051, #15982, #11432, #30603, #30382, #19782, #37280, #4435, #19067, #37056, #15506, #11907, #15748, #45167, #34417, #8052, #44928, #608, #12389, #33736, #23399, #30150, #4207, #15265, #22913, #40624, #4927, #23155, #44460, #38003, #26531, #5164, #11675, #37527, #18837, #7818, #4683, #22434, #29912, #12142, #40857, #26766, #41323, #8525, #37770, #16902, #16446, #31074, #20720, #31304, #20018, #2508, #17132, #38933, #16675, #5395, #45413, #9244, #16215, #13540, #23863, #13320, #35363, #23626, #20255, #30846, #5885, #45883, #46122, #6095, #34902, #9003, #13095, #2042, #34658, #27728, #46356, #42735, #1807, #42290, #31542, #2276, #31775, #45639, #28174, #9950, #27951, #5644, #24559, #20951, #9488, #39162, #24108, #35130, #20492, #6334, #27249, #12857, #35596, #42518, #41803, #12626, #38715, #27491, #38237, #9721, #24335, #10913, #46590, #3698, #21428, #39627, #43227, #7520, #28411, #32488, #31998, #43465, #24798, #36539, #17842, #13770, #22141, #25536, #32959, #10432, #36055, #47317, #42982, #47070, #40104, #10190, #18321, #39391, #46826, #35820, #10670, #29401, #7298, #14492, #2967, #21918, #25032, #32245, #39866, #81, #14014, #43707, #3213, #25278, #25762, #14262, #29152, #28904, #32725, #14729, #7055, #43946, #21681, #11143, #40332, #36311, #3466, #18077, #1032, #44632, #19253, #1269, #26710, #26945, #37233, #33435, #22621, #41501, #7758, #550, #15689, #30326, #40567, #8705, #41265, #7996, #15921, #8465, #22376, #3927, #41036, #15207, #15446, #44873, #18547, #36999, #33204, #4155, #29632, #37472, #12086, #36767, #4378, #19007, #23094, #44171, #8230, #29858, #37713, #4865, #19493, #45111, #12330, #22855, #327, #33671, #4619, #44398, #25985, #784, #18781, #14977, #11373, #11614, #26235, #40801, #27193, #42231, #20669, #35311, #13035, #42464, #27671, #27901, #16394, #19960, #42683, #23342, #41979, #38418, #34844, #19726, #9668, #5102, #24284, #24053, #13493, #31015, #45581, #12803, #30788, #9185, #5588, #9434, #38879, #28124, #1751, #38656, #41746, #6042, #27437, #2449, #23802, #45355, #8951, #1989, #34363, #46066, #16839, #38177, #17076, #20195, #31716, #5339, #16618, #12567, #46305, #31247, #37954, #16156, #45824, #34600, #5829, #1501, #20436, #35070, #2219, #23571, #31479, #13270, #24983, #13719, #25474, #43171, #17548, #39578, #28847, #35771, #40044, #6756, #14674, #28609, #47259, #24744, #39339, #39808, #6519, #10135, #21378, #28356, #29346, #7242, #10376, #32186, #36003, #43408, #2913, #21863, #3161, #9898, #17788, #14439, #21136, #46772, #6996, #13958, #32435, #47012, #42924, #24510, #39107, #29093, #14207, #36488, #43651, #10618, #6281, #25217, #21623, #36256, #3408, #20904, #18024, #35544, #32670, #2687, #10859, #3643, #24, #18261, #32907, #17314, #31952, #4320, #40514, #40982, #15631, #12031, #4560, #22797, #18953, #19193, #29799, #30035, #22317, #33145, #26176, #270, #44819, #33853, #7942, #11090, #8409, #14913, #15389, #41203, #23037, #33613, #30268, #727, #972, #36946, #7703, #15865, #43890, #15155, #11554, #22558, #40280, #26656, #25709, #37652, #44578, #34084, #4100, #18722, #33380, #3874, #40744, #37176, #11798, #4807, #1214, #497, #26415, #29576, #19433, #8169, #7467, #37403, #18492, #44121, #22087, #36711, #11320, #25933, #45296, #2165, #12749, #46010, #12513, #16337, #19672, #9613, #27379, #13213, #23282, #41922, #27137, #12976, #2393, #41687, #8891, #31193, #30727, #23523, #35014, #45525, #34314, #5287, #19905, #37896, #1689, #9130, #34788, #27848, #20612, #38128, #16560, #1443, #16789, #34535, #31427 ),
 ( #35260, #16103, #30959, #27612, #42167, #23745, #42411, #24232, #5770, #38356, #5528, #12264, #20142, #30491, #38829, #1929, #9373, #5991, #5053, #45764, #45051, #23996, #38594, #20376, #26887, #41443, #8644, #32123, #2854, #20847, #35718, #47205, #43593, #35489, #46712, #32378, #3103, #3352, #2628, #17961, #29033, #46959, #10075, #10804, #21808, #24689, #14385, #28547, #35944, #6700, #21561, #28072, #17260, #6939, #14148, #42633, #17027, #39287, #46481, #39053, #13441, #24453, #25162, #9844, #32617, #21079, #6462, #42861, #36433, #6223, #13900, #31664, #10319, #31899, #25417, #43113, #46240, #13661, #39750, #39991, #17492, #24930, #28791, #28299, #39523, #36197, #21315, #7183, #17729, #43356, #10562, #1818, #38486, #2286, #24348, #12638, #20265, #5176, #38726, #27262, #5894, #5409, #41571, #19794, #12870, #30617, #9500, #27740, #1574, #20506, #16455, #16916, #16226, #20030, #23411, #13333, #31088, #31555, #27022, #45652, #30858, #16690, #6111, #45421, #41814, #34913, #34428, #9015, #35143, #27503, #38015, #46133, #34671, #23637, #42054, #5656, #38248, #27962, #9255, #38945, #23875, #24121, #2056, #31317, #45892, #13109, #42306, #42529, #9731, #1338, #15994, #45181, #12402, #8776, #39882, #39176, #35376, #25044, #46605, #46839, #47082, #2520, #24577, #17146, #6349, #13553, #21441, #17856, #10925, #6589, #35837, #32498, #28189, #28676, #17376, #14276, #7066, #36326, #28915, #43478, #43244, #10686, #21203, #6822, #13784, #9966, #2983, #20963, #21694, #25293, #32261, #31790, #32738, #35609, #39640, #18092, #47333, #10446, #3480, #36069, #14504, #28430, #32013, #40117, #20735, #39407, #17615, #14029, #46372, #29166, #42748, #43720, #3224, #25547, #42995, #10205, #24809, #2750, #26000, #22388, #19023, #97, #15221, #3939, #4393, #26485, #22872, #15463, #33687, #29869, #30113, #40581, #40811, #33219, #43959, #37015, #11158, #8246, #44644, #18793, #21931, #19267, #25775, #26248, #4637, #33922, #44411, #41048, #11629, #11861, #343, #18562, #26725, #7312, #7772, #4169, #33449, #3712, #37484, #36551, #1047, #8007, #44888, #14992, #29644, #44185, #14744, #565, #22636, #37241, #15704, #12101, #11387, #798, #40347, #30339, #18335, #32973, #29415, #7538, #22150, #36783, #37728, #16631, #34859, #8720, #13049, #23583, #9451, #23356, #27210, #30564, #20450, #38192, #24065, #34154, #5353, #37966, #23815, #13907, #5116, #19740, #41993, #41515, #34377, #45840, #8963, #45126, #38674, #41760, #1516, #19976, #12818, #16169, #5842, #34615, #46721, #12584, #31262, #30803, #45369, #38434, #1764, #16405, #31031, #12342, #41280, #8480, #27685, #45598, #35726, #42247, #26962, #23114, #27450, #9197, #5601, #20208, #4882, #2005, #19506, #2862, #1282, #17498, #32129, #15938, #14393, #43601, #47453, #6948, #11273, #25425, #33333, #47212, #18447, #43363, #10571, #11044, #25172, #28799, #39999, #46966, #456, #28553, #33096, #29042, #25887, #217, #14155, #43122, #32859, #21569, #7192, #7424, #10326, #32385, #24938, #39756, #21323, #29295, #25660, #18673, #10813, #21817, #40236, #35954, #36445, #36207, #22043, #14867, #44077, #36668, #3826, #3597, #29526, #18218, #14626, #3359, #17735, #43843, #17971, #40468, #7651, #22268, #39531, #36904, #32625, #4058, #6710, #3112, #4765, #34270, #19392, #19629, #8128, #11752, #34494, #15109, #33813, #30225, #26611, #11505, #1401, #44302, #16060, #15827, #5243, #22751, #37358, #4510, #22511, #929, #44772, #34043, #30687, #19869, #40932, #1168, #33567, #45251, #19146, #12471, #15587, #37127, #684, #41164, #26127, #37855, #8602, #29992, #27092, #11988, #41643, #44536, #8367, #4276, #8847, #22993, #23484, #7893, #37605, #26373, #45008, #29755, #30452, #12221, #26844, #15339, #41405, #38085, #23242, #18910, #40697, #5010, #38560, #17222, #39244, #5725, #35214, #1890, #6181, #20341, #20805, #34979, #9089, #16525, #27814, #27337, #46435, #42592, #31154, #13615, #9572, #28256, #45723, #2124, #5489, #10030, #38793, #24651, #23708, #16985, #16754, #31624, #21035, #46204, #13403, #28033, #9805, #6418, #1649, #16293, #7839, #26552, #11643, #8021, #814, #15477, #41063, #12115, #22884, #7549, #30355, #41293, #26017, #40594, #23127, #22159, #16185, #12830, #34390, #20695, #35338, #5858, #34628, #13296, #35100, #1530, #30576, #20223, #41773, #42008, #42263, #45139, #19758, #12357, #30815, #8734, #16647, #13063, #6071, #1777, #31044, #27701, #23370, #23833, #12599, #9463, #2247, #31511, #24081, #38689, #38446, #20465, #16417, #2018, #8975, #5130, #45612, #45384, #16867, #46092, #27461, #26975, #27924, #27221, #34872, #42488, #9694, #5616, #24308, #31276, #38909, #23594, #38208, #15954, #41528, #9211, #45854, #37978, #5369, #19988, #31746, #21652, #3189, #40073, #42955, #24771, #39369, #9929, #21163, #17575, #6784, #2479, #39607, #2938, #32465, #25248, #35795, #42711, #32216, #46803, #6305, #13988, #32696, #29123, #20928, #28638, #17818, #36028, #36285, #35569, #3437, #14464, #47043, #10163, #43675, #7273, #6551, #47286, #43196, #21403, #14235, #7027, #13517, #2714, #39836, #28877, #28150, #17104, #10407, #31976, #24536, #46333, #39136, #10643, #17341, #18050, #25009, #43435, #28386, #21891, #46561, #10885, #13745, #25505, #43914, #30058, #40536, #3667, #4583, #37197, #44600, #295, #44146, #7965, #52, #25956, #4341, #36512, #41003, #36737, #14942, #25736, #22584, #14700, #22815, #8192, #29604, #37430, #4123, #3895, #33637, #22110, #11345, #22342, #36970, #33405, #15180, #18974, #29024, #35709, #14377, #43582, #28537, #10796, #21552, #25408, #29278, #3095, #39742, #17482, #39984, #6929, #7175, #43824, #21801, #22023, #32370, #43104, #17722, #36649, #2846, #10311, #36426, #3582, #32116, #18201, #32842, #47437, #46948, #21072, #13656, #24923, #31892, #11024, #39515, #14605, #25642, #39280, #35935, #40217, #28293, #7407, #14142, #21307, #6690, #3809, #10066, #28783, #46472, #25152, #6455, #42855, #43349, #24683, #46703, #13893, #10553, #36189, #3345, #17953, #32609, #47197, #8348, #37833, #34024, #7637, #15092, #201, #11735, #44988, #41145, #30210, #11257, #22974, #44281, #14849, #8111, #37582, #18425, #11972, #40682, #40915, #41381, #4259, #15571, #22252, #909, #44755, #29739, #26593, #22734, #4744, #15806, #37112, #26354, #4039, #19370, #37339, #1150, #30434, #12198, #8582, #18893, #11485, #33548, #23220, #36886, #26107, #26825 ) ),
 .UNSPECIFIED., .F., .F., .T. ) 
 B_SPLINE_SURFACE_WITH_KNOTS ( ( 2, 2 ),
 ( 3, 2, 2, 2, 2, 2, 2, 2, 2, 2, 2, 2, 2, 2, 2, 2, 2, 2, 2, 2, 2, 2, 2, 2, 2, 2, 2, 2, 2, 2, 2, 2, 2, 2, 2, 2, 2, 2, 2, 2, 2, 2, 2, 2, 2, 2, 2, 2, 2, 2, 2, 2, 2, 2, 2, 2, 2, 2, 2, 2, 2, 2, 2, 2, 2, 2, 2, 2, 2, 2, 2, 2, 2, 2, 2, 2, 2, 2, 2, 2, 2, 2, 2, 2, 2, 2, 2, 2, 2, 2, 2, 2, 2, 2, 2, 2, 2, 2, 2, 2, 2, 2, 2, 2, 2, 2, 2, 2, 2, 2, 2, 2, 2, 2, 2, 2, 2, 2, 2, 2, 2, 2, 2, 2, 2, 2, 2, 2, 2, 2, 2, 2, 2, 2, 2, 2, 2, 2, 2, 2, 2, 2, 2, 2, 2, 2, 2, 2, 2, 2, 2, 2, 2, 2, 2, 2, 2, 2, 2, 2, 2, 2, 2, 2, 2, 2, 2, 2, 2, 2, 2, 2, 2, 2, 2, 2, 2, 2, 2, 2, 2, 2, 2, 2, 2, 2, 2, 2, 2, 2, 2, 2, 2, 2, 2, 2, 2, 2, 2, 2, 2, 2, 2, 2, 2, 2, 2, 2, 2, 2, 2, 2, 2, 2, 2, 2, 2, 2, 2, 2, 2, 2, 2, 2, 2, 2, 2, 2, 2, 2, 2, 2, 2, 2, 2, 2, 2, 2, 2, 2, 2, 2, 2, 2, 2, 2, 2, 2, 2, 2, 2, 2, 2, 2, 2, 2, 2, 2, 2, 2, 2, 2, 2, 2, 2, 2, 2, 2, 2, 2, 2, 2, 2, 2, 2, 2, 2, 2, 2, 2, 2, 2, 2, 2, 2, 2, 2, 2, 2, 2, 2, 2, 2, 2, 2, 2, 2, 2, 2, 2, 2, 2, 2, 2, 2, 2, 2, 2, 2, 2, 2, 2, 2, 2, 2, 2, 2, 2, 2, 2, 2, 2, 2, 2, 2, 2, 2, 2, 2, 2, 2, 2, 2, 2, 2, 2, 2, 2, 2, 2, 2, 2, 2, 2, 2, 2, 2, 2, 2, 2, 2, 2, 2, 2, 2, 2, 2, 2, 2, 2, 2, 2, 2, 2, 2, 2, 2, 2, 2, 2, 2, 2, 2, 2, 2, 2, 2, 2, 2, 2, 2, 2, 2, 2, 2, 2, 2, 2, 2, 2, 2, 2, 2, 2, 2, 2, 2, 2, 2, 2, 3 ),
 ( 0.000000000000000000, 1.000000000000000000 ),
 ( 0.000000000000000000, 0.002500000000000000052, 0.005000000000000000104, 0.007499999999999999722, 0.01000000000000000021, 0.01250000000000000069, 0.01499999999999999944, 0.01750000000000000167, 0.02000000000000000042, 0.02249999999999999917, 0.02500000000000000139, 0.02750000000000000014, 0.02999999999999999889, 0.03250000000000000111, 0.03500000000000000333, 0.03749999999999999861, 0.04000000000000000083, 0.04250000000000000305, 0.04499999999999999833, 0.04750000000000000056, 0.05000000000000000278, 0.05249999999999999806, 0.05500000000000000028, 0.05750000000000000250, 0.05999999999999999778, 0.06250000000000000000, 0.06500000000000000222, 0.06750000000000000444, 0.07000000000000000666, 0.07249999999999999500, 0.07499999999999999722, 0.07749999999999999944, 0.08000000000000000167, 0.08250000000000000389, 0.08500000000000000611, 0.08749999999999999445, 0.08999999999999999667, 0.09249999999999999889, 0.09500000000000000111, 0.09750000000000000333, 0.1000000000000000056, 0.1024999999999999939, 0.1049999999999999961, 0.1074999999999999983, 0.1100000000000000006, 0.1125000000000000028, 0.1150000000000000050, 0.1174999999999999933, 0.1199999999999999956, 0.1224999999999999978, 0.1250000000000000000, 0.1275000000000000022, 0.1300000000000000044, 0.1325000000000000067, 0.1350000000000000089, 0.1375000000000000111, 0.1400000000000000133, 0.1424999999999999878, 0.1449999999999999900, 0.1474999999999999922, 0.1499999999999999944, 0.1524999999999999967, 0.1549999999999999989, 0.1575000000000000011, 0.1600000000000000033, 0.1625000000000000056, 0.1650000000000000078, 0.1675000000000000100, 0.1700000000000000122, 0.1724999999999999867, 0.1749999999999999889, 0.1774999999999999911, 0.1799999999999999933, 0.1824999999999999956, 0.1849999999999999978, 0.1875000000000000000, 0.1900000000000000022, 0.1925000000000000044, 0.1950000000000000067, 0.1975000000000000089, 0.2000000000000000111, 0.2025000000000000133, 0.2049999999999999878, 0.2074999999999999900, 0.2099999999999999922, 0.2124999999999999944, 0.2149999999999999967, 0.2174999999999999989, 0.2200000000000000011, 0.2225000000000000033, 0.2250000000000000056, 0.2275000000000000078, 0.2300000000000000100, 0.2325000000000000122, 0.2349999999999999867, 0.2374999999999999889, 0.2399999999999999911, 0.2424999999999999933, 0.2449999999999999956, 0.2474999999999999978, 0.2500000000000000000, 0.2525000000000000022, 0.2550000000000000044, 0.2575000000000000067, 0.2600000000000000089, 0.2625000000000000111, 0.2650000000000000133, 0.2675000000000000155, 0.2700000000000000178, 0.2725000000000000200, 0.2750000000000000222, 0.2775000000000000244, 0.2800000000000000266, 0.2824999999999999734, 0.2849999999999999756, 0.2874999999999999778, 0.2899999999999999800, 0.2924999999999999822, 0.2949999999999999845, 0.2974999999999999867, 0.2999999999999999889, 0.3024999999999999911, 0.3049999999999999933, 0.3074999999999999956, 0.3099999999999999978, 0.3125000000000000000, 0.3150000000000000022, 0.3175000000000000044, 0.3200000000000000067, 0.3225000000000000089, 0.3250000000000000111, 0.3275000000000000133, 0.3300000000000000155, 0.3325000000000000178, 0.3350000000000000200, 0.3375000000000000222, 0.3400000000000000244, 0.3425000000000000266, 0.3449999999999999734, 0.3474999999999999756, 0.3499999999999999778, 0.3524999999999999800, 0.3549999999999999822, 0.3574999999999999845, 0.3599999999999999867, 0.3624999999999999889, 0.3649999999999999911, 0.3674999999999999933, 0.3699999999999999956, 0.3724999999999999978, 0.3750000000000000000, 0.3775000000000000022, 0.3800000000000000044, 0.3825000000000000067, 0.3850000000000000089, 0.3875000000000000111, 0.3900000000000000133, 0.3925000000000000155, 0.3950000000000000178, 0.3975000000000000200, 0.4000000000000000222, 0.4025000000000000244, 0.4050000000000000266, 0.4074999999999999734, 0.4099999999999999756, 0.4124999999999999778, 0.4149999999999999800, 0.4174999999999999822, 0.4199999999999999845, 0.4224999999999999867, 0.4249999999999999889, 0.4274999999999999911, 0.4299999999999999933, 0.4324999999999999956, 0.4349999999999999978, 0.4375000000000000000, 0.4400000000000000022, 0.4425000000000000044, 0.4450000000000000067, 0.4475000000000000089, 0.4500000000000000111, 0.4525000000000000133, 0.4550000000000000155, 0.4575000000000000178, 0.4600000000000000200, 0.4625000000000000222, 0.4650000000000000244, 0.4675000000000000266, 0.4699999999999999734, 0.4724999999999999756, 0.4749999999999999778, 0.4774999999999999800, 0.4799999999999999822, 0.4824999999999999845, 0.4849999999999999867, 0.4874999999999999889, 0.4899999999999999911, 0.4924999999999999933, 0.4949999999999999956, 0.4974999999999999978, 0.5000000000000000000, 0.5024999999999999467, 0.5050000000000000044, 0.5074999999999999512, 0.5100000000000000089, 0.5124999999999999556, 0.5150000000000000133, 0.5174999999999999600, 0.5200000000000000178, 0.5224999999999999645, 0.5250000000000000222, 0.5274999999999999689, 0.5300000000000000266, 0.5324999999999999734, 0.5350000000000000311, 0.5374999999999999778, 0.5400000000000000355, 0.5424999999999999822, 0.5450000000000000400, 0.5474999999999999867, 0.5500000000000000444, 0.5524999999999999911, 0.5550000000000000488, 0.5574999999999999956, 0.5600000000000000533, 0.5625000000000000000, 0.5649999999999999467, 0.5675000000000000044, 0.5699999999999999512, 0.5725000000000000089, 0.5749999999999999556, 0.5775000000000000133, 0.5799999999999999600, 0.5825000000000000178, 0.5849999999999999645, 0.5875000000000000222, 0.5899999999999999689, 0.5925000000000000266, 0.5949999999999999734, 0.5975000000000000311, 0.5999999999999999778, 0.6025000000000000355, 0.6049999999999999822, 0.6075000000000000400, 0.6099999999999999867, 0.6125000000000000444, 0.6149999999999999911, 0.6175000000000000488, 0.6199999999999999956, 0.6225000000000000533, 0.6250000000000000000, 0.6274999999999999467, 0.6300000000000000044, 0.6324999999999999512, 0.6350000000000000089, 0.6374999999999999556, 0.6400000000000000133, 0.6424999999999999600, 0.6450000000000000178, 0.6474999999999999645, 0.6500000000000000222, 0.6524999999999999689, 0.6550000000000000266, 0.6574999999999999734, 0.6600000000000000311, 0.6624999999999999778, 0.6650000000000000355, 0.6674999999999999822, 0.6700000000000000400, 0.6724999999999999867, 0.6750000000000000444, 0.6774999999999999911, 0.6800000000000000488, 0.6824999999999999956, 0.6850000000000000533, 0.6875000000000000000, 0.6899999999999999467, 0.6925000000000000044, 0.6949999999999999512, 0.6975000000000000089, 0.6999999999999999556, 0.7025000000000000133, 0.7049999999999999600, 0.7075000000000000178, 0.7099999999999999645, 0.7125000000000000222, 0.7149999999999999689, 0.7175000000000000266, 0.7199999999999999734, 0.7225000000000000311, 0.7249999999999999778, 0.7275000000000000355, 0.7299999999999999822, 0.7325000000000000400, 0.7349999999999999867, 0.7375000000000000444, 0.7399999999999999911, 0.7425000000000000488, 0.7449999999999999956, 0.7475000000000000533, 0.7500000000000000000, 0.7524999999999999467, 0.7550000000000000044, 0.7574999999999999512, 0.7600000000000000089, 0.7624999999999999556, 0.7650000000000000133, 0.7674999999999999600, 0.7700000000000000178, 0.7724999999999999645, 0.7750000000000000222, 0.7774999999999999689, 0.7800000000000000266, 0.7824999999999999734, 0.7850000000000000311, 0.7874999999999999778, 0.7900000000000000355, 0.7924999999999999822, 0.7950000000000000400, 0.7974999999999999867, 0.8000000000000000444, 0.8024999999999999911, 0.8050000000000000488, 0.8074999999999999956, 0.8100000000000000533, 0.8125000000000000000, 0.8149999999999999467, 0.8175000000000000044, 0.8199999999999999512, 0.8225000000000000089, 0.8249999999999999556, 0.8275000000000000133, 0.8299999999999999600, 0.8325000000000000178, 0.8349999999999999645, 0.8375000000000000222, 0.8399999999999999689, 0.8425000000000000266, 0.8449999999999999734, 0.8475000000000000311, 0.8499999999999999778, 0.8525000000000000355, 0.8549999999999999822, 0.8575000000000000400, 0.8599999999999999867, 0.8625000000000000444, 0.8649999999999999911, 0.8675000000000000488, 0.8699999999999999956, 0.8725000000000000533, 0.8750000000000000000, 0.8774999999999999467, 0.8800000000000000044, 0.8824999999999999512, 0.8850000000000000089, 0.8874999999999999556, 0.8900000000000000133, 0.8924999999999999600, 0.8950000000000000178, 0.8974999999999999645, 0.9000000000000000222, 0.9024999999999999689, 0.9050000000000000266, 0.9074999999999999734, 0.9100000000000000311, 0.9124999999999999778, 0.9150000000000000355, 0.9174999999999999822, 0.9200000000000000400, 0.9224999999999999867, 0.9250000000000000444, 0.9274999999999999911, 0.9300000000000000488, 0.9324999999999999956, 0.9350000000000000533, 0.9375000000000000000, 0.9399999999999999467, 0.9425000000000000044, 0.9449999999999999512, 0.9475000000000000089, 0.9499999999999999556, 0.9525000000000000133, 0.9549999999999999600, 0.9575000000000000178, 0.9599999999999999645, 0.9625000000000000222, 0.9649999999999999689, 0.9675000000000000266, 0.9699999999999999734, 0.9725000000000000311, 0.9749999999999999778, 0.9775000000000000355, 0.9799999999999999822, 0.9825000000000000400, 0.9849999999999999867, 0.9875000000000000444, 0.9899999999999999911, 0.9925000000000000488, 0.9949999999999999956, 0.9975000000000000533, 1.000000000000000000 ),
 .UNSPECIFIED. ) 
 GEOMETRIC_REPRESENTATION_ITEM ( )  RATIONAL_B_SPLINE_SURFACE ( (
 ( 1.000000000000000000, 0.9238795325112869605, 1.000000000000000000, 0.9238795325112869605, 1.000000000000000000, 0.9238795325112869605, 1.000000000000000000, 0.9238795325112869605, 1.000000000000000000, 0.9238795325112869605, 1.000000000000000000, 0.9238795325112869605, 1.000000000000000000, 0.9238795325112869605, 1.000000000000000000, 0.9238795325112869605, 1.000000000000000000, 0.9238795325112869605, 1.000000000000000000, 0.9238795325112869605, 1.000000000000000000, 0.9238795325112869605, 1.000000000000000000, 0.9238795325112869605, 1.000000000000000000, 0.9238795325112869605, 1.000000000000000000, 0.9238795325112869605, 1.000000000000000000, 0.9238795325112869605, 1.000000000000000000, 0.9238795325112869605, 1.000000000000000000, 0.9238795325112869605, 1.000000000000000000, 0.9238795325112869605, 1.000000000000000000, 0.9238795325112869605, 1.000000000000000000, 0.9238795325112869605, 1.000000000000000000, 0.9238795325112869605, 1.000000000000000000, 0.9238795325112869605, 1.000000000000000000, 0.9238795325112869605, 1.000000000000000000, 0.9238795325112869605, 1.000000000000000000, 0.9238795325112869605, 1.000000000000000000, 0.9238795325112869605, 1.000000000000000000, 0.9238795325112869605, 1.000000000000000000, 0.9238795325112869605, 1.000000000000000000, 0.9238795325112869605, 1.000000000000000000, 0.9238795325112869605, 1.000000000000000000, 0.9238795325112869605, 1.000000000000000000, 0.9238795325112869605, 1.000000000000000000, 0.9238795325112869605, 1.000000000000000000, 0.9238795325112869605, 1.000000000000000000, 0.9238795325112869605, 1.000000000000000000, 0.9238795325112869605, 1.000000000000000000, 0.9238795325112869605, 1.000000000000000000, 0.9238795325112869605, 1.000000000000000000, 0.9238795325112869605, 1.000000000000000000, 0.9238795325112869605, 1.000000000000000000, 0.9238795325112869605, 1.000000000000000000, 0.9238795325112869605, 1.000000000000000000, 0.9238795325112869605, 1.000000000000000000, 0.9238795325112869605, 1.000000000000000000, 0.9238795325112869605, 1.000000000000000000, 0.9238795325112869605, 1.000000000000000000, 0.9238795325112869605, 1.000000000000000000, 0.9238795325112869605, 1.000000000000000000, 0.9238795325112869605, 1.000000000000000000, 0.9238795325112869605, 1.000000000000000000, 0.9238795325112869605, 1.000000000000000000, 0.9238795325112869605, 1.000000000000000000, 0.9238795325112869605, 1.000000000000000000, 0.9238795325112869605, 1.000000000000000000, 0.9238795325112869605, 1.000000000000000000, 0.9238795325112869605, 1.000000000000000000, 0.9238795325112869605, 1.000000000000000000, 0.9238795325112869605, 1.000000000000000000, 0.9238795325112869605, 1.000000000000000000, 0.9238795325112869605, 1.000000000000000000, 0.9238795325112869605, 1.000000000000000000, 0.9238795325112869605, 1.000000000000000000, 0.9238795325112869605, 1.000000000000000000, 0.9238795325112869605, 1.000000000000000000, 0.9238795325112869605, 1.000000000000000000, 0.9238795325112869605, 1.000000000000000000, 0.9238795325112869605, 1.000000000000000000, 0.9238795325112869605, 1.000000000000000000, 0.9238795325112869605, 1.000000000000000000, 0.9238795325112869605, 1.000000000000000000, 0.9238795325112869605, 1.000000000000000000, 0.9238795325112869605, 1.000000000000000000, 0.9238795325112869605, 1.000000000000000000, 0.9238795325112869605, 1.000000000000000000, 0.9238795325112869605, 1.000000000000000000, 0.9238795325112869605, 1.000000000000000000, 0.9238795325112869605, 1.000000000000000000, 0.9238795325112869605, 1.000000000000000000, 0.9238795325112869605, 1.000000000000000000, 0.9238795325112869605, 1.000000000000000000, 0.9238795325112869605, 1.000000000000000000, 0.9238795325112869605, 1.000000000000000000, 0.9238795325112869605, 1.000000000000000000, 0.9238795325112869605, 1.000000000000000000, 0.9238795325112869605, 1.000000000000000000, 0.9238795325112869605, 1.000000000000000000, 0.9238795325112869605, 1.000000000000000000, 0.9238795325112869605, 1.000000000000000000, 0.9238795325112869605, 1.000000000000000000, 0.9238795325112869605, 1.000000000000000000, 0.9238795325112869605, 1.000000000000000000, 0.9238795325112869605, 1.000000000000000000, 0.9238795325112869605, 1.000000000000000000, 0.9238795325112869605, 1.000000000000000000, 0.9238795325112869605, 1.000000000000000000, 0.9238795325112869605, 1.000000000000000000, 0.9238795325112869605, 1.000000000000000000, 0.9238795325112869605, 1.000000000000000000, 0.9238795325112869605, 1.000000000000000000, 0.9238795325112869605, 1.000000000000000000, 0.9238795325112869605, 1.000000000000000000, 0.9238795325112869605, 1.000000000000000000, 0.9238795325112869605, 1.000000000000000000, 0.9238795325112869605, 1.000000000000000000, 0.9238795325112869605, 1.000000000000000000, 0.9238795325112869605, 1.000000000000000000, 0.9238795325112869605, 1.000000000000000000, 0.9238795325112869605, 1.000000000000000000, 0.9238795325112869605, 1.000000000000000000, 0.9238795325112869605, 1.000000000000000000, 0.9238795325112869605, 1.000000000000000000, 0.9238795325112869605, 1.000000000000000000, 0.9238795325112869605, 1.000000000000000000, 0.9238795325112869605, 1.000000000000000000, 0.9238795325112869605, 1.000000000000000000, 0.9238795325112869605, 1.000000000000000000, 0.9238795325112869605, 1.000000000000000000, 0.9238795325112869605, 1.000000000000000000, 0.9238795325112869605, 1.000000000000000000, 0.9238795325112869605, 1.000000000000000000, 0.9238795325112869605, 1.000000000000000000, 0.9238795325112869605, 1.000000000000000000, 0.9238795325112869605, 1.000000000000000000, 0.9238795325112869605, 1.000000000000000000, 0.9238795325112869605, 1.000000000000000000, 0.9238795325112869605, 1.000000000000000000, 0.9238795325112869605, 1.000000000000000000, 0.9238795325112869605, 1.000000000000000000, 0.9238795325112869605, 1.000000000000000000, 0.9238795325112869605, 1.000000000000000000, 0.9238795325112869605, 1.000000000000000000, 0.9238795325112869605, 1.000000000000000000, 0.9238795325112869605, 1.000000000000000000, 0.9238795325112869605, 1.000000000000000000, 0.9238795325112869605, 1.000000000000000000, 0.9238795325112869605, 1.000000000000000000, 0.9238795325112869605, 1.000000000000000000, 0.9238795325112869605, 1.000000000000000000, 0.9238795325112869605, 1.000000000000000000, 0.9238795325112869605, 1.000000000000000000, 0.9238795325112869605, 1.000000000000000000, 0.9238795325112869605, 1.000000000000000000, 0.9238795325112869605, 1.000000000000000000, 0.9238795325112869605, 1.000000000000000000, 0.9238795325112869605, 1.000000000000000000, 0.9238795325112869605, 1.000000000000000000, 0.9238795325112869605, 1.000000000000000000, 0.9238795325112869605, 1.000000000000000000, 0.9238795325112869605, 1.000000000000000000, 0.9238795325112869605, 1.000000000000000000, 0.9238795325112869605, 1.000000000000000000, 0.9238795325112869605, 1.000000000000000000, 0.9238795325112869605, 1.000000000000000000, 0.9238795325112869605, 1.000000000000000000, 0.9238795325112869605, 1.000000000000000000, 0.9238795325112869605, 1.000000000000000000, 0.9238795325112869605, 1.000000000000000000, 0.9238795325112869605, 1.000000000000000000, 0.9238795325112869605, 1.000000000000000000, 0.9238795325112869605, 1.000000000000000000, 0.9238795325112869605, 1.000000000000000000, 0.9238795325112869605, 1.000000000000000000, 0.9238795325112869605, 1.000000000000000000, 0.9238795325112869605, 1.000000000000000000, 0.9238795325112869605, 1.000000000000000000, 0.9238795325112869605, 1.000000000000000000, 0.9238795325112869605, 1.000000000000000000, 0.9238795325112869605, 1.000000000000000000, 0.9238795325112869605, 1.000000000000000000, 0.9238795325112869605, 1.000000000000000000, 0.9238795325112869605, 1.000000000000000000, 0.9238795325112869605, 1.000000000000000000, 0.9238795325112869605, 1.000000000000000000, 0.9238795325112869605, 1.000000000000000000, 0.9238795325112869605, 1.000000000000000000, 0.9238795325112869605, 1.000000000000000000, 0.9238795325112869605, 1.000000000000000000, 0.9238795325112869605, 1.000000000000000000, 0.9238795325112869605, 1.000000000000000000, 0.9238795325112869605, 1.000000000000000000, 0.9238795325112869605, 1.000000000000000000, 0.9238795325112869605, 1.000000000000000000, 0.9238795325112869605, 1.000000000000000000, 0.9238795325112869605, 1.000000000000000000, 0.9238795325112869605, 1.000000000000000000, 0.9238795325112869605, 1.000000000000000000, 0.9238795325112869605, 1.000000000000000000, 0.9238795325112869605, 1.000000000000000000, 0.9238795325112869605, 1.000000000000000000, 0.9238795325112869605, 1.000000000000000000, 0.9238795325112869605, 1.000000000000000000, 0.9238795325112869605, 1.000000000000000000, 0.9238795325112869605, 1.000000000000000000, 0.9238795325112869605, 1.000000000000000000, 0.9238795325112869605, 1.000000000000000000, 0.9238795325112869605, 1.000000000000000000, 0.9238795325112869605, 1.000000000000000000, 0.9238795325112869605, 1.000000000000000000, 0.9238795325112869605, 1.000000000000000000, 0.9238795325112869605, 1.000000000000000000, 0.9238795325112869605, 1.000000000000000000, 0.9238795325112869605, 1.000000000000000000, 0.9238795325112869605, 1.000000000000000000, 0.9238795325112869605, 1.000000000000000000, 0.9238795325112869605, 1.000000000000000000, 0.9238795325112869605, 1.000000000000000000, 0.9238795325112869605, 1.000000000000000000, 0.9238795325112869605, 1.000000000000000000, 0.9238795325112869605, 1.000000000000000000, 0.9238795325112869605, 1.000000000000000000, 0.9238795325112869605, 1.000000000000000000, 0.9238795325112869605, 1.000000000000000000, 0.9238795325112869605, 1.000000000000000000, 0.9238795325112869605, 1.000000000000000000, 0.9238795325112869605, 1.000000000000000000, 0.9238795325112869605, 1.000000000000000000, 0.9238795325112869605, 1.000000000000000000, 0.9238795325112869605, 1.000000000000000000, 0.9238795325112869605, 1.000000000000000000, 0.9238795325112869605, 1.000000000000000000, 0.9238795325112869605, 1.000000000000000000, 0.9238795325112869605, 1.000000000000000000, 0.9238795325112869605, 1.000000000000000000, 0.9238795325112869605, 1.000000000000000000, 0.9238795325112869605, 1.000000000000000000, 0.9238795325112869605, 1.000000000000000000, 0.9238795325112869605, 1.000000000000000000, 0.9238795325112869605, 1.000000000000000000, 0.9238795325112869605, 1.000000000000000000, 0.9238795325112869605, 1.000000000000000000, 0.9238795325112869605, 1.000000000000000000, 0.9238795325112869605, 1.000000000000000000, 0.9238795325112869605, 1.000000000000000000, 0.9238795325112869605, 1.000000000000000000, 0.9238795325112869605, 1.000000000000000000, 0.9238795325112869605, 1.000000000000000000, 0.9238795325112869605, 1.000000000000000000, 0.9238795325112869605, 1.000000000000000000, 0.9238795325112869605, 1.000000000000000000, 0.9238795325112869605, 1.000000000000000000, 0.9238795325112869605, 1.000000000000000000, 0.9238795325112869605, 1.000000000000000000, 0.9238795325112869605, 1.000000000000000000, 0.9238795325112869605, 1.000000000000000000, 0.9238795325112869605, 1.000000000000000000, 0.9238795325112869605, 1.000000000000000000, 0.9238795325112869605, 1.000000000000000000, 0.9238795325112869605, 1.000000000000000000, 0.9238795325112869605, 1.000000000000000000, 0.9238795325112869605, 1.000000000000000000, 0.9238795325112869605, 1.000000000000000000, 0.9238795325112869605, 1.000000000000000000, 0.9238795325112869605, 1.000000000000000000, 0.9238795325112869605, 1.000000000000000000, 0.9238795325112869605, 1.000000000000000000, 0.9238795325112869605, 1.000000000000000000, 0.9238795325112869605, 1.000000000000000000, 0.9238795325112869605, 1.000000000000000000, 0.9238795325112869605, 1.000000000000000000, 0.9238795325112869605, 1.000000000000000000, 0.9238795325112869605, 1.000000000000000000, 0.9238795325112869605, 1.000000000000000000, 0.9238795325112869605, 1.000000000000000000, 0.9238795325112869605, 1.000000000000000000, 0.9238795325112869605, 1.000000000000000000, 0.9238795325112869605, 1.000000000000000000, 0.9238795325112869605, 1.000000000000000000, 0.9238795325112869605, 1.000000000000000000, 0.9238795325112869605, 1.000000000000000000, 0.9238795325112869605, 1.000000000000000000, 0.9238795325112869605, 1.000000000000000000, 0.9238795325112869605, 1.000000000000000000, 0.9238795325112869605, 1.000000000000000000, 0.9238795325112869605, 1.000000000000000000, 0.9238795325112869605, 1.000000000000000000, 0.9238795325112869605, 1.000000000000000000, 0.9238795325112869605, 1.000000000000000000, 0.9238795325112869605, 1.000000000000000000, 0.9238795325112869605, 1.000000000000000000, 0.9238795325112869605, 1.000000000000000000, 0.9238795325112869605, 1.000000000000000000, 0.9238795325112869605, 1.000000000000000000, 0.9238795325112869605, 1.000000000000000000, 0.9238795325112869605, 1.000000000000000000, 0.9238795325112869605, 1.000000000000000000, 0.9238795325112869605, 1.000000000000000000, 0.9238795325112869605, 1.000000000000000000, 0.9238795325112869605, 1.000000000000000000, 0.9238795325112869605, 1.000000000000000000, 0.9238795325112869605, 1.000000000000000000, 0.9238795325112869605, 1.000000000000000000, 0.9238795325112869605, 1.000000000000000000, 0.9238795325112869605, 1.000000000000000000, 0.9238795325112869605, 1.000000000000000000, 0.9238795325112869605, 1.000000000000000000, 0.9238795325112869605, 1.000000000000000000, 0.9238795325112869605, 1.000000000000000000, 0.9238795325112869605, 1.000000000000000000, 0.9238795325112869605, 1.000000000000000000, 0.9238795325112869605, 1.000000000000000000, 0.9238795325112869605, 1.000000000000000000, 0.9238795325112869605, 1.000000000000000000, 0.9238795325112869605, 1.000000000000000000, 0.9238795325112869605, 1.000000000000000000, 0.9238795325112869605, 1.000000000000000000, 0.9238795325112869605, 1.000000000000000000, 0.9238795325112869605, 1.000000000000000000, 0.9238795325112869605, 1.000000000000000000, 0.9238795325112869605, 1.000000000000000000, 0.9238795325112869605, 1.000000000000000000, 0.9238795325112869605, 1.000000000000000000, 0.9238795325112869605, 1.000000000000000000, 0.9238795325112869605, 1.000000000000000000, 0.9238795325112869605, 1.000000000000000000, 0.9238795325112869605, 1.000000000000000000, 0.9238795325112869605, 1.000000000000000000, 0.9238795325112869605, 1.000000000000000000, 0.9238795325112869605, 1.000000000000000000, 0.9238795325112869605, 1.000000000000000000, 0.9238795325112869605, 1.000000000000000000, 0.9238795325112869605, 1.000000000000000000, 0.9238795325112869605, 1.000000000000000000, 0.9238795325112869605, 1.000000000000000000, 0.9238795325112869605, 1.000000000000000000, 0.9238795325112869605, 1.000000000000000000, 0.9238795325112869605, 1.000000000000000000, 0.9238795325112869605, 1.000000000000000000, 0.9238795325112869605, 1.000000000000000000, 0.9238795325112869605, 1.000000000000000000, 0.9238795325112869605, 1.000000000000000000, 0.9238795325112869605, 1.000000000000000000, 0.9238795325112869605, 1.000000000000000000, 0.9238795325112869605, 1.000000000000000000, 0.9238795325112869605, 1.000000000000000000, 0.9238795325112869605, 1.000000000000000000, 0.9238795325112869605, 1.000000000000000000, 0.9238795325112869605, 1.000000000000000000, 0.9238795325112869605, 1.000000000000000000, 0.9238795325112869605, 1.000000000000000000, 0.9238795325112869605, 1.000000000000000000, 0.9238795325112869605, 1.000000000000000000, 0.9238795325112869605, 1.000000000000000000, 0.9238795325112869605, 1.000000000000000000, 0.9238795325112869605, 1.000000000000000000, 0.9238795325112869605, 1.000000000000000000, 0.9238795325112869605, 1.000000000000000000, 0.9238795325112869605, 1.000000000000000000, 0.9238795325112869605, 1.000000000000000000, 0.9238795325112869605, 1.000000000000000000, 0.9238795325112869605, 1.000000000000000000, 0.9238795325112869605, 1.000000000000000000, 0.9238795325112869605, 1.000000000000000000, 0.9238795325112869605, 1.000000000000000000, 0.9238795325112869605, 1.000000000000000000, 0.9238795325112869605, 1.000000000000000000, 0.9238795325112869605, 1.000000000000000000, 0.9238795325112869605, 1.000000000000000000, 0.9238795325112869605, 1.000000000000000000, 0.9238795325112869605, 1.000000000000000000, 0.9238795325112869605, 1.000000000000000000, 0.9238795325112869605, 1.000000000000000000, 0.9238795325112869605, 1.000000000000000000, 0.9238795325112869605, 1.000000000000000000, 0.9238795325112869605, 1.000000000000000000, 0.9238795325112869605, 1.000000000000000000, 0.9238795325112869605, 1.000000000000000000, 0.9238795325112869605, 1.000000000000000000, 0.9238795325112869605, 1.000000000000000000, 0.9238795325112869605, 1.000000000000000000, 0.9238795325112869605, 1.000000000000000000, 0.9238795325112869605, 1.000000000000000000, 0.9238795325112869605, 1.000000000000000000, 0.9238795325112869605, 1.000000000000000000, 0.9238795325112869605, 1.000000000000000000, 0.9238795325112869605, 1.000000000000000000, 0.9238795325112869605, 1.000000000000000000, 0.9238795325112869605, 1.000000000000000000, 0.9238795325112869605, 1.000000000000000000, 0.9238795325112869605, 1.000000000000000000, 0.9238795325112869605, 1.000000000000000000, 0.9238795325112869605, 1.000000000000000000, 0.9238795325112869605, 1.000000000000000000, 0.9238795325112869605, 1.000000000000000000, 0.9238795325112869605, 1.000000000000000000, 0.9238795325112869605, 1.000000000000000000, 0.9238795325112869605, 1.000000000000000000, 0.9238795325112869605, 1.000000000000000000, 0.9238795325112869605, 1.000000000000000000, 0.9238795325112869605, 1.000000000000000000, 0.9238795325112869605, 1.000000000000000000, 0.9238795325112869605, 1.000000000000000000, 0.9238795325112869605, 1.000000000000000000, 0.9238795325112869605, 1.000000000000000000, 0.9238795325112869605, 1.000000000000000000, 0.9238795325112869605, 1.000000000000000000, 0.9238795325112869605, 1.000000000000000000, 0.9238795325112869605, 1.000000000000000000, 0.9238795325112869605, 1.000000000000000000, 0.9238795325112869605, 1.000000000000000000, 0.9238795325112869605, 1.000000000000000000),
 ( 1.000000000000000000, 0.9238795325112869605, 1.000000000000000000, 0.9238795325112869605, 1.000000000000000000, 0.9238795325112869605, 1.000000000000000000, 0.9238795325112869605, 1.000000000000000000, 0.9238795325112869605, 1.000000000000000000, 0.9238795325112869605, 1.000000000000000000, 0.9238795325112869605, 1.000000000000000000, 0.9238795325112869605, 1.000000000000000000, 0.9238795325112869605, 1.000000000000000000, 0.9238795325112869605, 1.000000000000000000, 0.9238795325112869605, 1.000000000000000000, 0.9238795325112869605, 1.000000000000000000, 0.9238795325112869605, 1.000000000000000000, 0.9238795325112869605, 1.000000000000000000, 0.9238795325112869605, 1.000000000000000000, 0.9238795325112869605, 1.000000000000000000, 0.9238795325112869605, 1.000000000000000000, 0.9238795325112869605, 1.000000000000000000, 0.9238795325112869605, 1.000000000000000000, 0.9238795325112869605, 1.000000000000000000, 0.9238795325112869605, 1.000000000000000000, 0.9238795325112869605, 1.000000000000000000, 0.9238795325112869605, 1.000000000000000000, 0.9238795325112869605, 1.000000000000000000, 0.9238795325112869605, 1.000000000000000000, 0.9238795325112869605, 1.000000000000000000, 0.9238795325112869605, 1.000000000000000000, 0.9238795325112869605, 1.000000000000000000, 0.9238795325112869605, 1.000000000000000000, 0.9238795325112869605, 1.000000000000000000, 0.9238795325112869605, 1.000000000000000000, 0.9238795325112869605, 1.000000000000000000, 0.9238795325112869605, 1.000000000000000000, 0.9238795325112869605, 1.000000000000000000, 0.9238795325112869605, 1.000000000000000000, 0.9238795325112869605, 1.000000000000000000, 0.9238795325112869605, 1.000000000000000000, 0.9238795325112869605, 1.000000000000000000, 0.9238795325112869605, 1.000000000000000000, 0.9238795325112869605, 1.000000000000000000, 0.9238795325112869605, 1.000000000000000000, 0.9238795325112869605, 1.000000000000000000, 0.9238795325112869605, 1.000000000000000000, 0.9238795325112869605, 1.000000000000000000, 0.9238795325112869605, 1.000000000000000000, 0.9238795325112869605, 1.000000000000000000, 0.9238795325112869605, 1.000000000000000000, 0.9238795325112869605, 1.000000000000000000, 0.9238795325112869605, 1.000000000000000000, 0.9238795325112869605, 1.000000000000000000, 0.9238795325112869605, 1.000000000000000000, 0.9238795325112869605, 1.000000000000000000, 0.9238795325112869605, 1.000000000000000000, 0.9238795325112869605, 1.000000000000000000, 0.9238795325112869605, 1.000000000000000000, 0.9238795325112869605, 1.000000000000000000, 0.9238795325112869605, 1.000000000000000000, 0.9238795325112869605, 1.000000000000000000, 0.9238795325112869605, 1.000000000000000000, 0.9238795325112869605, 1.000000000000000000, 0.9238795325112869605, 1.000000000000000000, 0.9238795325112869605, 1.000000000000000000, 0.9238795325112869605, 1.000000000000000000, 0.9238795325112869605, 1.000000000000000000, 0.9238795325112869605, 1.000000000000000000, 0.9238795325112869605, 1.000000000000000000, 0.9238795325112869605, 1.000000000000000000, 0.9238795325112869605, 1.000000000000000000, 0.9238795325112869605, 1.000000000000000000, 0.9238795325112869605, 1.000000000000000000, 0.9238795325112869605, 1.000000000000000000, 0.9238795325112869605, 1.000000000000000000, 0.9238795325112869605, 1.000000000000000000, 0.9238795325112869605, 1.000000000000000000, 0.9238795325112869605, 1.000000000000000000, 0.9238795325112869605, 1.000000000000000000, 0.9238795325112869605, 1.000000000000000000, 0.9238795325112869605, 1.000000000000000000, 0.9238795325112869605, 1.000000000000000000, 0.9238795325112869605, 1.000000000000000000, 0.9238795325112869605, 1.000000000000000000, 0.9238795325112869605, 1.000000000000000000, 0.9238795325112869605, 1.000000000000000000, 0.9238795325112869605, 1.000000000000000000, 0.9238795325112869605, 1.000000000000000000, 0.9238795325112869605, 1.000000000000000000, 0.9238795325112869605, 1.000000000000000000, 0.9238795325112869605, 1.000000000000000000, 0.9238795325112869605, 1.000000000000000000, 0.9238795325112869605, 1.000000000000000000, 0.9238795325112869605, 1.000000000000000000, 0.9238795325112869605, 1.000000000000000000, 0.9238795325112869605, 1.000000000000000000, 0.9238795325112869605, 1.000000000000000000, 0.9238795325112869605, 1.000000000000000000, 0.9238795325112869605, 1.000000000000000000, 0.9238795325112869605, 1.000000000000000000, 0.9238795325112869605, 1.000000000000000000, 0.9238795325112869605, 1.000000000000000000, 0.9238795325112869605, 1.000000000000000000, 0.9238795325112869605, 1.000000000000000000, 0.9238795325112869605, 1.000000000000000000, 0.9238795325112869605, 1.000000000000000000, 0.9238795325112869605, 1.000000000000000000, 0.9238795325112869605, 1.000000000000000000, 0.9238795325112869605, 1.000000000000000000, 0.9238795325112869605, 1.000000000000000000, 0.9238795325112869605, 1.000000000000000000, 0.9238795325112869605, 1.000000000000000000, 0.9238795325112869605, 1.000000000000000000, 0.9238795325112869605, 1.000000000000000000, 0.9238795325112869605, 1.000000000000000000, 0.9238795325112869605, 1.000000000000000000, 0.9238795325112869605, 1.000000000000000000, 0.9238795325112869605, 1.000000000000000000, 0.9238795325112869605, 1.000000000000000000, 0.9238795325112869605, 1.000000000000000000, 0.9238795325112869605, 1.000000000000000000, 0.9238795325112869605, 1.000000000000000000, 0.9238795325112869605, 1.000000000000000000, 0.9238795325112869605, 1.000000000000000000, 0.9238795325112869605, 1.000000000000000000, 0.9238795325112869605, 1.000000000000000000, 0.9238795325112869605, 1.000000000000000000, 0.9238795325112869605, 1.000000000000000000, 0.9238795325112869605, 1.000000000000000000, 0.9238795325112869605, 1.000000000000000000, 0.9238795325112869605, 1.000000000000000000, 0.9238795325112869605, 1.000000000000000000, 0.9238795325112869605, 1.000000000000000000, 0.9238795325112869605, 1.000000000000000000, 0.9238795325112869605, 1.000000000000000000, 0.9238795325112869605, 1.000000000000000000, 0.9238795325112869605, 1.000000000000000000, 0.9238795325112869605, 1.000000000000000000, 0.9238795325112869605, 1.000000000000000000, 0.9238795325112869605, 1.000000000000000000, 0.9238795325112869605, 1.000000000000000000, 0.9238795325112869605, 1.000000000000000000, 0.9238795325112869605, 1.000000000000000000, 0.9238795325112869605, 1.000000000000000000, 0.9238795325112869605, 1.000000000000000000, 0.9238795325112869605, 1.000000000000000000, 0.9238795325112869605, 1.000000000000000000, 0.9238795325112869605, 1.000000000000000000, 0.9238795325112869605, 1.000000000000000000, 0.9238795325112869605, 1.000000000000000000, 0.9238795325112869605, 1.000000000000000000, 0.9238795325112869605, 1.000000000000000000, 0.9238795325112869605, 1.000000000000000000, 0.9238795325112869605, 1.000000000000000000, 0.9238795325112869605, 1.000000000000000000, 0.9238795325112869605, 1.000000000000000000, 0.9238795325112869605, 1.000000000000000000, 0.9238795325112869605, 1.000000000000000000, 0.9238795325112869605, 1.000000000000000000, 0.9238795325112869605, 1.000000000000000000, 0.9238795325112869605, 1.000000000000000000, 0.9238795325112869605, 1.000000000000000000, 0.9238795325112869605, 1.000000000000000000, 0.9238795325112869605, 1.000000000000000000, 0.9238795325112869605, 1.000000000000000000, 0.9238795325112869605, 1.000000000000000000, 0.9238795325112869605, 1.000000000000000000, 0.9238795325112869605, 1.000000000000000000, 0.9238795325112869605, 1.000000000000000000, 0.9238795325112869605, 1.000000000000000000, 0.9238795325112869605, 1.000000000000000000, 0.9238795325112869605, 1.000000000000000000, 0.9238795325112869605, 1.000000000000000000, 0.9238795325112869605, 1.000000000000000000, 0.9238795325112869605, 1.000000000000000000, 0.9238795325112869605, 1.000000000000000000, 0.9238795325112869605, 1.000000000000000000, 0.9238795325112869605, 1.000000000000000000, 0.9238795325112869605, 1.000000000000000000, 0.9238795325112869605, 1.000000000000000000, 0.9238795325112869605, 1.000000000000000000, 0.9238795325112869605, 1.000000000000000000, 0.9238795325112869605, 1.000000000000000000, 0.9238795325112869605, 1.000000000000000000, 0.9238795325112869605, 1.000000000000000000, 0.9238795325112869605, 1.000000000000000000, 0.9238795325112869605, 1.000000000000000000, 0.9238795325112869605, 1.000000000000000000, 0.9238795325112869605, 1.000000000000000000, 0.9238795325112869605, 1.000000000000000000, 0.9238795325112869605, 1.000000000000000000, 0.9238795325112869605, 1.000000000000000000, 0.9238795325112869605, 1.000000000000000000, 0.9238795325112869605, 1.000000000000000000, 0.9238795325112869605, 1.000000000000000000, 0.9238795325112869605, 1.000000000000000000, 0.9238795325112869605, 1.000000000000000000, 0.9238795325112869605, 1.000000000000000000, 0.9238795325112869605, 1.000000000000000000, 0.9238795325112869605, 1.000000000000000000, 0.9238795325112869605, 1.000000000000000000, 0.9238795325112869605, 1.000000000000000000, 0.9238795325112869605, 1.000000000000000000, 0.9238795325112869605, 1.000000000000000000, 0.9238795325112869605, 1.000000000000000000, 0.9238795325112869605, 1.000000000000000000, 0.9238795325112869605, 1.000000000000000000, 0.9238795325112869605, 1.000000000000000000, 0.9238795325112869605, 1.000000000000000000, 0.9238795325112869605, 1.000000000000000000, 0.9238795325112869605, 1.000000000000000000, 0.9238795325112869605, 1.000000000000000000, 0.9238795325112869605, 1.000000000000000000, 0.9238795325112869605, 1.000000000000000000, 0.9238795325112869605, 1.000000000000000000, 0.9238795325112869605, 1.000000000000000000, 0.9238795325112869605, 1.000000000000000000, 0.9238795325112869605, 1.000000000000000000, 0.9238795325112869605, 1.000000000000000000, 0.9238795325112869605, 1.000000000000000000, 0.9238795325112869605, 1.000000000000000000, 0.9238795325112869605, 1.000000000000000000, 0.9238795325112869605, 1.000000000000000000, 0.9238795325112869605, 1.000000000000000000, 0.9238795325112869605, 1.000000000000000000, 0.9238795325112869605, 1.000000000000000000, 0.9238795325112869605, 1.000000000000000000, 0.9238795325112869605, 1.000000000000000000, 0.9238795325112869605, 1.000000000000000000, 0.9238795325112869605, 1.000000000000000000, 0.9238795325112869605, 1.000000000000000000, 0.9238795325112869605, 1.000000000000000000, 0.9238795325112869605, 1.000000000000000000, 0.9238795325112869605, 1.000000000000000000, 0.9238795325112869605, 1.000000000000000000, 0.9238795325112869605, 1.000000000000000000, 0.9238795325112869605, 1.000000000000000000, 0.9238795325112869605, 1.000000000000000000, 0.9238795325112869605, 1.000000000000000000, 0.9238795325112869605, 1.000000000000000000, 0.9238795325112869605, 1.000000000000000000, 0.9238795325112869605, 1.000000000000000000, 0.9238795325112869605, 1.000000000000000000, 0.9238795325112869605, 1.000000000000000000, 0.9238795325112869605, 1.000000000000000000, 0.9238795325112869605, 1.000000000000000000, 0.9238795325112869605, 1.000000000000000000, 0.9238795325112869605, 1.000000000000000000, 0.9238795325112869605, 1.000000000000000000, 0.9238795325112869605, 1.000000000000000000, 0.9238795325112869605, 1.000000000000000000, 0.9238795325112869605, 1.000000000000000000, 0.9238795325112869605, 1.000000000000000000, 0.9238795325112869605, 1.000000000000000000, 0.9238795325112869605, 1.000000000000000000, 0.9238795325112869605, 1.000000000000000000, 0.9238795325112869605, 1.000000000000000000, 0.9238795325112869605, 1.000000000000000000, 0.9238795325112869605, 1.000000000000000000, 0.9238795325112869605, 1.000000000000000000, 0.9238795325112869605, 1.000000000000000000, 0.9238795325112869605, 1.000000000000000000, 0.9238795325112869605, 1.000000000000000000, 0.9238795325112869605, 1.000000000000000000, 0.9238795325112869605, 1.000000000000000000, 0.9238795325112869605, 1.000000000000000000, 0.9238795325112869605, 1.000000000000000000, 0.9238795325112869605, 1.000000000000000000, 0.9238795325112869605, 1.000000000000000000, 0.9238795325112869605, 1.000000000000000000, 0.9238795325112869605, 1.000000000000000000, 0.9238795325112869605, 1.000000000000000000, 0.9238795325112869605, 1.000000000000000000, 0.9238795325112869605, 1.000000000000000000, 0.9238795325112869605, 1.000000000000000000, 0.9238795325112869605, 1.000000000000000000, 0.9238795325112869605, 1.000000000000000000, 0.9238795325112869605, 1.000000000000000000, 0.9238795325112869605, 1.000000000000000000, 0.9238795325112869605, 1.000000000000000000, 0.9238795325112869605, 1.000000000000000000, 0.9238795325112869605, 1.000000000000000000, 0.9238795325112869605, 1.000000000000000000, 0.9238795325112869605, 1.000000000000000000, 0.9238795325112869605, 1.000000000000000000, 0.9238795325112869605, 1.000000000000000000, 0.9238795325112869605, 1.000000000000000000, 0.9238795325112869605, 1.000000000000000000, 0.9238795325112869605, 1.000000000000000000, 0.9238795325112869605, 1.000000000000000000, 0.9238795325112869605, 1.000000000000000000, 0.9238795325112869605, 1.000000000000000000, 0.9238795325112869605, 1.000000000000000000, 0.9238795325112869605, 1.000000000000000000, 0.9238795325112869605, 1.000000000000000000, 0.9238795325112869605, 1.000000000000000000, 0.9238795325112869605, 1.000000000000000000, 0.9238795325112869605, 1.000000000000000000, 0.9238795325112869605, 1.000000000000000000, 0.9238795325112869605, 1.000000000000000000, 0.9238795325112869605, 1.000000000000000000, 0.9238795325112869605, 1.000000000000000000, 0.9238795325112869605, 1.000000000000000000, 0.9238795325112869605, 1.000000000000000000, 0.9238795325112869605, 1.000000000000000000, 0.9238795325112869605, 1.000000000000000000, 0.9238795325112869605, 1.000000000000000000, 0.9238795325112869605, 1.000000000000000000, 0.9238795325112869605, 1.000000000000000000, 0.9238795325112869605, 1.000000000000000000, 0.9238795325112869605, 1.000000000000000000, 0.9238795325112869605, 1.000000000000000000, 0.9238795325112869605, 1.000000000000000000, 0.9238795325112869605, 1.000000000000000000, 0.9238795325112869605, 1.000000000000000000, 0.9238795325112869605, 1.000000000000000000, 0.9238795325112869605, 1.000000000000000000, 0.9238795325112869605, 1.000000000000000000, 0.9238795325112869605, 1.000000000000000000, 0.9238795325112869605, 1.000000000000000000, 0.9238795325112869605, 1.000000000000000000, 0.9238795325112869605, 1.000000000000000000, 0.9238795325112869605, 1.000000000000000000, 0.9238795325112869605, 1.000000000000000000, 0.9238795325112869605, 1.000000000000000000, 0.9238795325112869605, 1.000000000000000000, 0.9238795325112869605, 1.000000000000000000, 0.9238795325112869605, 1.000000000000000000, 0.9238795325112869605, 1.000000000000000000, 0.9238795325112869605, 1.000000000000000000, 0.9238795325112869605, 1.000000000000000000, 0.9238795325112869605, 1.000000000000000000, 0.9238795325112869605, 1.000000000000000000, 0.9238795325112869605, 1.000000000000000000, 0.9238795325112869605, 1.000000000000000000, 0.9238795325112869605, 1.000000000000000000, 0.9238795325112869605, 1.000000000000000000, 0.9238795325112869605, 1.000000000000000000, 0.9238795325112869605, 1.000000000000000000, 0.9238795325112869605, 1.000000000000000000, 0.9238795325112869605, 1.000000000000000000, 0.9238795325112869605, 1.000000000000000000, 0.9238795325112869605, 1.000000000000000000, 0.9238795325112869605, 1.000000000000000000, 0.9238795325112869605, 1.000000000000000000, 0.9238795325112869605, 1.000000000000000000, 0.9238795325112869605, 1.000000000000000000, 0.9238795325112869605, 1.000000000000000000, 0.9238795325112869605, 1.000000000000000000, 0.9238795325112869605, 1.000000000000000000, 0.9238795325112869605, 1.000000000000000000, 0.9238795325112869605, 1.000000000000000000, 0.9238795325112869605, 1.000000000000000000, 0.9238795325112869605, 1.000000000000000000, 0.9238795325112869605, 1.000000000000000000, 0.9238795325112869605, 1.000000000000000000, 0.9238795325112869605, 1.000000000000000000, 0.9238795325112869605, 1.000000000000000000, 0.9238795325112869605, 1.000000000000000000, 0.9238795325112869605, 1.000000000000000000, 0.9238795325112869605, 1.000000000000000000, 0.9238795325112869605, 1.000000000000000000, 0.9238795325112869605, 1.000000000000000000, 0.9238795325112869605, 1.000000000000000000, 0.9238795325112869605, 1.000000000000000000, 0.9238795325112869605, 1.000000000000000000, 0.9238795325112869605, 1.000000000000000000, 0.9238795325112869605, 1.000000000000000000, 0.9238795325112869605, 1.000000000000000000, 0.9238795325112869605, 1.000000000000000000, 0.9238795325112869605, 1.000000000000000000, 0.9238795325112869605, 1.000000000000000000, 0.9238795325112869605, 1.000000000000000000, 0.9238795325112869605, 1.000000000000000000, 0.9238795325112869605, 1.000000000000000000, 0.9238795325112869605, 1.000000000000000000, 0.9238795325112869605, 1.000000000000000000, 0.9238795325112869605, 1.000000000000000000, 0.9238795325112869605, 1.000000000000000000, 0.9238795325112869605, 1.000000000000000000, 0.9238795325112869605, 1.000000000000000000, 0.9238795325112869605, 1.000000000000000000, 0.9238795325112869605, 1.000000000000000000, 0.9238795325112869605, 1.000000000000000000, 0.9238795325112869605, 1.000000000000000000, 0.9238795325112869605, 1.000000000000000000, 0.9238795325112869605, 1.000000000000000000, 0.9238795325112869605, 1.000000000000000000, 0.9238795325112869605, 1.000000000000000000, 0.9238795325112869605, 1.000000000000000000, 0.9238795325112869605, 1.000000000000000000, 0.9238795325112869605, 1.000000000000000000, 0.9238795325112869605, 1.000000000000000000, 0.9238795325112869605, 1.000000000000000000, 0.9238795325112869605, 1.000000000000000000, 0.9238795325112869605, 1.000000000000000000, 0.9238795325112869605, 1.000000000000000000, 0.9238795325112869605, 1.000000000000000000, 0.9238795325112869605, 1.000000000000000000, 0.9238795325112869605, 1.000000000000000000, 0.9238795325112869605, 1.000000000000000000, 0.9238795325112869605, 1.000000000000000000, 0.9238795325112869605, 1.000000000000000000) ) ) 
 REPRESENTATION_ITEM ( '' )  SURFACE ( )  ) ;
#2443 = CARTESIAN_POINT ( 'NONE',  ( -1.054774247047244540, -0.07405724077823318263, 0.8513779527021426707 ) ) ;
#2445 = DIRECTION ( 'NONE',  ( 0.000000000000000000, 0.000000000000000000, 1.000000000000000000 ) ) ;
#2444 = CARTESIAN_POINT ( 'NONE',  ( -0.1113553986120547346, -0.8887795275590552047, 0.1113553986120547346 ) ) ;
#2447 = CARTESIAN_POINT ( 'NONE',  ( -0.7495874582379994377, -0.1138864663351371320, 1.985572741735574853 ) ) ;
#2446 = CARTESIAN_POINT ( 'NONE',  ( 0.1797182628040039087, -1.789906014307454551, -0.07444174185955065859 ) ) ;
#2448 = CARTESIAN_POINT ( 'NONE',  ( 0.1787899950787401882, -0.3745078739619845942, -2.189545951927503898E-17 ) ) ;
#2449 = CARTESIAN_POINT ( 'NONE',  ( 1.054774247047244540, 0.07405724077823318263, 1.525590551127340433 ) ) ;
#2451 = LINE ( 'NONE', #35773, #17015 ) ;
#2450 = CARTESIAN_POINT ( 'NONE',  ( 0.1478471407235095458, 0.09575019180979006672, -0.2000734843705069821 ) ) ;
#2452 = CARTESIAN_POINT ( 'NONE',  ( 0.9500414927467377701, -0.1787899950787401604, 0.3297244093950555954 ) ) ;
#2453 = ORIENTED_EDGE ( 'NONE', *, *, #10481, .F. ) ;
#2454 = CIRCLE ( 'NONE', #29322, 0.09842519685039370636 ) ;
#2456 = ORIENTED_EDGE ( 'NONE', *, *, #26497, .T. ) ;
#2455 = CARTESIAN_POINT ( 'NONE',  ( -0.1465245066994781686, -0.09658349877441900488, -0.2008369897430446471 ) ) ;
#2457 = LINE ( 'NONE', #17083, #4486 ) ;
#2458 = FACE_OUTER_BOUND ( 'NONE', #2611, .T. ) ;
#2459 = CARTESIAN_POINT ( 'NONE',  ( -0.1264236179284866091, -0.1579724408911182820, 0.1264236179284866091 ) ) ;
#2460 = CARTESIAN_POINT ( 'NONE',  ( 1.054774247047244540, 0.07405724077823318263, 0.6151574802611965431 ) ) ;
#2461 = CARTESIAN_POINT ( 'NONE',  ( -0.1787899950787401882, -0.9453740156942677109, 0.000000000000000000 ) ) ;
#2462 = CARTESIAN_POINT ( 'NONE',  ( 0.7952710522841902607, -0.1417631204022561375, 0.03937007543464863396 ) ) ;
#2463 = CARTESIAN_POINT ( 'NONE',  ( 0.000000000000000000, 0.3740157480314960647, 0.9783464566929134243 ) ) ;
#2464 = CARTESIAN_POINT ( 'NONE',  ( -0.9500414927467378812, -0.1787899950787401604, 1.510826771599780294 ) ) ;
#2465 = ORIENTED_EDGE ( 'NONE', *, *, #15820, .T. ) ;
#2466 = CARTESIAN_POINT ( 'NONE',  ( -0.3094241246319156535, -0.02236840013889242890, -1.042174736855756789 ) ) ;
#2467 = CARTESIAN_POINT ( 'NONE',  ( 0.6971942568897626646, 0.07405724077823318263, 0.9498031495525356416 ) ) ;
#2468 = ORIENTED_EDGE ( 'NONE', *, *, #9973, .F. ) ;
#2469 = CARTESIAN_POINT ( 'NONE',  ( -0.7646288533564489232, -0.1113553986120547346, 0.7332677164279054471 ) ) ;
#2470 = CARTESIAN_POINT ( 'NONE',  ( 0.4632545931758527691, 4.616380251121755931E-17, 0.000000000000000000 ) ) ;
#2471 = CARTESIAN_POINT ( 'NONE',  ( 1.054774247047244096, 0.000000000000000000, 1.715059055064346527 ) ) ;
#2472 = CARTESIAN_POINT ( 'NONE',  ( -0.8759842519685039353, 0.1574803149606299191, 1.358267716535433323 ) ) ;
#2473 = CARTESIAN_POINT ( 'NONE',  ( -0.7495606340400177148, -0.1264236179284866091, 0.8341535432533228045 ) ) ;
#2474 = CARTESIAN_POINT ( 'NONE',  ( 0.3690944881889770546, 0.1574803149606328057, 0.7480314960629921295 ) ) ;
#2475 = CARTESIAN_POINT ( 'NONE',  ( -0.7108038343253642033, 0.06841996760810098444, 0.03937007874015843040 ) ) ;
#2476 = CARTESIAN_POINT ( 'NONE',  ( 1.002407869896990045, -0.1264236179284866091, 0.1402559054580474474 ) ) ;
#2477 = CARTESIAN_POINT ( 'NONE',  ( -0.9500414927467377701, -0.1787899950787401604, 0.1328740156942679884 ) ) ;
#2478 = PRODUCT_DEFINITION_CONTEXT ( 'detailed design', #11336, 'design' ) ;
#2479 = CARTESIAN_POINT ( 'NONE',  ( 0.8107537697050253289, -0.1574803149606297803, 1.523129921152316379 ) ) ;
#2480 = VERTEX_POINT ( 'NONE', #27806 ) ;
#2481 = ( BOUNDED_CURVE ( )  B_SPLINE_CURVE ( 2, ( #14931, #40526, #18967, #3657, #36961, #11809, #41215, #33867, #11104 ),
 .UNSPECIFIED., .F., .T. ) 
 B_SPLINE_CURVE_WITH_KNOTS ( ( 3, 2, 2, 2, 3 ),
 ( 0.4400000000000000022, 0.4425000000000000044, 0.4450000000000000067, 0.4475000000000000089, 0.4500000000000000111 ),
 .UNSPECIFIED. ) 
 CURVE ( )  GEOMETRIC_REPRESENTATION_ITEM ( )  RATIONAL_B_SPLINE_CURVE ( ( 1.000000000000000000, 0.9238795325112869605, 1.000000000000000000, 0.9238795325112869605, 1.000000000000000000, 0.9238795325112869605, 1.000000000000000000, 0.9238795325112869605, 1.000000000000000000 ) ) 
 REPRESENTATION_ITEM ( '' )  ) ;
#2482 = DIRECTION ( 'NONE',  ( 0.000000000000000000, 0.000000000000000000, 1.000000000000000000 ) ) ;
#2483 = CARTESIAN_POINT ( 'NONE',  ( 0.2031507276427542419, -0.1782051049717964242, -0.05809220732314481633 ) ) ;
#2484 = CARTESIAN_POINT ( 'NONE',  ( -0.6971942568897648851, -0.07405724077823297447, 1.658464566875369472 ) ) ;
#2485 = ORIENTED_EDGE ( 'NONE', *, *, #8423, .F. ) ;
#2486 = CONICAL_SURFACE ( 'NONE', #27822, 0.09842519685039320676, 0.7853981633972574317 ) ;
#2487 = EDGE_CURVE ( 'NONE', #45388, #23548, #40954, .T. ) ;
#2488 = CARTESIAN_POINT ( 'NONE',  ( -0.2471922904502826535, 0.09312491272442048607, -0.03902281811272231143 ) ) ;
#2489 = CYLINDRICAL_SURFACE ( 'NONE', #43547, 0.1377952755905521298 ) ;
#2490 = CARTESIAN_POINT ( 'NONE',  ( -0.1264236179284866091, -1.202387747756797243, -0.1264236179284866091 ) ) ;
#2491 = ORIENTED_EDGE ( 'NONE', *, *, #37055, .T. ) ;
#2492 = CARTESIAN_POINT ( 'NONE',  ( -1.094772975963752103E-17, -0.1284448818360001965, -0.1787899950787401882 ) ) ;
#2493 = ORIENTED_EDGE ( 'NONE', *, *, #39271, .F. ) ;
#2494 = ORIENTED_EDGE ( 'NONE', *, *, #12903, .T. ) ;
#2495 = AXIS2_PLACEMENT_3D ( 'NONE', #41273, #45592, #27204 ) ;
#2496 = EDGE_CURVE ( 'NONE', #35936, #6499, #7675, .T. ) ;
#2497 = CARTESIAN_POINT ( 'NONE',  ( -0.3161444924769509779, 1.025704337919491005, -1.138861239548321524 ) ) ;
#2498 = DIRECTION ( 'NONE',  ( 1.822029033848725028E-16, 0.000000000000000000, 1.000000000000000000 ) ) ;
#2499 = EDGE_CURVE ( 'NONE', #37113, #40492, #32754, .T. ) ;
#2500 = CARTESIAN_POINT ( 'NONE',  ( 0.8759842519685039353, -0.1574803149606299191, 1.811023622047244208 ) ) ;
#2501 = AXIS2_PLACEMENT_3D ( 'NONE', #40743, #38067, #22556 ) ;
#2502 = CARTESIAN_POINT ( 'NONE',  ( 0.1270800023317771588, -0.2618548332050928962, 0.1270800023317771588 ) ) ;
#2503 = CARTESIAN_POINT ( 'NONE',  ( -1.094772975963752103E-17, -0.8026574802611967652, -0.1787899950787401882 ) ) ;
#2504 = CARTESIAN_POINT ( 'NONE',  ( -0.8019270111902716547, -0.1787899950787401604, 0.4084645668753704162 ) ) ;
#2505 = CARTESIAN_POINT ( 'NONE',  ( -0.9873396505805591694, -0.1113553986120547346, 1.067913385826771755 ) ) ;
#2506 = CARTESIAN_POINT ( 'NONE',  ( 0.1270800023317771588, -1.118154045803517738, -0.1270800023317771588 ) ) ;
#2507 = DIRECTION ( 'NONE',  ( 0.000000000000000000, 0.000000000000000000, -1.000000000000000000 ) ) ;
#2508 = CARTESIAN_POINT ( 'NONE',  ( 0.9500414927467378812, 0.1787899950787401604, 1.018700787347811110 ) ) ;
#2509 = CARTESIAN_POINT ( 'NONE',  ( 0.8759842519685039353, 0.1787899950787401882, 1.567421259788755794 ) ) ;
#2511 = DIRECTION ( 'NONE',  ( 0.000000000000000000, 0.000000000000000000, 1.000000000000000000 ) ) ;
#2510 = DIRECTION ( 'NONE',  ( -1.000000000000000000, 0.000000000000000000, 0.000000000000000000 ) ) ;
#2512 = CARTESIAN_POINT ( 'NONE',  ( -0.1574803149606299191, -0.2237541348899642346, -1.272196386806234925 ) ) ;
#2513 = CARTESIAN_POINT ( 'NONE',  ( -0.9873396505805591694, -0.1113553986120547346, 1.687992125876724536 ) ) ;
#2514 = VECTOR ( 'NONE', #2680, 39.37007874015748143 ) ;
#2515 = CARTESIAN_POINT ( 'NONE',  ( 0.3161444924769165610, 1.798092712879858279, -3.826876940038417718 ) ) ;
#2517 = FACE_OUTER_BOUND ( 'NONE', #41883, .T. ) ;
#2516 = CARTESIAN_POINT ( 'NONE',  ( 0.8759842519685039353, 0.1787899950787401882, 1.094980314906866203 ) ) ;
#2518 = CARTESIAN_POINT ( 'NONE',  ( 0.9500414927467377701, -0.1787899950787401604, 1.948818897584033705 ) ) ;
#2519 = CARTESIAN_POINT ( 'NONE',  ( -0.7495606340400177148, 0.1264236179284866091, 1.139271653489543290 ) ) ;
#2520 = CARTESIAN_POINT ( 'NONE',  ( 1.033464566929134687, 0.06523048226347956391, 0.4355314959554649756 ) ) ;
#2521 = VERTEX_POINT ( 'NONE', #38786 ) ;
#2522 = DIRECTION ( 'NONE',  ( 0.000000000000000000, -1.000000000000000000, 0.000000000000000000 ) ) ;
#2523 = CARTESIAN_POINT ( 'NONE',  ( 1.033416983624987129, 0.02228945808267622855, 0.03936935455931785816 ) ) ;
#2524 = CARTESIAN_POINT ( 'NONE',  ( -0.04517205677937032038, -0.09851383996395098042, -0.1820711016168421181 ) ) ;
#2525 = AXIS2_PLACEMENT_3D ( 'NONE', #19014, #29636, #37478 ) ;
#2526 = CARTESIAN_POINT ( 'NONE',  ( -0.7185039370078746268, 0.06523048226347956391, 0.2928149605223941965 ) ) ;
#2527 = ORIENTED_EDGE ( 'NONE', *, *, #37062, .T. ) ;
#2528 = CARTESIAN_POINT ( 'NONE',  ( 0.8019270111902717657, 0.1787899950787401604, 1.254921259788757348 ) ) ;
#2530 = CARTESIAN_POINT ( 'NONE',  ( 0.8759842519685039353, 0.000000000000000000, 4.498031496062992574 ) ) ;
#2529 = DIRECTION ( 'NONE',  ( -4.336808689942014285E-16, 0.000000000000000000, -1.000000000000000000 ) ) ;
#2531 = CARTESIAN_POINT ( 'NONE',  ( 0.8759842519685039353, 0.1574803149606299191, 0.7283464566929134243 ) ) ;
#2532 = AXIS2_PLACEMENT_3D ( 'NONE', #20521, #46857, #28201 ) ;
#2533 = VERTEX_POINT ( 'NONE', #45242 ) ;
#2534 = CARTESIAN_POINT ( 'NONE',  ( 0.1574803149606299191, 0.4666052258408008302, -0.7025346432751023995 ) ) ;
#2535 = CARTESIAN_POINT ( 'NONE',  ( -0.9412147342319837628, 0.1574803149606300301, 0.2042322833570397733 ) ) ;
#2536 = ADVANCED_FACE ( 'NONE', ( #5943 ), #34036, .T. ) ;
#2537 = ORIENTED_EDGE ( 'NONE', *, *, #20684, .T. ) ;
#2538 = CARTESIAN_POINT ( 'NONE',  ( -0.6971942568897648851, 0.07405724077823318263, 1.338582677111590069 ) ) ;
#2539 = CARTESIAN_POINT ( 'NONE',  ( 0.1787899950787401882, -1.757381889710015965, -2.189545951927503898E-17 ) ) ;
#2540 = CARTESIAN_POINT ( 'NONE',  ( -1.054774247047244540, -0.07405724077823318263, 0.9301181101824563813 ) ) ;
#2541 = CARTESIAN_POINT ( 'NONE',  ( -0.8759842519685039353, -0.1787899950787401882, 1.980807086560409491 ) ) ;
#2542 = CARTESIAN_POINT ( 'NONE',  ( -0.8019270111902716547, -0.1787899950787401604, 1.072834645615528659 ) ) ;
#2543 = CARTESIAN_POINT ( 'NONE',  ( -0.8019270111902717657, 0.1787899950787401604, 0.6692913385289144257 ) ) ;
#2544 = CARTESIAN_POINT ( 'NONE',  ( -0.8759842519685039353, 0.1574803149606299191, 0.08858267705782735257 ) ) ;
#2545 = CARTESIAN_POINT ( 'NONE',  ( -0.07405724077823318263, -0.6782735745284524942, 0.1787899950787401604 ) ) ;
#2546 = EDGE_LOOP ( 'NONE', ( #2786, #19871, #46673, #40472 ) ) ;
#2547 = CARTESIAN_POINT ( 'NONE',  ( -0.1272683714394354237, -0.08956149644601003879, 0.1005630977721749947 ) ) ;
#2548 = FACE_OUTER_BOUND ( 'NONE', #14526, .T. ) ;
#2549 = VERTEX_POINT ( 'NONE', #15817 ) ;
#2550 = CARTESIAN_POINT ( 'NONE',  ( 1.033464566929133799, 0.000000000000000000, 0.7972440944881890035 ) ) ;
#2551 = CARTESIAN_POINT ( 'NONE',  ( -0.8759842519685039353, 0.1787899950787401882, 0.7012795275052913224 ) ) ;
#2552 = CARTESIAN_POINT ( 'NONE',  ( 0.06523048226347956391, -0.01525590551181101734, 0.1574803149606297803 ) ) ;
#2553 = ORIENTED_EDGE ( 'NONE', *, *, #17261, .F. ) ;
#2554 = CARTESIAN_POINT ( 'NONE',  ( -1.002407869896990045, 0.1264236179284866091, 1.606791338528913426 ) ) ;
#2555 = CARTESIAN_POINT ( 'NONE',  ( -0.2559055569979697409, 0.07184629814250909075, -0.3092506151682454241 ) ) ;
#2556 = CARTESIAN_POINT ( 'NONE',  ( -0.9412147342319837628, 0.1574803149606300301, 0.4896653543307082357 ) ) ;
#2557 = CYLINDRICAL_SURFACE ( 'NONE', #31701, 0.1574803149606299191 ) ;
#2558 = CARTESIAN_POINT ( 'NONE',  ( -0.9412147342319837628, 0.1574803149606300301, 1.385334645561763667 ) ) ;
#2559 = CARTESIAN_POINT ( 'NONE',  ( 1.002407869896990045, 0.1264236179284866091, 0.6619094487651338010 ) ) ;
#2561 = CARTESIAN_POINT ( 'NONE',  ( -0.1275149678065370662, -0.09842519685039370636, 0.1062736314024527728 ) ) ;
#2560 = CARTESIAN_POINT ( 'NONE',  ( 0.1574803149606299191, -0.5984251968503937480, -1.928577636452523993E-17 ) ) ;
#2562 = CARTESIAN_POINT ( 'NONE',  ( 0.8759842519685039353, 0.000000000000000000, 4.498031496062992574 ) ) ;
#2563 = ORIENTED_EDGE ( 'NONE', *, *, #13616, .T. ) ;
#2564 = CARTESIAN_POINT ( 'NONE',  ( -0.7185039370078739607, 1.928577636452523993E-17, 0.6889763778452283605 ) ) ;
#2565 = CARTESIAN_POINT ( 'NONE',  ( 0.9412147342319837628, -0.1574803149606297803, 1.222933070866141669 ) ) ;
#2567 = LINE ( 'NONE', #3038, #197 ) ;
#2566 = DIRECTION ( 'NONE',  ( -3.769839275579535403E-17, 0.7880107536067207930, -0.6156614753256599570 ) ) ;
#2568 = DIRECTION ( 'NONE',  ( 1.000000000000000000, 0.000000000000000000, 0.000000000000000000 ) ) ;
#2570 = CARTESIAN_POINT ( 'NONE',  ( 0.3161444924769519216, 1.488499961090669288, -0.3513258257898460579 ) ) ;
#2569 = CARTESIAN_POINT ( 'NONE',  ( 1.002407869896990045, -0.1264236179284866091, 0.6865157479777322935 ) ) ;
#2571 = LINE ( 'NONE', #39233, #13199 ) ;
#2572 = CARTESIAN_POINT ( 'NONE',  ( 0.1787899950787401882, -0.6500984251430865779, -2.189545951927503898E-17 ) ) ;
#2573 = DIRECTION ( 'NONE',  ( -1.000000000000000000, -0.000000000000000000, 0.000000000000000000 ) ) ;
#2574 = VERTEX_POINT ( 'NONE', #1641 ) ;
#2575 = DIRECTION ( 'NONE',  ( 0.000000000000000000, 0.000000000000000000, -1.000000000000000000 ) ) ;
#2576 = CARTESIAN_POINT ( 'NONE',  ( 0.002317115957683009517, 0.1025658529673372232, -0.09794161051897268266 ) ) ;
#2577 = CARTESIAN_POINT ( 'NONE',  ( 0.8019270111902717657, 0.1787899950787401604, 0.9005905511273389896 ) ) ;
#2578 = EDGE_CURVE ( 'NONE', #11036, #3082, #8218, .T. ) ;
#2579 = CARTESIAN_POINT ( 'NONE',  ( 0.4934383202099732468, -0.08090551181102362266, 0.000000000000000000 ) ) ;
#2580 = FACE_OUTER_BOUND ( 'NONE', #28325, .T. ) ;
#2581 = CARTESIAN_POINT ( 'NONE',  ( -0.07444174185955065859, 0.07033020616498604494, -0.1797182628040039087 ) ) ;
#2582 = CARTESIAN_POINT ( 'NONE',  ( 3.284318927891251994E-17, -1.058562992072220377, 0.1787899950787401882 ) ) ;
#2583 = CARTESIAN_POINT ( 'NONE',  ( -0.06523048226347956391, -1.412893700787401174, -0.1574803149606300301 ) ) ;
#2584 = ( BOUNDED_CURVE ( )  B_SPLINE_CURVE ( 2, ( #46113, #31991, #9235, #24786, #2035, #16436, #27940, #27716, #42282 ),
 .UNSPECIFIED., .F., .T. ) 
 B_SPLINE_CURVE_WITH_KNOTS ( ( 3, 2, 2, 2, 3 ),
 ( 0.7299999999999999822, 0.7325000000000000400, 0.7349999999999999867, 0.7375000000000000444, 0.7399999999999999911 ),
 .UNSPECIFIED. ) 
 CURVE ( )  GEOMETRIC_REPRESENTATION_ITEM ( )  RATIONAL_B_SPLINE_CURVE ( ( 1.000000000000000000, 0.9238795325112869605, 1.000000000000000000, 0.9238795325112869605, 1.000000000000000000, 0.9238795325112869605, 1.000000000000000000, 0.9238795325112869605, 1.000000000000000000 ) ) 
 REPRESENTATION_ITEM ( '' )  ) ;
#2585 = ADVANCED_FACE ( 'NONE', ( #32325 ), #47154, .F. ) ;
#2586 = CARTESIAN_POINT ( 'NONE',  ( 0.1608809465420316664, 0.07793157280922068109, -0.1406091075617787456 ) ) ;
#2587 = CARTESIAN_POINT ( 'NONE',  ( -0.8759842519685039353, -0.1787899950787401882, 1.906988188922614125 ) ) ;
#2588 = ORIENTED_EDGE ( 'NONE', *, *, #47395, .F. ) ;
#2589 = ADVANCED_FACE ( 'NONE', ( #6411 ), #28495, .T. ) ;
#2590 = CARTESIAN_POINT ( 'NONE',  ( -0.9873396505805591694, -0.1113553986120547346, 0.8218503935932598425 ) ) ;
#2591 = ORIENTED_EDGE ( 'NONE', *, *, #46408, .T. ) ;
#2592 = CARTESIAN_POINT ( 'NONE',  ( 0.1574803149606299191, -1.415354330601133803, -1.928577636452523993E-17 ) ) ;
#2594 = CARTESIAN_POINT ( 'NONE',  ( -1.054774247047244540, 0.07405724077823318263, 1.919291338528913649 ) ) ;
#2593 = AXIS2_PLACEMENT_3D ( 'NONE', #22968, #30429, #44981 ) ;
#2595 = CARTESIAN_POINT ( 'NONE',  ( -1.054774247047244540, -0.07405724077823318263, 1.594488188922613237 ) ) ;
#2596 = FACE_OUTER_BOUND ( 'NONE', #27100, .T. ) ;
#2597 = CARTESIAN_POINT ( 'NONE',  ( -1.054774247047244540, 0.07405724077823318263, 0.9694881889226144578 ) ) ;
#2598 = CARTESIAN_POINT ( 'NONE',  ( -0.8019270111902717657, 0.1787899950787401604, 0.2362204723871814960 ) ) ;
#2599 = CARTESIAN_POINT ( 'NONE',  ( -0.2471922904502826812, 0.03219022224904106305, 0.1427165354330708902 ) ) ;
#2600 = CARTESIAN_POINT ( 'NONE',  ( -0.7495606340400177148, 0.1264236179284866091, 1.892224409395055096 ) ) ;
#2601 = CARTESIAN_POINT ( 'NONE',  ( 0.8107537697050254399, -0.1574803149606297803, 1.405019684931842816 ) ) ;
#2602 = CARTESIAN_POINT ( 'NONE',  ( -0.8759842519685039353, -0.1574803149606299191, 1.850393700787401619 ) ) ;
#2603 = MECHANICAL_DESIGN_GEOMETRIC_PRESENTATION_REPRESENTATION (  '', ( #12604 ), #30958 ) ;
#2604 = DIRECTION ( 'NONE',  ( 1.000000000000000000, 0.000000000000000000, 0.000000000000000000 ) ) ;
#2605 = CARTESIAN_POINT ( 'NONE',  ( -0.07405724077823318263, -0.2845727871268765585, 0.1787899950787401604 ) ) ;
#2606 = CARTESIAN_POINT ( 'NONE',  ( 0.08207288410471162698, -0.09842519685039370636, -0.1769814723687171687 ) ) ;
#2607 = DIRECTION ( 'NONE',  ( 0.000000000000000000, 0.7071067811862592478, 0.7071067811868357866 ) ) ;
#2608 = CARTESIAN_POINT ( 'NONE',  ( 0.5555748031496109407, 0.9100161909011688088, 0.01858545845903165558 ) ) ;
#2609 = ORIENTED_EDGE ( 'NONE', *, *, #8223, .F. ) ;
#2610 = CARTESIAN_POINT ( 'NONE',  ( -0.6971942568897637749, 2.189545951927499583E-17, 1.227854330654897685 ) ) ;
#2611 = EDGE_LOOP ( 'NONE', ( #44157, #40450, #15239, #25019 ) ) ;
#2612 = CARTESIAN_POINT ( 'NONE',  ( -0.1264236179284866091, -1.265255905458047225, -0.1264236179284866091 ) ) ;
#2613 = DIRECTION ( 'NONE',  ( -1.000000000000000000, 0.000000000000000000, 0.000000000000000000 ) ) ;
#2614 = ( NAMED_UNIT ( * ) PLANE_ANGLE_UNIT ( ) SI_UNIT ( $, .RADIAN. ) ) ;
#2615 = CARTESIAN_POINT ( 'NONE',  ( 3.301370929368692659E-17, -0.4636264867484000129, 0.1797182628040039365 ) ) ;
#2616 = VECTOR ( 'NONE', #7747, 39.37007874015748143 ) ;
#2617 = CARTESIAN_POINT ( 'NONE',  ( 0.1377952755905511861, 0.000000000000000000, -0.09302377043719921301 ) ) ;
#2618 = CARTESIAN_POINT ( 'NONE',  ( -0.9873396505805591694, 0.1113553986120547346, 0.7529527557979842634 ) ) ;
#2619 = CARTESIAN_POINT ( 'NONE',  ( -0.8107537697050253289, -0.1574803149606297803, 0.7849409448818904789 ) ) ;
#2620 = CARTESIAN_POINT ( 'NONE',  ( -0.06523048226347956391, 0.05856299212598428672, 0.1574803149606297803 ) ) ;
#2621 = AXIS2_PLACEMENT_3D ( 'NONE', #28, #28130, #42687 ) ;
#2622 = CARTESIAN_POINT ( 'NONE',  ( 0.8107537697050253289, -0.1574803149606297803, 0.8243110236220465570 ) ) ;
#2623 = CARTESIAN_POINT ( 'NONE',  ( 0.05770278849818187561, -0.2621795117899916594, -0.05428606100832126385 ) ) ;
#2624 = CARTESIAN_POINT ( 'NONE',  ( -0.7646288533564489232, 0.1113553986120547346, 1.245078740157480324 ) ) ;
#2626 = DIRECTION ( 'NONE',  ( 1.822029033848725028E-16, 0.000000000000000000, 1.000000000000000000 ) ) ;
#2625 = CARTESIAN_POINT ( 'NONE',  ( 1.033464566929134687, 0.06523048226347956391, 0.6028543307086614567 ) ) ;
#2627 = CARTESIAN_POINT ( 'NONE',  ( 1.033464566929133799, 0.000000000000000000, 1.102362204616881947 ) ) ;
#2628 = CARTESIAN_POINT ( 'NONE',  ( 0.7646288533564489232, 0.1113553986120547346, 0.1328740156405045225 ) ) ;
#2629 = VERTEX_POINT ( 'NONE', #35207 ) ;
#2630 = EDGE_CURVE ( 'NONE', #12184, #12474, #42498, .T. ) ;
#2631 = ORIENTED_EDGE ( 'NONE', *, *, #43981, .F. ) ;
#2632 = CARTESIAN_POINT ( 'NONE',  ( 1.033464566929133799, 0.000000000000000000, 0.3937007872940480047 ) ) ;
#2633 = CARTESIAN_POINT ( 'NONE',  ( -0.1264236179284866091, -0.5910433070328504623, 0.1264236179284866091 ) ) ;
#2634 = CARTESIAN_POINT ( 'NONE',  ( 0.07405724077823318263, -1.390748031442299082, -0.1787899950787401604 ) ) ;
#2635 = EDGE_CURVE ( 'NONE', #5875, #19741, #27333, .T. ) ;
#2636 = CARTESIAN_POINT ( 'NONE',  ( -0.8019270111902717657, 0.1787899950787401604, 1.845472440891119392 ) ) ;
#2637 = ORIENTED_EDGE ( 'NONE', *, *, #8911, .F. ) ;
#2638 = CARTESIAN_POINT ( 'NONE',  ( -1.054774247047244540, -0.07405724077823318263, 1.441929133804504604 ) ) ;
#2639 = ADVANCED_FACE ( 'NONE', ( #36141 ), #42143, .F. ) ;
#2640 = CARTESIAN_POINT ( 'NONE',  ( 1.002407869896990045, 0.1264236179284866091, 1.606791338528913426 ) ) ;
#2641 = CARTESIAN_POINT ( 'NONE',  ( 0.7646288533564489232, -0.1113553986120547346, 0.9301181101286929431 ) ) ;
#2642 = CARTESIAN_POINT ( 'NONE',  ( -1.002407869896990045, -0.1264236179284866091, 0.6126968503399370380 ) ) ;
#2643 = CARTESIAN_POINT ( 'NONE',  ( 0.7495606340400177148, -0.1264236179284866091, 0.1304133857730082613 ) ) ;
#2644 = EDGE_CURVE ( 'NONE', #46787, #41828, #31616, .T. ) ;
#2645 = CARTESIAN_POINT ( 'NONE',  ( 0.1116671475666351498, -0.09844346291898031787, -0.1397099940965207954 ) ) ;
#2646 = CARTESIAN_POINT ( 'NONE',  ( 0.8019270111902716547, 0.1787899950787401604, 0.6692913385289143147 ) ) ;
#2647 = CARTESIAN_POINT ( 'NONE',  ( -0.8759842519685039353, 0.1787899950787401882, 0.5831692912848189803 ) ) ;
#2648 = CARTESIAN_POINT ( 'NONE',  ( 0.7646288533564489232, -0.1113553986120547346, 0.6250000000000000000 ) ) ;
#2649 = CARTESIAN_POINT ( 'NONE',  ( -0.7185039370078739607, 1.928577636452523993E-17, 0.8562992125984251190 ) ) ;
#2650 = EDGE_LOOP ( 'NONE', ( #10832, #39250, #33625, #36885 ) ) ;
#2651 = CARTESIAN_POINT ( 'NONE',  ( -1.002407869896990045, 0.1264236179284866091, 1.409940944828126153 ) ) ;
#2652 = ORIENTED_EDGE ( 'NONE', *, *, #33847, .T. ) ;
#2653 = VECTOR ( 'NONE', #15346, 39.37007874015748143 ) ;
#2654 = CARTESIAN_POINT ( 'NONE',  ( -0.9873396505805591694, 0.1113553986120547346, 1.471456692913385877 ) ) ;
#2655 = CARTESIAN_POINT ( 'NONE',  ( -0.7185039370078739607, 1.928577636452523993E-17, 0.4232283464566928832 ) ) ;
#2656 = CARTESIAN_POINT ( 'NONE',  ( 1.002407869896990045, -0.1264236179284866091, 1.281988188922614125 ) ) ;
#2657 = CARTESIAN_POINT ( 'NONE',  ( -0.01791479000647193051, -0.09851385005614764212, 0.2243923354945216719 ) ) ;
#2658 = VECTOR ( 'NONE', #14061, 39.37007874015748143 ) ;
#2659 = CARTESIAN_POINT ( 'NONE',  ( -0.1377952755905509641, 0.000000000000000000, -0.06545654452343109553 ) ) ;
#2660 = ORIENTED_EDGE ( 'NONE', *, *, #34982, .T. ) ;
#2661 = CARTESIAN_POINT ( 'NONE',  ( -0.1264236179284866091, -1.714198771378844466, -0.1264236179284866091 ) ) ;
#2662 = ORIENTED_EDGE ( 'NONE', *, *, #14716, .F. ) ;
#2663 = CARTESIAN_POINT ( 'NONE',  ( 0.07405724077823318263, -0.6574803149068665364, 0.1787899950787401604 ) ) ;
#2664 = CARTESIAN_POINT ( 'NONE',  ( 0.1574803149606299746, 3.616083068348478250E-17, 0.2952755905511806334 ) ) ;
#2665 = ORIENTED_EDGE ( 'NONE', *, *, #13291, .F. ) ;
#2666 = CARTESIAN_POINT ( 'NONE',  ( 0.8759842519685039353, -0.1787899950787401882, 1.429625984198204858 ) ) ;
#2667 = CARTESIAN_POINT ( 'NONE',  ( -0.8759842519685039353, 0.000000000000000000, 0.000000000000000000 ) ) ;
#2668 = CARTESIAN_POINT ( 'NONE',  ( 3.284318927891251994E-17, -0.8174212597887557941, 0.1787899950787401882 ) ) ;
#2669 = CARTESIAN_POINT ( 'NONE',  ( 0.8107537697050254399, 0.1574803149606300301, 1.045767716535432879 ) ) ;
#2670 = CARTESIAN_POINT ( 'NONE',  ( 0.000000000000000000, 0.000000000000000000, -0.3001770169643759867 ) ) ;
#2671 = CARTESIAN_POINT ( 'NONE',  ( 1.054774247047244540, -0.07405724077823318263, 0.3346456692375748831 ) ) ;
#2672 = CARTESIAN_POINT ( 'NONE',  ( 0.1787899950787401604, 0.07960044121958026464, 0.07405724077823318263 ) ) ;
#2673 = CARTESIAN_POINT ( 'NONE',  ( -0.1787899950787401882, 0.07332677170730689253, 0.000000000000000000 ) ) ;
#2674 = CARTESIAN_POINT ( 'NONE',  ( -0.8759842519685039353, 0.000000000000000000, 0.000000000000000000 ) ) ;
#2675 = DIRECTION ( 'NONE',  ( -1.000000000000000000, 5.464378949326940770E-15, -4.275490733183370330E-15 ) ) ;
#2676 = AXIS2_PLACEMENT_3D ( 'NONE', #36439, #10566, #40228 ) ;
#2677 = CARTESIAN_POINT ( 'NONE',  ( 1.054774247047244540, -0.07405724077823318263, 0.5314960629383620461 ) ) ;
#2678 = CARTESIAN_POINT ( 'NONE',  ( -1.002407869896990045, 0.1264236179284866091, 0.8193897637257637756 ) ) ;
#2680 = DIRECTION ( 'NONE',  ( 1.822029033848725028E-16, 0.000000000000000000, 1.000000000000000000 ) ) ;
#2679 = CARTESIAN_POINT ( 'NONE',  ( 0.1113553986120547346, -0.8690944881889763884, -0.1113553986120547346 ) ) ;
#2681 = CARTESIAN_POINT ( 'NONE',  ( 0.07444174185955046430, -1.666874518244463310, -0.1797182628040039087 ) ) ;
#2682 = CARTESIAN_POINT ( 'NONE',  ( -9.642888182262618425E-18, -0.4999999998924724576, -0.1574803149606299191 ) ) ;
#2683 = VECTOR ( 'NONE', #9528, 39.37007874015748854 ) ;
#2684 = AXIS2_PLACEMENT_3D ( 'NONE', #41666, #8387, #15851 ) ;
#2685 = CARTESIAN_POINT ( 'NONE',  ( 0.1787899950787401604, -0.3769685038832444324, 0.07405724077823318263 ) ) ;
#2686 = CARTESIAN_POINT ( 'NONE',  ( -1.033464566929133799, 0.000000000000000000, 1.259842519577511810 ) ) ;
#2687 = CARTESIAN_POINT ( 'NONE',  ( 0.8019270111902717657, 0.1787899950787401604, 1.732283464513166615 ) ) ;
#2689 = CARTESIAN_POINT ( 'NONE',  ( 0.2559055118110236671, 0.01223568982215688349, -0.3149606299212600047 ) ) ;
#2688 = CARTESIAN_POINT ( 'NONE',  ( 0.9500414927467377701, -0.1787899950787401604, 1.943897637741510254 ) ) ;
#2690 = CARTESIAN_POINT ( 'NONE',  ( 0.6971942568897637749, 2.189545951927499583E-17, 0.3567913385289137596 ) ) ;
#2691 = AXIS2_PLACEMENT_3D ( 'NONE', #28111, #2436, #1734 ) ;
#2692 = ORIENTED_EDGE ( 'NONE', *, *, #35134, .T. ) ;
#2693 = FACE_OUTER_BOUND ( 'NONE', #5912, .T. ) ;
#2694 = CARTESIAN_POINT ( 'NONE',  ( 0.2133366555414178134, -0.1723185650269667135, -0.3044102143375118641 ) ) ;
#2695 = CARTESIAN_POINT ( 'NONE',  ( -0.1787899950787401882, -0.04478346451316559534, 0.000000000000000000 ) ) ;
#2696 = CARTESIAN_POINT ( 'NONE',  ( 1.054774247047244540, -0.07405724077823318263, 0.5708661416785201226 ) ) ;
#2697 = CARTESIAN_POINT ( 'NONE',  ( 0.1264236179284866091, -0.8912401574265511606, 0.1264236179284866091 ) ) ;
#2698 = CARTESIAN_POINT ( 'NONE',  ( 0.2204724409448818867, 0.000000000000000000, 0.2047244094488188948 ) ) ;
#2699 = EDGE_CURVE ( 'NONE', #47016, #17121, #46197, .T. ) ;
#2700 = CARTESIAN_POINT ( 'NONE',  ( 0.4399002236966062518, 0.8539303365987028771, -1.004656681308842447 ) ) ;
#2701 = FACE_OUTER_BOUND ( 'NONE', #16952, .T. ) ;
#2702 = ORIENTED_EDGE ( 'NONE', *, *, #7149, .T. ) ;
#2703 = CARTESIAN_POINT ( 'NONE',  ( 0.7185039370078739607, 1.928577636452523993E-17, 0.1476377952755905387 ) ) ;
#2704 = CARTESIAN_POINT ( 'NONE',  ( 1.002407869896990045, -0.1264236179284866091, 1.203248031442299304 ) ) ;
#2705 = ORIENTED_EDGE ( 'NONE', *, *, #4811, .F. ) ;
#2706 = CARTESIAN_POINT ( 'NONE',  ( -0.8107537697050253289, 0.1574803149606300301, 0.6815944880814486240 ) ) ;
#2707 = CARTESIAN_POINT ( 'NONE',  ( 0.8759842519685039353, 0.1787899950787401882, 1.882381889710015743 ) ) ;
#2708 = CARTESIAN_POINT ( 'NONE',  ( -1.033464566929133799, 0.000000000000000000, 1.427165354330708569 ) ) ;
#2709 = CARTESIAN_POINT ( 'NONE',  ( -0.7495606340400177148, 0.1264236179284866091, 0.8636811023084409733 ) ) ;
#2710 = EDGE_CURVE ( 'NONE', #3855, #15659, #13395, .T. ) ;
#2711 = DIRECTION ( 'NONE',  ( 0.000000000000000000, 1.000000000000000000, 0.000000000000000000 ) ) ;
#2712 = DIRECTION ( 'NONE',  ( 1.000000000000000000, 0.000000000000000000, 0.000000000000000000 ) ) ;
#2713 = CARTESIAN_POINT ( 'NONE',  ( 0.7495606340400177148, 0.1264236179284866091, 0.1599409448281264023 ) ) ;
#2714 = CARTESIAN_POINT ( 'NONE',  ( 0.8107537697050253289, -0.1574803149606297803, 1.601870078632630756 ) ) ;
#2715 = ORIENTED_EDGE ( 'NONE', *, *, #40441, .T. ) ;
#2716 = CARTESIAN_POINT ( 'NONE',  ( 0.1377952755905511861, 0.1574803149606299191, 0.8070866141732283561 ) ) ;
#2717 = CARTESIAN_POINT ( 'NONE',  ( -0.8019270111902716547, -0.1787899950787401604, 1.702755905458047003 ) ) ;
#2718 = DIRECTION ( 'NONE',  ( 1.822029033848725028E-16, 0.000000000000000000, 1.000000000000000000 ) ) ;
#2719 = DIRECTION ( 'NONE',  ( -3.469446951953590129E-15, -1.000000000000000000, 0.000000000000000000 ) ) ;
#2720 = CARTESIAN_POINT ( 'NONE',  ( -0.1264236179284866091, -1.192545228071757890, 0.1264236179284866091 ) ) ;
#2721 = ORIENTED_EDGE ( 'NONE', *, *, #27894, .F. ) ;
#2722 = CARTESIAN_POINT ( 'NONE',  ( 0.1787899950787401604, -0.09645669285962235606, -0.07405724077823318263 ) ) ;
#2723 = CIRCLE ( 'NONE', #21903, 0.5019685039370077595 ) ;
#2724 = CONICAL_SURFACE ( 'NONE', #18814, 0.2114570894355444486, 1.221730476396037490 ) ;
#2725 = ORIENTED_EDGE ( 'NONE', *, *, #23101, .F. ) ;
#2726 = DIRECTION ( 'NONE',  ( 0.000000000000000000, 0.2126700594527845267, -0.9771240687918546497 ) ) ;
#2727 = FACE_OUTER_BOUND ( 'NONE', #31753, .T. ) ;
#2728 = ( BOUNDED_CURVE ( )  B_SPLINE_CURVE ( 2, ( #8770, #42047, #33969 ),
 .UNSPECIFIED., .F., .T. ) 
 B_SPLINE_CURVE_WITH_KNOTS ( ( 3, 3 ),
 ( 0.1350000000000000089, 0.1355626965693000063 ),
 .UNSPECIFIED. ) 
 CURVE ( )  GEOMETRIC_REPRESENTATION_ITEM ( )  RATIONAL_B_SPLINE_CURVE ( ( 1.000000000000000000, 0.9828669096362359081, 0.9734464042078300183 ) ) 
 REPRESENTATION_ITEM ( '' )  ) ;
#2729 = CARTESIAN_POINT ( 'NONE',  ( 0.8107537697050253289, 0.1574803149606300301, 1.911909448818899238 ) ) ;
#2730 = ORIENTED_EDGE ( 'NONE', *, *, #11013, .T. ) ;
#2731 = CARTESIAN_POINT ( 'NONE',  ( -1.054774247047244540, 0.07405724077823318263, 0.3051181101824569919 ) ) ;
#2732 = CARTESIAN_POINT ( 'NONE',  ( -1.100456976456230270E-17, -1.310083179661785335, -0.1797182628040039365 ) ) ;
#2733 = DIRECTION ( 'NONE',  ( 1.000000000000000000, 0.000000000000000000, 0.000000000000000000 ) ) ;
#2734 = CARTESIAN_POINT ( 'NONE',  ( 0.8019270111902716547, 0.1787899950787401604, 1.491141732229701145 ) ) ;
#2735 = AXIS2_PLACEMENT_3D ( 'NONE', #15622, #15860, #22308 ) ;
#2736 = CARTESIAN_POINT ( 'NONE',  ( -0.8107537697050254399, 0.1574803149606300301, 1.911909448818897017 ) ) ;
#2737 = ADVANCED_FACE ( 'NONE', ( #13849 ), #7740, .F. ) ;
#2739 = CARTESIAN_POINT ( 'NONE',  ( 0.9873396505805591694, 0.1113553986120547346, 1.707677165354330562 ) ) ;
#2738 = CARTESIAN_POINT ( 'NONE',  ( 0.1555216598441131470, -0.02857485583077736674, 0.1377952755905512416 ) ) ;
#2740 = DIRECTION ( 'NONE',  ( 0.000000000000000000, -1.000000000000000000, 0.000000000000000000 ) ) ;
#2741 = CARTESIAN_POINT ( 'NONE',  ( -0.9412147342319837628, -0.1574803149606297803, 1.685531495955465697 ) ) ;
#2742 = CARTESIAN_POINT ( 'NONE',  ( 0.1264236179284866091, 0.02411417328210995956, -0.1264236179284866091 ) ) ;
#2744 = ( BOUNDED_CURVE ( )  B_SPLINE_CURVE ( 2, ( #47341, #3720, #40821, #3486, #43729, #15003, #29654, #18101, #33458 ),
 .UNSPECIFIED., .F., .T. ) 
 B_SPLINE_CURVE_WITH_KNOTS ( ( 3, 2, 2, 2, 3 ),
 ( 0.5300000000000000266, 0.5324999999999999734, 0.5350000000000000311, 0.5374999999999999778, 0.5400000000000000355 ),
 .UNSPECIFIED. ) 
 CURVE ( )  GEOMETRIC_REPRESENTATION_ITEM ( )  RATIONAL_B_SPLINE_CURVE ( ( 1.000000000000000000, 0.9238795325112869605, 1.000000000000000000, 0.9238795325112869605, 1.000000000000000000, 0.9238795325112869605, 1.000000000000000000, 0.9238795325112869605, 1.000000000000000000 ) ) 
 REPRESENTATION_ITEM ( '' )  ) ;
#2743 = CARTESIAN_POINT ( 'NONE',  ( 0.8759842519685039353, 0.1787899950787401882, 0.1894685038832444879 ) ) ;
#2745 = FACE_OUTER_BOUND ( 'NONE', #47152, .T. ) ;
#2746 = EDGE_CURVE ( 'NONE', #5495, #31112, #13627, .T. ) ;
#2748 = CARTESIAN_POINT ( 'NONE',  ( -0.8759842519685039353, 0.1574803149606299191, 1.948818897637795367 ) ) ;
#2747 = CARTESIAN_POINT ( 'NONE',  ( 0.8019270111902716547, 0.1787899950787401604, 1.176181102308441195 ) ) ;
#2749 = CARTESIAN_POINT ( 'NONE',  ( 0.6971942568897648851, -0.07405724077823297447, 1.978346456639149098 ) ) ;
#2750 = CARTESIAN_POINT ( 'NONE',  ( 0.7185039370078746268, -0.06523048226347956391, 0.5733267715460159675 ) ) ;
#2751 = ORIENTED_EDGE ( 'NONE', *, *, #19643, .T. ) ;
#2752 = CARTESIAN_POINT ( 'NONE',  ( 1.033464566929133799, 1.928577636452524610E-17, 4.498031496062992574 ) ) ;
#2753 = CARTESIAN_POINT ( 'NONE',  ( 1.024574034319794436, 0.06442505785855824618, 0.03937402314509768492 ) ) ;
#2754 = CIRCLE ( 'NONE', #29619, 0.1574803149606299191 ) ;
#2755 = CARTESIAN_POINT ( 'NONE',  ( 0.1574803149606299191, -1.021653543199559033, -1.928577636452523993E-17 ) ) ;
#2756 = CARTESIAN_POINT ( 'NONE',  ( -1.033464566929134687, -0.06523048226347956391, 0.3518700786326304231 ) ) ;
#2757 = VERTEX_POINT ( 'NONE', #40689 ) ;
#2758 = CARTESIAN_POINT ( 'NONE',  ( 0.8759842519685039353, -0.1787899950787401882, 1.429625984198204858 ) ) ;
#2759 = CARTESIAN_POINT ( 'NONE',  ( -0.7646288533564489232, -0.1113553986120547346, 1.766732283464566899 ) ) ;
#2760 = CARTESIAN_POINT ( 'NONE',  ( 0.07405724077823318263, -0.09153543301710270752, -0.1787899950787401604 ) ) ;
#2761 = ORIENTED_EDGE ( 'NONE', *, *, #28717, .F. ) ;
#2762 = CARTESIAN_POINT ( 'NONE',  ( 0.8107537697050254399, 0.1574803149606300301, 0.7308070866141727073 ) ) ;
#2763 = ORIENTED_EDGE ( 'NONE', *, *, #5694, .T. ) ;
#2764 = CARTESIAN_POINT ( 'NONE',  ( 0.1768440709656048937, 0.08559642391441268927, 0.1833320988895605352 ) ) ;
#2765 = LINE ( 'NONE', #46619, #44483 ) ;
#2766 = VERTEX_POINT ( 'NONE', #7882 ) ;
#2767 = CARTESIAN_POINT ( 'NONE',  ( 0.6971942568897626646, -0.07405724077823297447, 0.4035433070328508509 ) ) ;
#2768 = EDGE_LOOP ( 'NONE', ( #37512, #34957, #12199, #30879 ) ) ;
#2769 = CARTESIAN_POINT ( 'NONE',  ( -0.7495606340400177148, -0.1264236179284866091, 1.424704724355685181 ) ) ;
#2770 = CARTESIAN_POINT ( 'NONE',  ( -0.07405724077823318263, -1.705708661363559253, -0.1787899950787401604 ) ) ;
#2771 = CARTESIAN_POINT ( 'NONE',  ( -1.054774247047244096, 0.000000000000000000, 0.9325787401037164415 ) ) ;
#2772 = CARTESIAN_POINT ( 'NONE',  ( -1.002407869896990045, -0.1264236179284866091, 1.985728346402929168 ) ) ;
#2773 = ORIENTED_EDGE ( 'NONE', *, *, #9440, .F. ) ;
#2774 = CARTESIAN_POINT ( 'NONE',  ( -0.8019270111902716547, 0.1787899950787401604, 1.018700787347811110 ) ) ;
#2775 = CARTESIAN_POINT ( 'NONE',  ( -1.054774247047244096, 0.000000000000000000, 0.6176181101824566033 ) ) ;
#2776 = CARTESIAN_POINT ( 'NONE',  ( 0.002798995768878668067, 0.03701427616989226566, -0.1377952292137403223 ) ) ;
#2777 = CARTESIAN_POINT ( 'NONE',  ( 0.1787899950787401604, -0.6684310548434121424, 0.07405724077823318263 ) ) ;
#2778 = ORIENTED_EDGE ( 'NONE', *, *, #18356, .F. ) ;
#2779 = CARTESIAN_POINT ( 'NONE',  ( -0.7646288533564489232, 0.1113553986120547346, 0.06397637795275590289 ) ) ;
#2780 = VERTEX_POINT ( 'NONE', #27079 ) ;
#2781 = CARTESIAN_POINT ( 'NONE',  ( -0.7646288533564489232, -0.1113553986120547346, 0.3395669290263311213 ) ) ;
#2782 = DIRECTION ( 'NONE',  ( 1.822029033848725028E-16, 0.000000000000000000, 1.000000000000000000 ) ) ;
#2783 = EDGE_CURVE ( 'NONE', #41019, #860, #45985, .T. ) ;
#2784 = CARTESIAN_POINT ( 'NONE',  ( -0.9500414927467378812, -0.1787899950787401604, 0.6840551180564720113 ) ) ;
#2785 = LINE ( 'NONE', #46171, #32247 ) ;
#2786 = ORIENTED_EDGE ( 'NONE', *, *, #1840, .F. ) ;
#2787 = CARTESIAN_POINT ( 'NONE',  ( -0.8759842519685039353, -0.1787899950787401882, 1.592027559001354398 ) ) ;
#2788 = DIRECTION ( 'NONE',  ( 0.000000000000000000, 0.000000000000000000, 1.000000000000000000 ) ) ;
#2789 = CARTESIAN_POINT ( 'NONE',  ( -1.033464566929134687, 0.06523048226347956391, 0.4847440944881890590 ) ) ;
#2790 = ORIENTED_EDGE ( 'NONE', *, *, #43590, .F. ) ;
#2791 = CARTESIAN_POINT ( 'NONE',  ( 0.1270800023317771588, -0.8917760930476122949, 0.1270800023317771588 ) ) ;
#2792 = CARTESIAN_POINT ( 'NONE',  ( 0.7646288533564489232, 0.1113553986120547346, 0.6446850392625511628 ) ) ;
#2793 = CARTESIAN_POINT ( 'NONE',  ( -1.033464566929134687, -0.06523048226347956391, 1.414862204616882835 ) ) ;
#2794 = EDGE_CURVE ( 'NONE', #2574, #26779, #4956, .T. ) ;
#2795 = CARTESIAN_POINT ( 'NONE',  ( 0.1574803149606300301, -0.6353346456692916533, -0.06523048226347956391 ) ) ;
#2796 = DIRECTION ( 'NONE',  ( 0.000000000000000000, 0.000000000000000000, -1.000000000000000000 ) ) ;
#2797 = CARTESIAN_POINT ( 'NONE',  ( 0.7646288533564489232, -0.1113553986120547346, 1.294291338582677309 ) ) ;
#2799 = CARTESIAN_POINT ( 'NONE',  ( -0.1574803149606299191, 0.000000000000000000, -0.1966003937007873570 ) ) ;
#2798 = CARTESIAN_POINT ( 'NONE',  ( -1.033464566929133799, 1.928577636452524610E-17, 2.869337061179095023E-17 ) ) ;
#2800 = CARTESIAN_POINT ( 'NONE',  ( 0.9873396505805591694, -0.1113553986120547346, 1.973425196850393970 ) ) ;
#2801 = CARTESIAN_POINT ( 'NONE',  ( 0.1113553986120547346, -0.6230314959554646981, -0.1113553986120547346 ) ) ;
#2802 = EDGE_CURVE ( 'NONE', #8667, #32919, #11851, .T. ) ;
#2804 = CARTESIAN_POINT ( 'NONE',  ( -0.6195511811023656223, 0.4133858267716533086, 0.9891732283464566011 ) ) ;
#2803 = CARTESIAN_POINT ( 'NONE',  ( 1.054774247047244540, -0.07405724077823318263, 0.6889763778989936860 ) ) ;
#2805 = FACE_OUTER_BOUND ( 'NONE', #13667, .T. ) ;
#2806 = DIRECTION ( 'NONE',  ( 0.000000000000000000, -0.7880107536067206819, 0.6156614753256598460 ) ) ;
#2807 = ORIENTED_EDGE ( 'NONE', *, *, #4460, .F. ) ;
#2808 = CARTESIAN_POINT ( 'NONE',  ( 0.000000000000000000, 0.000000000000000000, 0.09842519685039370636 ) ) ;
#2809 = CARTESIAN_POINT ( 'NONE',  ( 1.033464566929133799, 0.000000000000000000, 1.742125984251968518 ) ) ;
#2810 = CARTESIAN_POINT ( 'NONE',  ( 0.1571288672381035423, 0.02360035419903267623, -0.1403980133540707609 ) ) ;
#2811 = CARTESIAN_POINT ( 'NONE',  ( 0.9500414927467378812, 0.1787899950787401604, 0.8956692912848198684 ) ) ;
#2812 = CARTESIAN_POINT ( 'NONE',  ( 1.033464566929133799, 0.000000000000000000, 1.466535433070866201 ) ) ;
#2813 = DIRECTION ( 'NONE',  ( 0.000000000000000000, 1.000000000000000000, 0.000000000000000000 ) ) ;
#2814 = CARTESIAN_POINT ( 'NONE',  ( 0.1797182628040039087, 0.1392278439602615547, -0.07444174185955065859 ) ) ;
#2815 = CARTESIAN_POINT ( 'NONE',  ( -1.094772975963752103E-17, -1.038877952702141672, -0.1787899950787401882 ) ) ;
#2816 = CARTESIAN_POINT ( 'NONE',  ( 0.06523048226347956391, -1.511318897637796255, 0.1574803149606297803 ) ) ;
#2817 = FACE_OUTER_BOUND ( 'NONE', #42425, .T. ) ;
#2818 = CARTESIAN_POINT ( 'NONE',  ( -0.8759842519685039353, 0.1787899950787401882, 1.966043307032850462 ) ) ;
#2819 = CARTESIAN_POINT ( 'NONE',  ( 0.9500414927467378812, 0.1787899950787401604, 1.924212598371433325 ) ) ;
#2820 = VERTEX_POINT ( 'NONE', #24403 ) ;
#2821 = CARTESIAN_POINT ( 'NONE',  ( 0.1113553986120547346, -1.410433070758614127, -0.1113553986120547346 ) ) ;
#2822 = CARTESIAN_POINT ( 'NONE',  ( -1.002407869896990045, 0.1264236179284866091, 1.882381889710015743 ) ) ;
#2823 = CARTESIAN_POINT ( 'NONE',  ( -0.6971942568897637749, 2.189545951927499583E-17, 1.577263779473795369 ) ) ;
#2824 = CARTESIAN_POINT ( 'NONE',  ( -0.8759842519685039353, -0.1787899950787401882, 0.2534448818360003908 ) ) ;
#2825 = DIRECTION ( 'NONE',  ( 0.000000000000000000, 0.000000000000000000, -1.000000000000000000 ) ) ;
#2826 = CARTESIAN_POINT ( 'NONE',  ( -1.002407869896990045, -0.1264236179284866091, 1.951279527505291433 ) ) ;
#2827 = CARTESIAN_POINT ( 'NONE',  ( -1.054774247047244096, 0.000000000000000000, 0.1451771653005673179 ) ) ;
#2828 = CARTESIAN_POINT ( 'NONE',  ( -0.9412147342319837628, 0.1574803149606300301, 1.867618110236221707 ) ) ;
#2829 = CARTESIAN_POINT ( 'NONE',  ( 0.2559055051320487939, 0.04218512718539534079, -0.03480397727850505912 ) ) ;
#2830 = CARTESIAN_POINT ( 'NONE',  ( -0.1787899950787401604, -0.2156751493316009516, -0.07405724077823318263 ) ) ;
#2831 = CARTESIAN_POINT ( 'NONE',  ( 0.1126279540338996077, -0.5708661417322835607, 1.206847064312610129 ) ) ;
#2832 = CARTESIAN_POINT ( 'NONE',  ( 0.8759842519685039353, 0.000000000000000000, 4.498031496062992574 ) ) ;
#2833 = CARTESIAN_POINT ( 'NONE',  ( -0.8759842519685039353, -0.1787899950787401882, 0.1304133857730082613 ) ) ;
#2834 = EDGE_LOOP ( 'NONE', ( #20225, #46223, #10055, #19298 ) ) ;
#2835 = CARTESIAN_POINT ( 'NONE',  ( -0.9500414927467377701, -0.1787899950787401604, 1.279527559001355730 ) ) ;
#2836 = ORIENTED_EDGE ( 'NONE', *, *, #3131, .F. ) ;
#2837 = EDGE_CURVE ( 'NONE', #24150, #15113, #31611, .T. ) ;
#2838 = CARTESIAN_POINT ( 'NONE',  ( 0.07405724077823318263, -1.213582677111591623, 0.1787899950787401604 ) ) ;
#2839 = CARTESIAN_POINT ( 'NONE',  ( 0.1787899950787401604, -1.435039370024976391, -0.07405724077823318263 ) ) ;
#2840 = DIRECTION ( 'NONE',  ( 1.734723475976806897E-15, -0.6156614753256597350, -0.7880107536067207930 ) ) ;
#2841 = ( NAMED_UNIT ( * ) SI_UNIT ( $, .STERADIAN. ) SOLID_ANGLE_UNIT ( ) ) ;
#2842 = CARTESIAN_POINT ( 'NONE',  ( -0.1797182628040039365, -0.4340989276932818997, 0.000000000000000000 ) ) ;
#2843 = CARTESIAN_POINT ( 'NONE',  ( -0.8759842519685039353, 0.000000000000000000, 0.03937007874015843040 ) ) ;
#2844 = CARTESIAN_POINT ( 'NONE',  ( -0.8759842519685039353, 0.1574803149606299191, 0.7283464566929134243 ) ) ;
#2845 = EDGE_CURVE ( 'NONE', #17977, #39669, #20793, .T. ) ;
#2846 = CARTESIAN_POINT ( 'NONE',  ( 0.7185039370078739607, 1.928577636452523993E-17, 1.791338582569637738 ) ) ;
#2847 = ORIENTED_EDGE ( 'NONE', *, *, #23390, .T. ) ;
#2848 = CARTESIAN_POINT ( 'NONE',  ( 0.7646288533564489232, 0.1113553986120547346, 0.7332677165354331006 ) ) ;
#2849 = CARTESIAN_POINT ( 'NONE',  ( 0.09240388072374286499, -0.2421448268523899161, -0.03441347972012361728 ) ) ;
#2850 = CARTESIAN_POINT ( 'NONE',  ( -1.033464566929133799, 0.000000000000000000, 1.614173228238929170 ) ) ;
#2851 = ( BOUNDED_CURVE ( )  B_SPLINE_CURVE ( 2, ( #38158, #30306, #27652, #42208, #1251, #38633, #19938, #8685, #37934 ),
 .UNSPECIFIED., .F., .T. ) 
 B_SPLINE_CURVE_WITH_KNOTS ( ( 3, 2, 2, 2, 3 ),
 ( 0.02999999999999999889, 0.03250000000000000111, 0.03500000000000000333, 0.03749999999999999861, 0.04000000000000000083 ),
 .UNSPECIFIED. ) 
 CURVE ( )  GEOMETRIC_REPRESENTATION_ITEM ( )  RATIONAL_B_SPLINE_CURVE ( ( 1.000000000000000000, 0.9238795325112869605, 1.000000000000000000, 0.9238795325112869605, 1.000000000000000000, 0.9238795325112869605, 1.000000000000000000, 0.9238795325112869605, 1.000000000000000000 ) ) 
 REPRESENTATION_ITEM ( '' )  ) ;
#2853 = CARTESIAN_POINT ( 'NONE',  ( 0.1577586585109236050, -0.1055041328676506324, -0.09810528961776883439 ) ) ;
#2852 = DIRECTION ( 'NONE',  ( 0.000000000000000000, 0.000000000000000000, -1.000000000000000000 ) ) ;
#2854 = CARTESIAN_POINT ( 'NONE',  ( 0.8759842519685039353, -0.1574803149606299191, 0.1082677164279060994 ) ) ;
#2855 = VERTEX_POINT ( 'NONE', #30338 ) ;
#2856 = ORIENTED_EDGE ( 'NONE', *, *, #40837, .F. ) ;
#2857 = CYLINDRICAL_SURFACE ( 'NONE', #40098, 0.1574803149606299191 ) ;
#2858 = CARTESIAN_POINT ( 'NONE',  ( -0.7661220286720177297, 0.1429759811008071424, 0.03937007874015843040 ) ) ;
#2859 = CARTESIAN_POINT ( 'NONE',  ( -0.1264236179284866091, -0.5123031495525355306, 0.1264236179284866091 ) ) ;
#2861 = AXIS2_PLACEMENT_3D ( 'NONE', #24245, #6007, #6478 ) ;
#2860 = CARTESIAN_POINT ( 'NONE',  ( 0.1574803149606299191, -1.110236220472440971, -1.928577636452523993E-17 ) ) ;
#2862 = CARTESIAN_POINT ( 'NONE',  ( 0.8107537697050253289, 0.1574803149606300301, 0.8784448817822366751 ) ) ;
#2863 = CARTESIAN_POINT ( 'NONE',  ( 1.033464566929134687, 0.06523048226347956391, 0.5241141732283461918 ) ) ;
#2864 = CARTESIAN_POINT ( 'NONE',  ( -0.6971942568897626646, -0.07405724077823297447, 0.3986220471903312301 ) ) ;
#2865 = ORIENTED_EDGE ( 'NONE', *, *, #33136, .F. ) ;
#2866 = ORIENTED_EDGE ( 'NONE', *, *, #24415, .F. ) ;
#2867 = VERTEX_POINT ( 'NONE', #44643 ) ;
#2868 = CARTESIAN_POINT ( 'NONE',  ( -0.8759842519685039353, -0.1787899950787401882, 1.473917322780881722 ) ) ;
#2869 = CARTESIAN_POINT ( 'NONE',  ( 0.8759842519685039353, 0.1787899950787401882, 1.572342519631275692 ) ) ;
#2870 = VERTEX_POINT ( 'NONE', #40346 ) ;
#2871 = CARTESIAN_POINT ( 'NONE',  ( 0.9873396505805591694, -0.1113553986120547346, 0.9399606298137322957 ) ) ;
#2872 = CARTESIAN_POINT ( 'NONE',  ( -1.054774247047244540, 0.07405724077823318263, 0.6200787401037165525 ) ) ;
#2873 = LINE ( 'NONE', #39303, #35054 ) ;
#2874 = CARTESIAN_POINT ( 'NONE',  ( 0.8019270111902716547, 0.1787899950787401604, 0.7480314960092282472 ) ) ;
#2875 = DIRECTION ( 'NONE',  ( -1.000000000000000000, 0.000000000000000000, 0.000000000000000000 ) ) ;
#2876 = CARTESIAN_POINT ( 'NONE',  ( 0.8759842519685039353, 0.1574803149606299191, 1.072834645561763889 ) ) ;
#2877 = CARTESIAN_POINT ( 'NONE',  ( 0.1574803149606300301, -0.1973425195775124208, 0.06523048226347956391 ) ) ;
#2878 = CARTESIAN_POINT ( 'NONE',  ( -0.9500414927467378812, -0.1787899950787401604, 1.397637795221827295 ) ) ;
#2879 = DIRECTION ( 'NONE',  ( 1.822029033848725028E-16, 0.000000000000000000, 1.000000000000000000 ) ) ;
#2880 = CARTESIAN_POINT ( 'NONE',  ( -0.8107537697050253289, 0.1574803149606300301, 0.4945866141732282451 ) ) ;
#2881 = CARTESIAN_POINT ( 'NONE',  ( 0.8759842519685039353, -0.1787899950787401882, 1.355807086560409491 ) ) ;
#2882 = CARTESIAN_POINT ( 'NONE',  ( -0.03000208359710393805, -0.09851384112419016292, -0.1860997263723594419 ) ) ;
#2883 = ORIENTED_EDGE ( 'NONE', *, *, #45099, .T. ) ;
#2884 = CARTESIAN_POINT ( 'NONE',  ( -0.9412147342319837628, -0.1574803149606297803, 0.5536417322834641386 ) ) ;
#2885 = VECTOR ( 'NONE', #9072, 39.37007874015748143 ) ;
#2886 = ORIENTED_EDGE ( 'NONE', *, *, #14250, .T. ) ;
#2887 = CARTESIAN_POINT ( 'NONE',  ( 0.8107537697050254399, -0.1574803149606297803, 0.3912401574803148208 ) ) ;
#2888 = VERTEX_POINT ( 'NONE', #25999 ) ;
#2889 = CARTESIAN_POINT ( 'NONE',  ( 0.8019270111902717657, 0.1787899950787401604, 1.451771653489543290 ) ) ;
#2890 = ADVANCED_FACE ( 'NONE', ( #15702 ), #1045, .T. ) ;
#2891 = LINE ( 'NONE', #17768, #16244 ) ;
#2892 = VECTOR ( 'NONE', #27863, 39.37007874015748143 ) ;
#2893 = CARTESIAN_POINT ( 'NONE',  ( 0.1787899950787401604, -0.2982283464029296116, -0.07405724077823318263 ) ) ;
#2894 = EDGE_CURVE ( 'NONE', #41647, #34447, #13153, .T. ) ;
#2895 = CARTESIAN_POINT ( 'NONE',  ( 0.1264236179284866091, -0.7239173227808818334, -0.1264236179284866091 ) ) ;
#2896 = CARTESIAN_POINT ( 'NONE',  ( 0.5555748031496123840, 1.332209862199691397, -0.06082000038405670217 ) ) ;
#2897 = CARTESIAN_POINT ( 'NONE',  ( 0.000000000000000000, -0.09842519685039370636, 0.1574803149606299191 ) ) ;
#2898 = CARTESIAN_POINT ( 'NONE',  ( 0.8019270111902717657, -0.1787899950787401604, 0.2854330708123783422 ) ) ;
#2899 = EDGE_CURVE ( 'NONE', #33124, #34176, #36831, .T. ) ;
#2900 = CARTESIAN_POINT ( 'NONE',  ( -1.094772975963752103E-17, 0.05253351208572189235, -0.1787899950787401882 ) ) ;
#2901 = CARTESIAN_POINT ( 'NONE',  ( 0.1787899950787401604, -0.2539370078202523584, -0.07405724077823318263 ) ) ;
#2902 = CARTESIAN_POINT ( 'NONE',  ( 0.1787899950787401604, 0.09547244099864542199, -0.07405724077823318263 ) ) ;
#2903 = DIRECTION ( 'NONE',  ( 1.822029033848725028E-16, 0.000000000000000000, 1.000000000000000000 ) ) ;
#2904 = DIRECTION ( 'NONE',  ( -0.5735764363510518216, 0.8191520442889876907, 1.003171929053519693E-16 ) ) ;
#2905 = EDGE_CURVE ( 'NONE', #13605, #29883, #29414, .T. ) ;
#2906 = CARTESIAN_POINT ( 'NONE',  ( 0.6971942568897637749, 2.189545951927499583E-17, 0.5536417322297008115 ) ) ;
#2907 = CARTESIAN_POINT ( 'NONE',  ( -0.7495606340400177148, 0.1264236179284866091, 1.026082677111590513 ) ) ;
#2909 = CARTESIAN_POINT ( 'NONE',  ( 1.033464566929133799, 1.928577636452524610E-17, 4.498031496062992574 ) ) ;
#2908 = CARTESIAN_POINT ( 'NONE',  ( 0.1574803149606299191, -0.8740157480314961758, -1.928577636452523993E-17 ) ) ;
#2911 = CARTESIAN_POINT ( 'NONE',  ( -0.8817724199485534875, -0.1746201713974357972, 1.988283497529828914 ) ) ;
#2910 = CARTESIAN_POINT ( 'NONE',  ( 0.07444174185955046430, -1.745614675724777021, -0.1797182628040039087 ) ) ;
#2912 = CARTESIAN_POINT ( 'NONE',  ( -0.8759842519685039353, 0.000000000000000000, 1.990649606245448844 ) ) ;
#2913 = CARTESIAN_POINT ( 'NONE',  ( 0.6971942568897637749, 2.189545951927499583E-17, 1.660925196796630088 ) ) ;
#2915 = CARTESIAN_POINT ( 'NONE',  ( 0.1574803149606300023, 0.7443365962042343131, -3.523993443072799270 ) ) ;
#2914 = PLANE ( 'NONE',  #36780 ) ;
#2916 = ORIENTED_EDGE ( 'NONE', *, *, #24893, .F. ) ;
#2917 = CARTESIAN_POINT ( 'NONE',  ( 0.4151545546392377273, 4.766607801171850497E-17, 0.000000000000000000 ) ) ;
#2918 = CARTESIAN_POINT ( 'NONE',  ( 0.3161444924769535869, 1.690605217543005745, -0.5092277576975102749 ) ) ;
#2920 = CARTESIAN_POINT ( 'NONE',  ( -1.094772975963752103E-17, -0.09399606293836239301, -0.1787899950787401882 ) ) ;
#2919 = CARTESIAN_POINT ( 'NONE',  ( 0.1113553986120547346, -0.9084645668216063674, 0.1113553986120547346 ) ) ;
#2921 = CARTESIAN_POINT ( 'NONE',  ( 0.8019270111902717657, -0.1787899950787401604, 0.6003937007336380693 ) ) ;
#2922 = CARTESIAN_POINT ( 'NONE',  ( -0.1787899950787401604, -0.9035433070328510174, 0.07405724077823318263 ) ) ;
#2923 = CARTESIAN_POINT ( 'NONE',  ( 0.8759842519685039353, -0.1787899950787401882, 0.05659448813521291560 ) ) ;
#2924 = CARTESIAN_POINT ( 'NONE',  ( 0.6971942568897648851, 0.07405724077823318263, 0.5511811023084406402 ) ) ;
#2925 = ORIENTED_EDGE ( 'NONE', *, *, #8325, .F. ) ;
#2926 = CARTESIAN_POINT ( 'NONE',  ( -0.2617501178043720178, -0.1661865978653772336, -0.8983733778024277639 ) ) ;
#2927 = CARTESIAN_POINT ( 'NONE',  ( 0.7495606340400177148, 0.1264236179284866091, 1.104822834591905556 ) ) ;
#2928 = CARTESIAN_POINT ( 'NONE',  ( -0.1113553986120547346, -1.164370078632629868, -0.1113553986120547346 ) ) ;
#2929 = CARTESIAN_POINT ( 'NONE',  ( -1.033464566929134687, 0.06523048226347956391, 0.7111220471365681250 ) ) ;
#2930 = CARTESIAN_POINT ( 'NONE',  ( 0.8019270111902717657, -0.1787899950787401604, 1.781496062938362934 ) ) ;
#2931 = CARTESIAN_POINT ( 'NONE',  ( -0.9412147342319837628, -0.1574803149606297803, 1.341043307086615455 ) ) ;
#2932 = CARTESIAN_POINT ( 'NONE',  ( -1.002407869896990045, -0.1264236179284866091, 0.8439960629383622681 ) ) ;
#2933 = LINE ( 'NONE', #17570, #8261 ) ;
#2934 = CARTESIAN_POINT ( 'NONE',  ( -0.7046433452555540544, -0.02693604437337100005, 0.03937007874015843040 ) ) ;
#2935 = CARTESIAN_POINT ( 'NONE',  ( 0.9500414927467377701, -0.1787899950787401604, 0.3740157479777325711 ) ) ;
#2936 = UNCERTAINTY_MEASURE_WITH_UNIT (LENGTH_MEASURE( 1.000000000000000082E-05 ), #19423, 'distance_accuracy_value', 'NONE') ;
#2937 = CARTESIAN_POINT ( 'NONE',  ( -0.8019270111902717657, 0.1787899950787401604, 0.5462598424659214080 ) ) ;
#2938 = CARTESIAN_POINT ( 'NONE',  ( 0.9412147342319837628, -0.1574803149606297803, 1.528051180994836056 ) ) ;
#2939 = ORIENTED_EDGE ( 'NONE', *, *, #6637, .T. ) ;
#2940 = VECTOR ( 'NONE', #17933, 39.37007874015748143 ) ;
#2941 = CARTESIAN_POINT ( 'NONE',  ( 0.07405724077823318263, -0.07185039364702389131, 0.1787899950787401604 ) ) ;
#2942 = CARTESIAN_POINT ( 'NONE',  ( 0.2001839496640331895, -0.1799179750364369168, -0.05578523004296986193 ) ) ;
#2943 = EDGE_LOOP ( 'NONE', ( #18676, #32852, #16050, #18806 ) ) ;
#2944 = EDGE_LOOP ( 'NONE', ( #31065, #44061, #24696, #6082 ) ) ;
#2945 = CARTESIAN_POINT ( 'NONE',  ( 0.6971942568897637749, 2.189545951927499583E-17, 0.8341535432533228045 ) ) ;
#2946 = CARTESIAN_POINT ( 'NONE',  ( -1.002407869896990045, 0.1264236179284866091, 1.719980314906866203 ) ) ;
#2947 = CARTESIAN_POINT ( 'NONE',  ( 0.07405724077823318263, -1.484251968450174930, 0.1787899950787401604 ) ) ;
#2948 = CARTESIAN_POINT ( 'NONE',  ( -0.7646288533564489232, 0.1113553986120547346, 0.6545275590551181688 ) ) ;
#2949 = DIRECTION ( 'NONE',  ( -0.000000000000000000, 1.000000000000000000, -0.000000000000000000 ) ) ;
#2950 = CARTESIAN_POINT ( 'NONE',  ( 0.07405724077823318263, -1.249139716260735611, -0.1787899950787401604 ) ) ;
#2951 = VERTEX_POINT ( 'NONE', #7536 ) ;
#2952 = CARTESIAN_POINT ( 'NONE',  ( -0.1787899950787401604, -0.07677165348954355373, 0.07405724077823318263 ) ) ;
#2953 = VERTEX_POINT ( 'NONE', #22870 ) ;
#2954 = CARTESIAN_POINT ( 'NONE',  ( 0.8019270111902717657, 0.1787899950787401604, 1.097440944828127041 ) ) ;
#2955 = LINE ( 'NONE', #43213, #5714 ) ;
#2956 = CARTESIAN_POINT ( 'NONE',  ( -0.9412147342319837628, 0.1574803149606300301, 0.9916338581601894520 ) ) ;
#2957 = EDGE_CURVE ( 'NONE', #4869, #17741, #22386, .T. ) ;
#2958 = CIRCLE ( 'NONE', #35153, 0.01968503937007875723 ) ;
#2959 = CARTESIAN_POINT ( 'NONE',  ( 0.9500414927467378812, -0.1787899950787401604, 0.05413385821395302888 ) ) ;
#2960 = VECTOR ( 'NONE', #34906, 39.37007874015748854 ) ;
#2961 = CARTESIAN_POINT ( 'NONE',  ( -0.1787899950787401604, -1.499015747977732627, 0.07405724077823318263 ) ) ;
#2962 = CARTESIAN_POINT ( 'NONE',  ( 3.284318927891251994E-17, -0.7436023621509606496, 0.1787899950787401882 ) ) ;
#2963 = EDGE_CURVE ( 'NONE', #28992, #31452, #45863, .T. ) ;
#2964 = CARTESIAN_POINT ( 'NONE',  ( -1.054774247047244096, 0.000000000000000000, 0.3813976377415121966 ) ) ;
#2965 = CARTESIAN_POINT ( 'NONE',  ( 0.1270800023317771588, -1.315004439504305012, -0.1270800023317771588 ) ) ;
#2966 = CARTESIAN_POINT ( 'NONE',  ( -0.09162190804155563584, 0.2425962989909478396, -0.03472289316813708532 ) ) ;
#2967 = CARTESIAN_POINT ( 'NONE',  ( 0.8759842519685039353, -0.1787899950787401882, 1.237696850339937038 ) ) ;
#2968 = VECTOR ( 'NONE', #28083, 39.37007874015748143 ) ;
#2969 = CARTESIAN_POINT ( 'NONE',  ( 0.9500414927467377701, 0.1787899950787401604, 1.525590551127339989 ) ) ;
#2970 = CARTESIAN_POINT ( 'NONE',  ( 0.6971942568897626646, 0.07405724077823318263, 0.1968503936470238636 ) ) ;
#2971 = LINE ( 'NONE', #28177, #16210 ) ;
#2972 = CARTESIAN_POINT ( 'NONE',  ( 1.033464566929134687, 0.06523048226347956391, 1.705216535433070613 ) ) ;
#2973 = CARTESIAN_POINT ( 'NONE',  ( 0.1564639344508098606, -0.02850229122252114292, 0.1403868508442179253 ) ) ;
#2974 = CARTESIAN_POINT ( 'NONE',  ( 0.8759842519685039353, -0.1574803149606299191, 1.446850393593259732 ) ) ;
#2975 = CARTESIAN_POINT ( 'NONE',  ( 0.7185039370078746268, -0.06523048226347956391, 0.7701771652468031304 ) ) ;
#2976 = CARTESIAN_POINT ( 'NONE',  ( -0.7185039370078739607, 1.928577636452523993E-17, 1.751968503829480106 ) ) ;
#2977 = CARTESIAN_POINT ( 'NONE',  ( -0.1264236179284866091, -0.005413385773008149403, -0.1264236179284866091 ) ) ;
#2978 = CARTESIAN_POINT ( 'NONE',  ( 0.6971942568897626646, 0.07405724077823318263, 0.1968503936470238913 ) ) ;
#2979 = CARTESIAN_POINT ( 'NONE',  ( 0.7033435294390766312, 0.03857964621150825751, 0.03937085465571968368 ) ) ;
#2981 = CARTESIAN_POINT ( 'NONE',  ( -0.9873396505805591694, 0.1113553986120547346, 1.815944881782236120 ) ) ;
#2980 = CARTESIAN_POINT ( 'NONE',  ( 1.002407869896990045, 0.1264236179284866091, 1.168799212544661348 ) ) ;
#2982 = CARTESIAN_POINT ( 'NONE',  ( -0.7185039370078739607, 1.928577636452523993E-17, 1.368110236220472675 ) ) ;
#2983 = CARTESIAN_POINT ( 'NONE',  ( 0.7646288533564489232, -0.1113553986120547346, 0.4970472439869613734 ) ) ;
#2984 = EDGE_LOOP ( 'NONE', ( #4268, #8274, #16882, #28951, #15427, #2790, #46729, #33220 ) ) ;
#2985 = CARTESIAN_POINT ( 'NONE',  ( -1.002407869896990045, -0.1264236179284866091, 1.045767716481669440 ) ) ;
#2986 = DIRECTION ( 'NONE',  ( 1.822029033848725028E-16, 0.000000000000000000, 1.000000000000000000 ) ) ;
#2987 = CARTESIAN_POINT ( 'NONE',  ( 0.9662619894878454740, 0.1420933317043502342, 0.03937004641417764239 ) ) ;
#2988 = CARTESIAN_POINT ( 'NONE',  ( -1.033464566929133799, 0.000000000000000000, 0.3543307085538902057 ) ) ;
#2989 = EDGE_LOOP ( 'NONE', ( #22664, #46106, #42101, #21732 ) ) ;
#2990 = CARTESIAN_POINT ( 'NONE',  ( 1.054774247047244096, 0.000000000000000000, 1.518208661363559031 ) ) ;
#2991 = CYLINDRICAL_SURFACE ( 'NONE', #16263, 0.1574803149606299191 ) ;
#2992 = CARTESIAN_POINT ( 'NONE',  ( -0.1787899950787401604, -0.002952755851748307785, -0.07405724077823318263 ) ) ;
#2993 = EDGE_LOOP ( 'NONE', ( #6858, #21214, #41669, #27403 ) ) ;
#2994 = DIRECTION ( 'NONE',  ( 1.000000000000000000, 0.000000000000000000, -1.822029033848725275E-16 ) ) ;
#2995 = VECTOR ( 'NONE', #35727, 39.37007874015748143 ) ;
#2996 = ORIENTED_EDGE ( 'NONE', *, *, #28580, .T. ) ;
#2997 = CARTESIAN_POINT ( 'NONE',  ( 0.1594274916601849112, 0.09247100924358107876, 0.1933875656399073328 ) ) ;
#2998 = DIRECTION ( 'NONE',  ( 1.000000000000000000, 0.000000000000000000, 0.000000000000000000 ) ) ;
#2999 = CARTESIAN_POINT ( 'NONE',  ( 0.9500414927467378812, 0.1787899950787401604, 0.5462598424659214080 ) ) ;
#3000 = ORIENTED_EDGE ( 'NONE', *, *, #13330, .F. ) ;
#3001 = CARTESIAN_POINT ( 'NONE',  ( -0.6971942568897637749, 2.189545951927499583E-17, 1.341043307032850462 ) ) ;
#3002 = CARTESIAN_POINT ( 'NONE',  ( -0.1787899950787401882, -1.658956692859621995, 0.000000000000000000 ) ) ;
#3003 = CARTESIAN_POINT ( 'NONE',  ( -0.6971942568897648851, 0.07405724077823318263, 1.186023621993481658 ) ) ;
#3004 = CARTESIAN_POINT ( 'NONE',  ( -1.002407869896990045, 0.1264236179284866091, 1.090059055064346527 ) ) ;
#3005 = CIRCLE ( 'NONE', #2230, 0.2362204724409449064 ) ;
#3006 = CARTESIAN_POINT ( 'NONE',  ( -0.9500414927467378812, -0.1787899950787401604, 0.7677165353793073965 ) ) ;
#3007 = ( BOUNDED_CURVE ( )  B_SPLINE_CURVE ( 2, ( #47135, #40159, #37052, #29453, #7115, #3525, #25815, #10736, #18835 ),
 .UNSPECIFIED., .F., .T. ) 
 B_SPLINE_CURVE_WITH_KNOTS ( ( 3, 2, 2, 2, 3 ),
 ( 0.1799999999999999933, 0.1824999999999999956, 0.1849999999999999978, 0.1875000000000000000, 0.1900000000000000022 ),
 .UNSPECIFIED. ) 
 CURVE ( )  GEOMETRIC_REPRESENTATION_ITEM ( )  RATIONAL_B_SPLINE_CURVE ( ( 1.000000000000000000, 0.9238795325112869605, 1.000000000000000000, 0.9238795325112869605, 1.000000000000000000, 0.9238795325112869605, 1.000000000000000000, 0.9238795325112869605, 1.000000000000000000 ) ) 
 REPRESENTATION_ITEM ( '' )  ) ;
#3008 = CARTESIAN_POINT ( 'NONE',  ( -1.054774247047244540, 0.07405724077823318263, 0.1476377952218269618 ) ) ;
#3009 = CARTESIAN_POINT ( 'NONE',  ( -0.9873396505805591694, -0.1113553986120547346, 0.3592519685039369803 ) ) ;
#3010 = CARTESIAN_POINT ( 'NONE',  ( 0.01036003557126029262, 0.07281034877059977539, -0.1377952755905511306 ) ) ;
#3011 = CARTESIAN_POINT ( 'NONE',  ( 0.07405724077823318263, -0.7766987713788455761, -0.1787899950787401604 ) ) ;
#3012 = VERTEX_POINT ( 'NONE', #33217 ) ;
#3013 = CARTESIAN_POINT ( 'NONE',  ( 0.1020804098320771541, -0.08956209254691890886, 0.1018622834461950927 ) ) ;
#3014 = ORIENTED_EDGE ( 'NONE', *, *, #14197, .T. ) ;
#3015 = CARTESIAN_POINT ( 'NONE',  ( 0.9412147342319837628, 0.1574803149606300301, 0.7652559055118115516 ) ) ;
#3016 = CARTESIAN_POINT ( 'NONE',  ( 0.4151545546392377273, 0.09842519685039370636, 0.000000000000000000 ) ) ;
#3017 = CARTESIAN_POINT ( 'NONE',  ( -0.7495606340400177148, -0.1264236179284866091, 0.5585629920722204877 ) ) ;
#3018 = EDGE_CURVE ( 'NONE', #40880, #7920, #44183, .T. ) ;
#3019 = VERTEX_POINT ( 'NONE', #18333 ) ;
#3020 = CARTESIAN_POINT ( 'NONE',  ( -0.7495606340400177148, 0.1264236179284866091, 1.734744094434425232 ) ) ;
#3021 = EDGE_CURVE ( 'NONE', #7776, #30501, #22148, .T. ) ;
#3022 = DIRECTION ( 'NONE',  ( 0.8191520442890009024, 0.4519843998600359125, -0.3531289150159101498 ) ) ;
#3023 = ( BOUNDED_CURVE ( )  B_SPLINE_CURVE ( 2, ( #15187, #37209, #37688, #18989, #12062, #29835, #8680, #26924, #761 ),
 .UNSPECIFIED., .F., .F. ) 
 B_SPLINE_CURVE_WITH_KNOTS ( ( 3, 2, 2, 2, 3 ),
 ( 0.1499999999999999944, 0.1524999999999999967, 0.1549999999999999989, 0.1575000000000000011, 0.1600000000000000033 ),
 .UNSPECIFIED. ) 
 CURVE ( )  GEOMETRIC_REPRESENTATION_ITEM ( )  RATIONAL_B_SPLINE_CURVE ( ( 1.000000000000000000, 0.9238795325112869605, 1.000000000000000000, 0.9238795325112869605, 1.000000000000000000, 0.9238795325112869605, 1.000000000000000000, 0.9238795325112869605, 1.000000000000000000 ) ) 
 REPRESENTATION_ITEM ( '' )  ) ;
#3024 = CIRCLE ( 'NONE', #723, 0.2559055118110236116 ) ;
#3025 = DIRECTION ( 'NONE',  ( 1.000000000000000000, 0.000000000000000000, -0.000000000000000000 ) ) ;
#3026 = CARTESIAN_POINT ( 'NONE',  ( 1.033464566929134687, 0.06523048226347956391, 0.6422244094488180899 ) ) ;
#3027 = CARTESIAN_POINT ( 'NONE',  ( 0.7646288533564489232, -0.1113553986120547346, 0.6250000000000000000 ) ) ;
#3028 = CARTESIAN_POINT ( 'NONE',  ( -0.1797182628040039087, -0.8696304237562747508, -0.07444174185955065859 ) ) ;
#3029 = LINE ( 'NONE', #24857, #4888 ) ;
#3030 = CARTESIAN_POINT ( 'NONE',  ( -0.8107537697050253289, -0.1574803149606297803, 1.365649606191684295 ) ) ;
#3031 = CARTESIAN_POINT ( 'NONE',  ( 0.8759842519685039353, -0.1787899950787401882, 0.8046259841982047467 ) ) ;
#3032 = CARTESIAN_POINT ( 'NONE',  ( -0.1113553986120547346, -0.5344488188976378451, 0.1113553986120547346 ) ) ;
#3033 = CARTESIAN_POINT ( 'NONE',  ( 1.033464566929134687, 0.06523048226347956391, 1.616633858160190229 ) ) ;
#3034 = ORIENTED_EDGE ( 'NONE', *, *, #40501, .T. ) ;
#3035 = CARTESIAN_POINT ( 'NONE',  ( 1.033464566929134687, 0.06523048226347956391, 0.1599409447743626866 ) ) ;
#3036 = CARTESIAN_POINT ( 'NONE',  ( 0.7185039370078746268, -0.06523048226347956391, 1.252460629921259061 ) ) ;
#3038 = CARTESIAN_POINT ( 'NONE',  ( 0.7185039370078739607, 0.000000000000000000, 4.498031496062992574 ) ) ;
#3037 = CARTESIAN_POINT ( 'NONE',  ( 0.7464489022532936335, -0.1098404454055766921, 1.985481321410791367 ) ) ;
#3039 = CIRCLE ( 'NONE', #11473, 0.1574803149606299191 ) ;
#3040 = CARTESIAN_POINT ( 'NONE',  ( 0.9412147342319837628, -0.1574803149606297803, 1.734744094488190003 ) ) ;
#3042 = CYLINDRICAL_SURFACE ( 'NONE', #26195, 0.1574803149606291142 ) ;
#3041 = CARTESIAN_POINT ( 'NONE',  ( 0.7495606340400177148, 0.1264236179284866091, 0.6274606298674959559 ) ) ;
#3043 = CARTESIAN_POINT ( 'NONE',  ( -0.7646288533564489232, -0.1113553986120547346, 0.3789370077664886427 ) ) ;
#3044 = ORIENTED_EDGE ( 'NONE', *, *, #24684, .T. ) ;
#3045 = FACE_OUTER_BOUND ( 'NONE', #6887, .T. ) ;
#3046 = CARTESIAN_POINT ( 'NONE',  ( 0.000000000000000000, 0.000000000000000000, -0.2748405511811023438 ) ) ;
#3047 = CARTESIAN_POINT ( 'NONE',  ( 0.8019270111902717657, 0.1787899950787401604, 0.9793307086076531442 ) ) ;
#3048 = CARTESIAN_POINT ( 'NONE',  ( 0.8759842519685039353, 0.1574803149606299191, 1.476377952755905554 ) ) ;
#3049 = CARTESIAN_POINT ( 'NONE',  ( 0.1574803149606339714, 0.5288907983920063671, -0.7507079620615686455 ) ) ;
#3050 = CARTESIAN_POINT ( 'NONE',  ( -0.1270800023317771588, 0.04326327703112763101, 0.1270800023317771588 ) ) ;
#3051 = CARTESIAN_POINT ( 'NONE',  ( -0.1787899950787401604, -0.9872047243556864027, 0.07405724077823318263 ) ) ;
#3052 = CARTESIAN_POINT ( 'NONE',  ( -0.06523048226347956391, -1.491633858267717549, -0.1574803149606300301 ) ) ;
#3053 = EDGE_CURVE ( 'NONE', #36104, #36896, #36781, .T. ) ;
#3054 = DIRECTION ( 'NONE',  ( -0.000000000000000000, 1.000000000000000000, -0.000000000000000000 ) ) ;
#3055 = EDGE_LOOP ( 'NONE', ( #8748, #27707, #12776, #33393, #5370, #22939, #8609, #37631, #5677, #29321, #36750, #3117 ) ) ;
#3056 = CARTESIAN_POINT ( 'NONE',  ( -0.8019270111902717657, -0.1787899950787401604, 0.1279527558517483676 ) ) ;
#3057 = VERTEX_POINT ( 'NONE', #11156 ) ;
#3058 = ORIENTED_EDGE ( 'NONE', *, *, #38098, .F. ) ;
#3059 = CARTESIAN_POINT ( 'NONE',  ( 1.054774247047244540, 0.07405724077823318263, 1.958661417269071947 ) ) ;
#3060 = VERTEX_POINT ( 'NONE', #33447 ) ;
#3061 = CARTESIAN_POINT ( 'NONE',  ( -0.8759842519685039353, -0.1787899950787401882, 1.946358267662771757 ) ) ;
#3062 = CARTESIAN_POINT ( 'NONE',  ( -0.9500414927467378812, 0.1787899950787401604, 1.525590551127340433 ) ) ;
#3063 = CARTESIAN_POINT ( 'NONE',  ( 0.8759842519685039353, -0.1787899950787401882, 0.8439960629383622681 ) ) ;
#3064 = CARTESIAN_POINT ( 'NONE',  ( -0.7495606340400177148, 0.1264236179284866091, 0.8243110235682834519 ) ) ;
#3065 = CARTESIAN_POINT ( 'NONE',  ( -0.8019270111902717657, 0.1787899950787401604, 0.3543307086076538659 ) ) ;
#3066 = VECTOR ( 'NONE', #30402, 39.37007874015748143 ) ;
#3067 = CARTESIAN_POINT ( 'NONE',  ( -0.8107537697050254399, -0.1574803149606297803, 0.6668307086614162493 ) ) ;
#3068 = CARTESIAN_POINT ( 'NONE',  ( -1.002407869896990045, 0.1264236179284866091, 1.921751968450173376 ) ) ;
#3069 = CARTESIAN_POINT ( 'NONE',  ( -1.033464566929134687, 0.06523048226347956391, 1.468996062992126150 ) ) ;
#3070 = CARTESIAN_POINT ( 'NONE',  ( -0.9412147342319837628, -0.1574803149606297803, 1.852854330708662012 ) ) ;
#3071 = DIRECTION ( 'NONE',  ( -1.000000000000000000, 0.000000000000000000, 0.000000000000000000 ) ) ;
#3072 = CARTESIAN_POINT ( 'NONE',  ( 0.1264236179284866091, -0.2771908973630972661, 0.1264236179284866091 ) ) ;
#3073 = EDGE_CURVE ( 'NONE', #43630, #31988, #3937, .T. ) ;
#3074 = DIRECTION ( 'NONE',  ( 0.000000000000000000, 0.7880107536067209040, -0.6156614753256596240 ) ) ;
#3075 = DIRECTION ( 'NONE',  ( 3.469446951953613794E-15, 1.000000000000000000, 0.000000000000000000 ) ) ;
#3076 = EDGE_CURVE ( 'NONE', #35796, #18058, #15219, .T. ) ;
#3077 = PRODUCT_DEFINITION_SHAPE ( 'NONE', 'NONE',  #47476 ) ;
#3078 = VECTOR ( 'NONE', #13038, 39.37007874015748143 ) ;
#3079 = VECTOR ( 'NONE', #879, 39.37007874015748143 ) ;
#3080 = CARTESIAN_POINT ( 'NONE',  ( -0.8019270111902717657, 0.1787899950787401604, 0.1131889763241894359 ) ) ;
#3081 = EDGE_CURVE ( 'NONE', #34571, #38848, #8006, .T. ) ;
#3082 = VERTEX_POINT ( 'NONE', #40809 ) ;
#3083 = VERTEX_POINT ( 'NONE', #34152 ) ;
#3084 = CARTESIAN_POINT ( 'NONE',  ( -1.002407869896990045, -0.1264236179284866091, 1.203248031442299304 ) ) ;
#3085 = ORIENTED_EDGE ( 'NONE', *, *, #10473, .F. ) ;
#3086 = EDGE_CURVE ( 'NONE', #23115, #28092, #1608, .T. ) ;
#3087 = CARTESIAN_POINT ( 'NONE',  ( -0.07405724077823318263, -1.193897637741512696, -0.1787899950787401604 ) ) ;
#3088 = CARTESIAN_POINT ( 'NONE',  ( -0.07405724077823318263, -1.331692913332063855, 0.1787899950787401604 ) ) ;
#3089 = EDGE_CURVE ( 'NONE', #43974, #17392, #15936, .T. ) ;
#3090 = DIRECTION ( 'NONE',  ( 0.000000000000000000, 0.000000000000000000, 1.000000000000000000 ) ) ;
#3091 = CARTESIAN_POINT ( 'NONE',  ( -0.7185039370078739607, 1.928577636452523993E-17, 0.8858267715460158565 ) ) ;
#3092 = CARTESIAN_POINT ( 'NONE',  ( -0.9412147342319837628, 0.1574803149606300301, 0.7652559055118115516 ) ) ;
#3093 = CARTESIAN_POINT ( 'NONE',  ( 1.054774247047244540, -0.07405724077823318263, 0.4183070865604097133 ) ) ;
#3094 = CARTESIAN_POINT ( 'NONE',  ( 0.06523048226347956391, -0.1333661417322835052, 0.1574803149606297803 ) ) ;
#3095 = CARTESIAN_POINT ( 'NONE',  ( 0.8107537697050253289, -0.1574803149606297803, 1.759350393593260842 ) ) ;
#3096 = VERTEX_POINT ( 'NONE', #47145 ) ;
#3097 = DIRECTION ( 'NONE',  ( -1.144917494144692682E-16, 3.972230510298674823E-31, -1.000000000000000000 ) ) ;
#3098 = CARTESIAN_POINT ( 'NONE',  ( 0.7185039370078746268, 0.06523048226347956391, 0.8144685039370082036 ) ) ;
#3099 = CARTESIAN_POINT ( 'NONE',  ( -0.7646288533564489232, 0.1113553986120547346, 1.087598425196850460 ) ) ;
#3100 = AXIS2_PLACEMENT_3D ( 'NONE', #44837, #45313, #7327 ) ;
#3102 = CARTESIAN_POINT ( 'NONE',  ( 0.1600714537641845792, -0.1485828198929936561, -0.02360507234447689617 ) ) ;
#3101 = CARTESIAN_POINT ( 'NONE',  ( 0.8759842519685039353, 0.000000000000000000, 4.498031496062992574 ) ) ;
#3103 = CARTESIAN_POINT ( 'NONE',  ( 0.8759842519685039353, 0.1574803149606299191, 0.1279527557979848462 ) ) ;
#3104 = CONICAL_SURFACE ( 'NONE', #11585, 0.2471922904502826812, 0.5235987755982992597 ) ;
#3105 = VERTEX_POINT ( 'NONE', #14329 ) ;
#3106 = FACE_OUTER_BOUND ( 'NONE', #33784, .T. ) ;
#3107 = CARTESIAN_POINT ( 'NONE',  ( -0.1574803149606300301, -1.594980314853101877, -0.06523048226347956391 ) ) ;
#3109 = CARTESIAN_POINT ( 'NONE',  ( 0.1264236179284866091, -0.5812007873478111097, 0.1264236179284866091 ) ) ;
#3108 = CARTESIAN_POINT ( 'NONE',  ( -0.1574803149606297803, -0.9995078739082206010, 0.06523048226347956391 ) ) ;
#3110 = VECTOR ( 'NONE', #33947, 39.37007874015748143 ) ;
#3111 = CARTESIAN_POINT ( 'NONE',  ( -0.1574803149606300301, -1.014271653543308060, -0.06523048226347956391 ) ) ;
#3112 = CARTESIAN_POINT ( 'NONE',  ( 0.7185039370078746268, -0.06523048226347956391, 1.045767716427905114 ) ) ;
#3113 = ORIENTED_EDGE ( 'NONE', *, *, #40975, .F. ) ;
#3114 = VERTEX_POINT ( 'NONE', #14802 ) ;
#3115 = CARTESIAN_POINT ( 'NONE',  ( -0.6971942568897637749, 2.189545951927499583E-17, 1.582185039316315045 ) ) ;
#3117 = ORIENTED_EDGE ( 'NONE', *, *, #33699, .F. ) ;
#3116 = CIRCLE ( 'NONE', #29957, 0.09842519685039317900 ) ;
#3118 = CARTESIAN_POINT ( 'NONE',  ( 1.002407869896990045, -0.1264236179284866091, 1.596948818843874074 ) ) ;
#3119 = CARTESIAN_POINT ( 'NONE',  ( -0.06523048226347956391, -1.270177165246803463, 0.1574803149606297803 ) ) ;
#3120 = CARTESIAN_POINT ( 'NONE',  ( -0.7495606340400177148, 0.1264236179284866091, 0.6323818897100157432 ) ) ;
#3121 = EDGE_CURVE ( 'NONE', #763, #4939, #47422, .T. ) ;
#3122 = CARTESIAN_POINT ( 'NONE',  ( -0.7185039370078746268, -0.06523048226347956391, 0.4552165353255435698 ) ) ;
#3123 = CARTESIAN_POINT ( 'NONE',  ( -1.054774247047244540, 0.07405724077823318263, 0.7332677164816705506 ) ) ;
#3124 = DIRECTION ( 'NONE',  ( -1.000000000000000000, -0.000000000000000000, -0.000000000000000000 ) ) ;
#3125 = CARTESIAN_POINT ( 'NONE',  ( -0.2066929133858267931, 0.1005108776172154716, -0.1165245190822937899 ) ) ;
#3126 = CARTESIAN_POINT ( 'NONE',  ( 0.1574803149606299191, -0.1555118109160950890, -1.928577636452523993E-17 ) ) ;
#3127 = CARTESIAN_POINT ( 'NONE',  ( -0.8019270111902717657, 0.1787899950787401604, 1.417322834591906222 ) ) ;
#3128 = VERTEX_POINT ( 'NONE', #28974 ) ;
#3129 = CARTESIAN_POINT ( 'NONE',  ( 0.1377952755905509641, 0.000000000000000000, -0.06545654452343109553 ) ) ;
#3130 = CARTESIAN_POINT ( 'NONE',  ( -0.7185039370078739607, 1.928577636452523993E-17, 0.3838582677165354173 ) ) ;
#3131 = EDGE_CURVE ( 'NONE', #40452, #34618, #3116, .T. ) ;
#3132 = CARTESIAN_POINT ( 'NONE',  ( 0.8019270111902716547, 0.1787899950787401604, 1.456692913332062522 ) ) ;
#3133 = CARTESIAN_POINT ( 'NONE',  ( 0.02145388603015350309, -0.09851384249135294868, -0.1903720119548976408 ) ) ;
#3134 = CARTESIAN_POINT ( 'NONE',  ( -0.8759842519685039353, 0.1574803149606299191, 0.3641732282389295583 ) ) ;
#3135 = ORIENTED_EDGE ( 'NONE', *, *, #11426, .T. ) ;
#3136 = CARTESIAN_POINT ( 'NONE',  ( 3.284318927891251994E-17, -1.699434991851285659, 0.1787899950787401882 ) ) ;
#3137 = ORIENTED_EDGE ( 'NONE', *, *, #14250, .F. ) ;
#3138 = ORIENTED_EDGE ( 'NONE', *, *, #37885, .T. ) ;
#3139 = CARTESIAN_POINT ( 'NONE',  ( 0.7495606340400177148, 0.1264236179284866091, 1.454232283410803017 ) ) ;
#3140 = CIRCLE ( 'NONE', #18475, 0.09842519685039370636 ) ;
#3141 = CIRCLE ( 'NONE', #35331, 0.01968503937007870172 ) ;
#3142 = AXIS2_PLACEMENT_3D ( 'NONE', #8163, #26882, #19187 ) ;
#3143 = DIRECTION ( 'NONE',  ( 1.822029033848725028E-16, 0.000000000000000000, 1.000000000000000000 ) ) ;
#3144 = CARTESIAN_POINT ( 'NONE',  ( 0.07405724077823318263, -0.2687007873478113318, 0.1787899950787401604 ) ) ;
#3145 = ( BOUNDED_CURVE ( )  B_SPLINE_CURVE ( 2, ( #34490, #30682, #4272, #11747, #44297, #8362, #41638, #37851, #41399 ),
 .UNSPECIFIED., .F., .T. ) 
 B_SPLINE_CURVE_WITH_KNOTS ( ( 3, 2, 2, 2, 3 ),
 ( 0.8800000000000000044, 0.8824999999999999512, 0.8850000000000000089, 0.8874999999999999556, 0.8900000000000000133 ),
 .UNSPECIFIED. ) 
 CURVE ( )  GEOMETRIC_REPRESENTATION_ITEM ( )  RATIONAL_B_SPLINE_CURVE ( ( 1.000000000000000000, 0.9238795325112869605, 1.000000000000000000, 0.9238795325112869605, 1.000000000000000000, 0.9238795325112869605, 1.000000000000000000, 0.9238795325112829637, 1.000000000000000000 ) ) 
 REPRESENTATION_ITEM ( '' )  ) ;
#3146 = CARTESIAN_POINT ( 'NONE',  ( -0.1787899950787401604, -0.8641732282926931630, 0.07405724077823318263 ) ) ;
#3147 = ADVANCED_FACE ( 'NONE', ( #18842 ), #8057, .T. ) ;
#3148 = CARTESIAN_POINT ( 'NONE',  ( -0.3551574803149606385, -2.130889186148732174E-17, 0.000000000000000000 ) ) ;
#3149 = CARTESIAN_POINT ( 'NONE',  ( 0.1638066842826735592, -0.1611410944699764314, 1.358467538918664965E-08 ) ) ;
#3150 = CARTESIAN_POINT ( 'NONE',  ( 0.8019270111902717657, 0.1787899950787401604, 0.3494094487651343006 ) ) ;
#3151 = CARTESIAN_POINT ( 'NONE',  ( -0.07405724077823318263, -0.1812263304339632453, -0.1787899950787401604 ) ) ;
#3152 = CARTESIAN_POINT ( 'NONE',  ( -1.094772975963752103E-17, 0.06348425202226751218, -0.1787899950787401882 ) ) ;
#3153 = FACE_OUTER_BOUND ( 'NONE', #4062, .T. ) ;
#3154 = CARTESIAN_POINT ( 'NONE',  ( -0.8759842519685039353, -0.1574803149606299191, 1.692913385826771533 ) ) ;
#3155 = CARTESIAN_POINT ( 'NONE',  ( 0.8759842519685039353, -0.1787899950787401882, 0.5634842519147401640 ) ) ;
#3156 = CARTESIAN_POINT ( 'NONE',  ( -1.002407869896990045, 0.1264236179284866091, 0.9768700786863937502 ) ) ;
#3158 = CARTESIAN_POINT ( 'NONE',  ( 0.4755220087074803481, 0.09842519685039370636, 0.000000000000000000 ) ) ;
#3157 = CARTESIAN_POINT ( 'NONE',  ( -0.9761154771909834604, 0.1345094614233016683, 0.03937007874015843734 ) ) ;
#3159 = CARTESIAN_POINT ( 'NONE',  ( -0.1270800023317771588, -1.698862707220840429, -0.1270800023317771588 ) ) ;
#3160 = DIRECTION ( 'NONE',  ( -1.000000000000000000, 0.000000000000000000, 0.000000000000000000 ) ) ;
#3161 = CARTESIAN_POINT ( 'NONE',  ( 0.7495606340400177148, -0.1264236179284866091, 1.665846456639149764 ) ) ;
#3163 = CARTESIAN_POINT ( 'NONE',  ( 0.2559055118110235005, 0.05276756496564156268, -0.3119197741533752954 ) ) ;
#3162 = CARTESIAN_POINT ( 'NONE',  ( 1.054774247047244540, -0.07405724077823318263, 1.948818897584033705 ) ) ;
#3164 = VERTEX_POINT ( 'NONE', #21748 ) ;
#3165 = VERTEX_POINT ( 'NONE', #10746 ) ;
#3166 = CARTESIAN_POINT ( 'NONE',  ( 0.1787899950787401604, -0.06692913380450424277, 0.07405724077823318263 ) ) ;
#3167 = CARTESIAN_POINT ( 'NONE',  ( 0.6971942568897626646, 0.07405724077823318263, 0.6692913385289144257 ) ) ;
#3168 = CARTESIAN_POINT ( 'NONE',  ( -0.1787899950787401604, -1.100393700733639069, 0.07405724077823318263 ) ) ;
#3169 = CARTESIAN_POINT ( 'NONE',  ( 0.9500414927467378812, -0.1787899950787401604, 0.09842519679663024046 ) ) ;
#3170 = CARTESIAN_POINT ( 'NONE',  ( 0.1968503937007874682, -0.5192708129487058066, -0.8938220056861535534 ) ) ;
#3171 = AXIS2_PLACEMENT_3D ( 'NONE', #38062, #5217, #38991 ) ;
#3172 = CARTESIAN_POINT ( 'NONE',  ( -0.8759842519685039353, -0.1787899950787401882, 1.626476377898992132 ) ) ;
#3173 = ORIENTED_EDGE ( 'NONE', *, *, #15768, .T. ) ;
#3174 = CARTESIAN_POINT ( 'NONE',  ( -0.7495606340400177148, 0.1264236179284866091, 1.104822834591905556 ) ) ;
#3175 = DIRECTION ( 'NONE',  ( -1.000000000000000000, 0.000000000000000000, 0.000000000000000000 ) ) ;
#3176 = CARTESIAN_POINT ( 'NONE',  ( 0.8759842519685039353, 0.1787899950787401882, 1.099901574749385880 ) ) ;
#3177 = CARTESIAN_POINT ( 'NONE',  ( -0.1113553986120547346, -1.154527558947590515, 0.1113553986120547346 ) ) ;
#3178 = CARTESIAN_POINT ( 'NONE',  ( -0.9873396505805591694, 0.1113553986120547346, 0.6742125983176693316 ) ) ;
#3179 = AXIS2_PLACEMENT_3D ( 'NONE', #18558, #11154, #32969 ) ;
#3180 = CARTESIAN_POINT ( 'NONE',  ( 0.8759842519685039353, -0.1787899950787401882, 1.862696850339937038 ) ) ;
#3181 = CARTESIAN_POINT ( 'NONE',  ( -0.8107537697050253289, 0.1574803149606300301, 0.5733267716535435099 ) ) ;
#3182 = CARTESIAN_POINT ( 'NONE',  ( -1.054774247047244540, 0.07405724077823318263, 0.8513779527021426707 ) ) ;
#3183 = EDGE_CURVE ( 'NONE', #44249, #11279, #817, .T. ) ;
#3184 = LINE ( 'NONE', #15175, #34310 ) ;
#3185 = DIRECTION ( 'NONE',  ( -1.000000000000000000, 0.000000000000000000, 0.000000000000000000 ) ) ;
#3186 = CARTESIAN_POINT ( 'NONE',  ( 0.9500414927467377701, -0.1787899950787401604, 0.2952755904974176948 ) ) ;
#3187 = CARTESIAN_POINT ( 'NONE',  ( -0.8759842519685039353, -0.1787899950787401882, 0.2091535432533232486 ) ) ;
#3188 = CARTESIAN_POINT ( 'NONE',  ( -1.002407869896990045, -0.1264236179284866091, 0.5684055117572598403 ) ) ;
#3189 = CARTESIAN_POINT ( 'NONE',  ( 0.9873396505805591694, 0.1113553986120547346, 1.500984251860976171 ) ) ;
#3190 = ORIENTED_EDGE ( 'NONE', *, *, #36320, .T. ) ;
#3191 = EDGE_CURVE ( 'NONE', #41717, #2, #33783, .T. ) ;
#3192 = CARTESIAN_POINT ( 'NONE',  ( -0.1787899950787401604, -0.04232283459190575026, 0.07405724077823318263 ) ) ;
#3193 = ORIENTED_EDGE ( 'NONE', *, *, #21733, .T. ) ;
#3194 = CARTESIAN_POINT ( 'NONE',  ( 1.054774247047244540, -0.07405724077823318263, 0.8120078739619844832 ) ) ;
#3195 = EDGE_CURVE ( 'NONE', #22011, #37817, #22200, .T. ) ;
#3196 = CARTESIAN_POINT ( 'NONE',  ( -0.7495606340400177148, 0.1264236179284866091, 1.847933070812378009 ) ) ;
#3197 = EDGE_CURVE ( 'NONE', #38861, #65, #15496, .T. ) ;
#3198 = CARTESIAN_POINT ( 'NONE',  ( 0.8759842519685039353, 0.000000000000000000, 4.498031496062992574 ) ) ;
#3199 = FACE_OUTER_BOUND ( 'NONE', #16797, .T. ) ;
#3200 = CARTESIAN_POINT ( 'NONE',  ( 0.1264236179284866091, -1.369710582402466681, -0.1264236179284866091 ) ) ;
#3201 = ORIENTED_EDGE ( 'NONE', *, *, #36095, .T. ) ;
#3202 = CARTESIAN_POINT ( 'NONE',  ( -0.1787899950787401882, -0.2367125983714334636, 0.000000000000000000 ) ) ;
#3203 = EDGE_LOOP ( 'NONE', ( #24466, #16321, #10489, #24480 ) ) ;
#3204 = AXIS2_PLACEMENT_3D ( 'NONE', #17491, #2626, #35943 ) ;
#3205 = FACE_OUTER_BOUND ( 'NONE', #16925, .T. ) ;
#3206 = CARTESIAN_POINT ( 'NONE',  ( -0.2471914725378674960, -0.08966515697905538818, 0.05042473337808872635 ) ) ;
#3207 = CARTESIAN_POINT ( 'NONE',  ( 0.9873396505805591694, -0.1113553986120547346, 1.934055118110236338 ) ) ;
#3208 = AXIS2_PLACEMENT_3D ( 'NONE', #14187, #36698, #3857 ) ;
#3209 = CARTESIAN_POINT ( 'NONE',  ( -0.07405724077823318263, -1.626968503883244876, -0.1787899950787401604 ) ) ;
#3210 = CARTESIAN_POINT ( 'NONE',  ( -0.9500414927467377701, 0.1787899950787401604, 0.4281496062454490659 ) ) ;
#3211 = FACE_OUTER_BOUND ( 'NONE', #29205, .T. ) ;
#3212 = CONICAL_SURFACE ( 'NONE', #921, 0.1377952755905511861, 1.047197551196598297 ) ;
#3213 = CARTESIAN_POINT ( 'NONE',  ( 0.8759842519685039353, 0.1787899950787401882, 1.257381889710015743 ) ) ;
#3214 = CARTESIAN_POINT ( 'NONE',  ( 1.002407869896990045, -0.1264236179284866091, 1.473917322780881722 ) ) ;
#3215 = CARTESIAN_POINT ( 'NONE',  ( 0.2519685039370078705, 0.08090551181102362266, 0.000000000000000000 ) ) ;
#3216 = DIRECTION ( 'NONE',  ( 0.000000000000000000, 1.000000000000000000, 0.000000000000000000 ) ) ;
#3217 = CARTESIAN_POINT ( 'NONE',  ( 0.7185039370078746268, 0.06523048226347956391, 0.6865157479239700766 ) ) ;
#3218 = CARTESIAN_POINT ( 'NONE',  ( -0.7646288533564489232, 0.1113553986120547346, 1.668307086506645609 ) ) ;
#3219 = CARTESIAN_POINT ( 'NONE',  ( -0.1787899950787401604, 0.001968503990771383692, 0.07405724077823318263 ) ) ;
#3220 = CARTESIAN_POINT ( 'NONE',  ( 0.7495606340400177148, 0.1264236179284866091, 0.1550196849856066983 ) ) ;
#3221 = CARTESIAN_POINT ( 'NONE',  ( 0.7058544154350729904, 0.05181626514163805569, 0.03937118780267125084 ) ) ;
#3223 = DIRECTION ( 'NONE',  ( 0.000000000000000000, 0.000000000000000000, 1.000000000000000000 ) ) ;
#3222 = CARTESIAN_POINT ( 'NONE',  ( 0.8019270111902716547, 0.1787899950787401604, 1.136811023568283119 ) ) ;
#3224 = CARTESIAN_POINT ( 'NONE',  ( 0.8759842519685039353, 0.1574803149606299191, 0.5610236219397165547 ) ) ;
#3225 = ORIENTED_EDGE ( 'NONE', *, *, #6637, .F. ) ;
#3226 = CARTESIAN_POINT ( 'NONE',  ( -1.054774247047244096, 0.000000000000000000, 1.050688976324189117 ) ) ;
#3227 = CARTESIAN_POINT ( 'NONE',  ( 0.2395294000716134131, 0.000000000000000000, 0.8759842519685039353 ) ) ;
#3228 = CARTESIAN_POINT ( 'NONE',  ( 0.9907320134992387839, 0.1205351961251636961, 0.03937007592068544892 ) ) ;
#3230 = ORIENTED_EDGE ( 'NONE', *, *, #31890, .T. ) ;
#3229 = CARTESIAN_POINT ( 'NONE',  ( 0.1113553986120547346, -1.026574803042078710, 0.1113553986120547346 ) ) ;
#3231 = CARTESIAN_POINT ( 'NONE',  ( -1.033464566929134687, 0.06523048226347956391, 0.3567913384751500994 ) ) ;
#3232 = ORIENTED_EDGE ( 'NONE', *, *, #31414, .F. ) ;
#3233 = CARTESIAN_POINT ( 'NONE',  ( 0.6971942568897648851, 0.07405724077823318263, 1.377952755851748146 ) ) ;
#3234 = FACE_OUTER_BOUND ( 'NONE', #27702, .T. ) ;
#3235 = CARTESIAN_POINT ( 'NONE',  ( 0.7185039370078746268, -0.06523048226347956391, 1.173720472440945350 ) ) ;
#3236 = CARTESIAN_POINT ( 'NONE',  ( -0.07405724077823318263, -0.08661417317458304510, -0.1787899950787401604 ) ) ;
#3237 = VERTEX_POINT ( 'NONE', #3536 ) ;
#3238 = CARTESIAN_POINT ( 'NONE',  ( 0.7185039370078746268, 0.06523048226347956391, 0.4502952754830242821 ) ) ;
#3239 = EDGE_CURVE ( 'NONE', #6537, #18481, #9773, .T. ) ;
#3240 = AXIS2_PLACEMENT_3D ( 'NONE', #24586, #9508, #14284 ) ;
#3241 = ORIENTED_EDGE ( 'NONE', *, *, #7301, .T. ) ;
#3242 = CYLINDRICAL_SURFACE ( 'NONE', #18362, 0.09842519685039310962 ) ;
#3243 = CARTESIAN_POINT ( 'NONE',  ( 0.1350242358428265510, -0.09796987684348243408, -0.2074744707780996344 ) ) ;
#3244 = ORIENTED_EDGE ( 'NONE', *, *, #38358, .T. ) ;
#3245 = CARTESIAN_POINT ( 'NONE',  ( 0.8019270111902717657, -0.1787899950787401604, 0.6053149605761579677 ) ) ;
#3247 = ADVANCED_FACE ( 'NONE', ( #147 ), #3212, .T. ) ;
#3246 = ORIENTED_EDGE ( 'NONE', *, *, #27251, .T. ) ;
#3248 = CARTESIAN_POINT ( 'NONE',  ( 0.1264236179284866091, -1.791830708607653699, -0.1264236179284866091 ) ) ;
#3249 = CARTESIAN_POINT ( 'NONE',  ( -0.8759842519685039353, -0.1787899950787401882, 1.158956692859621995 ) ) ;
#3250 = VECTOR ( 'NONE', #35313, 39.37007874015748143 ) ;
#3251 = CARTESIAN_POINT ( 'NONE',  ( -0.7646288533564489232, -0.1113553986120547346, 0.07381889763779526936 ) ) ;
#3252 = VERTEX_POINT ( 'NONE', #40862 ) ;
#3253 = CARTESIAN_POINT ( 'NONE',  ( -1.054774247047244540, -0.07405724077823318263, 1.161417322780881278 ) ) ;
#3254 = EDGE_CURVE ( 'NONE', #6831, #11278, #11439, .T. ) ;
#3255 = CARTESIAN_POINT ( 'NONE',  ( -0.6971942568897626646, -0.07405724077823297447, 0.2460629920722207375 ) ) ;
#3256 = CARTESIAN_POINT ( 'NONE',  ( 0.9412147342319837628, 0.1574803149606300301, 0.7947834644594015119 ) ) ;
#3257 = CARTESIAN_POINT ( 'NONE',  ( -0.1787899950787401882, -0.8825058579930176172, 0.000000000000000000 ) ) ;
#3258 = AXIS2_PLACEMENT_3D ( 'NONE', #29797, #27075, #45706 ) ;
#3259 = ORIENTED_EDGE ( 'NONE', *, *, #37025, .T. ) ;
#3260 = CARTESIAN_POINT ( 'NONE',  ( -0.1113553986120547346, -0.01279527548302413463, 0.1113553986120547346 ) ) ;
#3261 = CARTESIAN_POINT ( 'NONE',  ( 0.7374060038789669314, 0.1135695039425618086, 0.03936553649663185328 ) ) ;
#3262 = ORIENTED_EDGE ( 'NONE', *, *, #4046, .T. ) ;
#3263 = EDGE_LOOP ( 'NONE', ( #21572, #9337, #26416, #43733, #38615 ) ) ;
#3264 = CARTESIAN_POINT ( 'NONE',  ( 0.000000000000000000, 0.000000000000000000, -1.181102362204724310 ) ) ;
#3265 = CARTESIAN_POINT ( 'NONE',  ( -0.9500414927467378812, 0.1787899950787401604, 0.6594488188438737408 ) ) ;
#3266 = ORIENTED_EDGE ( 'NONE', *, *, #24133, .T. ) ;
#3267 = CARTESIAN_POINT ( 'NONE',  ( -0.6971942568897648851, -0.07405724077823297447, 1.781496062938362934 ) ) ;
#3268 = EDGE_CURVE ( 'NONE', #3438, #30045, #43775, .T. ) ;
#3269 = FACE_OUTER_BOUND ( 'NONE', #7093, .T. ) ;
#3270 = CIRCLE ( 'NONE', #23966, 0.09842519685039370636 ) ;
#3271 = ( NAMED_UNIT ( * ) PLANE_ANGLE_UNIT ( ) SI_UNIT ( $, .RADIAN. ) ) ;
#3272 = ORIENTED_EDGE ( 'NONE', *, *, #2496, .T. ) ;
#3273 = CARTESIAN_POINT ( 'NONE',  ( 0.8759842519685039353, 0.1574803149606299191, 0.6889763779527560139 ) ) ;
#3274 = CARTESIAN_POINT ( 'NONE',  ( -0.07444174185955065859, -0.8597879040712341769, 0.1797182628040039087 ) ) ;
#3275 = CARTESIAN_POINT ( 'NONE',  ( -0.7185039370078739607, 1.928577636452523993E-17, 0.9744094488188976833 ) ) ;
#3276 = CARTESIAN_POINT ( 'NONE',  ( -0.9873396505805591694, -0.1113553986120547346, 1.451771653435779408 ) ) ;
#3277 = CARTESIAN_POINT ( 'NONE',  ( 0.8019270111902717657, 0.1787899950787401604, 0.7086614172690703928 ) ) ;
#3278 = CARTESIAN_POINT ( 'NONE',  ( -0.1574803149606299191, -0.6574803149606299746, 0.000000000000000000 ) ) ;
#3279 = AXIS2_PLACEMENT_3D ( 'NONE', #15161, #44825, #30497 ) ;
#3280 = CARTESIAN_POINT ( 'NONE',  ( -9.642888182262618425E-18, 0.1200787401574803237, -0.1574803149606299191 ) ) ;
#3281 = VERTEX_POINT ( 'NONE', #37060 ) ;
#3282 = DIRECTION ( 'NONE',  ( 0.000000000000000000, 1.000000000000000000, 0.000000000000000000 ) ) ;
#3283 = CARTESIAN_POINT ( 'NONE',  ( 0.7646288533564489232, -0.1113553986120547346, 1.254921259842519676 ) ) ;
#3285 = DIRECTION ( 'NONE',  ( 0.000000000000000000, -1.000000000000000000, 0.000000000000000000 ) ) ;
#3284 = CARTESIAN_POINT ( 'NONE',  ( 0.7756356084717642707, -0.1385908279522278519, 1.986213216910492907 ) ) ;
#3286 = CARTESIAN_POINT ( 'NONE',  ( 0.000000000000000000, 0.000000000000000000, -0.1712639279175142137 ) ) ;
#3287 = CARTESIAN_POINT ( 'NONE',  ( 0.1574803149606299191, -0.6279527557979843744, -1.928577636452523993E-17 ) ) ;
#3289 = DIRECTION ( 'NONE',  ( 0.000000000000000000, 0.000000000000000000, 1.000000000000000000 ) ) ;
#3288 = CARTESIAN_POINT ( 'NONE',  ( 0.6971942568897648851, 0.07405724077823318263, 0.6299212597887560161 ) ) ;
#3290 = CARTESIAN_POINT ( 'NONE',  ( -0.9412147342319837628, 0.1574803149606300301, 0.6865157480314956207 ) ) ;
#3291 = CARTESIAN_POINT ( 'NONE',  ( -1.094772975963752103E-17, -0.6796259841982046357, -0.1787899950787401882 ) ) ;
#3292 = CARTESIAN_POINT ( 'NONE',  ( -0.2362204724409469325, 8.195543980992859667E-16, 0.9891732283464568232 ) ) ;
#3293 = EDGE_LOOP ( 'NONE', ( #20466, #20335, #40495, #27925 ) ) ;
#3294 = DIRECTION ( 'NONE',  ( -1.000000000000000000, 0.000000000000000000, 0.000000000000000000 ) ) ;
#3295 = CARTESIAN_POINT ( 'NONE',  ( 0.7185039370078739607, 1.928577636452523993E-17, 0.6988188976377952555 ) ) ;
#3296 = CARTESIAN_POINT ( 'NONE',  ( 0.6971942568897626646, 0.07405724077823318263, 0.9842519684501742638 ) ) ;
#3297 = ORIENTED_EDGE ( 'NONE', *, *, #11546, .F. ) ;
#3298 = DIRECTION ( 'NONE',  ( 0.000000000000000000, 0.000000000000000000, -1.000000000000000000 ) ) ;
#3299 = CARTESIAN_POINT ( 'NONE',  ( 0.1270800023317771588, 0.02357823766104893623, -0.1270800023317771588 ) ) ;
#3300 = CARTESIAN_POINT ( 'NONE',  ( 0.1264236179284866091, -1.211122047190330786, 0.1264236179284866091 ) ) ;
#3301 = CARTESIAN_POINT ( 'NONE',  ( 0.1113553986120547346, -1.548228346456692828, 0.1113553986120547346 ) ) ;
#3302 = CARTESIAN_POINT ( 'NONE',  ( -0.07874015748031495954, 0.3740157480314960092, 0.9783464566929293005 ) ) ;
#3303 = ( BOUNDED_CURVE ( )  B_SPLINE_CURVE ( 2, ( #6642, #7126, #11680, #22684, #37286, #33024, #11210, #37061, #21749 ),
 .UNSPECIFIED., .F., .T. ) 
 B_SPLINE_CURVE_WITH_KNOTS ( ( 3, 2, 2, 2, 3 ),
 ( 0.1400000000000000133, 0.1424999999999999878, 0.1449999999999999900, 0.1474999999999999922, 0.1499999999999999944 ),
 .UNSPECIFIED. ) 
 CURVE ( )  GEOMETRIC_REPRESENTATION_ITEM ( )  RATIONAL_B_SPLINE_CURVE ( ( 1.000000000000000000, 0.9238795325112869605, 1.000000000000000000, 0.9238795325112869605, 1.000000000000000000, 0.9238795325112869605, 1.000000000000000000, 0.9238795325112869605, 1.000000000000000000 ) ) 
 REPRESENTATION_ITEM ( '' )  ) ;
#3304 = EDGE_CURVE ( 'NONE', #26454, #17892, #7366, .T. ) ;
#3305 = CARTESIAN_POINT ( 'NONE',  ( -0.7495606340400177148, 0.1264236179284866091, 0.07627952750529173875 ) ) ;
#3306 = DIRECTION ( 'NONE',  ( 0.000000000000000000, 0.000000000000000000, -1.000000000000000000 ) ) ;
#3307 = ORIENTED_EDGE ( 'NONE', *, *, #17583, .F. ) ;
#3309 = CARTESIAN_POINT ( 'NONE',  ( -0.1264236179284866091, -1.417814960576157635, 0.1264236179284866091 ) ) ;
#3308 = CARTESIAN_POINT ( 'NONE',  ( 0.1574803149606300301, -1.412893700679873632, -0.06523048226347956391 ) ) ;
#3310 = DIRECTION ( 'NONE',  ( 1.822029033848725028E-16, 0.000000000000000000, 1.000000000000000000 ) ) ;
#3311 = CARTESIAN_POINT ( 'NONE',  ( -0.6971942568897637749, 2.189545951927499583E-17, 1.695374015694267822 ) ) ;
#3312 = CARTESIAN_POINT ( 'NONE',  ( 0.6971942568897648851, 0.07405724077823318263, 0.9104330708123777871 ) ) ;
#3313 = ADVANCED_FACE ( 'NONE', ( #391 ), #35406, .T. ) ;
#3314 = CARTESIAN_POINT ( 'NONE',  ( -0.8759842519685039353, -0.1787899950787401882, 1.075295275536787276 ) ) ;
#3315 = CARTESIAN_POINT ( 'NONE',  ( -1.054774247047244540, -0.07405724077823318263, 0.4183070865604097133 ) ) ;
#3316 = CARTESIAN_POINT ( 'NONE',  ( -0.8759842519685039353, -0.1574803149606299191, 0.6692913385826771977 ) ) ;
#3317 = CARTESIAN_POINT ( 'NONE',  ( -0.8759842519685039353, 0.1787899950787401882, 1.887303149552535420 ) ) ;
#3318 = CARTESIAN_POINT ( 'NONE',  ( -0.7646288533564489232, 0.1113553986120547346, 1.481299212598425230 ) ) ;
#3319 = CARTESIAN_POINT ( 'NONE',  ( -1.033464566929134687, 0.06523048226347956391, 1.862696850393700254 ) ) ;
#3320 = CARTESIAN_POINT ( 'NONE',  ( -0.7185039370078746268, 0.06523048226347956391, 0.3026574803149607029 ) ) ;
#3321 = CARTESIAN_POINT ( 'NONE',  ( 0.07405724077823318263, -0.3829979839772702510, -0.1787899950787401604 ) ) ;
#3322 = CARTESIAN_POINT ( 'NONE',  ( -0.06611196094510747578, -0.09842519685039370636, 0.1467257540889139733 ) ) ;
#3323 = ITEM_DEFINED_TRANSFORMATION ( 'NONE', 'NONE', #973,  #20860 ) ;
#3324 = LINE ( 'NONE', #29009, #47096 ) ;
#3325 = DIRECTION ( 'NONE',  ( 0.000000000000000000, 0.000000000000000000, 1.000000000000000000 ) ) ;
#3326 = AXIS2_PLACEMENT_3D ( 'NONE', #19243, #776, #8695 ) ;
#3327 = AXIS2_PLACEMENT_3D ( 'NONE', #20136, #12966, #17479 ) ;
#3328 = ( BOUNDED_CURVE ( )  B_SPLINE_CURVE ( 2, ( #43763, #21484, #7111, #14789, #26045, #17896, #18595, #29215, #37049, #25087, #32543, #10965, #43998, #7355, #381, #22191, #14318, #40388, #36825, #21735, #3977, #22428, #21968, #4202, #39925, #36592, #47131, #18831, #11200, #33486, #43520, #47373, #10488, #14545, #10733, #6864, #36116, #25342, #3522, #37274, #45162, #1803, #4678, #41799, #8521, #15977, #34192, #1555, #8044, #44683, #34412, #8757, #22674, #44455, #19307, #26523, #19061, #40850, #4429, #5158, #33729, #45409, #16211, #23149, #11669, #8999, #840, #12383, #23623, #38233, #1320, #30842, #26761, #15743, #33961, #34653, #16442, #26293, #44923, #12137, #4922, #12622, #15499, #27245, #30145, #41084, #11901, #41318, #19545, #8282, #22908, #27004, #5391, #37521, #20014, #23394, #37999, #45635, #5640, #2271, #35359, #42732, #31996, #16670, #9717, #27487, #6331, #24555, #13091, #2731, #13316, #46588, #27724, #16895, #20252, #10187, #27947, #13768, #23858, #38711, #28409, #42286, #5881, #21184, #20487, #42038, #9947, #13537, #34897, #42978, #31537, #35816, #17128, #20947, #31299, #39160, #24793, #39389, #35125, #6573, #2964, #9486, #24104, #31071, #46118, #42514, #24330, #2038, #9240, #38470, #38929, #2504, #31770, #46353, #36053, #32241, #21913, #43459, #36763, #3210, #46823, #32721, #3921, #29629, #76, #40329, #18544, #44166, #32954, #10666, #11369, #22371, #25273, #14972, #29146, #36535, #7293, #22136, #28659, #17840, #7514, #43224, #17599, #39861, #47067, #39625, #14011, #25030, #25759, #10429, #33200, #21676, #7052, #36307, #36996, #6805, #47312, #21424, #10910, #32485, #322, #14487, #3462, #18073, #7753, #14258, #28900, #43702, #25533, #40099, #3694, #25980, #18316, #40563, #14724, #29397, #43941, #11139, #15683, #19720, #45105, #34358, #44393, #12323, #22849, #30781, #18777, #26231, #37465, #8458, #4613, #41492, #1263, #7990, #34133, #15915, #779, #30542, #41258, #26939, #1495, #33665, #19247, #40797, #45348, #33905, #16150, #11609, #11841, #23333, #1027, #12561, #4858, #8224, #27186, #23088, #4372, #8698, #30320, #22615, #15202, #37705, #37948, #37227, #5096, #41739, #8944, #26468, #23564, #4151, #19002, #44867, #33432, #19484, #12079, #547, #29853, #26703, #15439, #30094, #44626, #41030, #34591, #45574, #46297, #1741, #39099, #42225, #27664, #16614, #42918, #16386, #20430, #5331, #31474, #12794, #24505, #31712, #19951, #9892, #20899, #10129, #38167, #9427, #5822, #2214, #31005, #42679, #27430, #6273, #38873, #28349, #31240, #28119, #16834, #35538, #13488, #6037, #2678, #41970, #13712, #17309, #9179, #23795, #24047, #42457, #38647, #31945, #35306, #38411, #20660, #2443, #34839, #17071, #27895, #46531, #5582, #35063, #46058, #20188, #1984, #13266, #45817, #13027, #9661, #24278, #10613, #22737, #26110, #28843, #33795, #44284, #24978, #29975, #39803, #28603, #35767, #30213, #44758, #40919, #43166, #11738, #4263, #32429, #22495, #44523, #32180, #43404, #24738, #14435, #25211, #7878, #667, #6992, #17542, #21618, #36251, #10371, #3402, #8114, #4493, #29087, #3156, #47007, #39573, #18014, #19131, #6513, #6750, #46767, #40685, #37115, #15574, #32666, #47254, #18896, #13952, #11489, #21371, #33551, #26358, #15322, #2907, #39335, #14199, #35998, #17781, #37342, #913, #21132, #12921, #30669, #1384, #37837, #31370, #37585, #41621, #26596, #5220, #34027, #45703, #8830, #45229, #12453, #2104, #41148, #4747, #27073, #23463, #38065, #19374, #31135, #1153, #27551, #27317, #12202, #4995, #42103, #19849, #9309, #20084, #23932, #26828, #34730, #34476, #38539, #41384, #8586, #1628, #45466, #41866, #34959, #23688, #23223, #27601, #8151, #26871, #22779, #19177, #33837, #956, #37635, #8629, #12014, #30253, #1426, #26637, #8394, #30711, #13882, #42618, #39504, #42844, #24435, #3084, #13643, #42396, #46693, #35471, #45993, #20366, #46938, #10300, #27836, #2610, #28282, #43095, #14127, #17245, #24913, #9596, #5974, #24671, #20595, #17012, #31882, #46460, #42149, #9356, #6679, #10056, #21059, #21295, #35922, #35699, #2835, #17707, #32358, #17470, #23979, #38582, #35003, #2149, #16776, #31416, #33537, #36413, #26094, #40205, #185, #18417, #25393, #25856, #425, #44269, #36869, #7623, #36637, #4024, #14595, #14834, #7164, #10541, #32828, #29267, #39729, #39971, #33064, #11470, #21539, #18643, #36177, #47423, #43340, #650, #3571, #43811, #40437, #29726, #14368, #7399, #25138, #33301, #22240, #43570, #15080, #11011, #40666, #10783, #25631, #17939, #3798, #11245, #7862, #22480, #28770, #22012, #21787, #18188, #18879, #29499, #6916, #37095, #4244, #32594, #3335, #44046, #47185, #29014, #5206, #893, #8569, #34241, #19831, #20067, #34011, #34460, #30197, #44741, #41606, #11960, #15555, #12186, #26579, #34711, #15305, #1610, #1137, #12672, #16258, #41135, #8334, #44973, #30893, #27298, #8808, #38049, #9054, #23675, #30652, #22962, #5452, #29958, #4730, #26342, #26811, #1370, #4976, #8099, #22720, #19355, #37329, #23445, #4477, #23204, #19118, #15797, #16027, #41370, #37820, #31590, #38522, #2787, #39212, #13370, #16489, #13826, #5693, #2554, #46641, #28469, #35647, #42785, #31122, #21002, #32053, #43035, #42340, #20541, #46406, #45685, #16953, #6388, #21243, #17414, #20303, #45933, #10244, #17187, #5923, #24850, #13584, #31821, #34944, #39449, #35176, #6627, #28222, #12906, #2091, #10000, #27538, #24614, #9536, #42090, #9296, #23916, #2321, #16720, #38981, #46172, #42562, #31352, #13145, #27781, #24159, #9770, #38763, #24380, #6145, #3020, #40154, #14315, #10729, #36113, #32776, #29682, #17655, #6859, #43287, #36590, #40615, #25335, #33252, #47372, #7353, #25583, #40383, #46880, #3267, #25811, #33011, #14066, #35870, #39922, #17893, #10486, #25084, #39676, #43997, #21478, #3976, #7576, #29212, #32538, #15031, #47125, #21965, #44221, #11422, #3748, #22187, #18131, #7109, #36367, #26041, #7810, #28959, #3518, #43760, #10962, #18593, #18370, #134, #14784, #29448, #35450, #10282, #39488, #17228, #2822, #10523, #21769, #46443, #14348, #24891, #32809, #20812, #42825, #6665, #25121, #17926, #7145, #39251, #32339, #2594, #28997, #47165, #21044, #25375, #35906, #36399, #35685, #21281, #10038, #47405, #3061, #3556, #13624, #13864, #39954, #24657, #46920, #39713, #43555, #10996, #17688, #10767, #17454, #32089, #36156, #28509, #6425, #14109, #43077 ),
 .UNSPECIFIED., .F., .F. ) 
 B_SPLINE_CURVE_WITH_KNOTS ( ( 3, 2, 2, 2, 2, 2, 2, 2, 2, 2, 2, 2, 2, 2, 2, 2, 2, 2, 2, 2, 2, 2, 2, 2, 2, 2, 2, 2, 2, 2, 2, 2, 2, 2, 2, 2, 2, 2, 2, 2, 2, 2, 2, 2, 2, 2, 2, 2, 2, 2, 2, 2, 2, 2, 2, 2, 2, 2, 2, 2, 2, 2, 2, 2, 2, 2, 2, 2, 2, 2, 2, 2, 2, 2, 2, 2, 2, 2, 2, 2, 2, 2, 2, 2, 2, 2, 2, 2, 2, 2, 2, 2, 2, 2, 2, 2, 2, 2, 2, 2, 2, 2, 2, 2, 2, 2, 2, 2, 2, 2, 2, 2, 2, 2, 2, 2, 2, 2, 2, 2, 2, 2, 2, 2, 2, 2, 2, 2, 2, 2, 2, 2, 2, 2, 2, 2, 2, 2, 2, 2, 2, 2, 2, 2, 2, 2, 2, 2, 2, 2, 2, 2, 2, 2, 2, 2, 2, 2, 2, 2, 2, 2, 2, 2, 2, 2, 2, 2, 2, 2, 2, 2, 2, 2, 2, 2, 2, 2, 2, 2, 2, 2, 2, 2, 2, 2, 2, 2, 2, 2, 2, 2, 2, 2, 2, 2, 2, 2, 2, 2, 2, 2, 2, 2, 2, 2, 2, 2, 2, 2, 2, 2, 2, 2, 2, 2, 2, 2, 2, 2, 2, 2, 2, 2, 2, 2, 2, 2, 2, 2, 2, 2, 2, 2, 2, 2, 2, 2, 2, 2, 2, 2, 2, 2, 2, 2, 2, 2, 2, 2, 2, 2, 2, 2, 2, 2, 2, 2, 2, 2, 2, 2, 2, 2, 2, 2, 2, 2, 2, 2, 2, 2, 2, 2, 2, 2, 2, 2, 2, 2, 2, 2, 2, 2, 2, 2, 2, 2, 2, 2, 2, 2, 2, 2, 2, 2, 2, 2, 2, 2, 2, 2, 2, 2, 2, 2, 2, 2, 2, 2, 2, 2, 2, 2, 2, 2, 2, 2, 2, 2, 2, 2, 2, 2, 2, 2, 2, 2, 2, 2, 2, 2, 2, 2, 2, 2, 2, 2, 2, 2, 2, 2, 2, 2, 2, 2, 2, 2, 2, 2, 2, 2, 2, 2, 2, 2, 2, 2, 2, 2, 2, 2, 2, 2, 2, 2, 2, 2, 2, 2, 2, 2, 2, 2, 2, 2, 2, 2, 2, 2, 2, 2, 2, 2, 2, 2, 2, 2, 2, 2, 2, 2, 2, 2, 2, 2, 2, 3 ),
 ( 0.006250000026272810663, 0.007499999999999999722, 0.01000000000000000021, 0.01250000000000000069, 0.01499999999999999944, 0.01750000000000000167, 0.02000000000000000042, 0.02249999999999999917, 0.02500000000000000139, 0.02749999999999999667, 0.02999999999999999889, 0.03250000000000000111, 0.03500000000000000333, 0.03749999999999999861, 0.04000000000000000083, 0.04250000000000000305, 0.04499999999999999833, 0.04750000000000000056, 0.05000000000000000278, 0.05250000000000000500, 0.05500000000000000028, 0.05750000000000000250, 0.05999999999999999778, 0.06250000000000000000, 0.06500000000000000222, 0.06750000000000000444, 0.07000000000000000666, 0.07249999999999999500, 0.07499999999999999722, 0.07749999999999999944, 0.08000000000000000167, 0.08250000000000000389, 0.08500000000000000611, 0.08749999999999999445, 0.08999999999999999667, 0.09249999999999999889, 0.09500000000000000111, 0.09750000000000000333, 0.1000000000000000056, 0.1024999999999999939, 0.1049999999999999961, 0.1074999999999999983, 0.1100000000000000006, 0.1125000000000000028, 0.1150000000000000050, 0.1174999999999999933, 0.1199999999999999956, 0.1224999999999999978, 0.1250000000000000000, 0.1275000000000000022, 0.1300000000000000044, 0.1325000000000000067, 0.1350000000000000089, 0.1375000000000000111, 0.1400000000000000133, 0.1424999999999999878, 0.1449999999999999900, 0.1474999999999999922, 0.1499999999999999944, 0.1524999999999999967, 0.1549999999999999989, 0.1575000000000000011, 0.1600000000000000033, 0.1625000000000000056, 0.1650000000000000078, 0.1674999999999999822, 0.1700000000000000122, 0.1724999999999999867, 0.1749999999999999889, 0.1774999999999999911, 0.1799999999999999933, 0.1824999999999999956, 0.1849999999999999978, 0.1875000000000000000, 0.1900000000000000022, 0.1925000000000000044, 0.1950000000000000067, 0.1975000000000000089, 0.2000000000000000111, 0.2025000000000000133, 0.2049999999999999878, 0.2074999999999999900, 0.2099999999999999922, 0.2124999999999999944, 0.2149999999999999967, 0.2174999999999999989, 0.2200000000000000011, 0.2225000000000000033, 0.2250000000000000056, 0.2275000000000000078, 0.2299999999999999822, 0.2325000000000000122, 0.2349999999999999867, 0.2374999999999999889, 0.2399999999999999911, 0.2424999999999999933, 0.2449999999999999956, 0.2474999999999999978, 0.2500000000000000000, 0.2525000000000000022, 0.2550000000000000044, 0.2575000000000000067, 0.2600000000000000089, 0.2625000000000000111, 0.2650000000000000133, 0.2675000000000000155, 0.2700000000000000733, 0.2725000000000000200, 0.2750000000000000222, 0.2775000000000000244, 0.2800000000000000266, 0.2824999999999999734, 0.2849999999999999756, 0.2874999999999999778, 0.2899999999999999800, 0.2924999999999999822, 0.2949999999999999845, 0.2974999999999999867, 0.2999999999999999889, 0.3024999999999999911, 0.3049999999999999933, 0.3074999999999999956, 0.3099999999999999978, 0.3125000000000000000, 0.3150000000000000022, 0.3175000000000000044, 0.3200000000000000067, 0.3225000000000000089, 0.3250000000000000111, 0.3275000000000000133, 0.3300000000000000155, 0.3325000000000000178, 0.3350000000000000200, 0.3375000000000000222, 0.3400000000000000244, 0.3425000000000000266, 0.3449999999999999734, 0.3474999999999999756, 0.3499999999999999778, 0.3524999999999999800, 0.3549999999999999822, 0.3574999999999999845, 0.3599999999999999867, 0.3624999999999999889, 0.3649999999999999911, 0.3674999999999999933, 0.3699999999999999956, 0.3724999999999999978, 0.3750000000000000000, 0.3775000000000000022, 0.3800000000000000044, 0.3825000000000000067, 0.3850000000000000089, 0.3875000000000000111, 0.3900000000000000133, 0.3925000000000000155, 0.3950000000000000733, 0.3975000000000000200, 0.4000000000000000222, 0.4025000000000000244, 0.4050000000000000266, 0.4074999999999999734, 0.4099999999999999756, 0.4124999999999999778, 0.4149999999999999800, 0.4174999999999999822, 0.4199999999999999845, 0.4224999999999999867, 0.4249999999999999889, 0.4274999999999999911, 0.4299999999999999933, 0.4324999999999999956, 0.4349999999999999978, 0.4375000000000000000, 0.4400000000000000022, 0.4425000000000000044, 0.4450000000000000067, 0.4475000000000000089, 0.4500000000000000111, 0.4525000000000000133, 0.4550000000000000155, 0.4575000000000000178, 0.4600000000000000200, 0.4625000000000000222, 0.4650000000000000244, 0.4675000000000000266, 0.4699999999999999734, 0.4724999999999999756, 0.4749999999999999778, 0.4774999999999999800, 0.4799999999999999822, 0.4824999999999999845, 0.4849999999999999867, 0.4874999999999999889, 0.4899999999999999911, 0.4924999999999999933, 0.4949999999999999956, 0.4974999999999999978, 0.5000000000000000000, 0.5024999999999999467, 0.5050000000000000044, 0.5074999999999999512, 0.5100000000000000089, 0.5124999999999999556, 0.5150000000000000133, 0.5174999999999999600, 0.5200000000000000178, 0.5224999999999999645, 0.5250000000000000222, 0.5274999999999999689, 0.5300000000000000266, 0.5324999999999999734, 0.5350000000000000311, 0.5374999999999999778, 0.5400000000000000355, 0.5424999999999999822, 0.5450000000000000400, 0.5474999999999999867, 0.5500000000000000444, 0.5524999999999999911, 0.5550000000000000488, 0.5574999999999999956, 0.5600000000000000533, 0.5625000000000000000, 0.5650000000000000577, 0.5675000000000000044, 0.5699999999999999512, 0.5725000000000000089, 0.5749999999999999556, 0.5775000000000000133, 0.5799999999999999600, 0.5825000000000000178, 0.5849999999999999645, 0.5875000000000000222, 0.5899999999999999689, 0.5925000000000000266, 0.5949999999999999734, 0.5975000000000000311, 0.5999999999999999778, 0.6025000000000000355, 0.6049999999999999822, 0.6075000000000000400, 0.6099999999999999867, 0.6125000000000000444, 0.6149999999999999911, 0.6175000000000000488, 0.6199999999999999956, 0.6225000000000000533, 0.6250000000000000000, 0.6274999999999999467, 0.6300000000000000044, 0.6324999999999999512, 0.6350000000000000089, 0.6374999999999999556, 0.6400000000000000133, 0.6424999999999999600, 0.6450000000000000178, 0.6474999999999999645, 0.6500000000000000222, 0.6524999999999999689, 0.6550000000000000266, 0.6574999999999999734, 0.6600000000000000311, 0.6624999999999999778, 0.6650000000000000355, 0.6674999999999999822, 0.6700000000000000400, 0.6724999999999999867, 0.6750000000000000444, 0.6774999999999999911, 0.6800000000000000488, 0.6824999999999999956, 0.6850000000000000533, 0.6875000000000000000, 0.6899999999999999467, 0.6925000000000000044, 0.6949999999999999512, 0.6975000000000000089, 0.6999999999999999556, 0.7025000000000000133, 0.7049999999999999600, 0.7075000000000000178, 0.7099999999999999645, 0.7125000000000000222, 0.7149999999999999689, 0.7175000000000000266, 0.7199999999999999734, 0.7225000000000000311, 0.7249999999999999778, 0.7275000000000000355, 0.7299999999999999822, 0.7325000000000000400, 0.7349999999999999867, 0.7375000000000000444, 0.7399999999999999911, 0.7425000000000000488, 0.7449999999999999956, 0.7475000000000000533, 0.7500000000000000000, 0.7524999999999999467, 0.7550000000000000044, 0.7574999999999999512, 0.7600000000000000089, 0.7624999999999999556, 0.7650000000000000133, 0.7674999999999999600, 0.7700000000000000178, 0.7724999999999999645, 0.7750000000000000222, 0.7774999999999999689, 0.7800000000000000266, 0.7824999999999999734, 0.7850000000000000311, 0.7874999999999999778, 0.7900000000000000355, 0.7924999999999999822, 0.7950000000000000400, 0.7974999999999999867, 0.8000000000000000444, 0.8024999999999999911, 0.8050000000000000488, 0.8074999999999999956, 0.8100000000000000533, 0.8125000000000000000, 0.8150000000000000577, 0.8175000000000000044, 0.8199999999999999512, 0.8225000000000000089, 0.8249999999999999556, 0.8275000000000000133, 0.8299999999999999600, 0.8325000000000000178, 0.8349999999999999645, 0.8375000000000000222, 0.8399999999999999689, 0.8425000000000000266, 0.8449999999999999734, 0.8475000000000000311, 0.8499999999999999778, 0.8525000000000000355, 0.8549999999999999822, 0.8575000000000000400, 0.8599999999999999867, 0.8625000000000000444, 0.8649999999999999911, 0.8675000000000000488, 0.8699999999999999956, 0.8725000000000000533, 0.8750000000000000000, 0.8774999999999999467, 0.8800000000000000044, 0.8824999999999999512, 0.8850000000000000089, 0.8874999999999999556, 0.8900000000000000133, 0.8924999999999999600, 0.8950000000000000178, 0.8974999999999999645, 0.9000000000000000222, 0.9024999999999999689, 0.9050000000000000266, 0.9074999999999999734, 0.9100000000000000311, 0.9124999999999999778, 0.9150000000000000355, 0.9174999999999999822, 0.9200000000000000400, 0.9224999999999999867, 0.9250000000000000444, 0.9274999999999999911, 0.9300000000000000488, 0.9324999999999999956, 0.9350000000000000533, 0.9375000000000000000, 0.9399999999999999467, 0.9425000000000000044, 0.9449999999999999512, 0.9475000000000000089, 0.9499999999999999556, 0.9525000000000000133, 0.9549999999999999600, 0.9575000000000000178, 0.9599999999999999645, 0.9625000000000000222, 0.9649999999999999689, 0.9675000000000000266, 0.9699999999999999734, 0.9725000000000000311, 0.9749999999999999778, 0.9775000000000000355, 0.9799999999999999822, 0.9825000000000000400, 0.9849999999999999867, 0.9875000000000000444, 0.9899999999999999911, 0.9925000000000000488, 0.9949999999999999956, 0.9975000000000000533 ),
 .UNSPECIFIED. ) 
 CURVE ( )  GEOMETRIC_REPRESENTATION_ITEM ( )  RATIONAL_B_SPLINE_CURVE ( ( 0.9619397662556429252, 0.9619397670556029123, 1.000000000000000000, 0.9238795325112869605, 1.000000000000000000, 0.9238795325112869605, 1.000000000000000000, 0.9238795325112869605, 1.000000000000000000, 0.9238795325112869605, 1.000000000000000000, 0.9238795325112869605, 1.000000000000000000, 0.9238795325112869605, 1.000000000000000000, 0.9238795325112869605, 1.000000000000000000, 0.9238795325112869605, 1.000000000000000000, 0.9238795325112869605, 1.000000000000000000, 0.9238795325112869605, 1.000000000000000000, 0.9238795325112869605, 1.000000000000000000, 0.9238795325112869605, 1.000000000000000000, 0.9238795325112869605, 1.000000000000000000, 0.9238795325112869605, 1.000000000000000000, 0.9238795325112869605, 1.000000000000000000, 0.9238795325112869605, 1.000000000000000000, 0.9238795325112869605, 1.000000000000000000, 0.9238795325112869605, 1.000000000000000000, 0.9238795325112869605, 1.000000000000000000, 0.9238795325112869605, 1.000000000000000000, 0.9238795325112869605, 1.000000000000000000, 0.9238795325112869605, 1.000000000000000000, 0.9238795325112869605, 1.000000000000000000, 0.9238795325112869605, 1.000000000000000000, 0.9238795325112869605, 1.000000000000000000, 0.9238795325112869605, 1.000000000000000000, 0.9238795325112869605, 1.000000000000000000, 0.9238795325112869605, 1.000000000000000000, 0.9238795325112869605, 1.000000000000000000, 0.9238795325112869605, 1.000000000000000000, 0.9238795325112869605, 1.000000000000000000, 0.9238795325112869605, 1.000000000000000000, 0.9238795325112869605, 1.000000000000000000, 0.9238795325112869605, 1.000000000000000000, 0.9238795325112869605, 1.000000000000000000, 0.9238795325112869605, 1.000000000000000000, 0.9238795325112869605, 1.000000000000000000, 0.9238795325112869605, 1.000000000000000000, 0.9238795325112869605, 1.000000000000000000, 0.9238795325112869605, 1.000000000000000000, 0.9238795325112869605, 1.000000000000000000, 0.9238795325112869605, 1.000000000000000000, 0.9238795325112869605, 1.000000000000000000, 0.9238795325112869605, 1.000000000000000000, 0.9238795325112869605, 1.000000000000000000, 0.9238795325112869605, 1.000000000000000000, 0.9238795325112869605, 1.000000000000000000, 0.9238795325112869605, 1.000000000000000000, 0.9238795325112869605, 1.000000000000000000, 0.9238795325112869605, 1.000000000000000000, 0.9238795325112869605, 1.000000000000000000, 0.9238795325112869605, 1.000000000000000000, 0.9238795325112869605, 1.000000000000000000, 0.9238795325112869605, 1.000000000000000000, 0.9238795325112869605, 1.000000000000000000, 0.9238795325112869605, 1.000000000000000000, 0.9238795325112869605, 1.000000000000000000, 0.9238795325112869605, 1.000000000000000000, 0.9238795325112869605, 1.000000000000000000, 0.9238795325112869605, 1.000000000000000000, 0.9238795325112869605, 1.000000000000000000, 0.9238795325112869605, 1.000000000000000000, 0.9238795325112869605, 1.000000000000000000, 0.9238795325112869605, 1.000000000000000000, 0.9238795325112869605, 1.000000000000000000, 0.9238795325112869605, 1.000000000000000000, 0.9238795325112869605, 1.000000000000000000, 0.9238795325112869605, 1.000000000000000000, 0.9238795325112869605, 1.000000000000000000, 0.9238795325112869605, 1.000000000000000000, 0.9238795325112869605, 1.000000000000000000, 0.9238795325112869605, 1.000000000000000000, 0.9238795325112869605, 1.000000000000000000, 0.9238795325112869605, 1.000000000000000000, 0.9238795325112869605, 1.000000000000000000, 0.9238795325112869605, 1.000000000000000000, 0.9238795325112869605, 1.000000000000000000, 0.9238795325112869605, 1.000000000000000000, 0.9238795325112869605, 1.000000000000000000, 0.9238795325112869605, 1.000000000000000000, 0.9238795325112869605, 1.000000000000000000, 0.9238795325112869605, 1.000000000000000000, 0.9238795325112869605, 1.000000000000000000, 0.9238795325112869605, 1.000000000000000000, 0.9238795325112869605, 1.000000000000000000, 0.9238795325112869605, 1.000000000000000000, 0.9238795325112869605, 1.000000000000000000, 0.9238795325112869605, 1.000000000000000000, 0.9238795325112869605, 1.000000000000000000, 0.9238795325112869605, 1.000000000000000000, 0.9238795325112869605, 1.000000000000000000, 0.9238795325112869605, 1.000000000000000000, 0.9238795325112869605, 1.000000000000000000, 0.9238795325112869605, 1.000000000000000000, 0.9238795325112869605, 1.000000000000000000, 0.9238795325112869605, 1.000000000000000000, 0.9238795325112869605, 1.000000000000000000, 0.9238795325112869605, 1.000000000000000000, 0.9238795325112869605, 1.000000000000000000, 0.9238795325112869605, 1.000000000000000000, 0.9238795325112869605, 1.000000000000000000, 0.9238795325112869605, 1.000000000000000000, 0.9238795325112869605, 1.000000000000000000, 0.9238795325112869605, 1.000000000000000000, 0.9238795325112869605, 1.000000000000000000, 0.9238795325112869605, 1.000000000000000000, 0.9238795325112869605, 1.000000000000000000, 0.9238795325112869605, 1.000000000000000000, 0.9238795325112869605, 1.000000000000000000, 0.9238795325112869605, 1.000000000000000000, 0.9238795325112869605, 1.000000000000000000, 0.9238795325112869605, 1.000000000000000000, 0.9238795325112869605, 1.000000000000000000, 0.9238795325112869605, 1.000000000000000000, 0.9238795325112869605, 1.000000000000000000, 0.9238795325112869605, 1.000000000000000000, 0.9238795325112869605, 1.000000000000000000, 0.9238795325112869605, 1.000000000000000000, 0.9238795325112869605, 1.000000000000000000, 0.9238795325112869605, 1.000000000000000000, 0.9238795325112869605, 1.000000000000000000, 0.9238795325112869605, 1.000000000000000000, 0.9238795325112869605, 1.000000000000000000, 0.9238795325112869605, 1.000000000000000000, 0.9238795325112869605, 1.000000000000000000, 0.9238795325112869605, 1.000000000000000000, 0.9238795325112869605, 1.000000000000000000, 0.9238795325112869605, 1.000000000000000000, 0.9238795325112869605, 1.000000000000000000, 0.9238795325112869605, 1.000000000000000000, 0.9238795325112869605, 1.000000000000000000, 0.9238795325112869605, 1.000000000000000000, 0.9238795325112869605, 1.000000000000000000, 0.9238795325112869605, 1.000000000000000000, 0.9238795325112869605, 1.000000000000000000, 0.9238795325112869605, 1.000000000000000000, 0.9238795325112869605, 1.000000000000000000, 0.9238795325112869605, 1.000000000000000000, 0.9238795325112869605, 1.000000000000000000, 0.9238795325112869605, 1.000000000000000000, 0.9238795325112869605, 1.000000000000000000, 0.9238795325112869605, 1.000000000000000000, 0.9238795325112869605, 1.000000000000000000, 0.9238795325112869605, 1.000000000000000000, 0.9238795325112869605, 1.000000000000000000, 0.9238795325112869605, 1.000000000000000000, 0.9238795325112869605, 1.000000000000000000, 0.9238795325112869605, 1.000000000000000000, 0.9238795325112869605, 1.000000000000000000, 0.9238795325112869605, 1.000000000000000000, 0.9238795325112869605, 1.000000000000000000, 0.9238795325112869605, 1.000000000000000000, 0.9238795325112869605, 1.000000000000000000, 0.9238795325112869605, 1.000000000000000000, 0.9238795325112869605, 1.000000000000000000, 0.9238795325112869605, 1.000000000000000000, 0.9238795325112869605, 1.000000000000000000, 0.9238795325112869605, 1.000000000000000000, 0.9238795325112869605, 1.000000000000000000, 0.9238795325112869605, 1.000000000000000000, 0.9238795325112869605, 1.000000000000000000, 0.9238795325112869605, 1.000000000000000000, 0.9238795325112869605, 1.000000000000000000, 0.9238795325112869605, 1.000000000000000000, 0.9238795325112869605, 1.000000000000000000, 0.9238795325112869605, 1.000000000000000000, 0.9238795325112869605, 1.000000000000000000, 0.9238795325112869605, 1.000000000000000000, 0.9238795325112869605, 1.000000000000000000, 0.9238795325112869605, 1.000000000000000000, 0.9238795325112869605, 1.000000000000000000, 0.9238795325112869605, 1.000000000000000000, 0.9238795325112869605, 1.000000000000000000, 0.9238795325112869605, 1.000000000000000000, 0.9238795325112869605, 1.000000000000000000, 0.9238795325112869605, 1.000000000000000000, 0.9238795325112869605, 1.000000000000000000, 0.9238795325112869605, 1.000000000000000000, 0.9238795325112869605, 1.000000000000000000, 0.9238795325112869605, 1.000000000000000000, 0.9238795325112869605, 1.000000000000000000, 0.9238795325112869605, 1.000000000000000000, 0.9238795325112869605, 1.000000000000000000, 0.9238795325112869605, 1.000000000000000000, 0.9238795325112869605, 1.000000000000000000, 0.9238795325112869605, 1.000000000000000000, 0.9238795325112869605, 1.000000000000000000, 0.9238795325112869605, 1.000000000000000000, 0.9238795325112869605, 1.000000000000000000, 0.9238795325112869605, 1.000000000000000000, 0.9238795325112869605, 1.000000000000000000, 0.9238795325112869605, 1.000000000000000000, 0.9238795325112869605, 1.000000000000000000, 0.9238795325112869605, 1.000000000000000000, 0.9238795325112869605, 1.000000000000000000, 0.9238795325112869605, 1.000000000000000000, 0.9238795325112869605, 1.000000000000000000, 0.9238795325112869605, 1.000000000000000000, 0.9238795325112869605, 1.000000000000000000, 0.9238795325112869605, 1.000000000000000000, 0.9238795325112869605, 1.000000000000000000, 0.9238795325112869605, 1.000000000000000000, 0.9238795325112869605, 1.000000000000000000, 0.9238795325112869605, 1.000000000000000000, 0.9238795325112869605, 1.000000000000000000, 0.9238795325112869605, 1.000000000000000000, 0.9238795325112869605, 1.000000000000000000, 0.9238795325112869605, 1.000000000000000000, 0.9238795325112869605, 1.000000000000000000, 0.9238795325112869605, 1.000000000000000000, 0.9238795325112869605, 1.000000000000000000, 0.9238795325112869605, 1.000000000000000000, 0.9238795325112869605, 1.000000000000000000, 0.9238795325112869605, 1.000000000000000000, 0.9238795325112869605, 1.000000000000000000, 0.9238795325112869605, 1.000000000000000000, 0.9238795325112869605, 1.000000000000000000, 0.9238795325112869605, 1.000000000000000000, 0.9238795325112869605, 1.000000000000000000, 0.9238795325112869605, 1.000000000000000000, 0.9238795325112869605, 1.000000000000000000, 0.9238795325112869605, 1.000000000000000000, 0.9238795325112869605, 1.000000000000000000, 0.9238795325112869605, 1.000000000000000000, 0.9238795325112869605, 1.000000000000000000, 0.9238795325112869605, 1.000000000000000000, 0.9238795325112869605, 1.000000000000000000, 0.9238795325112869605, 1.000000000000000000, 0.9238795325112869605, 1.000000000000000000, 0.9238795325112869605, 1.000000000000000000, 0.9238795325112869605, 1.000000000000000000, 0.9238795325112869605, 1.000000000000000000, 0.9238795325112869605, 1.000000000000000000, 0.9238795325112869605, 1.000000000000000000, 0.9238795325112869605, 1.000000000000000000, 0.9238795325112869605, 1.000000000000000000, 0.9238795325112869605, 1.000000000000000000, 0.9238795325112869605, 1.000000000000000000, 0.9238795325112869605, 1.000000000000000000, 0.9238795325112869605, 1.000000000000000000, 0.9238795325112869605, 1.000000000000000000, 0.9238795325112869605, 1.000000000000000000, 0.9238795325112869605, 1.000000000000000000, 0.9238795325112869605, 1.000000000000000000, 0.9238795325112869605, 1.000000000000000000, 0.9238795325112869605, 1.000000000000000000, 0.9238795325112869605, 1.000000000000000000, 0.9238795325112869605, 1.000000000000000000, 0.9238795325112869605, 1.000000000000000000, 0.9238795325112869605, 1.000000000000000000, 0.9238795325112869605, 1.000000000000000000, 0.9238795325112869605, 1.000000000000000000, 0.9238795325112869605, 1.000000000000000000, 0.9238795325112869605, 1.000000000000000000, 0.9238795325112869605, 1.000000000000000000, 0.9238795325112869605, 1.000000000000000000, 0.9238795325112869605, 1.000000000000000000, 0.9238795325112869605, 1.000000000000000000, 0.9238795325112869605, 1.000000000000000000, 0.9238795325112869605, 1.000000000000000000, 0.9238795325112869605, 1.000000000000000000, 0.9238795325112869605, 1.000000000000000000, 0.9238795325112869605, 1.000000000000000000, 0.9238795325112869605, 1.000000000000000000, 0.9238795325112869605, 1.000000000000000000, 0.9238795325112869605, 1.000000000000000000, 0.9238795325112869605, 1.000000000000000000, 0.9238795325112869605, 1.000000000000000000, 0.9238795325112869605, 1.000000000000000000, 0.9238795325112869605, 1.000000000000000000, 0.9238795325112869605, 1.000000000000000000, 0.9238795325112869605, 1.000000000000000000, 0.9238795325112869605, 1.000000000000000000, 0.9238795325112869605, 1.000000000000000000, 0.9238795325112869605, 1.000000000000000000, 0.9238795325112869605, 1.000000000000000000, 0.9238795325112869605, 1.000000000000000000, 0.9238795325112869605, 1.000000000000000000, 0.9238795325112869605, 1.000000000000000000, 0.9238795325112869605, 1.000000000000000000, 0.9238795325112869605, 1.000000000000000000, 0.9238795325112869605, 1.000000000000000000, 0.9238795325112869605, 1.000000000000000000, 0.9238795325112869605, 1.000000000000000000, 0.9238795325112869605, 1.000000000000000000, 0.9238795325112869605, 1.000000000000000000, 0.9238795325112869605, 1.000000000000000000, 0.9238795325112869605, 1.000000000000000000, 0.9238795325112869605, 1.000000000000000000, 0.9238795325112869605, 1.000000000000000000, 0.9238795325112869605, 1.000000000000000000, 0.9238795325112869605, 1.000000000000000000, 0.9238795325112869605, 1.000000000000000000, 0.9238795325112869605, 1.000000000000000000, 0.9238795325112869605, 1.000000000000000000, 0.9238795325112869605, 1.000000000000000000, 0.9238795325112869605, 1.000000000000000000, 0.9238795325112869605, 1.000000000000000000, 0.9238795325112869605, 1.000000000000000000, 0.9238795325112869605, 1.000000000000000000, 0.9238795325112869605, 1.000000000000000000, 0.9238795325112869605, 1.000000000000000000, 0.9238795325112869605, 1.000000000000000000, 0.9238795325112869605, 1.000000000000000000, 0.9238795325112869605, 1.000000000000000000, 0.9238795325112869605, 1.000000000000000000, 0.9238795325112869605, 1.000000000000000000, 0.9238795325112869605, 1.000000000000000000, 0.9238795325112869605, 1.000000000000000000, 0.9238795325112869605, 1.000000000000000000, 0.9238795325112869605, 1.000000000000000000, 0.9238795325112869605, 1.000000000000000000, 0.9238795325112869605, 1.000000000000000000, 0.9238795325112869605, 1.000000000000000000, 0.9238795325112869605, 1.000000000000000000, 0.9238795325112869605, 1.000000000000000000, 0.9238795325112869605, 1.000000000000000000, 0.9238795325112869605, 1.000000000000000000, 0.9238795325112869605, 1.000000000000000000, 0.9238795325112869605, 1.000000000000000000, 0.9238795325112869605, 1.000000000000000000, 0.9238795325112869605, 1.000000000000000000, 0.9238795325112869605, 1.000000000000000000, 0.9238795325112869605, 1.000000000000000000, 0.9238795325112869605, 1.000000000000000000, 0.9238795325112869605, 1.000000000000000000, 0.9238795325112869605, 1.000000000000000000, 0.9238795325112869605, 1.000000000000000000, 0.9238795325112869605, 1.000000000000000000, 0.9238795325112869605, 1.000000000000000000, 0.9238795325112869605, 1.000000000000000000, 0.9238795325112869605, 1.000000000000000000, 0.9238795325112869605, 1.000000000000000000, 0.9238795325112869605, 1.000000000000000000, 0.9238795325112869605, 1.000000000000000000, 0.9238795325112869605, 1.000000000000000000, 0.9238795325112869605, 1.000000000000000000, 0.9238795325112869605, 1.000000000000000000, 0.9238795325112869605, 1.000000000000000000, 0.9238795325112869605, 1.000000000000000000, 0.9238795325112869605, 1.000000000000000000, 0.9238795325112869605, 1.000000000000000000, 0.9238795325112869605, 1.000000000000000000, 0.9238795325112869605, 1.000000000000000000, 0.9238795325112869605, 1.000000000000000000, 0.9238795325112869605, 1.000000000000000000, 0.9238795325112869605, 1.000000000000000000, 0.9238795325112869605, 1.000000000000000000, 0.9238795325112869605, 1.000000000000000000, 0.9238795325112869605, 1.000000000000000000, 0.9238795325112869605, 1.000000000000000000, 0.9238795325112869605, 1.000000000000000000, 0.9238795325112869605, 1.000000000000000000, 0.9238795325112869605, 1.000000000000000000, 0.9238795325112869605, 1.000000000000000000, 0.9238795325112869605, 1.000000000000000000, 0.9238795325112869605, 1.000000000000000000, 0.9238795325112869605, 1.000000000000000000, 0.9238795325112869605, 1.000000000000000000, 0.9238795325112869605, 1.000000000000000000, 0.9238795325112869605, 1.000000000000000000, 0.9238795325112869605, 1.000000000000000000, 0.9238795325112869605, 1.000000000000000000, 0.9238795325112869605, 1.000000000000000000, 0.9238795325112869605, 1.000000000000000000, 0.9238795325112869605, 1.000000000000000000, 0.9238795325112869605, 1.000000000000000000, 0.9238795325112869605, 1.000000000000000000, 0.9238795325112869605, 1.000000000000000000, 0.9238795325112869605, 1.000000000000000000, 0.9238795325112869605, 1.000000000000000000, 0.9238795325112869605, 1.000000000000000000, 0.9238795325112869605, 1.000000000000000000, 0.9238795325112869605, 1.000000000000000000, 0.9238795325112869605, 1.000000000000000000, 0.9238795325112869605, 1.000000000000000000, 0.9238795325112869605, 1.000000000000000000, 0.9238795325112869605, 1.000000000000000000, 0.9238795325112869605, 1.000000000000000000, 0.9238795325112869605, 1.000000000000000000, 0.9238795325112869605, 1.000000000000000000, 0.9238795325112869605, 1.000000000000000000, 0.9238795325112869605, 1.000000000000000000, 0.9238795325112869605, 1.000000000000000000, 0.9238795325112869605, 1.000000000000000000, 0.9238795325112869605, 1.000000000000000000, 0.9238795325112869605, 1.000000000000000000, 0.9238795325112869605, 1.000000000000000000, 0.9238795325112869605, 1.000000000000000000, 0.9238795325112869605, 1.000000000000000000, 0.9238795325112869605, 1.000000000000000000, 0.9238795325112869605, 1.000000000000000000, 0.9238795325112869605, 1.000000000000000000, 0.9238795325112869605, 1.000000000000000000, 0.9238795325112869605, 1.000000000000000000, 0.9238795325112869605, 1.000000000000000000 ) ) 
 REPRESENTATION_ITEM ( '' )  ) ;
#3329 = CARTESIAN_POINT ( 'NONE',  ( -0.9500414927467378812, -0.1787899950787401604, 0.1328740156942679607 ) ) ;
#3330 = LINE ( 'NONE', #32591, #23506 ) ;
#3331 = VERTEX_POINT ( 'NONE', #7823 ) ;
#3332 = VERTEX_POINT ( 'NONE', #15512 ) ;
#3333 = ORIENTED_EDGE ( 'NONE', *, *, #7261, .F. ) ;
#3334 = ( BOUNDED_CURVE ( )  B_SPLINE_CURVE ( 2, ( #34876, #16652, #1301, #31280, #41296, #4900, #15959, #17108, #39139 ),
 .UNSPECIFIED., .F., .F. ) 
 B_SPLINE_CURVE_WITH_KNOTS ( ( 3, 2, 2, 2, 3 ),
 ( 0.2899999999999999800, 0.2924999999999999822, 0.2949999999999999845, 0.2974999999999999867, 0.2999999999999999889 ),
 .UNSPECIFIED. ) 
 CURVE ( )  GEOMETRIC_REPRESENTATION_ITEM ( )  RATIONAL_B_SPLINE_CURVE ( ( 1.000000000000000000, 0.9238795325112869605, 1.000000000000000000, 0.9238795325112869605, 1.000000000000000000, 0.9238795325112869605, 1.000000000000000000, 0.9238795325112869605, 1.000000000000000000 ) ) 
 REPRESENTATION_ITEM ( '' )  ) ;
#3335 = CARTESIAN_POINT ( 'NONE',  ( -0.9500414927467377701, 0.1787899950787401604, 1.451771653489543290 ) ) ;
#3336 = VERTEX_POINT ( 'NONE', #4931 ) ;
#3337 = CARTESIAN_POINT ( 'NONE',  ( 3.284318927891251994E-17, -1.137303149552535420, 0.1787899950787401882 ) ) ;
#3338 = ADVANCED_FACE ( 'NONE', ( #1812 ), #19787, .F. ) ;
#3339 = CARTESIAN_POINT ( 'NONE',  ( -0.1264236179284866091, -1.343996062938362268, -0.1264236179284866091 ) ) ;
#3340 = DIRECTION ( 'NONE',  ( 0.000000000000000000, 0.000000000000000000, -1.000000000000000000 ) ) ;
#3341 = CARTESIAN_POINT ( 'NONE',  ( -0.1270800023317771588, -0.5965005024964310509, -0.1270800023317771588 ) ) ;
#3342 = CARTESIAN_POINT ( 'NONE',  ( 0.7185039370078739607, 0.000000000000000000, 4.498031496062992574 ) ) ;
#3343 = CARTESIAN_POINT ( 'NONE',  ( -0.7185039370078746268, -0.06523048226347956391, 0.8882874014672753615 ) ) ;
#3344 = CARTESIAN_POINT ( 'NONE',  ( -0.06523048226347956391, -0.1136811023622046890, -0.1574803149606300301 ) ) ;
#3345 = CARTESIAN_POINT ( 'NONE',  ( 0.9873396505805591694, -0.1113553986120547346, 1.884842519577511810 ) ) ;
#3346 = ORIENTED_EDGE ( 'NONE', *, *, #18537, .F. ) ;
#3347 = DIRECTION ( 'NONE',  ( 0.000000000000000000, 0.000000000000000000, 1.000000000000000000 ) ) ;
#3348 = CARTESIAN_POINT ( 'NONE',  ( 0.8759842519685039353, 0.1574803149606299191, 0.7677165354330708347 ) ) ;
#3349 = CARTESIAN_POINT ( 'NONE',  ( -0.8759842519685039353, 0.1574803149606299191, 1.240157480314960647 ) ) ;
#3351 = CARTESIAN_POINT ( 'NONE',  ( 1.033464566929133799, 0.000000000000000000, 1.505905511811023612 ) ) ;
#3350 = CARTESIAN_POINT ( 'NONE',  ( -0.7185039370078746268, -0.06523048226347956391, 0.4650590551181104093 ) ) ;
#3352 = CARTESIAN_POINT ( 'NONE',  ( 0.8107537697050253289, 0.1574803149606300301, 0.1304133857192446289 ) ) ;
#3353 = EDGE_LOOP ( 'NONE', ( #10961, #43358, #12842, #5629 ) ) ;
#3354 = CARTESIAN_POINT ( 'NONE',  ( 0.8759842519685039353, 0.000000000000000000, 1.995570866087968520 ) ) ;
#3355 = CARTESIAN_POINT ( 'NONE',  ( 0.1113553986120547346, -1.567913385719246211, -0.1113553986120547346 ) ) ;
#3356 = CARTESIAN_POINT ( 'NONE',  ( 0.1264236179284866091, -0.7386811023084409733, 0.1264236179284866091 ) ) ;
#3357 = CARTESIAN_POINT ( 'NONE',  ( -1.033464566929134687, -0.06523048226347956391, 0.1550196849318430659 ) ) ;
#3358 = CARTESIAN_POINT ( 'NONE',  ( 0.1574803149606300301, -1.112696850393701142, 0.06523048226347956391 ) ) ;
#3359 = CARTESIAN_POINT ( 'NONE',  ( 0.9412147342319837628, -0.1574803149606297803, 1.016240157372787722 ) ) ;
#3360 = CARTESIAN_POINT ( 'NONE',  ( 0.7646288533564489232, 0.1113553986120547346, 0.5364173228346457156 ) ) ;
#3361 = EDGE_CURVE ( 'NONE', #37199, #1915, #34421, .T. ) ;
#3362 = CARTESIAN_POINT ( 'NONE',  ( -1.002407869896990045, -0.1264236179284866091, 0.4109251967966299213 ) ) ;
#3363 = ORIENTED_EDGE ( 'NONE', *, *, #21846, .F. ) ;
#3364 = ORIENTED_EDGE ( 'NONE', *, *, #37271, .F. ) ;
#3365 = STYLED_ITEM ( 'NONE', ( #18942 ), #4462 ) ;
#3366 = CARTESIAN_POINT ( 'NONE',  ( -1.054774247047244540, -0.07405724077823318263, 1.560039370024977057 ) ) ;
#3367 = ORIENTED_EDGE ( 'NONE', *, *, #44807, .F. ) ;
#3368 = CARTESIAN_POINT ( 'NONE',  ( 1.054774247047244096, 0.000000000000000000, 1.483759842465921075 ) ) ;
#3369 = ORIENTED_EDGE ( 'NONE', *, *, #29054, .T. ) ;
#3370 = CARTESIAN_POINT ( 'NONE',  ( -0.06523048226347956391, -1.284940944774363158, -0.1574803149606300301 ) ) ;
#3371 = CARTESIAN_POINT ( 'NONE',  ( -0.6971942568897626646, 0.07405724077823318263, 0.8316929133320636325 ) ) ;
#3372 = CARTESIAN_POINT ( 'NONE',  ( 1.002407869896990045, 0.1264236179284866091, 0.2288385826234019815 ) ) ;
#3373 = CARTESIAN_POINT ( 'NONE',  ( -0.7185039370078746268, 0.06523048226347956391, 0.2632874015748031260 ) ) ;
#3374 = CARTESIAN_POINT ( 'NONE',  ( 1.002407869896990045, -0.1264236179284866091, 0.7701771653005669016 ) ) ;
#3375 = CARTESIAN_POINT ( 'NONE',  ( -0.8759842519685039353, 0.1787899950787401882, 0.6619094487651338010 ) ) ;
#3376 = EDGE_CURVE ( 'NONE', #7349, #3083, #10152, .T. ) ;
#3377 = LINE ( 'NONE', #36680, #16947 ) ;
#3378 = CARTESIAN_POINT ( 'NONE',  ( 0.9412147342319837628, -0.1574803149606297803, 1.144192913385827737 ) ) ;
#3379 = CARTESIAN_POINT ( 'NONE',  ( -0.1574803149606300301, -0.2170275589475910150, -0.06523048226347956391 ) ) ;
#3380 = CARTESIAN_POINT ( 'NONE',  ( -0.9873396505805591694, -0.1113553986120547346, 1.845472440837354178 ) ) ;
#3381 = VERTEX_POINT ( 'NONE', #37531 ) ;
#3382 = CARTESIAN_POINT ( 'NONE',  ( -0.1586641775163213364, 1.975221432870719385, -0.9622519263226598785 ) ) ;
#3383 = CARTESIAN_POINT ( 'NONE',  ( -0.8759842519685039353, 0.1574803149606299191, 0.4133858267716535861 ) ) ;
#3384 = CARTESIAN_POINT ( 'NONE',  ( 0.9500414927467377701, -0.1787899950787401604, 1.437007873961985593 ) ) ;
#3385 = PLANE ( 'NONE',  #24870 ) ;
#3386 = CARTESIAN_POINT ( 'NONE',  ( 0.1787899950787401604, -1.765871999725300512, -0.07405724077823318263 ) ) ;
#3387 = VERTEX_POINT ( 'NONE', #41095 ) ;
#3388 = ( NAMED_UNIT ( * ) SI_UNIT ( $, .STERADIAN. ) SOLID_ANGLE_UNIT ( ) ) ;
#3389 = ORIENTED_EDGE ( 'NONE', *, *, #24381, .T. ) ;
#3390 = DIRECTION ( 'NONE',  ( -1.000000000000000000, -6.679788269418529283E-17, 0.000000000000000000 ) ) ;
#3391 = CARTESIAN_POINT ( 'NONE',  ( -0.1264236179284866091, -0.9502952755367874982, -0.1264236179284866091 ) ) ;
#3392 = DIRECTION ( 'NONE',  ( -1.000000000000000000, 0.000000000000000000, 0.000000000000000000 ) ) ;
#3393 = CARTESIAN_POINT ( 'NONE',  ( 0.1638905441107560423, -0.1612682469887707637, -2.622724073162300381E-07 ) ) ;
#3394 = CARTESIAN_POINT ( 'NONE',  ( 0.7495606340400177148, -0.1264236179284866091, 0.3223425196312759144 ) ) ;
#3395 = VECTOR ( 'NONE', #12019, 39.37007874015748143 ) ;
#3396 = CARTESIAN_POINT ( 'NONE',  ( 0.1270800023317771588, -0.1732721560397383898, -0.1270800023317771588 ) ) ;
#3397 = CARTESIAN_POINT ( 'NONE',  ( -0.1787899950787401604, -0.09756491311112856779, -0.07405724077823318263 ) ) ;
#3398 = CARTESIAN_POINT ( 'NONE',  ( 0.07405724077823318263, -0.2883858267178899260, -0.1787899950787401604 ) ) ;
#3399 = CARTESIAN_POINT ( 'NONE',  ( -0.1787899950787401882, -0.08415354325332302654, 0.000000000000000000 ) ) ;
#3400 = CARTESIAN_POINT ( 'NONE',  ( 0.2471922891335101569, -0.07779967023291604888, -0.07764737426208698223 ) ) ;
#3401 = CARTESIAN_POINT ( 'NONE',  ( 0.8019270111902717657, 0.1787899950787401604, 0.6643700786863951935 ) ) ;
#3402 = CARTESIAN_POINT ( 'NONE',  ( -1.002407869896990045, -0.1264236179284866091, 0.9670275590013542866 ) ) ;
#3404 = CARTESIAN_POINT ( 'NONE',  ( 0.1235961452251413406, -0.09842519685039370636, 0.2140748031496062798 ) ) ;
#3403 = CARTESIAN_POINT ( 'NONE',  ( -1.004065995148841539, 0.1041443272423887983, 0.03937007874015843734 ) ) ;
#3405 = CARTESIAN_POINT ( 'NONE',  ( -0.07444174185955065859, -1.725929636354700536, 0.1797182628040039087 ) ) ;
#3406 = CARTESIAN_POINT ( 'NONE',  ( 0.1787899950787401604, -0.4507874015210400209, -0.07405724077823318263 ) ) ;
#3407 = CARTESIAN_POINT ( 'NONE',  ( 1.033464566929133799, 0.000000000000000000, 1.702755905511810885 ) ) ;
#3408 = CARTESIAN_POINT ( 'NONE',  ( 1.054774247047244096, 0.000000000000000000, 1.719980314906866203 ) ) ;
#3410 = DIRECTION ( 'NONE',  ( 0.000000000000000000, 0.000000000000000000, 1.000000000000000000 ) ) ;
#3409 = CARTESIAN_POINT ( 'NONE',  ( 1.033464566929133799, 0.000000000000000000, 0.6299212597349921339 ) ) ;
#3411 = EDGE_CURVE ( 'NONE', #20105, #45765, #4689, .T. ) ;
#3412 = VERTEX_POINT ( 'NONE', #15752 ) ;
#3413 = DIRECTION ( 'NONE',  ( 0.000000000000000000, 0.000000000000000000, -1.000000000000000000 ) ) ;
#3414 = CARTESIAN_POINT ( 'NONE',  ( 0.7646288533564489232, -0.1113553986120547346, 1.323818897530267602 ) ) ;
#3415 = CARTESIAN_POINT ( 'NONE',  ( -0.07405724077823318263, -0.07677165348954355373, 0.1787899950787401604 ) ) ;
#3416 = CARTESIAN_POINT ( 'NONE',  ( -0.6971942568897626646, -0.07405724077823297447, 0.4429133857730075952 ) ) ;
#3417 = CARTESIAN_POINT ( 'NONE',  ( 0.1787899950787401882, -1.043799212544661348, -2.189545951927503898E-17 ) ) ;
#3418 = CARTESIAN_POINT ( 'NONE',  ( 0.8759842519685039353, 0.000000000000000000, 4.498031496062992574 ) ) ;
#3419 = CARTESIAN_POINT ( 'NONE',  ( 1.033464566929133799, 0.000000000000000000, 1.102362204616881947 ) ) ;
#3420 = EDGE_CURVE ( 'NONE', #11324, #20929, #5400, .T. ) ;
#3421 = CARTESIAN_POINT ( 'NONE',  ( -0.9500414927467378812, -0.1787899950787401604, 1.628937007820252303 ) ) ;
#3422 = ORIENTED_EDGE ( 'NONE', *, *, #18617, .F. ) ;
#3423 = AXIS2_PLACEMENT_3D ( 'NONE', #33122, #6972, #40258 ) ;
#3424 = CARTESIAN_POINT ( 'NONE',  ( -0.7495606340400177148, -0.1264236179284866091, 1.193405511757259951 ) ) ;
#3425 = CARTESIAN_POINT ( 'NONE',  ( 0.8759842519685039353, -0.1574803149606299191, 0.4330708661417322913 ) ) ;
#3426 = CARTESIAN_POINT ( 'NONE',  ( 1.002407869896990045, -0.1264236179284866091, 1.163877952702141672 ) ) ;
#3427 = CONICAL_SURFACE ( 'NONE', #33287, 0.09842519685039370636, 0.9599310885968824758 ) ;
#3428 = CARTESIAN_POINT ( 'NONE',  ( -1.033464566929134687, -0.06523048226347956391, 0.6668307085538908163 ) ) ;
#3429 = CARTESIAN_POINT ( 'NONE',  ( 0.7495606340400177148, -0.1264236179284866091, 1.897145669237574772 ) ) ;
#3430 = CARTESIAN_POINT ( 'NONE',  ( -0.8759842519685039353, -0.1574803149606299191, 0.5905511811023621549 ) ) ;
#3431 = CARTESIAN_POINT ( 'NONE',  ( -0.6971942568897626646, 0.07405724077823318263, 0.8267716534895444003 ) ) ;
#3432 = DIRECTION ( 'NONE',  ( 0.000000000000000000, -0.6156614753256597350, -0.7880107536067207930 ) ) ;
#3433 = CARTESIAN_POINT ( 'NONE',  ( 1.054774247047244540, -0.07405724077823318263, 0.3395669290800949480 ) ) ;
#3434 = CARTESIAN_POINT ( 'NONE',  ( -1.002407869896990045, -0.1264236179284866091, 0.2140748030958428971 ) ) ;
#3435 = PRODUCT_DEFINITION_CONTEXT ( 'detailed design', #30329, 'design' ) ;
#3436 = CARTESIAN_POINT ( 'NONE',  ( -0.8759842519685039353, 0.1787899950787401882, 0.7800196849856062542 ) ) ;
#3437 = CARTESIAN_POINT ( 'NONE',  ( 0.9873396505805591694, -0.1113553986120547346, 1.569881889656251861 ) ) ;
#3438 = VERTEX_POINT ( 'NONE', #8769 ) ;
#3439 = CARTESIAN_POINT ( 'NONE',  ( -0.07405724077823318263, 0.06594488194352732258, -0.1787899950787401604 ) ) ;
#3440 = ORIENTED_EDGE ( 'NONE', *, *, #25746, .T. ) ;
#3441 = CARTESIAN_POINT ( 'NONE',  ( 1.054774247047244540, -0.07405724077823318263, 0.8513779527021426707 ) ) ;
#3442 = CARTESIAN_POINT ( 'NONE',  ( 1.002407869896990045, -0.1264236179284866091, 1.085137795221826629 ) ) ;
#3443 = CARTESIAN_POINT ( 'NONE',  ( -0.8759842519685039353, 0.1787899950787401882, 1.921751968450173376 ) ) ;
#3444 = CARTESIAN_POINT ( 'NONE',  ( 0.6971942568897637749, 2.189545951927499583E-17, 1.892224409395055096 ) ) ;
#3445 = ORIENTED_EDGE ( 'NONE', *, *, #12750, .F. ) ;
#3446 = ( BOUNDED_CURVE ( )  B_SPLINE_CURVE ( 2, ( #28470, #25086, #10731, #43519, #26229, #24851, #40794, #7988, #39924 ),
 .UNSPECIFIED., .F., .T. ) 
 B_SPLINE_CURVE_WITH_KNOTS ( ( 3, 2, 2, 2, 3 ),
 ( 0.5500000000000000444, 0.5524999999999999911, 0.5550000000000000488, 0.5574999999999999956, 0.5600000000000000533 ),
 .UNSPECIFIED. ) 
 CURVE ( )  GEOMETRIC_REPRESENTATION_ITEM ( )  RATIONAL_B_SPLINE_CURVE ( ( 1.000000000000000000, 0.9238795325112869605, 1.000000000000000000, 0.9238795325112869605, 1.000000000000000000, 0.9238795325112869605, 1.000000000000000000, 0.9238795325112869605, 1.000000000000000000 ) ) 
 REPRESENTATION_ITEM ( '' )  ) ;
#3447 = CARTESIAN_POINT ( 'NONE',  ( -0.7646288533564489232, -0.1113553986120547346, 0.1919291338582677087 ) ) ;
#3448 = CARTESIAN_POINT ( 'NONE',  ( -1.094772975963752103E-17, -1.364789322559947005, -0.1787899950787401882 ) ) ;
#3449 = ORIENTED_EDGE ( 'NONE', *, *, #22998, .F. ) ;
#3450 = CARTESIAN_POINT ( 'NONE',  ( -0.07405724077823318263, -0.2834645668753703052, -0.1787899950787401604 ) ) ;
#3451 = ORIENTED_EDGE ( 'NONE', *, *, #11714, .F. ) ;
#3452 = CARTESIAN_POINT ( 'NONE',  ( 0.7495606340400177148, -0.1264236179284866091, 1.227854330654897685 ) ) ;
#3453 = LINE ( 'NONE', #20944, #35658 ) ;
#3454 = CARTESIAN_POINT ( 'NONE',  ( -0.2471921892202598448, -0.09660984127287174095, 0.02628542481997977326 ) ) ;
#3455 = CARTESIAN_POINT ( 'NONE',  ( 1.054774247047244096, 0.000000000000000000, 0.06151574797773248782 ) ) ;
#3456 = VECTOR ( 'NONE', #11530, 39.37007874015748854 ) ;
#3457 = AXIS2_PLACEMENT_3D ( 'NONE', #1367, #16022, #31816 ) ;
#3458 = VECTOR ( 'NONE', #44223, 39.37007874015748854 ) ;
#3459 = CARTESIAN_POINT ( 'NONE',  ( 0.1787899950787401882, -1.599901574749385880, -2.189545951927503898E-17 ) ) ;
#3460 = CARTESIAN_POINT ( 'NONE',  ( 0.1787899950787401604, -0.7362204723871804690, 0.07405724077823318263 ) ) ;
#3461 = EDGE_CURVE ( 'NONE', #4309, #26963, #33599, .T. ) ;
#3462 = CARTESIAN_POINT ( 'NONE',  ( -1.002407869896990045, -0.1264236179284866091, 0.5339566928596221063 ) ) ;
#3463 = CARTESIAN_POINT ( 'NONE',  ( 0.2759478392031617933, -0.09842519685039370636, 1.713085361781127913 ) ) ;
#3464 = CARTESIAN_POINT ( 'NONE',  ( -0.1797182628040039365, -1.260870581236588350, 0.000000000000000000 ) ) ;
#3465 = CARTESIAN_POINT ( 'NONE',  ( 0.9873396505805591694, 0.1113553986120547346, 1.432086614173228245 ) ) ;
#3466 = CARTESIAN_POINT ( 'NONE',  ( 1.002407869896990045, 0.1264236179284866091, 1.291830708607653477 ) ) ;
#3467 = CARTESIAN_POINT ( 'NONE',  ( 0.8019270111902716547, 0.1787899950787401604, 1.727362204670645385 ) ) ;
#3468 = ADVANCED_FACE ( 'NONE', ( #23632 ), #16285, .T. ) ;
#3469 = CARTESIAN_POINT ( 'NONE',  ( -1.033464566929133799, 0.000000000000000000, 0.5905511809948347235 ) ) ;
#3470 = CARTESIAN_POINT ( 'NONE',  ( -1.033464566929133799, 0.000000000000000000, 0.9940944881889764995 ) ) ;
#3471 = DIRECTION ( 'NONE',  ( 0.5735764363510447161, 0.8191520442889925757, 0.000000000000000000 ) ) ;
#3472 = CARTESIAN_POINT ( 'NONE',  ( -0.06523048226347956391, -0.7977362203649133177, 0.1574803149606297803 ) ) ;
#3473 = CARTESIAN_POINT ( 'NONE',  ( -0.9412147342319837628, 0.1574803149606300301, 1.660925196742867760 ) ) ;
#3474 = CARTESIAN_POINT ( 'NONE',  ( 0.8019270111902717657, -0.1787899950787401604, 0.1279527558517483676 ) ) ;
#3475 = DIRECTION ( 'NONE',  ( 0.000000000000000000, 0.000000000000000000, 1.000000000000000000 ) ) ;
#3477 = DIRECTION ( 'NONE',  ( -1.000000000000000000, 0.000000000000000000, 0.000000000000000000 ) ) ;
#3476 = CARTESIAN_POINT ( 'NONE',  ( 0.7495606340400177148, 0.1264236179284866091, 1.218011810969858111 ) ) ;
#3478 = CARTESIAN_POINT ( 'NONE',  ( -0.5555748031496040573, 0.7681739484881665581, -0.04983111751016756213 ) ) ;
#3479 = CARTESIAN_POINT ( 'NONE',  ( -1.002407869896990045, -0.1264236179284866091, 1.198326771599779628 ) ) ;
#3480 = CARTESIAN_POINT ( 'NONE',  ( 0.7646288533564489232, 0.1113553986120547346, 0.5265748030420794867 ) ) ;
#3481 = ORIENTED_EDGE ( 'NONE', *, *, #16668, .F. ) ;
#3482 = CARTESIAN_POINT ( 'NONE',  ( 0.8772383532517480376, 0.1744612781842942717, 0.03936828611531264371 ) ) ;
#3483 = CARTESIAN_POINT ( 'NONE',  ( -0.7185039370078746268, -0.06523048226347956391, 0.3371062991050715607 ) ) ;
#3484 = ORIENTED_EDGE ( 'NONE', *, *, #10963, .F. ) ;
#3485 = CARTESIAN_POINT ( 'NONE',  ( 0.6971942568897637749, 2.189545951927499583E-17, 1.498523621993480326 ) ) ;
#3486 = CARTESIAN_POINT ( 'NONE',  ( -0.8107537697050254399, -0.1574803149606297803, 1.090059055010582423 ) ) ;
#3488 = DIRECTION ( 'NONE',  ( 0.000000000000000000, 0.000000000000000000, 1.000000000000000000 ) ) ;
#3487 = CARTESIAN_POINT ( 'NONE',  ( 1.033464566929133799, 0.000000000000000000, 1.023622047136567126 ) ) ;
#3489 = CARTESIAN_POINT ( 'NONE',  ( 0.1264236179284866091, 0.01427165359707059308, 0.1264236179284866091 ) ) ;
#3490 = EDGE_LOOP ( 'NONE', ( #8008, #46438, #11694, #3034 ) ) ;
#3491 = CARTESIAN_POINT ( 'NONE',  ( 0.4620708661417345930, 0.6529540528279709211, 0.4629603087243970849 ) ) ;
#3492 = ORIENTED_EDGE ( 'NONE', *, *, #31532, .T. ) ;
#3493 = CIRCLE ( 'NONE', #30313, 0.3937007874015747699 ) ;
#3494 = CARTESIAN_POINT ( 'NONE',  ( -0.7646288533564489232, 0.1113553986120547346, 0.3789370078740157410 ) ) ;
#3495 = FILL_AREA_STYLE_COLOUR ( '', #6981 ) ;
#3496 = ORIENTED_EDGE ( 'NONE', *, *, #34588, .F. ) ;
#3497 = CARTESIAN_POINT ( 'NONE',  ( 0.8019270111902717657, 0.1787899950787401604, 0.5905511810485987167 ) ) ;
#3498 = VERTEX_POINT ( 'NONE', #26535 ) ;
#3499 = CARTESIAN_POINT ( 'NONE',  ( -0.7495606340400177148, -0.1264236179284866091, 1.503444881836000002 ) ) ;
#3500 = CARTESIAN_POINT ( 'NONE',  ( 0.1787899950787401604, -1.794291338528913426, -0.07405724077823318263 ) ) ;
#3501 = AXIS2_PLACEMENT_3D ( 'NONE', #22957, #645, #4726 ) ;
#3502 = CARTESIAN_POINT ( 'NONE',  ( -0.8107537697050234415, -0.1574803149606297803, 0.1156496062992125873 ) ) ;
#3503 = ORIENTED_EDGE ( 'NONE', *, *, #37106, .T. ) ;
#3504 = CARTESIAN_POINT ( 'NONE',  ( -1.002407869896990045, -0.1264236179284866091, 1.040846456639149764 ) ) ;
#3505 = CARTESIAN_POINT ( 'NONE',  ( -1.002407869896990045, -0.1264236179284866091, 0.7701771653005669016 ) ) ;
#3506 = CARTESIAN_POINT ( 'NONE',  ( -0.1939344384856130921, 0.1835261454399950420, -0.3085539532670508178 ) ) ;
#3507 = CARTESIAN_POINT ( 'NONE',  ( -0.6971942568897626646, -0.07405724077823297447, 0.1673228345919059168 ) ) ;
#3508 = CARTESIAN_POINT ( 'NONE',  ( 0.8759842519685039353, 0.1574803149606299191, 0.7972440943806614611 ) ) ;
#3509 = CARTESIAN_POINT ( 'NONE',  ( -0.1787899950787401882, -0.8037657005127029075, 0.000000000000000000 ) ) ;
#3510 = ORIENTED_EDGE ( 'NONE', *, *, #33798, .T. ) ;
#3511 = CARTESIAN_POINT ( 'NONE',  ( -0.06523048226347956391, -0.02509842508932336180, -0.1574803149606300301 ) ) ;
#3512 = CARTESIAN_POINT ( 'NONE',  ( 1.033464566929134687, -0.06523048226347956391, 1.070374015748031038 ) ) ;
#3513 = ORIENTED_EDGE ( 'NONE', *, *, #18454, .T. ) ;
#3514 = CARTESIAN_POINT ( 'NONE',  ( -0.7185039370078739607, 1.928577636452523993E-17, 1.722440944881889813 ) ) ;
#3515 = DIRECTION ( 'NONE',  ( 0.000000000000000000, 2.355041373848520102E-15, -1.000000000000000000 ) ) ;
#3516 = CARTESIAN_POINT ( 'NONE',  ( -0.9500414927467378812, 0.1787899950787401604, 0.7381889763241898939 ) ) ;
#3517 = VERTEX_POINT ( 'NONE', #19319 ) ;
#3518 = CARTESIAN_POINT ( 'NONE',  ( -0.7495606340400177148, 0.1264236179284866091, 1.852854330654897685 ) ) ;
#3519 = EDGE_CURVE ( 'NONE', #10456, #24872, #30387, .T. ) ;
#3520 = ORIENTED_EDGE ( 'NONE', *, *, #32106, .T. ) ;
#3521 = ADVANCED_FACE ( 'NONE', ( #23159 ), #45645, .T. ) ;
#3522 = CARTESIAN_POINT ( 'NONE',  ( -0.7495606340400177148, -0.1264236179284866091, 0.1304133857730082613 ) ) ;
#3523 = CARTESIAN_POINT ( 'NONE',  ( 1.033464566929134687, -0.06523048226347956391, 0.6373031496062994128 ) ) ;
#3524 = CARTESIAN_POINT ( 'NONE',  ( 0.1797182628040039087, -0.8450241245436764803, -0.07444174185955065859 ) ) ;
#3525 = CARTESIAN_POINT ( 'NONE',  ( -0.8107537697050254399, 0.1574803149606300301, 0.4060039369003470289 ) ) ;
#3526 = CARTESIAN_POINT ( 'NONE',  ( -0.8759842519685039353, -0.1574803149606299191, 1.328740157372787278 ) ) ;
#3527 = CARTESIAN_POINT ( 'NONE',  ( 0.7495606340400177148, -0.1264236179284866091, 0.7997047243556849594 ) ) ;
#3528 = EDGE_CURVE ( 'NONE', #20346, #18121, #39692, .T. ) ;
#3529 = CARTESIAN_POINT ( 'NONE',  ( -9.642888182262618425E-18, -0.5885826771653542844, -0.1574803149606299191 ) ) ;
#3530 = AXIS2_PLACEMENT_3D ( 'NONE', #41738, #30779, #8222 ) ;
#3531 = CARTESIAN_POINT ( 'NONE',  ( -0.1082836541852444240, 0.1230260985689107939, -0.1186662996108784202 ) ) ;
#3532 = EDGE_CURVE ( 'NONE', #47083, #10797, #23209, .T. ) ;
#3533 = LINE ( 'NONE', #17426, #25380 ) ;
#3534 = CARTESIAN_POINT ( 'NONE',  ( 0.7646288533564489232, 0.1113553986120547346, 1.205708661417322913 ) ) ;
#3536 = CARTESIAN_POINT ( 'NONE',  ( -1.033464566929133799, 0.000000000000000000, 0.8267716534357796299 ) ) ;
#3535 = CARTESIAN_POINT ( 'NONE',  ( 0.7698820887372280763, -0.1341113977068105756, 1.986080103382252826 ) ) ;
#3537 = LINE ( 'NONE', #15513, #9076 ) ;
#3538 = CARTESIAN_POINT ( 'NONE',  ( -0.1574803149606299191, -0.6476377951680629685, 0.000000000000000000 ) ) ;
#3539 = ORIENTED_EDGE ( 'NONE', *, *, #34881, .T. ) ;
#3540 = B_SPLINE_CURVE_WITH_KNOTS ( 'NONE', 3,
 ( #8889, #33849, #4804, #15626, #45048, #1211, #12261, #15150, #30265, #12027, #26652, #16336, #41919, #30957, #27377, #28070, #45523, #20845, #23994, #9371, #13659, #2391, #46008, #10072, #17258, #31897, #9611, #39051, #24230, #24450, #12974, #16559, #39285, #19904, #5768, #35013, #42408, #12747, #6221, #1687, #35486 ),
 .UNSPECIFIED., .F., .F.,
 ( 4, 1, 1, 1, 1, 1, 1, 2, 2, 1, 1, 1, 1, 2, 2, 2, 1, 1, 1, 1, 2, 2, 1, 1, 1, 1, 1, 2, 2, 4 ),
 ( 0.000000000000000000, 0.1249999999999960865, 0.1874999999999940326, 0.2187499999999930334, 0.2343749999999925338, 0.2421874999999922562, 0.2460937499999920341, 0.2480468749999919786, 0.2499999999999919231, 0.3124999999999915068, 0.3437499999999912292, 0.3593749999999910627, 0.3671874999999910627, 0.3710937499999910627, 0.3749999999999910072, 0.4999999999999903411, 0.5624999999999898970, 0.5937499999999898970, 0.6093749999999897859, 0.6171874999999897859, 0.6210937499999897859, 0.6249999999999897859, 0.6874999999999873435, 0.7187499999999860112, 0.7343749999999855671, 0.7421874999999853451, 0.7460937499999852340, 0.7480468749999852340, 0.7499999999999852340, 1.000000000000000000 ),
 .UNSPECIFIED. ) ;
#3542 = CARTESIAN_POINT ( 'NONE',  ( -0.8759842519685039353, 0.000000000000000000, 0.000000000000000000 ) ) ;
#3541 = CARTESIAN_POINT ( 'NONE',  ( 0.8019270111902716547, 0.1787899950787401604, 0.6249999999462366729 ) ) ;
#3543 = CARTESIAN_POINT ( 'NONE',  ( -0.1787899950787401604, -0.6279527558517482566, 0.07405724077823318263 ) ) ;
#3544 = CARTESIAN_POINT ( 'NONE',  ( 0.8107537697050254399, 0.1574803149606300301, 1.557578740157481212 ) ) ;
#3545 = CARTESIAN_POINT ( 'NONE',  ( -1.033464566929133799, 0.000000000000000000, 1.151574803149606474 ) ) ;
#3546 = CARTESIAN_POINT ( 'NONE',  ( 0.004280036809600739831, -0.1422536944054435537, 0.02921503453321950064 ) ) ;
#3547 = CARTESIAN_POINT ( 'NONE',  ( 0.6971942568897648851, 0.07405724077823318263, 1.023622047190330342 ) ) ;
#3548 = CARTESIAN_POINT ( 'NONE',  ( 0.5660731898098425585, 4.766607801171850497E-17, 0.000000000000000000 ) ) ;
#3549 = CARTESIAN_POINT ( 'NONE',  ( 0.1787899950787401604, -1.169291338528914537, 0.07405724077823318263 ) ) ;
#3550 = CARTESIAN_POINT ( 'NONE',  ( -0.1113553986120547346, -1.489173228346456712, -0.1113553986120547346 ) ) ;
#3551 = CARTESIAN_POINT ( 'NONE',  ( 0.1184675242425281411, 0.3740157480314960647, 1.224299699984021661 ) ) ;
#3552 = CARTESIAN_POINT ( 'NONE',  ( -0.9500414927467378812, -0.1787899950787401604, 0.1722440944344254266 ) ) ;
#3553 = CARTESIAN_POINT ( 'NONE',  ( 0.7646288533564489232, 0.1113553986120547346, 1.756889763779527547 ) ) ;
#3554 = ORIENTED_EDGE ( 'NONE', *, *, #31241, .F. ) ;
#3555 = CARTESIAN_POINT ( 'NONE',  ( -0.07405724077823318263, -1.415354330654897019, 0.1787899950787401604 ) ) ;
#3556 = CARTESIAN_POINT ( 'NONE',  ( -0.9500414927467377701, -0.1787899950787401604, 1.948818897584033705 ) ) ;
#3557 = CARTESIAN_POINT ( 'NONE',  ( -1.054774247047244540, -0.07405724077823318263, 1.673228346402929834 ) ) ;
#3558 = AXIS2_PLACEMENT_3D ( 'NONE', #20219, #16415, #38686 ) ;
#3559 = CARTESIAN_POINT ( 'NONE',  ( -1.054774247047244540, 0.07405724077823318263, 1.048228346402928723 ) ) ;
#3560 = CARTESIAN_POINT ( 'NONE',  ( -1.054774247047244540, 0.07405724077823318263, 0.3444881889226146243 ) ) ;
#3561 = CARTESIAN_POINT ( 'NONE',  ( -0.2471922904502826535, 0.08969147984774068771, 0.05033842647026517958 ) ) ;
#3562 = CARTESIAN_POINT ( 'NONE',  ( 0.9873396505805591694, 0.1113553986120547346, 0.2903543307086614012 ) ) ;
#3563 = CARTESIAN_POINT ( 'NONE',  ( -0.7646288533564489232, 0.1113553986120547346, 1.875000000000000000 ) ) ;
#3564 = CARTESIAN_POINT ( 'NONE',  ( 0.2026160082443593247, -0.5228204797047603103, -0.8983653719476394350 ) ) ;
#3565 = CARTESIAN_POINT ( 'NONE',  ( -0.1264236179284866091, -0.3657735745284516060, 0.1264236179284866091 ) ) ;
#3566 = CARTESIAN_POINT ( 'NONE',  ( 0.2442368959035201015, -0.5708661417322835607, 1.119822416324439018 ) ) ;
#3567 = CARTESIAN_POINT ( 'NONE',  ( -0.4330708661417322913, 0.1574803149606299191, -1.186023622047243986 ) ) ;
#3568 = CARTESIAN_POINT ( 'NONE',  ( -0.9500414927467378812, -0.1787899950787401604, 0.2903543306548980185 ) ) ;
#3569 = CARTESIAN_POINT ( 'NONE',  ( 0.2471922904502827645, -0.09842519685039372024, 0.006644306898576237720 ) ) ;
#3570 = ORIENTED_EDGE ( 'NONE', *, *, #1554, .T. ) ;
#3571 = CARTESIAN_POINT ( 'NONE',  ( -0.8019270111902716547, 0.1787899950787401604, 1.377952755851748368 ) ) ;
#3572 = ORIENTED_EDGE ( 'NONE', *, *, #45147, .T. ) ;
#3573 = CARTESIAN_POINT ( 'NONE',  ( 3.284318927891251994E-17, -1.176673228292692830, 0.1787899950787401882 ) ) ;
#3574 = CARTESIAN_POINT ( 'NONE',  ( -0.07405724077823318263, -1.425196850339937482, -0.1787899950787401604 ) ) ;
#3575 = ADVANCED_FACE ( 'NONE', ( #38939 ), #43233, .F. ) ;
#3576 = CARTESIAN_POINT ( 'NONE',  ( 1.339088206907401712, 0.9211694353608268493, 0.8759842519680315354 ) ) ;
#3577 = CARTESIAN_POINT ( 'NONE',  ( 0.9412147342319837628, -0.1574803149606297803, 0.3961614173228344971 ) ) ;
#3578 = CARTESIAN_POINT ( 'NONE',  ( 3.301370929368692659E-17, -0.5817367229688724661, 0.1797182628040039365 ) ) ;
#3579 = CARTESIAN_POINT ( 'NONE',  ( -0.3100393700787401619, 0.000000000000000000, 1.181102362204724310 ) ) ;
#3580 = CARTESIAN_POINT ( 'NONE',  ( -0.8107537697050253289, 0.1574803149606300301, 0.9571850392625528281 ) ) ;
#3581 = CARTESIAN_POINT ( 'NONE',  ( 1.002407869896990045, -0.1264236179284866091, 0.4552165353793071745 ) ) ;
#3582 = CARTESIAN_POINT ( 'NONE',  ( 0.8107537697050253289, -0.1574803149606297803, 1.798720472333418918 ) ) ;
#3583 = EDGE_CURVE ( 'NONE', #46340, #15018, #34907, .T. ) ;
#3584 = DIRECTION ( 'NONE',  ( 0.000000000000000000, -0.6156614753256597350, -0.7880107536067207930 ) ) ;
#3585 = CARTESIAN_POINT ( 'NONE',  ( 0.7646288533564489232, 0.1113553986120547346, 0.8120078740157481434 ) ) ;
#3586 = CARTESIAN_POINT ( 'NONE',  ( 0.000000000000000000, -0.09842519685039370636, 0.000000000000000000 ) ) ;
#3588 = CARTESIAN_POINT ( 'NONE',  ( 1.033464566929134687, -0.06523048226347956391, 0.7554133858267708668 ) ) ;
#3587 = LINE ( 'NONE', #6698, #28632 ) ;
#3589 = CARTESIAN_POINT ( 'NONE',  ( 3.414809992080330995E-16, 0.2954942322624074524, -0.3149606299212598381 ) ) ;
#3590 = ORIENTED_EDGE ( 'NONE', *, *, #47018, .T. ) ;
#3591 = CARTESIAN_POINT ( 'NONE',  ( -0.8107537697050254399, -0.1574803149606297803, 0.6176181101286931652 ) ) ;
#3592 = CARTESIAN_POINT ( 'NONE',  ( 0.1787899950787401604, -1.631889763725764553, -0.07405724077823318263 ) ) ;
#3593 = CARTESIAN_POINT ( 'NONE',  ( -0.1113553986120547346, -1.597440944774362048, -0.1113553986120547346 ) ) ;
#3594 = CARTESIAN_POINT ( 'NONE',  ( -0.1264236179284866091, -0.7189960629383621571, -0.1264236179284866091 ) ) ;
#3595 = CARTESIAN_POINT ( 'NONE',  ( -0.9412147342319837628, 0.1574803149606300301, 0.1648622046168823629 ) ) ;
#3596 = CARTESIAN_POINT ( 'NONE',  ( -0.1113553986120547346, -1.046259842519685179, 0.1113553986120547346 ) ) ;
#3597 = CARTESIAN_POINT ( 'NONE',  ( 0.7185039370078746268, -0.06523048226347956391, 1.006397637687749036 ) ) ;
#3598 = CARTESIAN_POINT ( 'NONE',  ( -0.1476377952755905387, -0.2237541348899636795, -1.272196386806235813 ) ) ;
#3599 = CARTESIAN_POINT ( 'NONE',  ( -1.054774247047244096, 0.000000000000000000, 0.3371062991588349989 ) ) ;
#3600 = ORIENTED_EDGE ( 'NONE', *, *, #47358, .T. ) ;
#3601 = ORIENTED_EDGE ( 'NONE', *, *, #10246, .F. ) ;
#3602 = ORIENTED_EDGE ( 'NONE', *, *, #47057, .T. ) ;
#3603 = CARTESIAN_POINT ( 'NONE',  ( -1.054774247047244540, 0.07405724077823318263, 1.604330708607653921 ) ) ;
#3604 = EDGE_LOOP ( 'NONE', ( #26995, #473, #33235, #7368 ) ) ;
#3605 = CARTESIAN_POINT ( 'NONE',  ( 0.9500414927467378812, 0.1787899950787401604, 1.569881889710015299 ) ) ;
#3606 = VERTEX_POINT ( 'NONE', #32002 ) ;
#3607 = CARTESIAN_POINT ( 'NONE',  ( -0.8759842519685039353, 0.1787899950787401882, 0.8243110235682834519 ) ) ;
#3608 = CARTESIAN_POINT ( 'NONE',  ( -0.9412147342319837628, -0.1574803149606297803, 0.4650590550105836440 ) ) ;
#3609 = CARTESIAN_POINT ( 'NONE',  ( -1.054774247047244540, -0.07405724077823318263, 0.7677165353793073965 ) ) ;
#3610 = DIRECTION ( 'NONE',  ( 0.000000000000000000, 0.000000000000000000, 1.000000000000000000 ) ) ;
#3611 = ( BOUNDED_CURVE ( )  B_SPLINE_CURVE ( 2, ( #23975, #31875, #5971, #13637, #28276, #46221, #42839, #31175, #35694 ),
 .UNSPECIFIED., .F., .T. ) 
 B_SPLINE_CURVE_WITH_KNOTS ( ( 3, 2, 2, 2, 3 ),
 ( 0.7500000000000000000, 0.7524999999999999467, 0.7550000000000000044, 0.7574999999999999512, 0.7600000000000000089 ),
 .UNSPECIFIED. ) 
 CURVE ( )  GEOMETRIC_REPRESENTATION_ITEM ( )  RATIONAL_B_SPLINE_CURVE ( ( 1.000000000000000000, 0.9238795325112869605, 1.000000000000000000, 0.9238795325112869605, 1.000000000000000000, 0.9238795325112869605, 1.000000000000000000, 0.9238795325112869605, 1.000000000000000000 ) ) 
 REPRESENTATION_ITEM ( '' )  ) ;
#3612 = DIRECTION ( 'NONE',  ( 0.000000000000000000, -1.000000000000000000, 0.000000000000000000 ) ) ;
#3613 = CARTESIAN_POINT ( 'NONE',  ( -0.9500414927467378812, -0.1787899950787401604, 1.515748031442299526 ) ) ;
#3614 = CARTESIAN_POINT ( 'NONE',  ( -0.7185039370078746268, -0.06523048226347956391, 1.872539369971213841 ) ) ;
#3615 = ORIENTED_EDGE ( 'NONE', *, *, #41505, .T. ) ;
#3616 = ( BOUNDED_CURVE ( )  B_SPLINE_CURVE ( 2, ( #15712, #37971, #12824, #31269, #37734, #19749, #30347, #5362, #16177 ),
 .UNSPECIFIED., .F., .F. ) 
 B_SPLINE_CURVE_WITH_KNOTS ( ( 3, 2, 2, 2, 3 ),
 ( 0.4000000000000000222, 0.4025000000000000244, 0.4050000000000000266, 0.4074999999999999734, 0.4099999999999999756 ),
 .UNSPECIFIED. ) 
 CURVE ( )  GEOMETRIC_REPRESENTATION_ITEM ( )  RATIONAL_B_SPLINE_CURVE ( ( 1.000000000000000000, 0.9238795325112869605, 1.000000000000000000, 0.9238795325112869605, 1.000000000000000000, 0.9238795325112869605, 1.000000000000000000, 0.9238795325112849621, 1.000000000000000000 ) ) 
 REPRESENTATION_ITEM ( '' )  ) ;
#3617 = CARTESIAN_POINT ( 'NONE',  ( 0.8759842519685039353, -0.1574803149606299191, 0.9744094487113701408 ) ) ;
#3618 = CARTESIAN_POINT ( 'NONE',  ( 0.7495606340400177148, 0.1264236179284866091, 1.498523621993480326 ) ) ;
#3619 = CARTESIAN_POINT ( 'NONE',  ( -0.04013712062794118351, -0.09851384031509645423, -0.1835615954122362392 ) ) ;
#3620 = CARTESIAN_POINT ( 'NONE',  ( -0.7185039370078739607, 1.928577636452523993E-17, 0.3740157479239689664 ) ) ;
#3621 = ORIENTED_EDGE ( 'NONE', *, *, #35353, .T. ) ;
#3622 = CARTESIAN_POINT ( 'NONE',  ( 0.1787899950787401604, -1.731423180827664110, 0.07405724077823318263 ) ) ;
#3623 = VERTEX_POINT ( 'NONE', #42524 ) ;
#3624 = ORIENTED_EDGE ( 'NONE', *, *, #6205, .F. ) ;
#3625 = CYLINDRICAL_SURFACE ( 'NONE', #33839, 0.1574803149606299191 ) ;
#3626 = CARTESIAN_POINT ( 'NONE',  ( -0.07405724077823318263, -0.9527559054580476694, -0.1787899950787401604 ) ) ;
#3627 = ADVANCED_FACE ( 'NONE', ( #9726 ), #9493, .F. ) ;
#3628 = CARTESIAN_POINT ( 'NONE',  ( -0.2471922599940329923, -0.09336655125506164443, -0.03811991455052992500 ) ) ;
#3629 = CARTESIAN_POINT ( 'NONE',  ( 0.6971942568897637749, 2.189545951927499583E-17, 0.3567913385289137596 ) ) ;
#3630 = CARTESIAN_POINT ( 'NONE',  ( -0.1797182628040039087, -0.1954178253310769053, 0.07444174185955065859 ) ) ;
#3631 = CARTESIAN_POINT ( 'NONE',  ( -0.1787899950787401882, -0.1738444406701836475, 0.000000000000000000 ) ) ;
#3632 = CARTESIAN_POINT ( 'NONE',  ( -0.1264236179284866091, -0.3105314960092286913, 0.1264236179284866091 ) ) ;
#3633 = CARTESIAN_POINT ( 'NONE',  ( -1.094772975963752103E-17, -0.01525590545804752021, -0.1787899950787401882 ) ) ;
#3634 = ITEM_DEFINED_TRANSFORMATION ( 'NONE', 'NONE', #7119,  #20860 ) ;
#3635 = CARTESIAN_POINT ( 'NONE',  ( 0.1574803149606300023, 1.126631386849005878, -3.440787370833236380 ) ) ;
#3636 = ADVANCED_FACE ( 'NONE', ( #14019 ), #31615, .T. ) ;
#3637 = CARTESIAN_POINT ( 'NONE',  ( 1.002407869896990045, -0.1264236179284866091, 0.5684055117572598403 ) ) ;
#3639 = CARTESIAN_POINT ( 'NONE',  ( 1.033464566929134687, 0.06523048226347956391, 1.114665354330708125 ) ) ;
#3638 = CARTESIAN_POINT ( 'NONE',  ( -0.9909871089404796995, 0.1202360962797062310, 0.03937007874015843040 ) ) ;
#3640 = DIRECTION ( 'NONE',  ( 0.000000000000000000, 1.000000000000000000, 0.000000000000000000 ) ) ;
#3641 = CARTESIAN_POINT ( 'NONE',  ( 0.1787899950787401604, -0.4557086613635593086, 0.07405724077823318263 ) ) ;
#3642 = CARTESIAN_POINT ( 'NONE',  ( -0.1377952755905510474, 0.000000000000000000, -0.2610569382242185488 ) ) ;
#3643 = CARTESIAN_POINT ( 'NONE',  ( 0.6971942568897648851, 0.07405724077823318263, 1.737204724355685848 ) ) ;
#3645 = DIRECTION ( 'NONE',  ( 1.000000000000000000, -0.000000000000000000, -0.000000000000000000 ) ) ;
#3644 = CARTESIAN_POINT ( 'NONE',  ( -0.1350242358423168476, -0.09796987684348246184, 0.2074744707784313413 ) ) ;
#3646 = EDGE_LOOP ( 'NONE', ( #29664, #18189, #18677, #755, #45195 ) ) ;
#3647 = CARTESIAN_POINT ( 'NONE',  ( 0.1377952755905511861, 0.1574803149606299191, 0.8070866141732283561 ) ) ;
#3648 = CARTESIAN_POINT ( 'NONE',  ( -0.1787899950787401882, -0.2022637794737956740, 0.000000000000000000 ) ) ;
#3650 = CARTESIAN_POINT ( 'NONE',  ( -0.3690944881889761664, 0.1574803149606353592, -0.7480314960629921295 ) ) ;
#3649 = CARTESIAN_POINT ( 'NONE',  ( -1.002407869896990045, 0.1264236179284866091, 0.4650590550643464716 ) ) ;
#3651 = CARTESIAN_POINT ( 'NONE',  ( 0.1787899950787401882, -1.122539370024976391, -2.189545951927503898E-17 ) ) ;
#3652 = CARTESIAN_POINT ( 'NONE',  ( 0.7495606340400177148, -0.1264236179284866091, 0.09104330703285078152 ) ) ;
#3653 = CARTESIAN_POINT ( 'NONE',  ( 0.1641609508012460417, 0.08087345834217524176, -0.1400729584206018841 ) ) ;
#3654 = CARTESIAN_POINT ( 'NONE',  ( -1.054774247047244540, -0.07405724077823318263, 1.633858267662771313 ) ) ;
#3655 = VERTEX_POINT ( 'NONE', #24567 ) ;
#3656 = CARTESIAN_POINT ( 'NONE',  ( -1.002407869896990045, 0.1264236179284866091, 1.213090551127338435 ) ) ;
#3657 = CARTESIAN_POINT ( 'NONE',  ( -0.9412147342319837628, 0.1574803149606300301, 0.8833661417322832277 ) ) ;
#3658 = CARTESIAN_POINT ( 'NONE',  ( 0.8019270111902717657, -0.1787899950787401604, 1.117125984198206412 ) ) ;
#3659 = CARTESIAN_POINT ( 'NONE',  ( 0.9500414927467378812, -0.1787899950787401604, 1.865157480261195877 ) ) ;
#3660 = CARTESIAN_POINT ( 'NONE',  ( -0.9412147342319837628, -0.1574803149606297803, 0.6323818897637792924 ) ) ;
#3661 = CARTESIAN_POINT ( 'NONE',  ( -0.6971942568897637749, 2.189545951927499583E-17, 1.026082677111590513 ) ) ;
#3662 = CARTESIAN_POINT ( 'NONE',  ( 0.1619907858921093569, 0.08803158632528092220, -0.1285577739724623192 ) ) ;
#3663 = CARTESIAN_POINT ( 'NONE',  ( -0.08812199945791716893, -0.2446169721538513642, -0.03618545512905850525 ) ) ;
#3664 = CARTESIAN_POINT ( 'NONE',  ( 0.7495606340400177148, 0.1264236179284866091, 0.2780511810485988278 ) ) ;
#3665 = CARTESIAN_POINT ( 'NONE',  ( -1.002407869896990045, 0.1264236179284866091, 0.3026574802611972648 ) ) ;
#3666 = CARTESIAN_POINT ( 'NONE',  ( -0.6971942568897626646, 0.07405724077823318263, 0.6692913385289144257 ) ) ;
#3667 = CARTESIAN_POINT ( 'NONE',  ( 0.9412147342319837628, 0.1574803149606300301, 1.660925196742867760 ) ) ;
#3668 = VERTEX_POINT ( 'NONE', #46595 ) ;
#3669 = EDGE_CURVE ( 'NONE', #8361, #5177, #6963, .T. ) ;
#3670 = CARTESIAN_POINT ( 'NONE',  ( -0.1787899950787401604, 0.07086614178604697112, -0.07405724077823318263 ) ) ;
#3671 = CARTESIAN_POINT ( 'NONE',  ( 1.054774247047244096, 0.000000000000000000, 0.7750984251430865779 ) ) ;
#3672 = CARTESIAN_POINT ( 'NONE',  ( 0.7495606340400177148, 0.1264236179284866091, 1.026082677111590513 ) ) ;
#3673 = CARTESIAN_POINT ( 'NONE',  ( -0.6971942568897637749, 2.189545951927499583E-17, 1.931594488135212728 ) ) ;
#3674 = CARTESIAN_POINT ( 'NONE',  ( 1.054774247047244540, -0.07405724077823318263, 1.948818897584033927 ) ) ;
#3675 = CIRCLE ( 'NONE', #41893, 0.09842519685039310962 ) ;
#3676 = DIRECTION ( 'NONE',  ( -1.000000000000000000, 0.000000000000000000, 0.000000000000000000 ) ) ;
#3677 = CARTESIAN_POINT ( 'NONE',  ( -0.1787899950787401882, -1.236836566654435199, 0.000000000000000000 ) ) ;
#3678 = ORIENTED_EDGE ( 'NONE', *, *, #17590, .F. ) ;
#3679 = CARTESIAN_POINT ( 'NONE',  ( 0.1787899950787401882, -0.3351377952218271283, -2.189545951927503898E-17 ) ) ;
#3680 = EDGE_CURVE ( 'NONE', #36578, #22073, #43222, .T. ) ;
#3681 = CARTESIAN_POINT ( 'NONE',  ( 0.1476377952755906220, 0.7443365962042343131, -3.523993443072799270 ) ) ;
#3682 = ORIENTED_EDGE ( 'NONE', *, *, #15135, .T. ) ;
#3683 = CARTESIAN_POINT ( 'NONE',  ( 0.7495606340400177148, -0.1264236179284866091, 1.149114173174582643 ) ) ;
#3684 = CARTESIAN_POINT ( 'NONE',  ( 0.01230737760510409486, -0.1591122789105269553, -1.990515434288500257E-18 ) ) ;
#3685 = CARTESIAN_POINT ( 'NONE',  ( -0.2471922904502826812, -0.03219022224904102836, 0.1427165354330708902 ) ) ;
#3686 = EDGE_CURVE ( 'NONE', #1004, #10953, #29361, .T. ) ;
#3687 = CARTESIAN_POINT ( 'NONE',  ( 0.8019270111902717657, 0.1787899950787401604, 1.530511810969859443 ) ) ;
#3688 = CARTESIAN_POINT ( 'NONE',  ( 1.033464566929134687, -0.06523048226347956391, 1.975885826771653475 ) ) ;
#3689 = CARTESIAN_POINT ( 'NONE',  ( 0.1787899950787401604, -1.602362204670647161, 0.07405724077823318263 ) ) ;
#3690 = CARTESIAN_POINT ( 'NONE',  ( 0.1787899950787401882, -1.673720472387181024, -2.189545951927503898E-17 ) ) ;
#3691 = APPLICATION_CONTEXT ( 'automotive_design' ) ;
#3692 = EDGE_CURVE ( 'NONE', #30045, #26635, #32407, .T. ) ;
#3693 = EDGE_CURVE ( 'NONE', #23379, #46614, #31138, .T. ) ;
#3694 = CARTESIAN_POINT ( 'NONE',  ( -0.7495606340400177148, 0.1264236179284866091, 0.5536417322297008115 ) ) ;
#3695 = CARTESIAN_POINT ( 'NONE',  ( 0.2362204724409448509, 0.000000000000000000, -0.9891732283464566011 ) ) ;
#3696 = CARTESIAN_POINT ( 'NONE',  ( -0.7103770212304942877, 0.007401083536364823356, 1.983133876338081913 ) ) ;
#3697 = CARTESIAN_POINT ( 'NONE',  ( -0.7185039370078739607, 1.928577636452523993E-17, 1.210629921259842590 ) ) ;
#3698 = CARTESIAN_POINT ( 'NONE',  ( 0.9500414927467378812, -0.1787899950787401604, 1.161417322780881278 ) ) ;
#3699 = CARTESIAN_POINT ( 'NONE',  ( 0.6971942568897648851, -0.07405724077823297447, 1.737204724355685626 ) ) ;
#3700 = CARTESIAN_POINT ( 'NONE',  ( 0.9412147342319837628, 0.1574803149606300301, 1.503444881782235232 ) ) ;
#3702 = CARTESIAN_POINT ( 'NONE',  ( -0.7733127964711655755, 0.1243806286706488490, 1.980518068217838268 ) ) ;
#3701 = DIRECTION ( 'NONE',  ( 1.822029033848725028E-16, 0.000000000000000000, 1.000000000000000000 ) ) ;
#3703 = CARTESIAN_POINT ( 'NONE',  ( -0.2066929133858267931, 1.126631386849004990, -3.440787370833234604 ) ) ;
#3704 = CARTESIAN_POINT ( 'NONE',  ( -0.1264236179284866091, 0.1471456693451021758, -0.1264236179284866091 ) ) ;
#3705 = CARTESIAN_POINT ( 'NONE',  ( 0.9412147342319837628, 0.1574803149606300301, 0.7554133857192454338 ) ) ;
#3706 = AXIS2_PLACEMENT_3D ( 'NONE', #42837, #2604, #10047 ) ;
#3707 = CARTESIAN_POINT ( 'NONE',  ( 1.002407869896990045, 0.1264236179284866091, 0.2239173227808822775 ) ) ;
#3708 = CARTESIAN_POINT ( 'NONE',  ( 0.7322234030063883292, -0.08795665246346720534, 0.03937064163498438241 ) ) ;
#3710 = DIRECTION ( 'NONE',  ( 1.822029033848725028E-16, 0.000000000000000000, 1.000000000000000000 ) ) ;
#3709 = CARTESIAN_POINT ( 'NONE',  ( 0.6971942568897637749, 2.189545951927499583E-17, 1.222933070812378009 ) ) ;
#3711 = CARTESIAN_POINT ( 'NONE',  ( -1.054774247047244096, 0.000000000000000000, 1.203248031442299304 ) ) ;
#3712 = CARTESIAN_POINT ( 'NONE',  ( 1.033464566929134687, 0.06523048226347956391, 0.6717519683964102706 ) ) ;
#3713 = VERTEX_POINT ( 'NONE', #2107 ) ;
#3714 = CARTESIAN_POINT ( 'NONE',  ( 0.2395294000716133853, 3.218313930830148909E-16, -0.8759842519685039353 ) ) ;
#3715 = CARTESIAN_POINT ( 'NONE',  ( 0.9291354005038431341, 0.1626576089091155419, 0.03937007862967787514 ) ) ;
#3716 = CARTESIAN_POINT ( 'NONE',  ( 0.7185039370078739607, 1.928577636452523993E-17, 0.8464566928058583350 ) ) ;
#3717 = CARTESIAN_POINT ( 'NONE',  ( -0.9873396505805591694, 0.1113553986120547346, 0.3592519683964098820 ) ) ;
#3718 = CARTESIAN_POINT ( 'NONE',  ( 0.001488155332080226502, 0.02696424538979726865, 0.1377975042921876780 ) ) ;
#3719 = CARTESIAN_POINT ( 'NONE',  ( 1.002407869896990045, -0.1264236179284866091, 1.395177165300567124 ) ) ;
#3720 = CARTESIAN_POINT ( 'NONE',  ( -0.7185039370078746268, -0.06523048226347956391, 1.085137795168063191 ) ) ;
#3721 = CYLINDRICAL_SURFACE ( 'NONE', #12744, 0.1574803149606299191 ) ;
#3722 = CARTESIAN_POINT ( 'NONE',  ( -0.1787899950787401604, -0.1210629920722208208, -0.07405724077823318263 ) ) ;
#3723 = VERTEX_POINT ( 'NONE', #22315 ) ;
#3724 = CARTESIAN_POINT ( 'NONE',  ( -0.2559055118110236116, -0.1477471161312049197, -0.1122047244094488277 ) ) ;
#3725 = ( BOUNDED_CURVE ( )  B_SPLINE_CURVE ( 2, ( #35668, #14564, #28738, #28244, #10020, #3544, #43782, #21265, #10507 ),
 .UNSPECIFIED., .F., .T. ) 
 B_SPLINE_CURVE_WITH_KNOTS ( ( 3, 2, 2, 2, 3 ),
 ( 0.7800000000000000266, 0.7824999999999999734, 0.7850000000000000311, 0.7874999999999999778, 0.7900000000000000355 ),
 .UNSPECIFIED. ) 
 CURVE ( )  GEOMETRIC_REPRESENTATION_ITEM ( )  RATIONAL_B_SPLINE_CURVE ( ( 1.000000000000000000, 0.9238795325112869605, 1.000000000000000000, 0.9238795325112869605, 1.000000000000000000, 0.9238795325112869605, 1.000000000000000000, 0.9238795325112869605, 1.000000000000000000 ) ) 
 REPRESENTATION_ITEM ( '' )  ) ;
#3726 = CARTESIAN_POINT ( 'NONE',  ( 0.000000000000000000, 0.000000000000000000, 0.000000000000000000 ) ) ;
#3727 = VERTEX_POINT ( 'NONE', #20087 ) ;
#3728 = CARTESIAN_POINT ( 'NONE',  ( 0.6971942568897637749, 2.189545951927499583E-17, 0.5191929133320630774 ) ) ;
#3729 = ORIENTED_EDGE ( 'NONE', *, *, #1554, .F. ) ;
#3730 = CARTESIAN_POINT ( 'NONE',  ( 0.1787899950787401882, -1.796751968450173376, -2.189545951927503898E-17 ) ) ;
#3731 = CARTESIAN_POINT ( 'NONE',  ( -0.8019270111902717657, -0.1787899950787401604, 1.077755905458048113 ) ) ;
#3732 = VERTEX_POINT ( 'NONE', #7701 ) ;
#3733 = ADVANCED_FACE ( 'NONE', ( #495 ), #30907, .T. ) ;
#3734 = CARTESIAN_POINT ( 'NONE',  ( -0.7185039370078746268, 0.06523048226347956391, 0.4896653542231815259 ) ) ;
#3735 = CARTESIAN_POINT ( 'NONE',  ( -0.6971942568897626646, 0.07405724077823318263, 0.8316929133320636325 ) ) ;
#3736 = ADVANCED_FACE ( 'NONE', ( #31374 ), #30099, .T. ) ;
#3737 = CARTESIAN_POINT ( 'NONE',  ( -1.054774247047244096, 0.000000000000000000, 0.2632874015210397434 ) ) ;
#3738 = CARTESIAN_POINT ( 'NONE',  ( 0.003857550520859602799, 0.1410454915399580178, -0.03130963158115300515 ) ) ;
#3739 = CARTESIAN_POINT ( 'NONE',  ( -0.07405724077823318263, -0.7963838107489246143, 0.1787899950787401604 ) ) ;
#3740 = CARTESIAN_POINT ( 'NONE',  ( 0.8107537697050254399, -0.1574803149606297803, 1.060531496062992352 ) ) ;
#3741 = ADVANCED_FACE ( 'NONE', ( #38301 ), #12924, .F. ) ;
#3742 = ORIENTED_EDGE ( 'NONE', *, *, #23227, .T. ) ;
#3743 = CARTESIAN_POINT ( 'NONE',  ( -0.7185039370078739607, 1.928577636452523993E-17, 0.5413385826771653919 ) ) ;
#3744 = AXIS2_PLACEMENT_3D ( 'NONE', #44263, #36406, #11461 ) ;
#3745 = ( BOUNDED_CURVE ( )  B_SPLINE_CURVE ( 2, ( #37142, #40012, #44316, #43856, #18462, #22056, #36920, #43377, #43615 ),
 .UNSPECIFIED., .F., .T. ) 
 B_SPLINE_CURVE_WITH_KNOTS ( ( 3, 2, 2, 2, 3 ),
 ( 0.1049999999999999961, 0.1074999999999999983, 0.1100000000000000006, 0.1125000000000000028, 0.1150000000000000050 ),
 .UNSPECIFIED. ) 
 CURVE ( )  GEOMETRIC_REPRESENTATION_ITEM ( )  RATIONAL_B_SPLINE_CURVE ( ( 1.000000000000000000, 0.9238795325112869605, 1.000000000000000000, 0.9238795325112869605, 1.000000000000000000, 0.9238795325112869605, 1.000000000000000000, 0.9238795325112869605, 1.000000000000000000 ) ) 
 REPRESENTATION_ITEM ( '' )  ) ;
#3746 = CARTESIAN_POINT ( 'NONE',  ( -0.9500414927467378812, -0.1787899950787401604, 0.7627952755367881643 ) ) ;
#3747 = EDGE_LOOP ( 'NONE', ( #10577, #3201, #42550, #19624 ) ) ;
#3748 = CARTESIAN_POINT ( 'NONE',  ( -1.002407869896990045, -0.1264236179284866091, 1.833169291284818758 ) ) ;
#3749 = CARTESIAN_POINT ( 'NONE',  ( 0.1264236179284866091, -0.4926181101824567143, -0.1264236179284866091 ) ) ;
#3750 = CARTESIAN_POINT ( 'NONE',  ( 0.7646288533564489232, -0.1113553986120547346, 0.6643700787401575214 ) ) ;
#3751 = CARTESIAN_POINT ( 'NONE',  ( 0.1270800023317771588, -0.8425634946224153099, -0.1270800023317771588 ) ) ;
#3752 = DIRECTION ( 'NONE',  ( -6.679788269418529283E-17, 1.000000000000000000, 0.000000000000000000 ) ) ;
#3753 = CARTESIAN_POINT ( 'NONE',  ( -0.8107537697050253289, -0.1574803149606297803, 1.483759842412158525 ) ) ;
#3754 = CARTESIAN_POINT ( 'NONE',  ( 1.002407869896990045, 0.1264236179284866091, 0.8193897637257637756 ) ) ;
#3755 = CARTESIAN_POINT ( 'NONE',  ( -0.2559055118110236116, 0.007127922025054847163, -0.02740704184215039807 ) ) ;
#3756 = CARTESIAN_POINT ( 'NONE',  ( 0.7185039370078746268, 0.06523048226347956391, 1.483759842519686067 ) ) ;
#3757 = EDGE_CURVE ( 'NONE', #30017, #22098, #35438, .T. ) ;
#3759 = DIRECTION ( 'NONE',  ( 0.000000000000000000, 0.000000000000000000, -1.000000000000000000 ) ) ;
#3758 = CARTESIAN_POINT ( 'NONE',  ( 0.8502105270501296719, -0.1718181285865334196, 1.987735233414207769 ) ) ;
#3760 = DIRECTION ( 'NONE',  ( -1.000000000000000000, 0.000000000000000000, 0.000000000000000000 ) ) ;
#3761 = ORIENTED_EDGE ( 'NONE', *, *, #5244, .F. ) ;
#3763 = CARTESIAN_POINT ( 'NONE',  ( 0.1574803149606300023, 0.3743908788525355247, -3.616772362661642148 ) ) ;
#3762 = CARTESIAN_POINT ( 'NONE',  ( 0.8759842519685039353, -0.1787899950787401882, 0.7997047243556849594 ) ) ;
#3764 = AXIS2_PLACEMENT_3D ( 'NONE', #43714, #10917, #3931 ) ;
#3765 = CARTESIAN_POINT ( 'NONE',  ( -0.1264236179284866091, -0.8223425196312754704, 0.1264236179284866091 ) ) ;
#3766 = CARTESIAN_POINT ( 'NONE',  ( 0.000000000000000000, 0.0004086818895575684884, 0.000000000000000000 ) ) ;
#3767 = ORIENTED_EDGE ( 'NONE', *, *, #37986, .T. ) ;
#3768 = DIRECTION ( 'NONE',  ( -4.336808689942014285E-16, 0.000000000000000000, -1.000000000000000000 ) ) ;
#3769 = DIRECTION ( 'NONE',  ( 1.000000000000000000, -0.000000000000000000, -0.000000000000000000 ) ) ;
#3770 = CARTESIAN_POINT ( 'NONE',  ( 0.6971942568897637749, 2.189545951927499583E-17, 0.9079724408911180600 ) ) ;
#3771 = CARTESIAN_POINT ( 'NONE',  ( -0.2066929133858267931, -0.5175744617845221551, -0.9076376772307634955 ) ) ;
#3773 = AXIS2_PLACEMENT_3D ( 'NONE', #35805, #2949, #32229 ) ;
#3772 = CARTESIAN_POINT ( 'NONE',  ( 0.1574803149606299191, -1.582677165354330784, -1.928577636452523993E-17 ) ) ;
#3774 = FACE_OUTER_BOUND ( 'NONE', #21502, .T. ) ;
#3775 = ORIENTED_EDGE ( 'NONE', *, *, #13482, .F. ) ;
#3776 = CARTESIAN_POINT ( 'NONE',  ( 0.2204724409448818867, 0.07955613945526338049, -0.1377952755905511861 ) ) ;
#3777 = CARTESIAN_POINT ( 'NONE',  ( -1.054774247047244096, 0.000000000000000000, 1.995570866087968520 ) ) ;
#3778 = VECTOR ( 'NONE', #30865, 39.37007874015748143 ) ;
#3779 = CARTESIAN_POINT ( 'NONE',  ( 0.7185039370078739607, 1.928577636452523993E-17, 0.9350393700787401619 ) ) ;
#3780 = CARTESIAN_POINT ( 'NONE',  ( -0.1787899950787401604, -1.425196850339937482, -0.07405724077823318263 ) ) ;
#3781 = CARTESIAN_POINT ( 'NONE',  ( -0.6971942568897637749, 2.189545951927499583E-17, 1.656003936954110412 ) ) ;
#3782 = ORIENTED_EDGE ( 'NONE', *, *, #13868, .F. ) ;
#3783 = ADVANCED_FACE ( 'NONE', ( #23465 ), #27554, .T. ) ;
#3784 = CARTESIAN_POINT ( 'NONE',  ( -0.8019270111902717657, 0.1787899950787401604, 1.058070866087969186 ) ) ;
#3785 = CARTESIAN_POINT ( 'NONE',  ( -0.8759842519685039353, 0.1787899950787401882, 0.4306102361667086820 ) ) ;
#3786 = EDGE_CURVE ( 'NONE', #40728, #6896, #36945, .T. ) ;
#3787 = LINE ( 'NONE', #43799, #29921 ) ;
#3788 = DIRECTION ( 'NONE',  ( -1.000000000000000000, 0.000000000000000000, 0.000000000000000000 ) ) ;
#3789 = CARTESIAN_POINT ( 'NONE',  ( 0.8107537697050254399, 0.1574803149606300301, 0.2977362204724410821 ) ) ;
#3790 = CARTESIAN_POINT ( 'NONE',  ( 0.6971942568897626646, -0.07405724077823297447, 0.08366141726907129483 ) ) ;
#3791 = DIRECTION ( 'NONE',  ( 0.5735764363510447161, 0.8191520442889925757, 0.000000000000000000 ) ) ;
#3792 = CARTESIAN_POINT ( 'NONE',  ( -0.1787899950787401604, -0.3731554642922310649, -0.07405724077823318263 ) ) ;
#3793 = CYLINDRICAL_SURFACE ( 'NONE', #25751, 0.1574803149606299191 ) ;
#3794 = ADVANCED_FACE ( 'NONE', ( #5222 ), #18951, .T. ) ;
#3795 = EDGE_CURVE ( 'NONE', #15794, #46578, #21638, .T. ) ;
#3796 = CARTESIAN_POINT ( 'NONE',  ( -0.8759842519685039353, -0.1787899950787401882, 0.3666338582139531677 ) ) ;
#3797 = AXIS2_PLACEMENT_3D ( 'NONE', #37657, #19436, #732 ) ;
#3798 = CARTESIAN_POINT ( 'NONE',  ( -0.8019270111902716547, 0.1787899950787401604, 1.417322834591906444 ) ) ;
#3799 = VERTEX_POINT ( 'NONE', #2799 ) ;
#3800 = CARTESIAN_POINT ( 'NONE',  ( -0.1787899950787401604, -1.302165354276944242, 0.07405724077823318263 ) ) ;
#3801 = CONICAL_SURFACE ( 'NONE', #46656, 0.08090551181102362266, 0.9599310885968742602 ) ;
#3802 = CARTESIAN_POINT ( 'NONE',  ( 0.07405724077823318263, -1.312007873961984705, -0.1787899950787401604 ) ) ;
#3803 = CARTESIAN_POINT ( 'NONE',  ( 0.1184675242425198838, 0.000000000000000000, -8.353959598330964227E-16 ) ) ;
#3804 = CARTESIAN_POINT ( 'NONE',  ( 1.001134792037401633, 0.9202755905601969211, -0.4736248074374803108 ) ) ;
#3805 = DIRECTION ( 'NONE',  ( 0.000000000000000000, 0.000000000000000000, -1.000000000000000000 ) ) ;
#3806 = CARTESIAN_POINT ( 'NONE',  ( -0.7185039370078746268, 0.06523048226347956391, 1.080216535325543958 ) ) ;
#3807 = CARTESIAN_POINT ( 'NONE',  ( 1.002407869896990045, 0.1264236179284866091, 0.4650590550643464716 ) ) ;
#3808 = CARTESIAN_POINT ( 'NONE',  ( 0.1574803149606300301, -0.1284448818897638567, 0.06523048226347956391 ) ) ;
#3809 = CARTESIAN_POINT ( 'NONE',  ( 1.033464566929134687, 0.06523048226347956391, 1.852854330601134691 ) ) ;
#3810 = CARTESIAN_POINT ( 'NONE',  ( -0.1586641775163213364, 2.559880088878760951, -3.648497683167374550 ) ) ;
#3811 = CARTESIAN_POINT ( 'NONE',  ( 0.9412147342319837628, -0.1574803149606297803, 0.9473425196850395746 ) ) ;
#3812 = FACE_BOUND ( 'NONE', #17412, .T. ) ;
#3814 = CARTESIAN_POINT ( 'NONE',  ( 0.9873396505805591694, -0.1113553986120547346, 1.540354330708661568 ) ) ;
#3813 = FACE_BOUND ( 'NONE', #38772, .T. ) ;
#3815 = CARTESIAN_POINT ( 'NONE',  ( 0.7646288533564489232, -0.1113553986120547346, 0.7824803149606299746 ) ) ;
#3816 = CARTESIAN_POINT ( 'NONE',  ( -0.3009843105729483326, 0.07510662309419850746, 1.025909792018103728 ) ) ;
#3817 = VERTEX_POINT ( 'NONE', #28483 ) ;
#3818 = VERTEX_POINT ( 'NONE', #16967 ) ;
#3819 = DIRECTION ( 'NONE',  ( 0.000000000000000000, 0.000000000000000000, 1.000000000000000000 ) ) ;
#3820 = FACE_OUTER_BOUND ( 'NONE', #2989, .T. ) ;
#3821 = CARTESIAN_POINT ( 'NONE',  ( 0.1264236179284866091, -1.550688976324188895, -0.1264236179284866091 ) ) ;
#3822 = CARTESIAN_POINT ( 'NONE',  ( -0.1113553986120547346, -1.479330708553889817, -0.1113553986120547346 ) ) ;
#3823 = CARTESIAN_POINT ( 'NONE',  ( -0.1264236179284866091, -0.7091535432533228045, 0.1264236179284866091 ) ) ;
#3824 = CARTESIAN_POINT ( 'NONE',  ( -0.9873396505805591694, 0.1113553986120547346, 0.08366141721530767628 ) ) ;
#3825 = CARTESIAN_POINT ( 'NONE',  ( 2.892866454678787531E-17, -1.001968503937007871, 0.1574803149606299191 ) ) ;
#3826 = CARTESIAN_POINT ( 'NONE',  ( 0.7185039370078739607, 1.928577636452523993E-17, 1.003937007766488199 ) ) ;
#3827 = DIRECTION ( 'NONE',  ( 0.000000000000000000, -1.000000000000000000, 0.000000000000000000 ) ) ;
#3828 = VECTOR ( 'NONE', #39185, 39.37007874015748143 ) ;
#3829 = ORIENTED_EDGE ( 'NONE', *, *, #27144, .T. ) ;
#3830 = ORIENTED_EDGE ( 'NONE', *, *, #41683, .T. ) ;
#3831 = ORIENTED_EDGE ( 'NONE', *, *, #9928, .T. ) ;
#3832 = CARTESIAN_POINT ( 'NONE',  ( -0.9500414927467378812, 0.1787899950787401604, 1.569881889710015299 ) ) ;
#3833 = CARTESIAN_POINT ( 'NONE',  ( 1.054774247047244540, -0.07405724077823318263, 1.678149606245448622 ) ) ;
#3834 = VERTEX_POINT ( 'NONE', #35885 ) ;
#3835 = CARTESIAN_POINT ( 'NONE',  ( -0.8759842519685039353, 0.1787899950787401882, 0.7455708660879684091 ) ) ;
#3836 = CARTESIAN_POINT ( 'NONE',  ( 0.8019270111902717657, -0.1787899950787401604, 0.3297244093950552069 ) ) ;
#3837 = CARTESIAN_POINT ( 'NONE',  ( -0.7646288533564489232, -0.1113553986120547346, 0.4576771652468039631 ) ) ;
#3838 = CARTESIAN_POINT ( 'NONE',  ( -1.054774247047244540, 0.07405724077823318263, 0.6938976377415124741 ) ) ;
#3839 = VECTOR ( 'NONE', #5194, 39.37007874015748143 ) ;
#3840 = CARTESIAN_POINT ( 'NONE',  ( -0.8759842519685039353, 0.000000000000000000, 0.000000000000000000 ) ) ;
#3841 = EDGE_CURVE ( 'NONE', #8310, #43583, #2567, .T. ) ;
#3842 = CARTESIAN_POINT ( 'NONE',  ( -0.7185039370078739607, 1.928577636452523993E-17, 1.673228346349165285 ) ) ;
#3843 = CARTESIAN_POINT ( 'NONE',  ( -0.8759842519685039353, -0.1787899950787401882, 1.631397637741511808 ) ) ;
#3844 = CARTESIAN_POINT ( 'NONE',  ( -0.8759842519685039353, -0.1574803149606299191, 1.840551180994834501 ) ) ;
#3845 = EDGE_LOOP ( 'NONE', ( #17687, #36233, #28151, #41572 ) ) ;
#3846 = CARTESIAN_POINT ( 'NONE',  ( -1.033464566929134687, -0.06523048226347956391, 1.621555118110237004 ) ) ;
#3847 = DIRECTION ( 'NONE',  ( -1.000000000000000000, 0.000000000000000000, 0.000000000000000000 ) ) ;
#3848 = CARTESIAN_POINT ( 'NONE',  ( 0.8759842519685039353, -0.1787899950787401882, 1.395177165300567124 ) ) ;
#3849 = CARTESIAN_POINT ( 'NONE',  ( 0.1468505162521946683, -0.09851384555016987066, -0.1345416994043196757 ) ) ;
#3850 = CARTESIAN_POINT ( 'NONE',  ( -0.8759842519685039353, -0.1574803149606299191, 1.574803149606299302 ) ) ;
#3851 = EDGE_LOOP ( 'NONE', ( #30997, #24195, #8872, #24931 ) ) ;
#3852 = EDGE_CURVE ( 'NONE', #33479, #32278, #44586, .T. ) ;
#3853 = DIRECTION ( 'NONE',  ( 0.000000000000000000, 0.000000000000000000, 1.000000000000000000 ) ) ;
#3854 = ORIENTED_EDGE ( 'NONE', *, *, #16088, .T. ) ;
#3855 = VERTEX_POINT ( 'NONE', #13599 ) ;
#3856 = B_SPLINE_CURVE_WITH_KNOTS ( 'NONE', 3,
 ( #448, #33557, #25878, #36658, #26118, #3816, #8360, #22985, #18436, #22034, #676, #11745, #14616, #15102, #7884, #11034, #33088, #37121, #7645, #22260, #36895, #4050, #18666, #4269, #15330, #29984, #8595, #30445, #41396, #42112, #44999, #34970, #38077, #23475 ),
 .UNSPECIFIED., .F., .F.,
 ( 4, 2, 2, 2, 2, 2, 2, 2, 2, 2, 2, 2, 2, 2, 2, 2, 4 ),
 ( 0.01356295551947108401, 0.01440869495260772501, 0.01525443438574436775, 0.01610017381888101048, 0.01694591325201764975, 0.01779165268515429249, 0.01863739211829093523, 0.01948313155142757797, 0.02032887098456421723, 0.02117461041770085997, 0.02202034985083749924, 0.02286608928397414198, 0.02371182871711078471, 0.02455756815024742745, 0.02540330758338407019, 0.02624904701652071293, 0.02709478644965735220 ),
 .UNSPECIFIED. ) ;
#3857 = DIRECTION ( 'NONE',  ( 1.000000000000000000, 0.000000000000000000, 0.000000000000000000 ) ) ;
#3858 = CARTESIAN_POINT ( 'NONE',  ( 3.284318927891251994E-17, -0.4286417322297008115, 0.1787899950787401882 ) ) ;
#3859 = CARTESIAN_POINT ( 'NONE',  ( 0.1264236179284866091, -0.9601377952218268508, -0.1264236179284866091 ) ) ;
#3860 = AXIS2_PLACEMENT_3D ( 'NONE', #42916, #11255, #46765 ) ;
#3861 = CARTESIAN_POINT ( 'NONE',  ( 0.8759842519685039353, 0.000000000000000000, 1.990649606245448844 ) ) ;
#3862 = MANIFOLD_SOLID_BREP ( 'Hook Bracket', #17070 ) ;
#3863 = CARTESIAN_POINT ( 'NONE',  ( 1.054774247047244540, 0.07405724077823318263, 1.796259842465923073 ) ) ;
#3864 = CARTESIAN_POINT ( 'NONE',  ( 0.07444174185955065859, -0.2643154631263528453, 0.1797182628040039087 ) ) ;
#3865 = CARTESIAN_POINT ( 'NONE',  ( 0.1787899950787401882, -0.07541924381978995506, -2.189545951927503898E-17 ) ) ;
#3866 = AXIS2_PLACEMENT_3D ( 'NONE', #19137, #5003, #15329 ) ;
#3867 = CARTESIAN_POINT ( 'NONE',  ( -1.094772975963752103E-17, -0.05462598419820496182, -0.1787899950787401882 ) ) ;
#3868 = CARTESIAN_POINT ( 'NONE',  ( 0.8107537697050234415, -0.1574803149606297803, 0.1451771652468037688 ) ) ;
#3869 = CARTESIAN_POINT ( 'NONE',  ( 0.7495606340400177148, -0.1264236179284866091, 0.5585629920722204877 ) ) ;
#3870 = CIRCLE ( 'NONE', #45935, 0.2204724409448818867 ) ;
#3872 = DIRECTION ( 'NONE',  ( 0.8191520442889980158, 1.003171929053532266E-16, -0.5735764363510372776 ) ) ;
#3871 = ( LENGTH_UNIT ( ) NAMED_UNIT ( * ) SI_UNIT ( $, .METRE. ) ) ;
#3873 = CARTESIAN_POINT ( 'NONE',  ( 0.3246033735368759610, -0.09842519685039370636, 1.205361022782828805E-17 ) ) ;
#3874 = CARTESIAN_POINT ( 'NONE',  ( 0.6971942568897648851, -0.07405724077823297447, 1.860236220418677089 ) ) ;
#3876 = CARTESIAN_POINT ( 'NONE',  ( 1.033464566929136907, -0.06523048226347749612, 1.887303149498772425 ) ) ;
#3875 = DIRECTION ( 'NONE',  ( 0.000000000000000000, 0.000000000000000000, 1.000000000000000000 ) ) ;
#3877 = FACE_OUTER_BOUND ( 'NONE', #1532, .T. ) ;
#3879 = CARTESIAN_POINT ( 'NONE',  ( 0.1787899950787401604, -0.3031496062454492879, 0.07405724077823318263 ) ) ;
#3878 = CARTESIAN_POINT ( 'NONE',  ( 0.06523048226347956391, -0.9355314959554644760, -0.1574803149606300301 ) ) ;
#3881 = CARTESIAN_POINT ( 'NONE',  ( 0.1564139474901022064, 0.1282476652663593897, 0.05864041697631208749 ) ) ;
#3880 = CARTESIAN_POINT ( 'NONE',  ( -0.6971942568897626646, -0.07405724077823297447, 0.4822834645131655606 ) ) ;
#3882 = CARTESIAN_POINT ( 'NONE',  ( -0.1264236179284866091, -1.097933070812378009, 0.1264236179284866091 ) ) ;
#3883 = CARTESIAN_POINT ( 'NONE',  ( 0.8019270111902717657, -0.1787899950787401604, 0.1328740156942679607 ) ) ;
#3884 = CARTESIAN_POINT ( 'NONE',  ( 0.1643970176816420548, 0.08114889158698145033, -0.1405540032085720592 ) ) ;
#3885 = CARTESIAN_POINT ( 'NONE',  ( -1.054774247047244540, 0.07405724077823318263, 1.599409448765135133 ) ) ;
#3886 = ORIENTED_EDGE ( 'NONE', *, *, #18130, .T. ) ;
#3887 = DIRECTION ( 'NONE',  ( 0.000000000000000000, 0.000000000000000000, 1.000000000000000000 ) ) ;
#3888 = CARTESIAN_POINT ( 'NONE',  ( 0.8759842519685039353, -0.1787899950787401882, 0.05659448813521291560 ) ) ;
#3889 = CARTESIAN_POINT ( 'NONE',  ( -0.7185039370078739607, 1.928577636452523993E-17, 0.5413385826771653919 ) ) ;
#3890 = CARTESIAN_POINT ( 'NONE',  ( -0.8019270111902717657, 0.1787899950787401604, 1.018700787347811110 ) ) ;
#3891 = CARTESIAN_POINT ( 'NONE',  ( -0.1595947434768149320, -0.2033521641548195757, -0.03294411891278189314 ) ) ;
#3892 = CARTESIAN_POINT ( 'NONE',  ( 0.7495606340400177148, -0.1264236179284866091, 0.3666338582139531677 ) ) ;
#3893 = CARTESIAN_POINT ( 'NONE',  ( -0.9500414927467377701, 0.1787899950787401604, 0.3051181101824569919 ) ) ;
#3894 = CARTESIAN_POINT ( 'NONE',  ( -1.054774247047244540, -0.07405724077823318263, 0.8070866141194653620 ) ) ;
#3895 = CARTESIAN_POINT ( 'NONE',  ( 0.7185039370078746268, -0.06523048226347956391, 1.715059055010583311 ) ) ;
#3896 = ADVANCED_FACE ( 'NONE', ( #24175 ), #42358, .F. ) ;
#3897 = VECTOR ( 'NONE', #44937, 39.37007874015748854 ) ;
#3898 = CARTESIAN_POINT ( 'NONE',  ( -0.1264236179284866091, -0.01033464561552783524, -0.1264236179284866091 ) ) ;
#3899 = CARTESIAN_POINT ( 'NONE',  ( 0.9500414927467377701, -0.1787899950787401604, 1.122047244040725422 ) ) ;
#3900 = CARTESIAN_POINT ( 'NONE',  ( -0.7495606340400177148, -0.1264236179284866091, 1.818405511757259729 ) ) ;
#3901 = EDGE_LOOP ( 'NONE', ( #21553, #3621, #40491, #10280 ) ) ;
#3902 = CIRCLE ( 'NONE', #29213, 0.09842519685039317900 ) ;
#3903 = EDGE_CURVE ( 'NONE', #21477, #40961, #16322, .T. ) ;
#3904 = CARTESIAN_POINT ( 'NONE',  ( 0.6971942568897648851, 0.07405724077823318263, 1.889763779473794258 ) ) ;
#3905 = CIRCLE ( 'NONE', #30723, 0.1377952755905510196 ) ;
#3906 = DIRECTION ( 'NONE',  ( 1.000000000000000000, 0.000000000000000000, -1.822029033848725275E-16 ) ) ;
#3907 = CARTESIAN_POINT ( 'NONE',  ( -0.1787899950787401604, -1.357407432796167379, -0.07405724077823318263 ) ) ;
#3908 = ORIENTED_EDGE ( 'NONE', *, *, #23614, .T. ) ;
#3909 = VECTOR ( 'NONE', #25774, 39.37007874015748854 ) ;
#3910 = CARTESIAN_POINT ( 'NONE',  ( -0.1787899950787401604, -0.1998031495525358359, -0.07405724077823318263 ) ) ;
#3911 = ORIENTED_EDGE ( 'NONE', *, *, #13388, .T. ) ;
#3912 = CARTESIAN_POINT ( 'NONE',  ( 0.7495606340400177148, 0.1264236179284866091, 1.178641732229700922 ) ) ;
#3913 = DIRECTION ( 'NONE',  ( -5.159318851433039196E-16, -0.6156614753256609562, -0.7880107536067197938 ) ) ;
#3914 = CARTESIAN_POINT ( 'NONE',  ( 0.7185039370078692977, 0.06523048226347515077, 1.395177165246803908 ) ) ;
#3915 = CARTESIAN_POINT ( 'NONE',  ( 1.054774247047244540, -0.07405724077823318263, 1.476377952702141449 ) ) ;
#3916 = CARTESIAN_POINT ( 'NONE',  ( 0.6971942568897637749, 2.189545951927499583E-17, 0.1599409448281264023 ) ) ;
#3917 = CARTESIAN_POINT ( 'NONE',  ( 0.1264236179284866091, -1.604822834591905556, 0.1264236179284866091 ) ) ;
#3918 = CARTESIAN_POINT ( 'NONE',  ( 0.1787899950787401882, -1.634350393647023614, -2.189545951927503898E-17 ) ) ;
#3919 = ADVANCED_FACE ( 'NONE', ( #25099 ), #31607, .T. ) ;
#3920 = VECTOR ( 'NONE', #28608, 39.37007874015748143 ) ;
#3921 = CARTESIAN_POINT ( 'NONE',  ( -0.7495606340400177148, 0.1264236179284866091, 0.4355314960092284138 ) ) ;
#3922 = CARTESIAN_POINT ( 'NONE',  ( -0.9412147342319837628, -0.1574803149606297803, 1.291830708553889595 ) ) ;
#3923 = DIRECTION ( 'NONE',  ( -2.114720919224289611E-16, 1.000000000000000000, 0.000000000000000000 ) ) ;
#3925 = CARTESIAN_POINT ( 'NONE',  ( -0.7096583094928544666, -0.002683553454102774460, 1.983317742401899286 ) ) ;
#3924 = CARTESIAN_POINT ( 'NONE',  ( -0.1797182628040039087, -1.376520187535801520, 0.07444174185955065859 ) ) ;
#3926 = CARTESIAN_POINT ( 'NONE',  ( 0.7646288533564489232, 0.1113553986120547346, 1.441929133858267598 ) ) ;
#3927 = CARTESIAN_POINT ( 'NONE',  ( 0.6971942568897648851, -0.07405724077823297447, 1.348425196796630976 ) ) ;
#3928 = CARTESIAN_POINT ( 'NONE',  ( 0.8759842519685039353, 0.1787899950787401882, 1.685531496009228469 ) ) ;
#3929 = DIRECTION ( 'NONE',  ( 0.000000000000000000, 1.000000000000000000, 0.000000000000000000 ) ) ;
#3930 = VECTOR ( 'NONE', #23402, 39.37007874015748143 ) ;
#3931 = DIRECTION ( 'NONE',  ( 1.000000000000000000, 0.000000000000000000, 0.000000000000000000 ) ) ;
#3932 = DIRECTION ( 'NONE',  ( 0.000000000000000000, 0.000000000000000000, -1.000000000000000000 ) ) ;
#3933 = CARTESIAN_POINT ( 'NONE',  ( 0.8759842519685039353, 0.1574803149606299191, 0.7578740156405039397 ) ) ;
#3934 = CARTESIAN_POINT ( 'NONE',  ( 0.8019270111902717657, -0.1787899950787401604, 0.2854330708123783422 ) ) ;
#3935 = CARTESIAN_POINT ( 'NONE',  ( -0.7185039370078739607, 0.000000000000000000, -2.869337061179095023E-17 ) ) ;
#3936 = CARTESIAN_POINT ( 'NONE',  ( 0.000000000000000000, 0.000000000000000000, -0.2610569382242185488 ) ) ;
#3937 = LINE ( 'NONE', #341, #13875 ) ;
#3938 = CARTESIAN_POINT ( 'NONE',  ( -0.6971942568897648851, 0.07405724077823318263, 1.259842519631276359 ) ) ;
#3939 = CARTESIAN_POINT ( 'NONE',  ( 1.033464566929134687, -0.06523048226347956391, 0.5880905510735753294 ) ) ;
#3940 = VERTEX_POINT ( 'NONE', #24864 ) ;
#3941 = LENGTH_MEASURE_WITH_UNIT ( LENGTH_MEASURE( 0.02539999999999999897 ), #37017 ) ;
#3942 = CARTESIAN_POINT ( 'NONE',  ( 0.9297866679844647431, 0.1623955463951254619, 0.03937007045119578913 ) ) ;
#3943 = DIRECTION ( 'NONE',  ( 0.000000000000000000, -1.000000000000000000, 0.000000000000000000 ) ) ;
#3944 = CARTESIAN_POINT ( 'NONE',  ( 0.6971942568897648851, 0.07405724077823318263, 1.574803149552536530 ) ) ;
#3945 = DIRECTION ( 'NONE',  ( 0.000000000000000000, 0.000000000000000000, 1.000000000000000000 ) ) ;
#3946 = DIRECTION ( 'NONE',  ( -0.000000000000000000, -0.000000000000000000, -1.000000000000000000 ) ) ;
#3947 = CARTESIAN_POINT ( 'NONE',  ( 0.8107537697050254399, -0.1574803149606297803, 1.178641732283464583 ) ) ;
#3948 = CARTESIAN_POINT ( 'NONE',  ( -0.1787899950787401882, -0.1973425196312759700, 0.000000000000000000 ) ) ;
#3949 = ORIENTED_EDGE ( 'NONE', *, *, #32760, .F. ) ;
#3950 = ADVANCED_FACE ( 'NONE', ( #21260 ), #39689, .F. ) ;
#3951 = CARTESIAN_POINT ( 'NONE',  ( 2.892866454678787531E-17, 0.1003937007874015908, 0.1574803149606299191 ) ) ;
#3952 = CARTESIAN_POINT ( 'NONE',  ( -0.05612302249891534811, -0.07766248740294821873, 0.2530304272095453277 ) ) ;
#3953 = VERTEX_POINT ( 'NONE', #21496 ) ;
#3954 = CARTESIAN_POINT ( 'NONE',  ( 0.8759842519685039353, 0.1787899950787401882, 0.6274606298674959559 ) ) ;
#3955 = VERTEX_POINT ( 'NONE', #28016 ) ;
#3956 = CARTESIAN_POINT ( 'NONE',  ( -0.9500414927467377701, -0.1787899950787401604, 1.471456692859622217 ) ) ;
#3957 = CARTESIAN_POINT ( 'NONE',  ( -0.1787899950787401882, -1.777066929080094670, 0.000000000000000000 ) ) ;
#3958 = CARTESIAN_POINT ( 'NONE',  ( -0.6971942568897648851, -0.07405724077823297447, 1.072834645615528659 ) ) ;
#3959 = CARTESIAN_POINT ( 'NONE',  ( -0.2559055118110235560, -0.08321452205036067307, -0.05565866801132852287 ) ) ;
#3960 = CIRCLE ( 'NONE', #43844, 0.1574803149606299191 ) ;
#3961 = ADVANCED_FACE ( 'NONE', ( #13385 ), #8628, .F. ) ;
#3962 = CARTESIAN_POINT ( 'NONE',  ( -0.7495606340400177148, -0.1264236179284866091, 0.7603346456155274380 ) ) ;
#3963 = AXIS2_PLACEMENT_3D ( 'NONE', #21985, #36607, #33273 ) ;
#3964 = CARTESIAN_POINT ( 'NONE',  ( -0.1871882013107595277, 0.1874210200769348689, -0.3098131533095127010 ) ) ;
#3965 = CARTESIAN_POINT ( 'NONE',  ( -1.054774247047244540, -0.07405724077823318263, 0.2214566928596220785 ) ) ;
#3966 = CARTESIAN_POINT ( 'NONE',  ( 0.005686768416221401126, 0.1458881524273768215, -0.02291217744946314958 ) ) ;
#3967 = CYLINDRICAL_SURFACE ( 'NONE', #45037, 0.09842519685039370636 ) ;
#3968 = CARTESIAN_POINT ( 'NONE',  ( -0.1264236179284866091, -0.8775845981504979409, 0.1264236179284866091 ) ) ;
#3969 = ORIENTED_EDGE ( 'NONE', *, *, #37217, .F. ) ;
#3970 = CARTESIAN_POINT ( 'NONE',  ( -0.1787899950787401604, 0.1200787402112438867, 0.07405724077823318263 ) ) ;
#3971 = APPLICATION_CONTEXT ( 'automotive_design' ) ;
#3972 = EDGE_LOOP ( 'NONE', ( #24578, #14128, #46856, #40143 ) ) ;
#3973 = CONICAL_SURFACE ( 'NONE', #33075, 0.08090551181102362266, 0.9599310885968742602 ) ;
#3974 = CARTESIAN_POINT ( 'NONE',  ( -0.9500414927467378812, -0.1787899950787401604, 0.7234251967966300878 ) ) ;
#3975 = CARTESIAN_POINT ( 'NONE',  ( 0.6195511811023624027, 0.9842519685039370358, -0.5511811023622036343 ) ) ;
#3976 = CARTESIAN_POINT ( 'NONE',  ( -0.8019270111902716547, 0.1787899950787401604, 1.811023621993480548 ) ) ;
#3977 = CARTESIAN_POINT ( 'NONE',  ( -0.6971942568897637749, 2.189545951927499583E-17, 0.08612204719033110523 ) ) ;
#3978 = CARTESIAN_POINT ( 'NONE',  ( -1.033464566929133799, 0.000000000000000000, 0.9153543307086614567 ) ) ;
#3979 = CARTESIAN_POINT ( 'NONE',  ( -0.07444174185955065859, -0.9926619198192657700, -0.1797182628040039087 ) ) ;
#3980 = LINE ( 'NONE', #606, #11849 ) ;
#3981 = CARTESIAN_POINT ( 'NONE',  ( -0.9873396505805591694, -0.1113553986120547346, 1.569881889656251861 ) ) ;
#3982 = CARTESIAN_POINT ( 'NONE',  ( 0.7495606340400177148, -0.1264236179284866091, 0.8390748030958424808 ) ) ;
#3983 = ADVANCED_FACE ( 'NONE', ( #13018 ), #33958, .T. ) ;
#3984 = VECTOR ( 'NONE', #43167, 39.37007874015748143 ) ;
#3985 = CARTESIAN_POINT ( 'NONE',  ( 0.7646288533564489232, -0.1113553986120547346, 1.451771653543306950 ) ) ;
#3986 = CARTESIAN_POINT ( 'NONE',  ( 0.9720564657138344167, -0.1495739268380064380, 1.989996134449682375 ) ) ;
#3987 = DIRECTION ( 'NONE',  ( 1.822029033848725028E-16, 0.000000000000000000, 1.000000000000000000 ) ) ;
#3988 = ( BOUNDED_CURVE ( )  B_SPLINE_CURVE ( 2, ( #12209, #27561, #16513, #38072, #8356, #38547, #26833, #27323, #5711 ),
 .UNSPECIFIED., .F., .T. ) 
 B_SPLINE_CURVE_WITH_KNOTS ( ( 3, 2, 2, 2, 3 ),
 ( 0.6199999999999999956, 0.6225000000000000533, 0.6250000000000000000, 0.6274999999999999467, 0.6300000000000000044 ),
 .UNSPECIFIED. ) 
 CURVE ( )  GEOMETRIC_REPRESENTATION_ITEM ( )  RATIONAL_B_SPLINE_CURVE ( ( 1.000000000000000000, 0.9238795325112869605, 1.000000000000000000, 0.9238795325112869605, 1.000000000000000000, 0.9238795325112869605, 1.000000000000000000, 0.9238795325112829637, 1.000000000000000000 ) ) 
 REPRESENTATION_ITEM ( '' )  ) ;
#3989 = CARTESIAN_POINT ( 'NONE',  ( 0.8759842519685039353, 0.1787899950787401882, 0.8587598424659212970 ) ) ;
#3990 = CARTESIAN_POINT ( 'NONE',  ( 0.1787899950787401882, -0.8075787401037164415, -2.189545951927503898E-17 ) ) ;
#3991 = VERTEX_POINT ( 'NONE', #22424 ) ;
#3992 = EDGE_CURVE ( 'NONE', #35281, #23980, #2207, .T. ) ;
#3993 = CARTESIAN_POINT ( 'NONE',  ( 0.9873396505805591694, 0.1113553986120547346, 1.077755905511811108 ) ) ;
#3995 = CARTESIAN_POINT ( 'NONE',  ( 0.4755220087074803481, 1.205361022782824954E-17, -0.09842519685039370636 ) ) ;
#3994 = CIRCLE ( 'NONE', #30835, 0.1377952755905511861 ) ;
#3996 = CARTESIAN_POINT ( 'NONE',  ( 1.002407869896990045, 0.1264236179284866091, 1.050688976324189117 ) ) ;
#3997 = CARTESIAN_POINT ( 'NONE',  ( 0.6195511811023612925, 0.6529540528279703659, 0.4629603087243970849 ) ) ;
#3998 = CARTESIAN_POINT ( 'NONE',  ( -0.1574803149606297803, -1.599901574803148652, 0.06523048226347956391 ) ) ;
#3999 = DIRECTION ( 'NONE',  ( 0.000000000000000000, -1.000000000000000000, 0.000000000000000000 ) ) ;
#4000 = VERTEX_POINT ( 'NONE', #1317 ) ;
#4001 = FACE_BOUND ( 'NONE', #1482, .T. ) ;
#4002 = CARTESIAN_POINT ( 'NONE',  ( -0.8759842519685039353, 0.1787899950787401882, 0.2288385826234019815 ) ) ;
#4003 = CARTESIAN_POINT ( 'NONE',  ( 0.9873396505805591694, 0.1113553986120547346, 1.747047244094488194 ) ) ;
#4004 = CARTESIAN_POINT ( 'NONE',  ( -0.07405724077823318263, -1.454724409395055096, 0.1787899950787401604 ) ) ;
#4005 = CARTESIAN_POINT ( 'NONE',  ( 0.000000000000000000, 0.1193342091828950846, -0.06889763779527559306 ) ) ;
#4006 = CARTESIAN_POINT ( 'NONE',  ( -0.9500414927467378812, 0.1787899950787401604, 1.683070866087970074 ) ) ;
#4007 = CARTESIAN_POINT ( 'NONE',  ( -1.002407869896990045, -0.1264236179284866091, 0.8439960629383622681 ) ) ;
#4008 = CARTESIAN_POINT ( 'NONE',  ( -0.9500414927467378812, 0.1787899950787401604, 1.053149606245450176 ) ) ;
#4009 = ( BOUNDED_CURVE ( )  B_SPLINE_CURVE ( 2, ( #28269, #18174, #24662, #10529, #47408, #29255, #25126, #29001, #6668 ),
 .UNSPECIFIED., .F., .T. ) 
 B_SPLINE_CURVE_WITH_KNOTS ( ( 3, 2, 2, 2, 3 ),
 ( 0.8900000000000000133, 0.8924999999999999600, 0.8950000000000000178, 0.8974999999999999645, 0.9000000000000000222 ),
 .UNSPECIFIED. ) 
 CURVE ( )  GEOMETRIC_REPRESENTATION_ITEM ( )  RATIONAL_B_SPLINE_CURVE ( ( 1.000000000000000000, 0.9238795325112899581, 1.000000000000000000, 0.9238795325112869605, 1.000000000000000000, 0.9238795325112869605, 1.000000000000000000, 0.9238795325112869605, 1.000000000000000000 ) ) 
 REPRESENTATION_ITEM ( '' )  ) ;
#4010 = EDGE_CURVE ( 'NONE', #32338, #35869, #33163, .T. ) ;
#4011 = LINE ( 'NONE', #414, #45904 ) ;
#4012 = CARTESIAN_POINT ( 'NONE',  ( -0.02899999999999994943, 0.5288907983920058120, -0.7507079620615694227 ) ) ;
#4013 = CARTESIAN_POINT ( 'NONE',  ( -0.7185039370078739607, 1.928577636452523993E-17, 0.3346456691838114450 ) ) ;
#4014 = CARTESIAN_POINT ( 'NONE',  ( 1.002407869896990045, 0.1264236179284866091, 0.02706692908009476414 ) ) ;
#4015 = CARTESIAN_POINT ( 'NONE',  ( -0.2801604161619158928, 0.1329643277078512986, -0.9781273115788398087 ) ) ;
#4016 = CARTESIAN_POINT ( 'NONE',  ( 0.07405724077823318263, -0.3583916847646721471, 0.1787899950787401604 ) ) ;
#4017 = CARTESIAN_POINT ( 'NONE',  ( -0.2061074570449838439, -0.08955986677483838976, 0.1074491168787045231 ) ) ;
#4018 = DIRECTION ( 'NONE',  ( 1.000000000000000000, 0.000000000000000000, 0.000000000000000000 ) ) ;
#4019 = CARTESIAN_POINT ( 'NONE',  ( 0.2559043039006217990, -0.06897312490620088887, -0.04680397461132097814 ) ) ;
#4020 = CARTESIAN_POINT ( 'NONE',  ( -0.8019270111902717657, -0.1787899950787401604, 0.3641732282926931630 ) ) ;
#4021 = AXIS2_PLACEMENT_3D ( 'NONE', #30055, #45315, #26672 ) ;
#4022 = CARTESIAN_POINT ( 'NONE',  ( 0.7185039370078741827, 0.06523048226347841205, 0.8144685039370075375 ) ) ;
#4023 = EDGE_LOOP ( 'NONE', ( #45619, #3829, #31901, #19977 ) ) ;
#4024 = CARTESIAN_POINT ( 'NONE',  ( -0.8759842519685039353, 0.1787899950787401882, 1.336122047190330786 ) ) ;
#4025 = ORIENTED_EDGE ( 'NONE', *, *, #7280, .T. ) ;
#4026 = VECTOR ( 'NONE', #38304, 39.37007874015748854 ) ;
#4027 = CARTESIAN_POINT ( 'NONE',  ( -1.094772975963752103E-17, -1.314468503883243988, -0.1787899950787401882 ) ) ;
#4028 = CARTESIAN_POINT ( 'NONE',  ( -0.1264236179284866091, -1.462106299158834721, -0.1264236179284866091 ) ) ;
#4029 = LINE ( 'NONE', #32833, #13335 ) ;
#4030 = DIRECTION ( 'NONE',  ( 0.000000000000000000, 2.999999999999999839E-15, 1.000000000000000000 ) ) ;
#4031 = CARTESIAN_POINT ( 'NONE',  ( 0.8759842519685039353, 0.1574803149606299191, 0.4133858267716535861 ) ) ;
#4032 = CARTESIAN_POINT ( 'NONE',  ( -0.1797182628040039365, -0.5915792426539113746, 0.000000000000000000 ) ) ;
#4033 = FACE_OUTER_BOUND ( 'NONE', #33455, .T. ) ;
#4034 = CARTESIAN_POINT ( 'NONE',  ( -1.033464566929133799, 0.000000000000000000, 1.062992125876724314 ) ) ;
#4035 = VECTOR ( 'NONE', #37518, 39.37007874015748854 ) ;
#4036 = CARTESIAN_POINT ( 'NONE',  ( 1.002407869896990045, -0.1264236179284866091, 0.4158464566391496531 ) ) ;
#4037 = CARTESIAN_POINT ( 'NONE',  ( 1.033464566929134687, 0.06523048226347956391, 0.5536417321759372623 ) ) ;
#4038 = CARTESIAN_POINT ( 'NONE',  ( 0.1574803149606300301, -0.3252952755905512694, 0.06523048226347956391 ) ) ;
#4039 = CARTESIAN_POINT ( 'NONE',  ( 0.9412147342319837628, 0.1574803149606300301, 1.975885826664125711 ) ) ;
#4040 = ORIENTED_EDGE ( 'NONE', *, *, #27793, .F. ) ;
#4041 = EDGE_CURVE ( 'NONE', #3723, #15821, #12497, .T. ) ;
#4042 = DIRECTION ( 'NONE',  ( -1.000000000000000000, 0.000000000000000000, 0.000000000000000000 ) ) ;
#4043 = CARTESIAN_POINT ( 'NONE',  ( 0.7185039370078746268, 0.06523048226347956391, 1.011318897637796033 ) ) ;
#4044 = CARTESIAN_POINT ( 'NONE',  ( 0.1574803149606299746, 0.1473293504822046074, -0.5595480905233950475 ) ) ;
#4045 = CARTESIAN_POINT ( 'NONE',  ( 0.06523048226347956391, -0.5172244093412917687, 0.1574803149606297803 ) ) ;
#4046 = EDGE_CURVE ( 'NONE', #28221, #6310, #37272, .T. ) ;
#4047 = CARTESIAN_POINT ( 'NONE',  ( 0.8107537697050254399, -0.1574803149606297803, 0.7455708661417325134 ) ) ;
#4048 = CARTESIAN_POINT ( 'NONE',  ( -0.1676346118796341045, -0.08956121678320581869, 0.01619327428367629829 ) ) ;
#4049 = EDGE_CURVE ( 'NONE', #20929, #39852, #37902, .T. ) ;
#4050 = CARTESIAN_POINT ( 'NONE',  ( -0.2713217623817691382, 0.1501096695199154452, 0.8012500425422474093 ) ) ;
#4051 = ORIENTED_EDGE ( 'NONE', *, *, #11781, .F. ) ;
#4052 = EDGE_LOOP ( 'NONE', ( #2493, #38155, #12831, #11444 ) ) ;
#4053 = CARTESIAN_POINT ( 'NONE',  ( -0.7646288533564489232, -0.1113553986120547346, 0.6151574802074331050 ) ) ;
#4054 = DIRECTION ( 'NONE',  ( 7.047314121155781188E-15, 0.000000000000000000, 1.000000000000000000 ) ) ;
#4055 = CARTESIAN_POINT ( 'NONE',  ( -0.1787899950787401604, -1.499015747977732627, -0.07405724077823318263 ) ) ;
#4056 = CARTESIAN_POINT ( 'NONE',  ( 0.1787899950787401604, -0.8149606298674965110, 0.07405724077823318263 ) ) ;
#4057 = CARTESIAN_POINT ( 'NONE',  ( 0.1113553986120547346, -1.154527559055118058, 0.1113553986120547346 ) ) ;
#4058 = CARTESIAN_POINT ( 'NONE',  ( 0.7185039370078746268, 0.06523048226347956391, 1.040846456585385882 ) ) ;
#4059 = CARTESIAN_POINT ( 'NONE',  ( 0.7185039370078746268, 0.06523048226347956391, 1.838090551181102317 ) ) ;
#4060 = CIRCLE ( 'NONE', #35456, 0.09842519685039370636 ) ;
#4061 = ORIENTED_EDGE ( 'NONE', *, *, #26809, .T. ) ;
#4062 = EDGE_LOOP ( 'NONE', ( #22601, #3570, #16300, #5663 ) ) ;
#4063 = ORIENTED_EDGE ( 'NONE', *, *, #31353, .F. ) ;
#4064 = CARTESIAN_POINT ( 'NONE',  ( -0.8759842519685039353, -0.1787899950787401882, 1.592027559001354398 ) ) ;
#4065 = CARTESIAN_POINT ( 'NONE',  ( 0.6971942568897637749, 2.189545951927499583E-17, 1.779035433017102319 ) ) ;
#4066 = CARTESIAN_POINT ( 'NONE',  ( -1.054774247047244540, 0.07405724077823318263, 0.8169291338045038264 ) ) ;
#4067 = AXIS2_PLACEMENT_3D ( 'NONE', #43576, #32603, #25399 ) ;
#4069 = DIRECTION ( 'NONE',  ( 0.000000000000000000, 0.000000000000000000, 1.000000000000000000 ) ) ;
#4068 = AXIS2_PLACEMENT_3D ( 'NONE', #37085, #22707, #4234 ) ;
#4070 = CARTESIAN_POINT ( 'NONE',  ( 0.8759842519685039353, 0.1787899950787401882, 0.3124999999462365619 ) ) ;
#4071 = DIRECTION ( 'NONE',  ( 1.000000000000000000, 0.000000000000000000, 0.000000000000000000 ) ) ;
#4072 = CARTESIAN_POINT ( 'NONE',  ( -0.6971942568897637749, 2.189545951927499583E-17, 1.262303149552535420 ) ) ;
#4073 = CARTESIAN_POINT ( 'NONE',  ( -0.1476377952755905387, -0.4889725119976395251, -0.8550419489141688478 ) ) ;
#4074 = CARTESIAN_POINT ( 'NONE',  ( 0.09432024557780893659, 0.09445537554013619386, 0.2309772516917621976 ) ) ;
#4075 = CARTESIAN_POINT ( 'NONE',  ( -0.7495606340400177148, -0.1264236179284866091, 1.547736220418677089 ) ) ;
#4076 = CARTESIAN_POINT ( 'NONE',  ( -0.9873396505805591694, 0.1113553986120547346, 1.855314960522393530 ) ) ;
#4077 = VERTEX_POINT ( 'NONE', #5814 ) ;
#4078 = DIRECTION ( 'NONE',  ( 0.000000000000000000, 0.7071067811867007835, 0.7071067811863941399 ) ) ;
#4079 = CARTESIAN_POINT ( 'NONE',  ( 0.8759842519685039353, -0.1787899950787401882, 1.434547244040724534 ) ) ;
#4080 = CARTESIAN_POINT ( 'NONE',  ( -0.03607162715213074744, -0.09851382849536771680, 0.1546661156032805018 ) ) ;
#4081 = FACE_OUTER_BOUND ( 'NONE', #15189, .T. ) ;
#4082 = ORIENTED_EDGE ( 'NONE', *, *, #37554, .T. ) ;
#4083 = VERTEX_POINT ( 'NONE', #15259 ) ;
#4084 = CARTESIAN_POINT ( 'NONE',  ( -0.07405724077823318263, -0.8248031495525351975, 0.1787899950787401604 ) ) ;
#4085 = CARTESIAN_POINT ( 'NONE',  ( 0.1787899950787401604, -0.4163385826234020093, -0.07405724077823318263 ) ) ;
#4086 = CARTESIAN_POINT ( 'NONE',  ( -0.1787899950787401604, -0.9822834645131651721, 0.07405724077823318263 ) ) ;
#4087 = CARTESIAN_POINT ( 'NONE',  ( 0.1270800023317771588, -0.2126422347798960499, -0.1270800023317771588 ) ) ;
#4088 = CARTESIAN_POINT ( 'NONE',  ( -0.1574803149606299191, 0.1299212598425196763, 0.000000000000000000 ) ) ;
#4089 = VECTOR ( 'NONE', #22486, 39.37007874015748143 ) ;
#4090 = CARTESIAN_POINT ( 'NONE',  ( 0.07405724077823318263, -0.01771653537930735489, -0.1787899950787401604 ) ) ;
#4091 = CARTESIAN_POINT ( 'NONE',  ( 1.033464566929133799, 0.000000000000000000, 1.348425196850393748 ) ) ;
#4092 = EDGE_CURVE ( 'NONE', #31834, #16796, #4674, .T. ) ;
#4093 = CARTESIAN_POINT ( 'NONE',  ( 0.6971942568897626646, -0.07405724077823297447, 0.7135826771115916234 ) ) ;
#4094 = EDGE_CURVE ( 'NONE', #47236, #43450, #29902, .T. ) ;
#4096 = CARTESIAN_POINT ( 'NONE',  ( 1.033464566929133799, 0.000000000000000000, 1.771653543199558811 ) ) ;
#4095 = CARTESIAN_POINT ( 'NONE',  ( -0.9862283977965377035, 0.1251934987593905646, 0.03937007874015843734 ) ) ;
#4098 = DIRECTION ( 'NONE',  ( 0.000000000000000000, 0.000000000000000000, 1.000000000000000000 ) ) ;
#4097 = DIRECTION ( 'NONE',  ( 0.000000000000000000, 0.000000000000000000, 1.000000000000000000 ) ) ;
#4099 = FACE_OUTER_BOUND ( 'NONE', #40715, .T. ) ;
#4100 = CARTESIAN_POINT ( 'NONE',  ( 0.7495606340400177148, 0.1264236179284866091, 1.852854330654897685 ) ) ;
#4101 = CARTESIAN_POINT ( 'NONE',  ( -0.6195511811023656223, 0.9842519685039375910, -0.7135826771653542844 ) ) ;
#4102 = ADVANCED_FACE ( 'NONE', ( #42216 ), #15498, .T. ) ;
#4103 = ORIENTED_EDGE ( 'NONE', *, *, #34435, .T. ) ;
#4104 = EDGE_CURVE ( 'NONE', #17196, #38075, #16827, .T. ) ;
#4105 = CARTESIAN_POINT ( 'NONE',  ( 0.7185039370078746268, 0.06523048226347956391, 0.06643700787401589369 ) ) ;
#4106 = FACE_OUTER_BOUND ( 'NONE', #1892, .T. ) ;
#4108 = CARTESIAN_POINT ( 'NONE',  ( -0.1264236179284866091, -0.2760826771115909573, 0.1264236179284866091 ) ) ;
#4107 = CARTESIAN_POINT ( 'NONE',  ( -0.1574803149606300301, -0.9650590550105839771, -0.06523048226347956391 ) ) ;
#4109 = CARTESIAN_POINT ( 'NONE',  ( 0.8759842519685039353, 0.000000000000000000, 4.498031496062992574 ) ) ;
#4110 = CARTESIAN_POINT ( 'NONE',  ( 0.1264236179284866091, -1.284940944828125930, 0.1264236179284866091 ) ) ;
#4111 = CARTESIAN_POINT ( 'NONE',  ( 0.9500414927467378812, 0.1787899950787401604, 0.2312992125446618197 ) ) ;
#4112 = CARTESIAN_POINT ( 'NONE',  ( 0.7646288533564489232, 0.1113553986120547346, 1.117125984144440975 ) ) ;
#4113 = CARTESIAN_POINT ( 'NONE',  ( -0.9500414927467378812, 0.1787899950787401604, 1.643700787347811998 ) ) ;
#4114 = ORIENTED_EDGE ( 'NONE', *, *, #15099, .T. ) ;
#4115 = CARTESIAN_POINT ( 'NONE',  ( -0.8759842519685039353, -0.1787899950787401882, 1.158956692859621995 ) ) ;
#4116 = CARTESIAN_POINT ( 'NONE',  ( -1.033464566929133799, 0.000000000000000000, 0.3248031496062992463 ) ) ;
#4117 = CARTESIAN_POINT ( 'NONE',  ( 1.002407869896990045, -0.1264236179284866091, 0.06151574797773248782 ) ) ;
#4118 = CARTESIAN_POINT ( 'NONE',  ( -1.002407869896990045, 0.1264236179284866091, 1.129429133804503937 ) ) ;
#4119 = CARTESIAN_POINT ( 'NONE',  ( -0.08985779549332877092, -0.2436148098455482858, -0.03544556188504763977 ) ) ;
#4120 = CARTESIAN_POINT ( 'NONE',  ( 0.7495606340400177148, -0.1264236179284866091, 0.4453740156942677664 ) ) ;
#4121 = CARTESIAN_POINT ( 'NONE',  ( -0.6971942568897626646, 0.07405724077823318263, 0.2755905511273391006 ) ) ;
#4122 = CARTESIAN_POINT ( 'NONE',  ( -1.002407869896990045, -0.1264236179284866091, 0.6865157479777322935 ) ) ;
#4123 = CARTESIAN_POINT ( 'NONE',  ( 0.7185039370078739607, 1.928577636452523993E-17, 1.712598425089322918 ) ) ;
#4124 = VERTEX_POINT ( 'NONE', #31468 ) ;
#4125 = LINE ( 'NONE', #8196, #30626 ) ;
#4126 = ORIENTED_EDGE ( 'NONE', *, *, #29729, .F. ) ;
#4127 = CARTESIAN_POINT ( 'NONE',  ( 0.6971942568897637749, 2.189545951927499583E-17, 0.8735236219934803259 ) ) ;
#4128 = CARTESIAN_POINT ( 'NONE',  ( 1.054774247047244540, 0.07405724077823318263, 1.053149606245450176 ) ) ;
#4129 = CARTESIAN_POINT ( 'NONE',  ( -0.9500414927467377701, -0.1787899950787401604, 1.904527559001354398 ) ) ;
#4130 = ORIENTED_EDGE ( 'NONE', *, *, #20495, .F. ) ;
#4131 = EDGE_CURVE ( 'NONE', #38785, #19774, #16494, .T. ) ;
#4132 = CARTESIAN_POINT ( 'NONE',  ( 0.8759842519685039353, -0.1787899950787401882, 1.902066929080094448 ) ) ;
#4133 = CARTESIAN_POINT ( 'NONE',  ( -0.6971942568897626646, 0.07405724077823318263, 0.8710629920722218200 ) ) ;
#4134 = CARTESIAN_POINT ( 'NONE',  ( -0.8759842519685039353, 0.000000000000000000, 0.000000000000000000 ) ) ;
#4135 = CARTESIAN_POINT ( 'NONE',  ( 0.1264236179284866091, -1.409080661142624091, -0.1264236179284866091 ) ) ;
#4136 = AXIS2_PLACEMENT_3D ( 'NONE', #27125, #30952, #45286 ) ;
#4137 = VERTEX_POINT ( 'NONE', #41315 ) ;
#4138 = FACE_BOUND ( 'NONE', #41382, .T. ) ;
#4139 = CARTESIAN_POINT ( 'NONE',  ( -0.07405724077823318263, -0.3474409448281265411, 0.1787899950787401604 ) ) ;
#4140 = FACE_OUTER_BOUND ( 'NONE', #39147, .T. ) ;
#4141 = ORIENTED_EDGE ( 'NONE', *, *, #5419, .F. ) ;
#4142 = CARTESIAN_POINT ( 'NONE',  ( 1.054774247047244540, -0.07405724077823318263, 1.122047244040725644 ) ) ;
#4144 = ADVANCED_FACE ( 'NONE', ( #23147 ), #37762, .T. ) ;
#4143 = DIRECTION ( 'NONE',  ( -1.000000000000000000, 0.000000000000000000, -7.051687499798870116E-15 ) ) ;
#4145 = CARTESIAN_POINT ( 'NONE',  ( 0.7495606340400177148, 0.1264236179284866091, 0.1943897637257641919 ) ) ;
#4146 = CARTESIAN_POINT ( 'NONE',  ( 3.284318927891251994E-17, -1.688484251914740275, 0.1787899950787401882 ) ) ;
#4147 = CARTESIAN_POINT ( 'NONE',  ( 0.1787899950787401604, -1.749999999946236340, -0.07405724077823318263 ) ) ;
#4148 = APPLICATION_PROTOCOL_DEFINITION ( 'draft international standard', 'automotive_design', 1998, #35549 ) ;
#4149 = CARTESIAN_POINT ( 'NONE',  ( 0.002061874009640850183, -0.03163730233503504047, -0.1377906290935765887 ) ) ;
#4150 = EDGE_CURVE ( 'NONE', #1170, #31291, #25492, .T. ) ;
#4151 = CARTESIAN_POINT ( 'NONE',  ( -1.054774247047244540, 0.07405724077823318263, 0.6988188975840318173 ) ) ;
#4152 = PRESENTATION_STYLE_ASSIGNMENT (( #37229 ) ) ;
#4153 = CARTESIAN_POINT ( 'NONE',  ( 0.1797182628040039087, -1.401126486748399458, 0.07444174185955046430 ) ) ;
#4154 = CIRCLE ( 'NONE', #8875, 0.04921259842519691563 ) ;
#4155 = CARTESIAN_POINT ( 'NONE',  ( 1.054774247047244540, 0.07405724077823318263, 1.368110236166710125 ) ) ;
#4156 = CARTESIAN_POINT ( 'NONE',  ( 0.8019270111902716547, -0.1787899950787401604, 1.663385826717890925 ) ) ;
#4157 = CIRCLE ( 'NONE', #26400, 0.1377952755905509641 ) ;
#4158 = CONICAL_SURFACE ( 'NONE', #12620, 0.2471922904502826812, 0.5235987755982992597 ) ;
#4159 = CARTESIAN_POINT ( 'NONE',  ( -0.8107537697050254399, -0.1574803149606297803, 1.641240157372788389 ) ) ;
#4160 = EDGE_CURVE ( 'NONE', #14831, #38424, #44591, .T. ) ;
#4162 = CARTESIAN_POINT ( 'NONE',  ( -0.8216075239166756861, 0.1504252669448082336, 1.979429770448521531 ) ) ;
#4161 = CARTESIAN_POINT ( 'NONE',  ( -0.7185039370078739607, 1.928577636452523993E-17, 1.437007873908220601 ) ) ;
#4163 = LINE ( 'NONE', #19012, #46583 ) ;
#4164 = DIRECTION ( 'NONE',  ( -5.298843091159153171E-15, -2.355041373848512214E-15, 1.000000000000000000 ) ) ;
#4165 = FACE_OUTER_BOUND ( 'NONE', #41792, .T. ) ;
#4166 = CARTESIAN_POINT ( 'NONE',  ( -0.9412147342319837628, -0.1574803149606297803, 1.921751968396409493 ) ) ;
#4167 = CARTESIAN_POINT ( 'NONE',  ( -0.9873396505805591694, 0.1113553986120547346, 0.9498031494987716483 ) ) ;
#4168 = CARTESIAN_POINT ( 'NONE',  ( -0.8759842519685039353, 0.1787899950787401882, 1.173720472387181246 ) ) ;
#4169 = CARTESIAN_POINT ( 'NONE',  ( 1.033464566929134687, -0.06523048226347956391, 0.6668307085538908163 ) ) ;
#4170 = EDGE_LOOP ( 'NONE', ( #24125, #6496, #36526, #10576 ) ) ;
#4171 = CARTESIAN_POINT ( 'NONE',  ( 0.1113553986120547346, -0.05216535433070866590, 0.1113553986120547346 ) ) ;
#4172 = VERTEX_POINT ( 'NONE', #9654 ) ;
#4173 = CARTESIAN_POINT ( 'NONE',  ( -0.07444174185955065859, -0.1117564080082424360, 0.1797182628040039087 ) ) ;
#4174 = CARTESIAN_POINT ( 'NONE',  ( -0.7185039370078739607, 1.928577636452523993E-17, 1.604330708661417360 ) ) ;
#4175 = CARTESIAN_POINT ( 'NONE',  ( 0.9500414927467378812, -0.1787899950787401604, 1.550196850339937926 ) ) ;
#4176 = LINE ( 'NONE', #10695, #1333 ) ;
#4177 = CARTESIAN_POINT ( 'NONE',  ( 0.1600714537641758362, -0.09473400225499722938, 0.1168739604209794586 ) ) ;
#4178 = CARTESIAN_POINT ( 'NONE',  ( 1.033464566929134687, -0.06523048226347956391, 1.926673228238929170 ) ) ;
#4179 = CARTESIAN_POINT ( 'NONE',  ( 0.1787899950787401604, -0.1751968503399373434, -0.07405724077823318263 ) ) ;
#4180 = VERTEX_POINT ( 'NONE', #43155 ) ;
#4181 = CARTESIAN_POINT ( 'NONE',  ( -0.7185039370078746268, 0.06523048226347956391, 0.3813976377952755237 ) ) ;
#4182 = CARTESIAN_POINT ( 'NONE',  ( -0.05264611394417081230, -0.07553294269950990014, 0.2550375247538705925 ) ) ;
#4183 = CARTESIAN_POINT ( 'NONE',  ( 0.9500414927467377701, 0.1787899950787401604, 0.8218503936470251681 ) ) ;
#4184 = CARTESIAN_POINT ( 'NONE',  ( 0.1787899950787401604, -1.799212598371432659, 0.07405724077823318263 ) ) ;
#4185 = CARTESIAN_POINT ( 'NONE',  ( -0.6971942568897648851, 0.07405724077823318263, 1.343503936954111744 ) ) ;
#4186 = ORIENTED_EDGE ( 'NONE', *, *, #24423, .F. ) ;
#4187 = EDGE_CURVE ( 'NONE', #26918, #1846, #23978, .T. ) ;
#4188 = CARTESIAN_POINT ( 'NONE',  ( -0.1387951811623720499, 0.2153607970560884322, -0.3149606299212598381 ) ) ;
#4189 = CARTESIAN_POINT ( 'NONE',  ( -0.6971942568897637749, 2.189545951927499583E-17, 0.3617125983714334359 ) ) ;
#4190 = VECTOR ( 'NONE', #3913, 39.37007874015748143 ) ;
#4191 = CARTESIAN_POINT ( 'NONE',  ( 0.7646288533564489232, 0.1113553986120547346, 0.8021653542231811373 ) ) ;
#4192 = CARTESIAN_POINT ( 'NONE',  ( -0.1787899950787401882, -0.9612460154733326601, 0.000000000000000000 ) ) ;
#4193 = ORIENTED_EDGE ( 'NONE', *, *, #17844, .F. ) ;
#4194 = CARTESIAN_POINT ( 'NONE',  ( -0.1787899950787401604, 0.1545275591088816070, -0.07405724077823318263 ) ) ;
#4195 = CIRCLE ( 'NONE', #42468, 0.09940944881889761386 ) ;
#4196 = MECHANICAL_DESIGN_GEOMETRIC_PRESENTATION_REPRESENTATION (  '', ( #6491 ), #44754 ) ;
#4197 = ORIENTED_EDGE ( 'NONE', *, *, #32553, .F. ) ;
#4198 = LINE ( 'NONE', #30373, #20248 ) ;
#4199 = DIRECTION ( 'NONE',  ( 0.000000000000000000, -1.000000000000000000, 0.000000000000000000 ) ) ;
#4200 = CARTESIAN_POINT ( 'NONE',  ( 0.1787899950787401882, -0.4975393700249764461, -2.189545951927503898E-17 ) ) ;
#4201 = ADVANCED_FACE ( 'NONE', ( #21360 ), #17048, .F. ) ;
#4202 = CARTESIAN_POINT ( 'NONE',  ( -0.8019270111902716547, -0.1787899950787401604, 0.09350393695411057804 ) ) ;
#4203 = CARTESIAN_POINT ( 'NONE',  ( -0.8759842519685039353, -0.1574803149606299191, 0.9448818897637796255 ) ) ;
#4204 = PLANE ( 'NONE',  #12619 ) ;
#4205 = CARTESIAN_POINT ( 'NONE',  ( -0.1797182628040039087, -0.9828194001342275277, 0.07444174185955065859 ) ) ;
#4206 = CARTESIAN_POINT ( 'NONE',  ( -0.9873396505805591694, 0.1113553986120547346, 1.540354330601133803 ) ) ;
#4207 = CARTESIAN_POINT ( 'NONE',  ( 0.7495606340400177148, 0.1264236179284866091, 0.9473425196312755814 ) ) ;
#4208 = CARTESIAN_POINT ( 'NONE',  ( 1.054774247047244096, 0.000000000000000000, 1.360728346402929168 ) ) ;
#4209 = AXIS2_PLACEMENT_3D ( 'NONE', #9083, #5720, #1643 ) ;
#4210 = EDGE_CURVE ( 'NONE', #34447, #9079, #42757, .T. ) ;
#4211 = CARTESIAN_POINT ( 'NONE',  ( 0.7185039370078746268, -0.06523048226347956391, 1.409940944881891367 ) ) ;
#4213 = CARTESIAN_POINT ( 'NONE',  ( -0.4330708661417337901, 0.1574803149606330277, 0.9891732283464568232 ) ) ;
#4212 = CARTESIAN_POINT ( 'NONE',  ( 0.7332986977137438966, -0.09085960385660657446, 1.985055299648571969 ) ) ;
#4214 = CARTESIAN_POINT ( 'NONE',  ( 0.7185039370078739607, 0.000000000000000000, 4.498031496062992574 ) ) ;
#4216 = CARTESIAN_POINT ( 'NONE',  ( 0.1608764814808671395, 0.07794373349925551309, 0.1405880446287834651 ) ) ;
#4215 = CARTESIAN_POINT ( 'NONE',  ( 0.6971942568897648851, -0.07405724077823297447, 0.7923228345919055560 ) ) ;
#4218 = TOROIDAL_SURFACE ( 'NONE', #9594, 0.01968503937007873988, 0.009842519685039369942 ) ;
#4217 = CARTESIAN_POINT ( 'NONE',  ( -0.1787899950787401604, -0.7509842519147402751, -0.07405724077823318263 ) ) ;
#4219 = ORIENTED_EDGE ( 'NONE', *, *, #21706, .F. ) ;
#4220 = CARTESIAN_POINT ( 'NONE',  ( 0.7185039370078739607, 1.928577636452523993E-17, 0.9350393700787401619 ) ) ;
#4221 = DIRECTION ( 'NONE',  ( 0.000000000000000000, 0.000000000000000000, -1.000000000000000000 ) ) ;
#4222 = CARTESIAN_POINT ( 'NONE',  ( 0.8759842519685039353, -0.1787899950787401882, 1.193405511757259951 ) ) ;
#4223 = CARTESIAN_POINT ( 'NONE',  ( 0.02847999302535491814, 0.6072747502901004735, -0.8119482170283445210 ) ) ;
#4224 = CARTESIAN_POINT ( 'NONE',  ( -0.1113553986120547346, -1.646653543307086798, -0.1113553986120547346 ) ) ;
#4225 = CARTESIAN_POINT ( 'NONE',  ( -1.033464566929133799, 0.000000000000000000, 0.5216535433070865757 ) ) ;
#4226 = CARTESIAN_POINT ( 'NONE',  ( 0.2204724409448818867, 0.1591122789105269553, 0.000000000000000000 ) ) ;
#4227 = CARTESIAN_POINT ( 'NONE',  ( -0.6971942568897626646, 0.07405724077823318263, 0.1968503936470238913 ) ) ;
#4228 = DIRECTION ( 'NONE',  ( 0.000000000000000000, 0.000000000000000000, -1.000000000000000000 ) ) ;
#4229 = CARTESIAN_POINT ( 'NONE',  ( 0.1574803149606300301, -0.3105314959554651977, -0.06523048226347956391 ) ) ;
#4230 = CARTESIAN_POINT ( 'NONE',  ( -0.8019270111902717657, 0.1787899950787401604, 1.687992125930489307 ) ) ;
#4231 = CARTESIAN_POINT ( 'NONE',  ( -0.8759842519685039353, -0.1787899950787401882, 0.8390748030958424808 ) ) ;
#4232 = CARTESIAN_POINT ( 'NONE',  ( -0.8019270111902717657, -0.1787899950787401604, 0.5265748030958428139 ) ) ;
#4233 = CARTESIAN_POINT ( 'NONE',  ( 0.1574803149606299191, -0.03740157469562260112, -1.928577636452523993E-17 ) ) ;
#4234 = DIRECTION ( 'NONE',  ( 1.000000000000000000, 0.000000000000000000, 0.000000000000000000 ) ) ;
#4235 = CARTESIAN_POINT ( 'NONE',  ( 1.002407869896990045, -0.1264236179284866091, 0.05659448813521283234 ) ) ;
#4236 = CARTESIAN_POINT ( 'NONE',  ( 0.2066929133858267653, -0.5221178280460081478, -0.9040880104747088808 ) ) ;
#4237 = CARTESIAN_POINT ( 'NONE',  ( -0.1264236179284866091, -0.4543562516938055573, -0.1264236179284866091 ) ) ;
#4238 = CARTESIAN_POINT ( 'NONE',  ( -0.2343560426797417495, -0.08955971028938346234, 0.03132653569787429565 ) ) ;
#4239 = VECTOR ( 'NONE', #39476, 39.37007874015748143 ) ;
#4240 = CARTESIAN_POINT ( 'NONE',  ( 0.2559055118110236116, -4.594920972184172978E-16, -0.02740704184215071032 ) ) ;
#4241 = CARTESIAN_POINT ( 'NONE',  ( -0.8019270111902717657, 0.1787899950787401604, 0.3887795275052913224 ) ) ;
#4242 = ORIENTED_EDGE ( 'NONE', *, *, #38095, .T. ) ;
#4243 = EDGE_CURVE ( 'NONE', #20918, #23956, #35192, .T. ) ;
#4244 = CARTESIAN_POINT ( 'NONE',  ( -1.054774247047244540, 0.07405724077823318263, 1.446850393647023836 ) ) ;
#4245 = ORIENTED_EDGE ( 'NONE', *, *, #837, .F. ) ;
#4246 = CIRCLE ( 'NONE', #26398, 0.1377952755905511861 ) ;
#4247 = CARTESIAN_POINT ( 'NONE',  ( -0.1264236179284866091, -1.348917322780881944, -0.1264236179284866091 ) ) ;
#4248 = CARTESIAN_POINT ( 'NONE',  ( -0.1787899950787401604, -1.577755905458046115, -0.07405724077823318263 ) ) ;
#4249 = ( BOUNDED_CURVE ( )  B_SPLINE_CURVE ( 2, ( #20318, #1380, #13157, #8826, #38771, #5932, #16038, #30665, #13380 ),
 .UNSPECIFIED., .F., .T. ) 
 B_SPLINE_CURVE_WITH_KNOTS ( ( 3, 2, 2, 2, 3 ),
 ( 0.2000000000000000111, 0.2025000000000000133, 0.2049999999999999878, 0.2074999999999999900, 0.2099999999999999922 ),
 .UNSPECIFIED. ) 
 CURVE ( )  GEOMETRIC_REPRESENTATION_ITEM ( )  RATIONAL_B_SPLINE_CURVE ( ( 1.000000000000000000, 0.9238795325112869605, 1.000000000000000000, 0.9238795325112869605, 1.000000000000000000, 0.9238795325112869605, 1.000000000000000000, 0.9238795325112869605, 1.000000000000000000 ) ) 
 REPRESENTATION_ITEM ( '' )  ) ;
#4250 = EDGE_CURVE ( 'NONE', #712, #6130, #37711, .T. ) ;
#4251 = CARTESIAN_POINT ( 'NONE',  ( 0.5358894627757212481, -3.032960542342102697E-32, 0.09842519685039370636 ) ) ;
#4252 = DIRECTION ( 'NONE',  ( 0.002429491788810000594, -0.9185655563779312471, -0.3952611999750921257 ) ) ;
#4253 = LINE ( 'NONE', #3579, #24031 ) ;
#4254 = CARTESIAN_POINT ( 'NONE',  ( -0.7646288533564489232, 0.1113553986120547346, 1.117125984144440975 ) ) ;
#4255 = CARTESIAN_POINT ( 'NONE',  ( 0.8019270111902717657, 0.1787899950787401604, 0.5118110235682844511 ) ) ;
#4256 = CARTESIAN_POINT ( 'NONE',  ( -1.033464566929134687, -0.06523048226347956391, 1.493602362097197211 ) ) ;
#4257 = CARTESIAN_POINT ( 'NONE',  ( -0.1574803149606297803, -0.2219488188976377896, 0.06523048226347956391 ) ) ;
#4258 = EDGE_LOOP ( 'NONE', ( #4245, #23915, #16817, #44504 ) ) ;
#4259 = CARTESIAN_POINT ( 'NONE',  ( 0.7185039370078746268, 0.06523048226347956391, 1.946358267609010095 ) ) ;
#4260 = ORIENTED_EDGE ( 'NONE', *, *, #34875, .T. ) ;
#4261 = CARTESIAN_POINT ( 'NONE',  ( 0.8759842519685039353, -0.1574803149606300579, 0.03937007874015747977 ) ) ;
#4262 = ADVANCED_FACE ( 'NONE', ( #39565 ), #35497, .T. ) ;
#4263 = CARTESIAN_POINT ( 'NONE',  ( -1.002407869896990045, -0.1264236179284866091, 0.9276574802611967652 ) ) ;
#4264 = CARTESIAN_POINT ( 'NONE',  ( 0.7185039370078739607, 1.928577636452523993E-17, 1.013779527559055094 ) ) ;
#4265 = CARTESIAN_POINT ( 'NONE',  ( -0.1574803149606299191, 0.3171096708378827178, -3.631137952917390166 ) ) ;
#4266 = CARTESIAN_POINT ( 'NONE',  ( -0.1574803149606300301, -0.5713582676090083190, -0.06523048226347956391 ) ) ;
#4267 = CARTESIAN_POINT ( 'NONE',  ( -0.1345756647787081373, -0.08956061689499753009, 0.09177022885256264084 ) ) ;
#4268 = ORIENTED_EDGE ( 'NONE', *, *, #43106, .F. ) ;
#4269 = CARTESIAN_POINT ( 'NONE',  ( -0.2801604161619160038, 0.1329643277078509933, 0.7738411923581678398 ) ) ;
#4270 = AXIS2_PLACEMENT_3D ( 'NONE', #26413, #43887, #40980 ) ;
#4271 = ORIENTED_EDGE ( 'NONE', *, *, #16678, .T. ) ;
#4272 = CARTESIAN_POINT ( 'NONE',  ( -0.9873396505805591694, 0.1113553986120547346, 1.776574803042078488 ) ) ;
#4273 = CARTESIAN_POINT ( 'NONE',  ( 0.4736248074375630224, 0.4457451269443653552, -1.671447902550338815 ) ) ;
#4274 = CARTESIAN_POINT ( 'NONE',  ( -0.07405724077823318263, -0.7460629920722210429, 0.1787899950787401604 ) ) ;
#4275 = CARTESIAN_POINT ( 'NONE',  ( 0.1113553986120547346, -1.193897637795275690, 0.1113553986120547346 ) ) ;
#4277 = ( BOUNDED_CURVE ( )  B_SPLINE_CURVE ( 2, ( #44654, #45381, #33700, #38203, #8490, #26734, #15715, #42003, #15472 ),
 .UNSPECIFIED., .F., .T. ) 
 B_SPLINE_CURVE_WITH_KNOTS ( ( 3, 2, 2, 2, 3 ),
 ( 0.2800000000000000266, 0.2824999999999999734, 0.2849999999999999756, 0.2874999999999999778, 0.2899999999999999800 ),
 .UNSPECIFIED. ) 
 CURVE ( )  GEOMETRIC_REPRESENTATION_ITEM ( )  RATIONAL_B_SPLINE_CURVE ( ( 1.000000000000000000, 0.9238795325112869605, 1.000000000000000000, 0.9238795325112869605, 1.000000000000000000, 0.9238795325112869605, 1.000000000000000000, 0.9238795325112869605, 1.000000000000000000 ) ) 
 REPRESENTATION_ITEM ( '' )  ) ;
#4276 = CARTESIAN_POINT ( 'NONE',  ( 0.7185039370078746268, 0.06523048226347956391, 1.158956692805858113 ) ) ;
#4278 = LINE ( 'NONE', #30688, #6833 ) ;
#4279 = CARTESIAN_POINT ( 'NONE',  ( -0.8019270111902717657, -0.1787899950787401604, 0.4822834645131655606 ) ) ;
#4280 = ORIENTED_EDGE ( 'NONE', *, *, #27532, .F. ) ;
#4281 = ORIENTED_EDGE ( 'NONE', *, *, #43584, .T. ) ;
#4282 = ORIENTED_EDGE ( 'NONE', *, *, #8277, .F. ) ;
#4283 = CARTESIAN_POINT ( 'NONE',  ( -0.8019270111902717657, 0.1787899950787401604, 1.771653543253322249 ) ) ;
#4284 = CARTESIAN_POINT ( 'NONE',  ( 0.8019270111902717657, -0.1787899950787401604, 1.707677165300566235 ) ) ;
#4285 = CARTESIAN_POINT ( 'NONE',  ( -0.6971942568897637749, 2.189545951927499583E-17, 0.7947834645131652831 ) ) ;
#4286 = CARTESIAN_POINT ( 'NONE',  ( -1.284448818897637956, -0.3937007874015748254, -1.181102362204724310 ) ) ;
#4287 = CARTESIAN_POINT ( 'NONE',  ( 1.054774247047244540, 0.07405724077823318263, 0.3444881889226146243 ) ) ;
#4288 = CARTESIAN_POINT ( 'NONE',  ( -0.9412147342319837628, 0.1574803149606300301, 1.503444881782235232 ) ) ;
#4289 = CARTESIAN_POINT ( 'NONE',  ( -0.8019270111902716547, -0.1787899950787401604, 1.190944881836001112 ) ) ;
#4290 = CARTESIAN_POINT ( 'NONE',  ( -0.6971942568897626646, -0.07405724077823297447, 0.9104330708123776761 ) ) ;
#4291 = CARTESIAN_POINT ( 'NONE',  ( 0.8107537697050254399, 0.1574803149606300301, 0.9178149605223947516 ) ) ;
#4292 = FACE_OUTER_BOUND ( 'NONE', #11893, .T. ) ;
#4293 = CARTESIAN_POINT ( 'NONE',  ( -0.6971942568897637749, 2.189545951927499583E-17, 1.660925196796630088 ) ) ;
#4294 = CARTESIAN_POINT ( 'NONE',  ( -0.8759842519685039353, 0.1574803149606299191, 1.820866141624755796 ) ) ;
#4295 = ORIENTED_EDGE ( 'NONE', *, *, #5961, .T. ) ;
#4296 = CARTESIAN_POINT ( 'NONE',  ( -0.9412147342319837628, 0.1574803149606300301, 1.631397637795275468 ) ) ;
#4297 = CARTESIAN_POINT ( 'NONE',  ( -0.7185039370078739607, 1.928577636452523993E-17, 0.2263779527559055260 ) ) ;
#4298 = CARTESIAN_POINT ( 'NONE',  ( 0.8019270111902716547, -0.1787899950787401604, 1.589566929080094226 ) ) ;
#4299 = CARTESIAN_POINT ( 'NONE',  ( -0.02050768364047031445, -0.09851382972412085770, 0.1561483119320291324 ) ) ;
#4300 = LINE ( 'NONE', #5270, #3456 ) ;
#4301 = ORIENTED_EDGE ( 'NONE', *, *, #47118, .T. ) ;
#4302 = ADVANCED_FACE ( 'NONE', ( #20891 ), #35532, .F. ) ;
#4303 = ORIENTED_EDGE ( 'NONE', *, *, #18459, .T. ) ;
#4304 = EDGE_CURVE ( 'NONE', #24004, #44436, #35757, .T. ) ;
#4305 = ORIENTED_EDGE ( 'NONE', *, *, #13909, .F. ) ;
#4306 = CARTESIAN_POINT ( 'NONE',  ( 3.284318927891251994E-17, -0.9010826771115905132, 0.1787899950787401882 ) ) ;
#4307 = CARTESIAN_POINT ( 'NONE',  ( 0.1787899950787401882, -0.3794291338045042705, -2.189545951927503898E-17 ) ) ;
#4308 = CARTESIAN_POINT ( 'NONE',  ( -0.1787899950787401604, -1.144685039316316599, -0.07405724077823318263 ) ) ;
#4309 = VERTEX_POINT ( 'NONE', #17534 ) ;
#4310 = CARTESIAN_POINT ( 'NONE',  ( 0.9500414927467378812, 0.1787899950787401604, 1.801181102308441861 ) ) ;
#4311 = CARTESIAN_POINT ( 'NONE',  ( 3.301370929368692659E-17, -0.3455162505279275598, 0.1797182628040039365 ) ) ;
#4312 = CARTESIAN_POINT ( 'NONE',  ( 0.1574803149606300301, 0.1077755905511811885, 0.06523048226347956391 ) ) ;
#4313 = CARTESIAN_POINT ( 'NONE',  ( -0.9412147342319837628, -0.1574803149606297803, 0.8981299211523156023 ) ) ;
#4314 = CARTESIAN_POINT ( 'NONE',  ( 0.6971942568897626646, -0.07405724077823297447, 0.8316929133320636325 ) ) ;
#4316 = SURFACE_STYLE_USAGE ( .BOTH. , #8166 ) ;
#4315 = CARTESIAN_POINT ( 'NONE',  ( -0.7185039370078739607, 1.928577636452523993E-17, 1.082677165246803241 ) ) ;
#4318 = CARTESIAN_POINT ( 'NONE',  ( 1.614954907737318939E-16, 0.1574803149606340824, 0.3937007874015748254 ) ) ;
#4317 = CARTESIAN_POINT ( 'NONE',  ( 0.1864803149606299171, 1.086379535891623949, -0.03715491745706173132 ) ) ;
#4319 = CARTESIAN_POINT ( 'NONE',  ( 0.2204724409448818867, -0.1591122789105269553, 0.000000000000000000 ) ) ;
#4320 = CARTESIAN_POINT ( 'NONE',  ( 0.9500414927467378812, -0.1787899950787401604, 1.751968503883245765 ) ) ;
#4321 = CARTESIAN_POINT ( 'NONE',  ( -0.1574803149606299191, 0.000000000000000000, -0.0009999999999999347518 ) ) ;
#4322 = EDGE_LOOP ( 'NONE', ( #23508, #9476 ) ) ;
#4323 = CARTESIAN_POINT ( 'NONE',  ( 1.033464566929134687, -0.06523048226347956391, 0.04675196850393704279 ) ) ;
#4324 = CARTESIAN_POINT ( 'NONE',  ( 0.5113546317124669782, 1.205361022782824954E-17, -0.09842519685039370636 ) ) ;
#4325 = CARTESIAN_POINT ( 'NONE',  ( 3.284318927891251994E-17, -0.2317913385289138151, 0.1787899950787401882 ) ) ;
#4326 = CARTESIAN_POINT ( 'NONE',  ( 0.1587072800412982765, 0.1427694538647063249, 0.03362159989229027840 ) ) ;
#4327 = CARTESIAN_POINT ( 'NONE',  ( 0.1787899950787401882, -1.240649606245448622, -2.189545951927503898E-17 ) ) ;
#4328 = CARTESIAN_POINT ( 'NONE',  ( 0.8759842519685039353, -0.1787899950787401882, 0.1747047243556852092 ) ) ;
#4329 = CARTESIAN_POINT ( 'NONE',  ( 0.8759842519685039353, 0.1574803149606299191, 1.112204724301921299 ) ) ;
#4330 = CARTESIAN_POINT ( 'NONE',  ( -0.6971942568897648851, -0.07405724077823297447, 1.815944881835999558 ) ) ;
#4331 = EDGE_LOOP ( 'NONE', ( #6224, #7246, #9355, #26838 ) ) ;
#4332 = CARTESIAN_POINT ( 'NONE',  ( -1.054774247047244540, 0.07405724077823318263, 1.249999999946235896 ) ) ;
#4333 = DIRECTION ( 'NONE',  ( 0.000000000000000000, 0.000000000000000000, -1.000000000000000000 ) ) ;
#4334 = CARTESIAN_POINT ( 'NONE',  ( 1.054774247047244096, 0.000000000000000000, 1.326279527505291433 ) ) ;
#4335 = CARTESIAN_POINT ( 'NONE',  ( 0.8759842519685039353, -0.1787899950787401882, 1.902066929080094448 ) ) ;
#4336 = CARTESIAN_POINT ( 'NONE',  ( -0.9500414927467378812, -0.1787899950787401604, 1.038385826717890259 ) ) ;
#4337 = CARTESIAN_POINT ( 'NONE',  ( -0.07262103558693376593, -0.09842518455345698747, -0.1633777802328124917 ) ) ;
#4338 = CARTESIAN_POINT ( 'NONE',  ( 0.9873396505805591694, 0.1113553986120547346, 0.04429133847515007855 ) ) ;
#4339 = CARTESIAN_POINT ( 'NONE',  ( 1.054774247047244096, 0.000000000000000000, 0.4601377952218267953 ) ) ;
#4340 = CARTESIAN_POINT ( 'NONE',  ( -1.054774247047244096, 0.000000000000000000, 0.4158464566391496531 ) ) ;
#4341 = CARTESIAN_POINT ( 'NONE',  ( 0.8759842519685039353, -0.1574803149606299191, 1.683070866034204638 ) ) ;
#4342 = ORIENTED_EDGE ( 'NONE', *, *, #33149, .T. ) ;
#4343 = ORIENTED_EDGE ( 'NONE', *, *, #45808, .T. ) ;
#4344 = DIRECTION ( 'NONE',  ( 0.000000000000000000, 0.000000000000000000, 1.000000000000000000 ) ) ;
#4345 = CARTESIAN_POINT ( 'NONE',  ( -0.7185039370078739607, 1.928577636452523993E-17, 0.06889763779527559306 ) ) ;
#4346 = CARTESIAN_POINT ( 'NONE',  ( 0.6971942568897648851, -0.07405724077823297447, 1.033464566875371027 ) ) ;
#4347 = CARTESIAN_POINT ( 'NONE',  ( -1.054774247047244540, -0.07405724077823318263, 1.948818897584033705 ) ) ;
#4348 = ORIENTED_EDGE ( 'NONE', *, *, #28268, .T. ) ;
#4349 = ADVANCED_FACE ( 'NONE', ( #32168 ), #41573, .T. ) ;
#4350 = CARTESIAN_POINT ( 'NONE',  ( 0.000000000000000000, 0.000000000000000000, -0.3149606299212598381 ) ) ;
#4351 = ADVANCED_FACE ( 'NONE', ( #8 ), #36296, .T. ) ;
#4352 = CARTESIAN_POINT ( 'NONE',  ( 0.1555213372790614501, -0.1050481006241407722, -0.09364190366147240319 ) ) ;
#4353 = CARTESIAN_POINT ( 'NONE',  ( -0.7185039370078739607, 1.928577636452523993E-17, 1.870078740049952559 ) ) ;
#4354 = CARTESIAN_POINT ( 'NONE',  ( 0.1264236179284866091, -1.497663338307978487, 0.1264236179284866091 ) ) ;
#4355 = ORIENTED_EDGE ( 'NONE', *, *, #17582, .F. ) ;
#4356 = CARTESIAN_POINT ( 'NONE',  ( 0.1787899950787401882, -0.3745078739619845942, -2.189545951927503898E-17 ) ) ;
#4357 = ADVANCED_FACE ( 'NONE', ( #25697 ), #29564, .T. ) ;
#4358 = CARTESIAN_POINT ( 'NONE',  ( -0.2559097037360847371, 0.05003845355613480150, -0.3122011391401430802 ) ) ;
#4359 = CARTESIAN_POINT ( 'NONE',  ( -0.2801779484932495623, -0.1329283866310996265, 0.7737913416150018486 ) ) ;
#4360 = ORIENTED_EDGE ( 'NONE', *, *, #40924, .F. ) ;
#4361 = CARTESIAN_POINT ( 'NONE',  ( 0.8759842519685039353, -0.1787899950787401882, 1.193405511757259951 ) ) ;
#4362 = EDGE_CURVE ( 'NONE', #19564, #25854, #22784, .T. ) ;
#4363 = CARTESIAN_POINT ( 'NONE',  ( -0.7646288533564489232, 0.1113553986120547346, 0.8415354329633386588 ) ) ;
#4364 = DIRECTION ( 'NONE',  ( 1.000000000000000000, 0.000000000000000000, -1.822029033848725275E-16 ) ) ;
#4365 = VECTOR ( 'NONE', #28429, 39.37007874015748143 ) ;
#4366 = CARTESIAN_POINT ( 'NONE',  ( 0.003457534521343415441, -0.09882139917207719004, -0.1044452803222859771 ) ) ;
#4367 = CARTESIAN_POINT ( 'NONE',  ( 0.6971942568897637749, 2.189545951927499583E-17, 0.1205708660879689087 ) ) ;
#4368 = CARTESIAN_POINT ( 'NONE',  ( -0.1264236179284866091, 0.1361949294085564865, -0.1264236179284866091 ) ) ;
#4369 = CARTESIAN_POINT ( 'NONE',  ( -0.1264236179284866091, -1.698326771599779628, -0.1264236179284866091 ) ) ;
#4370 = CARTESIAN_POINT ( 'NONE',  ( -0.8070866141732283561, 0.3779527559055118058, 0.7574803149606299524 ) ) ;
#4371 = CARTESIAN_POINT ( 'NONE',  ( 0.9412147342319837628, -0.1574803149606297803, 1.341043307086613456 ) ) ;
#4372 = CARTESIAN_POINT ( 'NONE',  ( -0.8759842519685039353, 0.1787899950787401882, 0.6668307086076534773 ) ) ;
#4374 = LINE ( 'NONE', #44870, #28589 ) ;
#4373 = CARTESIAN_POINT ( 'NONE',  ( -0.1113553986120547346, -0.8198818897637795144, -0.1113553986120547346 ) ) ;
#4375 = CARTESIAN_POINT ( 'NONE',  ( 0.07444174185955046430, -1.351913888323203139, -0.1797182628040039087 ) ) ;
#4376 = DIRECTION ( 'NONE',  ( 1.000000000000000000, -0.000000000000000000, -0.000000000000000000 ) ) ;
#4377 = CARTESIAN_POINT ( 'NONE',  ( 0.1602931993194442739, 0.07955613945526338049, 0.1377952755905511861 ) ) ;
#4378 = CARTESIAN_POINT ( 'NONE',  ( 0.7495606340400177148, 0.1264236179284866091, 1.380413385773007873 ) ) ;
#4379 = CARTESIAN_POINT ( 'NONE',  ( 0.6971942568897648851, 0.07405724077823318263, 1.653543307032850462 ) ) ;
#4380 = CYLINDRICAL_SURFACE ( 'NONE', #7763, 0.1574803149606299191 ) ;
#4381 = DIRECTION ( 'NONE',  ( 0.000000000000000000, 0.000000000000000000, -1.000000000000000000 ) ) ;
#4382 = CARTESIAN_POINT ( 'NONE',  ( 0.8070866141732283561, -0.0009842519685049383633, -0.7574803149606299524 ) ) ;
#4384 = DIRECTION ( 'NONE',  ( 0.000000000000000000, -0.6156614753256598460, -0.7880107536067206819 ) ) ;
#4383 = CARTESIAN_POINT ( 'NONE',  ( 0.1113553986120547346, -0.8297244093412913246, 0.1113553986120547346 ) ) ;
#4385 = DIRECTION ( 'NONE',  ( -0.000000000000000000, -0.7880107536067200158, 0.6156614753256608452 ) ) ;
#4386 = CARTESIAN_POINT ( 'NONE',  ( 0.8759842519685039353, 0.1787899950787401882, 0.2682086613635594752 ) ) ;
#4387 = ( BOUNDED_CURVE ( )  B_SPLINE_CURVE ( 2, ( #45691, #15800, #30658, #45218, #30427, #27062, #23212, #8814, #38288 ),
 .UNSPECIFIED., .F., .T. ) 
 B_SPLINE_CURVE_WITH_KNOTS ( ( 3, 2, 2, 2, 3 ),
 ( 0.4799999999999999822, 0.4824999999999999845, 0.4849999999999999867, 0.4874999999999999889, 0.4899999999999999911 ),
 .UNSPECIFIED. ) 
 CURVE ( )  GEOMETRIC_REPRESENTATION_ITEM ( )  RATIONAL_B_SPLINE_CURVE ( ( 1.000000000000000000, 0.9238795325112869605, 1.000000000000000000, 0.9238795325112869605, 1.000000000000000000, 0.9238795325112869605, 1.000000000000000000, 0.9238795325112869605, 1.000000000000000000 ) ) 
 REPRESENTATION_ITEM ( '' )  ) ;
#4388 = CARTESIAN_POINT ( 'NONE',  ( 0.7331294905545601148, -0.08922581545105803813, 0.03937007875388988387 ) ) ;
#4389 = DIRECTION ( 'NONE',  ( 0.000000000000000000, 0.000000000000000000, 1.000000000000000000 ) ) ;
#4390 = AXIS2_PLACEMENT_3D ( 'NONE', #10675, #40108, #14018 ) ;
#4391 = CARTESIAN_POINT ( 'NONE',  ( -0.8759842519685039353, 0.1574803149606299191, 0.9547244093412913246 ) ) ;
#4392 = CARTESIAN_POINT ( 'NONE',  ( -1.002407869896990045, 0.1264236179284866091, 1.286909448765133801 ) ) ;
#4393 = CARTESIAN_POINT ( 'NONE',  ( 1.033464566929133799, 0.000000000000000000, 0.5905511809948347235 ) ) ;
#4394 = ORIENTED_EDGE ( 'NONE', *, *, #25772, .T. ) ;
#4395 = CARTESIAN_POINT ( 'NONE',  ( 0.8759842519685039353, 0.1574803149606299191, 1.397637795275590511 ) ) ;
#4396 = CARTESIAN_POINT ( 'NONE',  ( -0.1613934693438489332, -0.4404989748867991217, -0.9678556472999616522 ) ) ;
#4397 = EDGE_LOOP ( 'NONE', ( #42354, #25632, #16710, #37834 ) ) ;
#4398 = CARTESIAN_POINT ( 'NONE',  ( 0.07444174185955065859, -0.02809499068540773775, 0.1797182628040039087 ) ) ;
#4400 = EDGE_CURVE ( 'NONE', #26106, #15853, #7688, .T. ) ;
#4399 = DIRECTION ( 'NONE',  ( 0.000000000000000000, -6.938893903907227392E-16, -1.000000000000000000 ) ) ;
#4401 = CARTESIAN_POINT ( 'NONE',  ( 0.1264236179284866091, -1.240649606245448622, -0.1264236179284866091 ) ) ;
#4402 = CARTESIAN_POINT ( 'NONE',  ( -0.8107537697050254399, 0.1574803149606300301, 1.114665354223180804 ) ) ;
#4403 = CARTESIAN_POINT ( 'NONE',  ( -0.7646288533564489232, -0.1113553986120547346, 1.254921259842519676 ) ) ;
#4404 = CARTESIAN_POINT ( 'NONE',  ( 0.8759842519685039353, 0.1574803149606299191, 0.2460629920184571051 ) ) ;
#4406 = CARTESIAN_POINT ( 'NONE',  ( -0.2471922904502826812, -0.03219022224904102836, 0.1427165354330708902 ) ) ;
#4405 = CARTESIAN_POINT ( 'NONE',  ( 0.1583858528204782623, -0.1411902173418210782, 0.03633609477024421497 ) ) ;
#4407 = CARTESIAN_POINT ( 'NONE',  ( 0.9500414927467377701, -0.1787899950787401604, 0.05905511805647267048 ) ) ;
#4408 = CARTESIAN_POINT ( 'NONE',  ( 0.1787899950787401604, -0.1013779527021420185, 0.07405724077823318263 ) ) ;
#4409 = ORIENTED_EDGE ( 'NONE', *, *, #4243, .T. ) ;
#4410 = AXIS2_PLACEMENT_3D ( 'NONE', #21098, #12991, #35031 ) ;
#4411 = CARTESIAN_POINT ( 'NONE',  ( -0.9412147342319837628, 0.1574803149606300301, 0.3715551181102362266 ) ) ;
#4412 = CARTESIAN_POINT ( 'NONE',  ( 0.7495606340400177148, -0.1264236179284866091, 0.9178149605761574126 ) ) ;
#4413 = CARTESIAN_POINT ( 'NONE',  ( -1.054774247047244096, 0.000000000000000000, 1.518208661363559031 ) ) ;
#4414 = CARTESIAN_POINT ( 'NONE',  ( 0.1113553986120547346, 0.006889763887054606122, -0.1113553986120547346 ) ) ;
#4415 = CARTESIAN_POINT ( 'NONE',  ( -0.8019270111902717657, -0.1787899950787401604, 1.235236220418678199 ) ) ;
#4416 = ORIENTED_EDGE ( 'NONE', *, *, #40562, .F. ) ;
#4417 = EDGE_CURVE ( 'NONE', #4137, #38595, #486, .T. ) ;
#4418 = CARTESIAN_POINT ( 'NONE',  ( -0.1657973489137827550, 0.1997733981813884230, -0.3128311589625774047 ) ) ;
#4419 = CARTESIAN_POINT ( 'NONE',  ( 1.033464566929133799, 0.000000000000000000, 0.8661417321759370402 ) ) ;
#4420 = CARTESIAN_POINT ( 'NONE',  ( -0.1787899950787401882, -0.9218759367331751386, 0.000000000000000000 ) ) ;
#4421 = ORIENTED_EDGE ( 'NONE', *, *, #36897, .F. ) ;
#4422 = CARTESIAN_POINT ( 'NONE',  ( -0.1264236179284866091, 0.03395669296714932950, -0.1264236179284866091 ) ) ;
#4423 = ORIENTED_EDGE ( 'NONE', *, *, #15019, .T. ) ;
#4424 = VERTEX_POINT ( 'NONE', #26405 ) ;
#4425 = ADVANCED_FACE ( 'NONE', ( #36701 ), #15141, .T. ) ;
#4426 = CYLINDRICAL_SURFACE ( 'NONE', #28701, 0.1574803149606299191 ) ;
#4427 = CARTESIAN_POINT ( 'NONE',  ( 0.9873396505805591694, -0.1113553986120547346, 0.1131889762704257896 ) ) ;
#4428 = DIRECTION ( 'NONE',  ( 0.000000000000000000, 0.000000000000000000, 1.000000000000000000 ) ) ;
#4429 = CARTESIAN_POINT ( 'NONE',  ( -1.002407869896990045, -0.1264236179284866091, 0.1796259841982051075 ) ) ;
#4430 = CARTESIAN_POINT ( 'NONE',  ( -0.7646288533564489232, -0.1113553986120547346, 0.9399606299212598381 ) ) ;
#4431 = DIRECTION ( 'NONE',  ( 1.000000000000000000, 0.000000000000000000, -1.822029033848725275E-16 ) ) ;
#4432 = CARTESIAN_POINT ( 'NONE',  ( 0.1270800023317771588, -1.049256408008242270, 0.1270800023317771588 ) ) ;
#4433 = CARTESIAN_POINT ( 'NONE',  ( 1.181102362204724310, 0.000000000000000000, -0.9842519685039370358 ) ) ;
#4434 = CARTESIAN_POINT ( 'NONE',  ( -0.7185039370078746268, -0.06523048226347956391, 1.557578740049953225 ) ) ;
#4435 = CARTESIAN_POINT ( 'NONE',  ( 0.6971942568897626646, 0.07405724077823318263, 0.9104330708123776761 ) ) ;
#4436 = CARTESIAN_POINT ( 'NONE',  ( 1.033464566929133799, 0.000000000000000000, 0.5118110235145204578 ) ) ;
#4437 = CARTESIAN_POINT ( 'NONE',  ( 1.033464566929134687, -0.06523048226347956391, 1.345964566929133133 ) ) ;
#4439 = DIRECTION ( 'NONE',  ( -0.000000000000000000, 1.000000000000000000, -0.000000000000000000 ) ) ;
#4438 = CARTESIAN_POINT ( 'NONE',  ( 0.7275679244916588573, 0.06900988131655333424, 1.981898831895456681 ) ) ;
#4440 = DIRECTION ( 'NONE',  ( 0.000000000000000000, 0.000000000000000000, -1.000000000000000000 ) ) ;
#4441 = CARTESIAN_POINT ( 'NONE',  ( 0.9500414927467377701, 0.1787899950787401604, 0.8562992125446617919 ) ) ;
#4442 = CARTESIAN_POINT ( 'NONE',  ( 0.8019270111902716547, -0.1787899950787401604, 1.786417322780882388 ) ) ;
#4443 = CARTESIAN_POINT ( 'NONE',  ( 3.284318927891251994E-17, -0.7386811023084409733, 0.1787899950787401882 ) ) ;
#4444 = FACE_OUTER_BOUND ( 'NONE', #303, .T. ) ;
#4445 = EDGE_LOOP ( 'NONE', ( #3241, #15111, #25556, #32618 ) ) ;
#4446 = CARTESIAN_POINT ( 'NONE',  ( -0.7185039370078739607, 1.928577636452523993E-17, 0.9744094488188976833 ) ) ;
#4447 = CARTESIAN_POINT ( 'NONE',  ( 0.6971942568897637749, 2.189545951927499583E-17, 1.183562992072220599 ) ) ;
#4448 = PLANE ( 'NONE',  #30350 ) ;
#4449 = CARTESIAN_POINT ( 'NONE',  ( 0.1113553986120547346, -1.666338582677165503, 0.1113553986120547346 ) ) ;
#4450 = DIRECTION ( 'NONE',  ( -1.000000000000000000, 3.469446951953613794E-15, 1.144917494144692682E-16 ) ) ;
#4451 = AXIS2_PLACEMENT_3D ( 'NONE', #29922, #3987, #36380 ) ;
#4452 = ORIENTED_EDGE ( 'NONE', *, *, #12571, .F. ) ;
#4453 = CARTESIAN_POINT ( 'NONE',  ( -1.054774247047244540, 0.07405724077823318263, 0.2608267715997796832 ) ) ;
#4454 = EDGE_LOOP ( 'NONE', ( #30362, #10226, #35204, #29981 ) ) ;
#4455 = AXIS2_PLACEMENT_3D ( 'NONE', #5889, #2280, #16908 ) ;
#4456 = CARTESIAN_POINT ( 'NONE',  ( 0.1787899950787401604, -1.479330708607653699, -0.07405724077823318263 ) ) ;
#4457 = CARTESIAN_POINT ( 'NONE',  ( -0.6971942568897637749, 2.189545951927499583E-17, 1.892224409395055096 ) ) ;
#4458 = CARTESIAN_POINT ( 'NONE',  ( -0.6971942568897648851, 0.07405724077823318263, 0.9448818897100165204 ) ) ;
#4459 = CARTESIAN_POINT ( 'NONE',  ( -1.054774247047244540, 0.07405724077823318263, 0.5019685038832442103 ) ) ;
#4460 = EDGE_CURVE ( 'NONE', #894, #45730, #7163, .T. ) ;
#4461 = CARTESIAN_POINT ( 'NONE',  ( -0.8107537697050234415, -0.1574803149606297803, 0.1550196850393702197 ) ) ;
#4462 = MANIFOLD_SOLID_BREP ( 'ISO 10513 M8 Lock Nut', #14905 ) ;
#4463 = CARTESIAN_POINT ( 'NONE',  ( 0.000000000000000000, 0.09842519685039370636, 0.000000000000000000 ) ) ;
#4464 = CARTESIAN_POINT ( 'NONE',  ( 0.05613986198065472333, 0.07767250275969861395, -0.2530207064393421579 ) ) ;
#4465 = CARTESIAN_POINT ( 'NONE',  ( -0.2664436179446793562, 0.1586070934160171142, -0.9304076372001184314 ) ) ;
#4466 = CARTESIAN_POINT ( 'NONE',  ( 3.284318927891251994E-17, -0.5183326296465614602, 0.1787899950787401882 ) ) ;
#4467 = CARTESIAN_POINT ( 'NONE',  ( 0.06899553503110708585, -0.09842519685039370636, 0.1342099080972281588 ) ) ;
#4468 = CARTESIAN_POINT ( 'NONE',  ( -0.9412147342319837628, 0.1574803149606300301, 1.897145669183811778 ) ) ;
#4469 = DIRECTION ( 'NONE',  ( -1.000000000000000000, 0.000000000000000000, 0.000000000000000000 ) ) ;
#4470 = EDGE_CURVE ( 'NONE', #32150, #42931, #18249, .T. ) ;
#4471 = CARTESIAN_POINT ( 'NONE',  ( -1.033464566929134687, 0.06523048226347956391, 1.970964566821606034 ) ) ;
#4472 = CARTESIAN_POINT ( 'NONE',  ( -1.054774247047244096, 0.000000000000000000, 0.2583661416785200671 ) ) ;
#4473 = CARTESIAN_POINT ( 'NONE',  ( -0.07405724077823318263, -1.780635779252860651, 0.1787899950787401604 ) ) ;
#4474 = ORIENTED_EDGE ( 'NONE', *, *, #40182, .T. ) ;
#4475 = FACE_OUTER_BOUND ( 'NONE', #37850, .T. ) ;
#4476 = EDGE_LOOP ( 'NONE', ( #32160, #30356, #15719, #2883 ) ) ;
#4477 = CARTESIAN_POINT ( 'NONE',  ( -0.9500414927467377701, 0.1787899950787401604, 1.569881889710015299 ) ) ;
#4478 = ORIENTED_EDGE ( 'NONE', *, *, #27532, .T. ) ;
#4479 = CARTESIAN_POINT ( 'NONE',  ( -0.07405724077823318263, -1.312007873961984705, -0.1787899950787401604 ) ) ;
#4480 = CARTESIAN_POINT ( 'NONE',  ( 0.1787899950787401604, -1.592519684985606254, -0.07405724077823318263 ) ) ;
#4481 = AXIS2_PLACEMENT_3D ( 'NONE', #6050, #17084, #13724 ) ;
#4482 = DIRECTION ( 'NONE',  ( 1.822029033848725028E-16, 0.000000000000000000, 1.000000000000000000 ) ) ;
#4483 = CARTESIAN_POINT ( 'NONE',  ( 0.7646288533564489232, -0.1113553986120547346, 0.5068897637795275468 ) ) ;
#4484 = FACE_BOUND ( 'NONE', #14477, .T. ) ;
#4485 = CARTESIAN_POINT ( 'NONE',  ( -1.033464566929134687, -0.06523048226347956391, 1.060531495955465031 ) ) ;
#4486 = VECTOR ( 'NONE', #16161, 39.37007874015748143 ) ;
#4487 = CARTESIAN_POINT ( 'NONE',  ( 1.054774247047244096, 0.000000000000000000, 0.5782480314422993040 ) ) ;
#4489 = CARTESIAN_POINT ( 'NONE',  ( -0.8759842519685039353, 0.000000000000000000, 0.000000000000000000 ) ) ;
#4488 = CARTESIAN_POINT ( 'NONE',  ( -0.1574803149606300301, -0.3056102362204722867, -0.06523048226347956391 ) ) ;
#4490 = CARTESIAN_POINT ( 'NONE',  ( -0.7185039370078739607, 1.928577636452523993E-17, 1.879921259842519676 ) ) ;
#4491 = VERTEX_POINT ( 'NONE', #44335 ) ;
#4492 = DIRECTION ( 'NONE',  ( 0.000000000000000000, -1.000000000000000000, 0.000000000000000000 ) ) ;
#4493 = CARTESIAN_POINT ( 'NONE',  ( -1.054774247047244096, 0.000000000000000000, 0.9719488188438739629 ) ) ;
#4494 = CARTESIAN_POINT ( 'NONE',  ( 1.033464566929133799, 0.000000000000000000, 0.9940944881889764995 ) ) ;
#4495 = AXIS2_PLACEMENT_3D ( 'NONE', #30589, #15731, #19531 ) ;
#4496 = LINE ( 'NONE', #22739, #29482 ) ;
#4497 = EDGE_CURVE ( 'NONE', #827, #6014, #27115, .T. ) ;
#4499 = DIRECTION ( 'NONE',  ( 0.000000000000000000, -0.7880107536067207930, 0.6156614753256598460 ) ) ;
#4498 = CARTESIAN_POINT ( 'NONE',  ( -1.033464566929133799, 1.928577636452524610E-17, 2.869337061179095023E-17 ) ) ;
#4500 = CARTESIAN_POINT ( 'NONE',  ( -0.1564850196914947811, -0.08956157248042134755, 0.05474941646345270196 ) ) ;
#4501 = EDGE_LOOP ( 'NONE', ( #6202, #25796, #24719, #33065 ) ) ;
#4502 = CARTESIAN_POINT ( 'NONE',  ( 0.1637370647600281393, -0.08228083545669484522, -0.1377952755905511584 ) ) ;
#4503 = CARTESIAN_POINT ( 'NONE',  ( 1.054774247047244096, 0.000000000000000000, 0.6914370078202519698 ) ) ;
#4504 = EDGE_LOOP ( 'NONE', ( #35377, #46108, #45244, #25612 ) ) ;
#4505 = CARTESIAN_POINT ( 'NONE',  ( -0.09216395708618665972, 0.09383642490574134465, -0.2322221854328508361 ) ) ;
#4506 = CARTESIAN_POINT ( 'NONE',  ( -0.7185039370078739607, 0.000000000000000000, -2.869337061179095023E-17 ) ) ;
#4507 = CARTESIAN_POINT ( 'NONE',  ( 0.07405724077823318263, -1.548228346402928723, -0.1787899950787401604 ) ) ;
#4509 = CARTESIAN_POINT ( 'NONE',  ( -0.07405724077823318263, -0.9429133857730090940, 0.1787899950787401604 ) ) ;
#4508 = CARTESIAN_POINT ( 'NONE',  ( -0.1113553986120547346, -1.006889763672000004, -0.1113553986120547346 ) ) ;
#4510 = CARTESIAN_POINT ( 'NONE',  ( 0.9412147342319837628, -0.1574803149606297803, 1.094980314853103653 ) ) ;
#4511 = CARTESIAN_POINT ( 'NONE',  ( 0.8759842519685039353, 0.1574803149606299191, 1.830708661417322913 ) ) ;
#4512 = CARTESIAN_POINT ( 'NONE',  ( -1.054774247047244096, 0.000000000000000000, 0.4945866141194645849 ) ) ;
#4513 = ORIENTED_EDGE ( 'NONE', *, *, #9113, .T. ) ;
#4514 = CARTESIAN_POINT ( 'NONE',  ( -0.8759842519685039353, -0.1787899950787401882, 1.788877952702141672 ) ) ;
#4515 = ORIENTED_EDGE ( 'NONE', *, *, #37372, .F. ) ;
#4516 = EDGE_CURVE ( 'NONE', #39441, #47216, #7454, .T. ) ;
#4517 = CARTESIAN_POINT ( 'NONE',  ( 0.9500414927467378812, 0.1787899950787401604, 1.687992125930489307 ) ) ;
#4518 = ORIENTED_EDGE ( 'NONE', *, *, #44084, .T. ) ;
#4519 = CARTESIAN_POINT ( 'NONE',  ( -1.054774247047244096, 0.000000000000000000, 0.8932086613635591421 ) ) ;
#4520 = CARTESIAN_POINT ( 'NONE',  ( -0.08476992594631420352, -0.2465534299915450589, -0.3121915932859496423 ) ) ;
#4521 = CARTESIAN_POINT ( 'NONE',  ( -0.6971942568897637749, 2.189545951927499583E-17, 1.419783464513165505 ) ) ;
#4522 = DIRECTION ( 'NONE',  ( -0.000000000000000000, 1.000000000000000000, -0.000000000000000000 ) ) ;
#4523 = CARTESIAN_POINT ( 'NONE',  ( -0.8759842519685039353, -0.1787899950787401882, 1.193405511757259951 ) ) ;
#4524 = EDGE_CURVE ( 'NONE', #39582, #3381, #29455, .T. ) ;
#4525 = CARTESIAN_POINT ( 'NONE',  ( -1.002407869896990045, -0.1264236179284866091, 0.06151574797773248782 ) ) ;
#4526 = ADVANCED_FACE ( 'NONE', ( #12501 ), #2154, .F. ) ;
#4527 = VECTOR ( 'NONE', #17737, 39.37007874015748143 ) ;
#4528 = CARTESIAN_POINT ( 'NONE',  ( -0.9873396505805591694, 0.1113553986120547346, 1.658464566821606256 ) ) ;
#4529 = CARTESIAN_POINT ( 'NONE',  ( -0.9500414927467378812, -0.1787899950787401604, 1.555118110182455382 ) ) ;
#4530 = CARTESIAN_POINT ( 'NONE',  ( -0.9500414927467378812, 0.1787899950787401604, 0.07381889758403178958 ) ) ;
#4531 = EDGE_LOOP ( 'NONE', ( #18099, #28878, #35700, #13225 ) ) ;
#4532 = CARTESIAN_POINT ( 'NONE',  ( -0.7185039370078746268, -0.06523048226347956391, 1.567421259842519676 ) ) ;
#4533 = CARTESIAN_POINT ( 'NONE',  ( 0.9412147342319837628, -0.1574803149606297803, 0.9768700786326298680 ) ) ;
#4534 = CARTESIAN_POINT ( 'NONE',  ( 1.054774247047244540, -0.07405724077823318263, 1.599409448765134911 ) ) ;
#4535 = CARTESIAN_POINT ( 'NONE',  ( -0.2333336438806818958, -0.09842519685039370636, 0.05221132881278717219 ) ) ;
#4536 = CARTESIAN_POINT ( 'NONE',  ( 1.033464566929133799, 0.000000000000000000, 0.1968503935932602311 ) ) ;
#4537 = EDGE_LOOP ( 'NONE', ( #25418, #27235, #19220, #19481 ) ) ;
#4538 = CARTESIAN_POINT ( 'NONE',  ( 1.033464566929133799, 0.000000000000000000, 0.2755905510735752184 ) ) ;
#4539 = ORIENTED_EDGE ( 'NONE', *, *, #21973, .T. ) ;
#4540 = EDGE_CURVE ( 'NONE', #829, #21151, #16422, .T. ) ;
#4541 = CIRCLE ( 'NONE', #17594, 0.1377952755905510196 ) ;
#4542 = ( BOUNDED_CURVE ( )  B_SPLINE_CURVE ( 2, ( #40469, #22269, #26375, #8129, #4511, #36906, #45010, #4059, #12222 ),
 .UNSPECIFIED., .F., .F. ) 
 B_SPLINE_CURVE_WITH_KNOTS ( ( 3, 2, 2, 2, 3 ),
 ( 0.9200000000000000400, 0.9224999999999999867, 0.9250000000000000444, 0.9274999999999999911, 0.9300000000000000488 ),
 .UNSPECIFIED. ) 
 CURVE ( )  GEOMETRIC_REPRESENTATION_ITEM ( )  RATIONAL_B_SPLINE_CURVE ( ( 1.000000000000000000, 0.9238795325112869605, 1.000000000000000000, 0.9238795325112869605, 1.000000000000000000, 0.9238795325112869605, 1.000000000000000000, 0.9238795325112869605, 1.000000000000000000 ) ) 
 REPRESENTATION_ITEM ( '' )  ) ;
#4543 = EDGE_CURVE ( 'NONE', #27121, #2057, #46998, .T. ) ;
#4544 = ORIENTED_EDGE ( 'NONE', *, *, #35034, .F. ) ;
#4545 = AXIS2_PLACEMENT_3D ( 'NONE', #16240, #35154, #45663 ) ;
#4546 = ORIENTED_EDGE ( 'NONE', *, *, #46961, .F. ) ;
#4547 = CARTESIAN_POINT ( 'NONE',  ( -0.07405724077823318263, -0.9035433070328510174, 0.1787899950787401604 ) ) ;
#4548 = CARTESIAN_POINT ( 'NONE',  ( 0.1264236179284866091, -1.088090551127338657, 0.1264236179284866091 ) ) ;
#4549 = CARTESIAN_POINT ( 'NONE',  ( 0.8019270111902717657, -0.1787899950787401604, 1.820866141678520789 ) ) ;
#4550 = CARTESIAN_POINT ( 'NONE',  ( 0.07444174185955046430, -0.3282918410791086927, -0.1797182628040039087 ) ) ;
#4551 = CARTESIAN_POINT ( 'NONE',  ( 0.1113553986120547346, 0.1446850393700787329, 0.1113553986120547346 ) ) ;
#4552 = CARTESIAN_POINT ( 'NONE',  ( 1.033464566929133799, 1.928577636452524610E-17, 4.498031496062992574 ) ) ;
#4553 = CARTESIAN_POINT ( 'NONE',  ( 0.8759842519685039353, 0.1787899950787401882, 0.7800196849856062542 ) ) ;
#4554 = ( BOUNDED_CURVE ( )  B_SPLINE_CURVE ( 2, ( #20692, #42259, #28633, #43190, #13742, #9691, #21158, #10159, #9458 ),
 .UNSPECIFIED., .F., .T. ) 
 B_SPLINE_CURVE_WITH_KNOTS ( ( 3, 2, 2, 2, 3 ),
 ( 0.2399999999999999911, 0.2424999999999999933, 0.2449999999999999956, 0.2474999999999999978, 0.2500000000000000000 ),
 .UNSPECIFIED. ) 
 CURVE ( )  GEOMETRIC_REPRESENTATION_ITEM ( )  RATIONAL_B_SPLINE_CURVE ( ( 1.000000000000000000, 0.9238795325112869605, 1.000000000000000000, 0.9238795325112869605, 1.000000000000000000, 0.9238795325112869605, 1.000000000000000000, 0.9238795325112869605, 1.000000000000000000 ) ) 
 REPRESENTATION_ITEM ( '' )  ) ;
#4555 = CIRCLE ( 'NONE', #9964, 0.04921259842519686706 ) ;
#4557 = LINE ( 'NONE', #36708, #16259 ) ;
#4556 = DIRECTION ( 'NONE',  ( 0.000000000000000000, -1.000000000000000000, 0.000000000000000000 ) ) ;
#4558 = DIRECTION ( 'NONE',  ( 0.000000000000000000, 0.000000000000000000, -1.000000000000000000 ) ) ;
#4559 = CARTESIAN_POINT ( 'NONE',  ( -1.033464566929133799, 0.000000000000000000, 0.07874015737278799998 ) ) ;
#4560 = CARTESIAN_POINT ( 'NONE',  ( 1.002407869896990045, 0.1264236179284866091, 1.764271653489543290 ) ) ;
#4561 = ORIENTED_EDGE ( 'NONE', *, *, #23328, .T. ) ;
#4562 = CARTESIAN_POINT ( 'NONE',  ( 0.7185039370078746268, 0.06523048226347956391, 0.1451771653543309226 ) ) ;
#4563 = CARTESIAN_POINT ( 'NONE',  ( -0.8759842519685039353, 0.000000000000000000, 0.000000000000000000 ) ) ;
#4564 = CARTESIAN_POINT ( 'NONE',  ( 0.1787899950787401604, -0.2982283464029296116, -0.07405724077823318263 ) ) ;
#4565 = FACE_OUTER_BOUND ( 'NONE', #13758, .T. ) ;
#4566 = VECTOR ( 'NONE', #29486, 39.37007874015748143 ) ;
#4567 = CARTESIAN_POINT ( 'NONE',  ( 3.284318927891251994E-17, -1.289862204670645607, 0.1787899950787401882 ) ) ;
#4568 = CARTESIAN_POINT ( 'NONE',  ( 1.002407869896990045, -0.1264236179284866091, 0.2977362204186775885 ) ) ;
#4569 = CARTESIAN_POINT ( 'NONE',  ( 0.8759842519685039353, 0.1574803149606299191, 0.05905511811023622659 ) ) ;
#4570 = ADVANCED_FACE ( 'NONE', ( #16553 ), #16092, .T. ) ;
#4571 = CARTESIAN_POINT ( 'NONE',  ( -0.9500414927467378812, -0.1787899950787401604, 1.825787401521040243 ) ) ;
#4572 = ORIENTED_EDGE ( 'NONE', *, *, #20233, .T. ) ;
#4573 = CARTESIAN_POINT ( 'NONE',  ( -0.8759842519685039353, -0.1787899950787401882, 1.277066929080094448 ) ) ;
#4574 = EDGE_CURVE ( 'NONE', #19636, #4842, #20134, .T. ) ;
#4575 = CARTESIAN_POINT ( 'NONE',  ( 0.9500414927467378812, -0.1787899950787401604, 1.240157480261197431 ) ) ;
#4576 = CARTESIAN_POINT ( 'NONE',  ( 0.8759842519685039353, 0.1787899950787401882, 1.921751968450173376 ) ) ;
#4577 = CARTESIAN_POINT ( 'NONE',  ( -1.002407869896990045, -0.1264236179284866091, 1.080216535379306952 ) ) ;
#4578 = FACE_OUTER_BOUND ( 'NONE', #46724, .T. ) ;
#4579 = CARTESIAN_POINT ( 'NONE',  ( 0.02733683484473901221, -0.09840216969744279563, -0.1767045507392152881 ) ) ;
#4580 = CARTESIAN_POINT ( 'NONE',  ( 0.000000000000000000, 0.000000000000000000, -0.2357204724409448504 ) ) ;
#4581 = CARTESIAN_POINT ( 'NONE',  ( 1.002407869896990045, -0.1264236179284866091, 0.4158464566391496531 ) ) ;
#4582 = CARTESIAN_POINT ( 'NONE',  ( -0.9500414927467377701, -0.1787899950787401604, 0.4084645668753704162 ) ) ;
#4583 = CARTESIAN_POINT ( 'NONE',  ( 0.8759842519685039353, 0.1574803149606299191, 1.663385826664125933 ) ) ;
#4584 = ORIENTED_EDGE ( 'NONE', *, *, #32997, .F. ) ;
#4585 = ORIENTED_EDGE ( 'NONE', *, *, #8223, .T. ) ;
#4586 = DIRECTION ( 'NONE',  ( -3.469446951953614189E-15, -1.000000000000000000, -1.118797478067273468E-31 ) ) ;
#4587 = CARTESIAN_POINT ( 'NONE',  ( -0.8759842519685039353, -0.1574803149606299191, 0.07874015748031495954 ) ) ;
#4588 = CARTESIAN_POINT ( 'NONE',  ( 0.7495606340400177148, -0.1264236179284866091, 1.154035433017102319 ) ) ;
#4589 = CARTESIAN_POINT ( 'NONE',  ( 0.000000000000000000, 0.000000000000000000, 0.000000000000000000 ) ) ;
#4590 = VERTEX_POINT ( 'NONE', #8400 ) ;
#4591 = CARTESIAN_POINT ( 'NONE',  ( 1.002407869896990045, -0.1264236179284866091, 1.985728346402929168 ) ) ;
#4592 = CARTESIAN_POINT ( 'NONE',  ( -1.002407869896990045, 0.1264236179284866091, 0.8981299212060788184 ) ) ;
#4593 = VECTOR ( 'NONE', #29577, 39.37007874015748143 ) ;
#4594 = ADVANCED_FACE ( 'NONE', ( #26644 ), #41438, .T. ) ;
#4595 = CARTESIAN_POINT ( 'NONE',  ( 0.1526809758745832635, -0.1331472126641777554, -0.04497281396056834746 ) ) ;
#4596 = CARTESIAN_POINT ( 'NONE',  ( -1.002407869896990045, 0.1264236179284866091, 0.02706692908009476414 ) ) ;
#4597 = CARTESIAN_POINT ( 'NONE',  ( -0.1787899950787401604, -1.436147590276483088, -0.07405724077823318263 ) ) ;
#4598 = ORIENTED_EDGE ( 'NONE', *, *, #7307, .F. ) ;
#4599 = DIRECTION ( 'NONE',  ( 0.000000000000000000, 0.000000000000000000, -1.000000000000000000 ) ) ;
#4600 = CARTESIAN_POINT ( 'NONE',  ( -0.1787899950787401882, -0.4335629920722205433, 0.000000000000000000 ) ) ;
#4601 = ORIENTED_EDGE ( 'NONE', *, *, #11577, .T. ) ;
#4602 = CARTESIAN_POINT ( 'NONE',  ( 0.9500414927467378812, 0.1787899950787401604, 1.368110236166710125 ) ) ;
#4603 = AXIS2_PLACEMENT_3D ( 'NONE', #24873, #32797, #3768 ) ;
#4604 = AXIS2_PLACEMENT_3D ( 'NONE', #16171, #30805, #39125 ) ;
#4605 = CARTESIAN_POINT ( 'NONE',  ( 0.7185039370078760701, -0.06523048226348075740, 0.7308070865066462751 ) ) ;
#4606 = CARTESIAN_POINT ( 'NONE',  ( -0.07405724077823318263, -0.2342519684501733479, 0.1787899950787401604 ) ) ;
#4607 = CARTESIAN_POINT ( 'NONE',  ( 0.7495606340400177148, -0.1264236179284866091, 1.542814960576157413 ) ) ;
#4608 = CARTESIAN_POINT ( 'NONE',  ( 0.9500414927467378812, -0.1787899950787401604, 0.1722440944344254266 ) ) ;
#4609 = CARTESIAN_POINT ( 'NONE',  ( 0.1264236179284866091, -1.713090551127338657, -0.1264236179284866091 ) ) ;
#4610 = CARTESIAN_POINT ( 'NONE',  ( 0.1787899950787401882, -1.713090551127338657, -2.189545951927503898E-17 ) ) ;
#4611 = APPLICATION_PROTOCOL_DEFINITION ( 'draft international standard', 'automotive_design', 1998, #10140 ) ;
#4612 = CARTESIAN_POINT ( 'NONE',  ( 0.1781957201322358353, -0.09842519685039370636, -0.01456528979491370120 ) ) ;
#4613 = CARTESIAN_POINT ( 'NONE',  ( -0.7495606340400177148, -0.1264236179284866091, 0.6028543306548976854 ) ) ;
#4615 = FACE_OUTER_BOUND ( 'NONE', #31841, .T. ) ;
#4614 = CARTESIAN_POINT ( 'NONE',  ( 0.1574803149606300301, -0.6747047244094498408, -0.06523048226347956391 ) ) ;
#4616 = CARTESIAN_POINT ( 'NONE',  ( -1.100456976456230270E-17, -1.428193415882257788, -0.1797182628040039365 ) ) ;
#4617 = DIRECTION ( 'NONE',  ( 0.000000000000000000, 0.000000000000000000, -1.000000000000000000 ) ) ;
#4618 = CARTESIAN_POINT ( 'NONE',  ( 0.2471922904502825702, 0.09210780053718577165, -0.04262551151394824989 ) ) ;
#4619 = CARTESIAN_POINT ( 'NONE',  ( 0.8759842519685039353, 0.1787899950787401882, 1.414862204670645829 ) ) ;
#4620 = CARTESIAN_POINT ( 'NONE',  ( 1.002407869896990045, -0.1264236179284866091, 1.828248031442299082 ) ) ;
#4621 = CARTESIAN_POINT ( 'NONE',  ( 0.7495606340400177148, 0.1264236179284866091, 0.2731299212060791515 ) ) ;
#4624 = EDGE_LOOP ( 'NONE', ( #6787, #17164, #42331, #39743 ) ) ;
#4623 = EDGE_CURVE ( 'NONE', #18116, #2953, #18310, .T. ) ;
#4622 = CARTESIAN_POINT ( 'NONE',  ( 0.1235961452251413406, 0.09842519685039370636, 0.2140748031496062798 ) ) ;
#4625 = CARTESIAN_POINT ( 'NONE',  ( 0.1184675242425078795, -0.09842519685039370636, 1.713085361781127913 ) ) ;
#4626 = DIRECTION ( 'NONE',  ( 2.263915770909195608E-15, -0.6156614753256604011, -0.7880107536067204599 ) ) ;
#4627 = CARTESIAN_POINT ( 'NONE',  ( -0.8107537697050254399, -0.1574803149606297803, 1.926673228346456490 ) ) ;
#4628 = CARTESIAN_POINT ( 'NONE',  ( -0.9873396505805591694, 0.1113553986120547346, 1.225393700679874076 ) ) ;
#4629 = ADVANCED_FACE ( 'NONE', ( #45517 ), #5760, .F. ) ;
#4630 = CARTESIAN_POINT ( 'NONE',  ( 0.7505145642813948470, -0.1098182161263852180, 0.03937465431229628110 ) ) ;
#4632 = CARTESIAN_POINT ( 'NONE',  ( -9.642888182262618425E-18, 0.01181102372957427288, -0.1574803149606299191 ) ) ;
#4631 = CARTESIAN_POINT ( 'NONE',  ( 0.8019270111902716547, 0.1787899950787401604, 1.254921259788757348 ) ) ;
#4633 = AXIS2_PLACEMENT_3D ( 'NONE', #24573, #6345, #46368 ) ;
#4634 = DIRECTION ( 'NONE',  ( -1.000000000000000000, 0.000000000000000000, 0.000000000000000000 ) ) ;
#4635 = CARTESIAN_POINT ( 'NONE',  ( -0.9873396505805591694, 0.1113553986120547346, 0.7627952755905511584 ) ) ;
#4636 = CARTESIAN_POINT ( 'NONE',  ( -0.9500414927467378812, 0.1787899950787401604, 1.289370078686393750 ) ) ;
#4637 = CARTESIAN_POINT ( 'NONE',  ( 0.8759842519685039353, 0.1574803149606299191, 0.6397637794200314865 ) ) ;
#4638 = VERTEX_POINT ( 'NONE', #27368 ) ;
#4639 = CARTESIAN_POINT ( 'NONE',  ( -0.7185039370078746268, 0.06523048226347956391, 1.759350393700788162 ) ) ;
#4640 = EDGE_CURVE ( 'NONE', #11651, #16491, #15246, .T. ) ;
#4641 = CARTESIAN_POINT ( 'NONE',  ( 0.8759842519685039353, 0.1574803149606299191, 0.6889763779527560139 ) ) ;
#4642 = ORIENTED_EDGE ( 'NONE', *, *, #11875, .T. ) ;
#4643 = CARTESIAN_POINT ( 'NONE',  ( -1.100456976456230270E-17, -0.08961073871690393433, -0.1797182628040039365 ) ) ;
#4644 = PRODUCT_DEFINITION_SHAPE ( 'NONE', 'NONE',  #47463 ) ;
#4646 = CARTESIAN_POINT ( 'NONE',  ( 0.07405724077823318263, -1.238188976324190005, -0.1787899950787401604 ) ) ;
#4645 = CARTESIAN_POINT ( 'NONE',  ( -0.06523048226347956391, -1.048720472333417142, -0.1574803149606300301 ) ) ;
#4647 = PRESENTATION_LAYER_ASSIGNMENT (  '', '', ( #19186 ) ) ;
#4648 = CARTESIAN_POINT ( 'NONE',  ( -1.033464566929134687, -0.06523048226347956391, 0.04675196850393695952 ) ) ;
#4649 = CARTESIAN_POINT ( 'NONE',  ( 0.7495606340400177148, -0.1264236179284866091, 1.582185039316315045 ) ) ;
#4650 = CARTESIAN_POINT ( 'NONE',  ( -0.9873396505805591694, 0.1113553986120547346, 1.235236220472440971 ) ) ;
#4651 = ADVANCED_FACE ( 'NONE', ( #9121 ), #1853, .T. ) ;
#4652 = DIRECTION ( 'NONE',  ( 1.000000000000000000, -0.000000000000000000, -0.000000000000000000 ) ) ;
#4653 = CARTESIAN_POINT ( 'NONE',  ( -1.033464566929134687, 0.06523048226347956391, 1.823326771653542178 ) ) ;
#4654 = LINE ( 'NONE', #33703, #22763 ) ;
#4655 = CIRCLE ( 'NONE', #23032, 0.009842519685039363003 ) ;
#4656 = ORIENTED_EDGE ( 'NONE', *, *, #24415, .T. ) ;
#4657 = CARTESIAN_POINT ( 'NONE',  ( 2.048885995248196921E-16, -0.5708661417322835607, 0.9783464566929134243 ) ) ;
#4658 = ORIENTED_EDGE ( 'NONE', *, *, #12078, .F. ) ;
#4659 = VECTOR ( 'NONE', #30111, 39.37007874015748143 ) ;
#4660 = CARTESIAN_POINT ( 'NONE',  ( -0.9500414927467377701, 0.1787899950787401604, 1.525590551127339989 ) ) ;
#4661 = CARTESIAN_POINT ( 'NONE',  ( 0.06523048226347956391, -0.1235236219397170543, 0.1574803149606297803 ) ) ;
#4662 = CARTESIAN_POINT ( 'NONE',  ( -1.054774247047244096, 0.000000000000000000, 1.208169291284818980 ) ) ;
#4663 = DIRECTION ( 'NONE',  ( -4.275490733183370330E-15, 0.000000000000000000, 1.000000000000000000 ) ) ;
#4664 = CARTESIAN_POINT ( 'NONE',  ( -0.7495606340400177148, -0.1264236179284866091, 0.3666338582139531677 ) ) ;
#4665 = CARTESIAN_POINT ( 'NONE',  ( 0.06801279071809869514, -0.09842519685039370636, 1.224299699984025658 ) ) ;
#4666 = CARTESIAN_POINT ( 'NONE',  ( -0.03598878106637547203, -0.09842522444525984848, 0.1542999736886214723 ) ) ;
#4667 = CARTESIAN_POINT ( 'NONE',  ( -0.07405724077823318263, -1.007997983977270140, -0.1787899950787401604 ) ) ;
#4668 = EDGE_LOOP ( 'NONE', ( #34347, #651, #38280, #27775 ) ) ;
#4669 = CARTESIAN_POINT ( 'NONE',  ( 0.1787899950787401882, 0.01919291343959027632, -2.189545951927503898E-17 ) ) ;
#4670 = VERTEX_POINT ( 'NONE', #5519 ) ;
#4671 = ORIENTED_EDGE ( 'NONE', *, *, #17308, .F. ) ;
#4672 = CARTESIAN_POINT ( 'NONE',  ( 0.01230737760510393873, -0.07955613945526318620, 0.1377952755905511861 ) ) ;
#4673 = CARTESIAN_POINT ( 'NONE',  ( 0.5660731898098425585, 4.766607801171850497E-17, 0.000000000000000000 ) ) ;
#4674 = LINE ( 'NONE', #20423, #1748 ) ;
#4675 = CIRCLE ( 'NONE', #8518, 0.2559055118110236116 ) ;
#4676 = CIRCLE ( 'NONE', #26052, 0.1377952755905511861 ) ;
#4677 = SHAPE_REPRESENTATION ( 'Catch Plate', ( #20860 ), #39224 ) ;
#4678 = CARTESIAN_POINT ( 'NONE',  ( -1.002407869896990045, -0.1264236179284866091, 0.1402559054580474474 ) ) ;
#4679 = CARTESIAN_POINT ( 'NONE',  ( -0.7185039370078746268, 0.06523048226347956391, 0.8144685039370082036 ) ) ;
#4680 = CARTESIAN_POINT ( 'NONE',  ( 0.1797182628040039087, -1.007425699346825576, 0.07444174185955046430 ) ) ;
#4681 = CARTESIAN_POINT ( 'NONE',  ( 0.9873396505805591694, 0.1113553986120547346, 0.4084645669291339098 ) ) ;
#4682 = CARTESIAN_POINT ( 'NONE',  ( -0.7646288533564489232, -0.1113553986120547346, 1.560039369971212508 ) ) ;
#4683 = CARTESIAN_POINT ( 'NONE',  ( 0.8759842519685039353, 0.1787899950787401882, 0.9817913385289134265 ) ) ;
#4684 = CARTESIAN_POINT ( 'NONE',  ( 0.8759842519685039353, 0.1787899950787401882, 1.409940944828126153 ) ) ;
#4685 = CARTESIAN_POINT ( 'NONE',  ( 1.002407869896990045, 0.1264236179284866091, 0.1058070865604098382 ) ) ;
#4686 = FACE_OUTER_BOUND ( 'NONE', #11455, .T. ) ;
#4687 = CARTESIAN_POINT ( 'NONE',  ( 0.8759842519685039353, -0.1574803149606299191, 1.377952755905512028 ) ) ;
#4689 = LINE ( 'NONE', #16220, #17803 ) ;
#4688 = CARTESIAN_POINT ( 'NONE',  ( 0.7434085338012068611, 0.09442915021634661066, 1.981317316331754563 ) ) ;
#4690 = DIRECTION ( 'NONE',  ( 0.000000000000000000, 0.000000000000000000, -1.000000000000000000 ) ) ;
#4691 = ADVANCED_FACE ( 'NONE', ( #21545, #20835, #17017 ), #27840, .T. ) ;
#4692 = CARTESIAN_POINT ( 'NONE',  ( 0.1574803149606299191, 0.000000000000000000, -0.2357204724409448504 ) ) ;
#4693 = CARTESIAN_POINT ( 'NONE',  ( 1.054774247047244096, 0.000000000000000000, 0.8882874015210394658 ) ) ;
#4694 = CARTESIAN_POINT ( 'NONE',  ( 0.8759842519685039353, -0.1787899950787401882, 1.749507873961984483 ) ) ;
#4695 = CARTESIAN_POINT ( 'NONE',  ( -0.07405724077823318263, -0.7952755904974174728, -0.1787899950787401604 ) ) ;
#4696 = ORIENTED_EDGE ( 'NONE', *, *, #24787, .F. ) ;
#4697 = CARTESIAN_POINT ( 'NONE',  ( 0.8759842519685039353, 0.1574803149606299191, 0.9251968503937008093 ) ) ;
#4698 = EDGE_CURVE ( 'NONE', #39085, #20854, #31420, .T. ) ;
#4699 = CARTESIAN_POINT ( 'NONE',  ( -0.1574803149606299191, -1.553149606191686960, 0.000000000000000000 ) ) ;
#4700 = CARTESIAN_POINT ( 'NONE',  ( -0.9412147342319837628, 0.1574803149606300301, 0.04675196839640998608 ) ) ;
#4701 = CARTESIAN_POINT ( 'NONE',  ( 0.8759842519685039353, 0.1787899950787401882, 1.094980314906866203 ) ) ;
#4702 = EDGE_CURVE ( 'NONE', #39448, #17524, #41605, .T. ) ;
#4703 = CARTESIAN_POINT ( 'NONE',  ( 0.7185039370078739607, 1.928577636452523993E-17, 1.486220472440944906 ) ) ;
#4704 = CARTESIAN_POINT ( 'NONE',  ( -9.642888182262618425E-18, -1.612204724409448842, -0.1574803149606299191 ) ) ;
#4705 = CARTESIAN_POINT ( 'NONE',  ( 0.1377952755905511861, 0.1564960629921262614, 0.8070866141732283561 ) ) ;
#4706 = VECTOR ( 'NONE', #35203, 39.37007874015748143 ) ;
#4707 = DIRECTION ( 'NONE',  ( -0.000000000000000000, 0.000000000000000000, 1.000000000000000000 ) ) ;
#4708 = CARTESIAN_POINT ( 'NONE',  ( -0.7495606340400177148, 0.1264236179284866091, 0.1943897637257641919 ) ) ;
#4709 = ORIENTED_EDGE ( 'NONE', *, *, #13004, .F. ) ;
#4710 = VERTEX_POINT ( 'NONE', #13206 ) ;
#4711 = DIRECTION ( 'NONE',  ( 0.000000000000000000, -1.000000000000000000, 0.000000000000000000 ) ) ;
#4712 = CARTESIAN_POINT ( 'NONE',  ( -0.1264236179284866091, -1.457185039316315045, 0.1264236179284866091 ) ) ;
#4713 = VECTOR ( 'NONE', #3390, 39.37007874015748143 ) ;
#4714 = AXIS2_PLACEMENT_3D ( 'NONE', #12097, #26721, #36779 ) ;
#4715 = CARTESIAN_POINT ( 'NONE',  ( -1.002407869896990045, 0.1264236179284866091, 1.838090551127338657 ) ) ;
#4716 = CARTESIAN_POINT ( 'NONE',  ( -0.8759842519685039353, 0.1787899950787401882, 0.9374999999462362288 ) ) ;
#4717 = CARTESIAN_POINT ( 'NONE',  ( -0.8759842519685039353, -0.1787899950787401882, 0.5684055117572598403 ) ) ;
#4718 = DIRECTION ( 'NONE',  ( -0.000000000000000000, 0.000000000000000000, 1.000000000000000000 ) ) ;
#4719 = DIRECTION ( 'NONE',  ( -0.5735764363510332808, 0.6455006197386625733, -0.5043203561029951931 ) ) ;
#4720 = DIRECTION ( 'NONE',  ( 0.000000000000000000, 0.000000000000000000, -1.000000000000000000 ) ) ;
#4721 = CARTESIAN_POINT ( 'NONE',  ( 0.1377952755905509363, 0.000000000000000000, -0.1045766232635885612 ) ) ;
#4722 = CARTESIAN_POINT ( 'NONE',  ( 3.284318927891251994E-17, -0.4789625509064039943, 0.1787899950787401882 ) ) ;
#4723 = CARTESIAN_POINT ( 'NONE',  ( -0.1723604372983632005, -0.08955946469359528372, -0.1761694098153657739 ) ) ;
#4724 = CARTESIAN_POINT ( 'NONE',  ( 0.06523048226347956391, 0.04872047254847189368, -0.1574803149606300301 ) ) ;
#4725 = CARTESIAN_POINT ( 'NONE',  ( 0.000000000000000000, 3.616083068348484413E-17, -0.2952755905511810774 ) ) ;
#4726 = DIRECTION ( 'NONE',  ( 0.000000000000000000, 0.000000000000000000, 1.000000000000000000 ) ) ;
#4727 = CARTESIAN_POINT ( 'NONE',  ( -1.054774247047244096, 0.000000000000000000, 0.4158464566391496531 ) ) ;
#4728 = ORIENTED_EDGE ( 'NONE', *, *, #31626, .T. ) ;
#4729 = CARTESIAN_POINT ( 'NONE',  ( 0.2471922927914619317, -0.07821957050365321851, 0.07683452368278725908 ) ) ;
#4730 = CARTESIAN_POINT ( 'NONE',  ( -0.6971942568897648851, -0.07405724077823297447, 1.545275590497419138 ) ) ;
#4731 = CIRCLE ( 'NONE', #26220, 0.09842519685039370636 ) ;
#4732 = CARTESIAN_POINT ( 'NONE',  ( -0.1264236179284866091, -1.388287401521039355, -0.1264236179284866091 ) ) ;
#4733 = CARTESIAN_POINT ( 'NONE',  ( 0.07405724077823318263, -1.508858267662772867, -0.1787899950787401604 ) ) ;
#4734 = DIRECTION ( 'NONE',  ( 0.000000000000000000, -1.000000000000000000, 0.000000000000000000 ) ) ;
#4735 = CARTESIAN_POINT ( 'NONE',  ( 0.1636882031642129531, -0.08048656780410663736, 0.1394067246032472951 ) ) ;
#4736 = CARTESIAN_POINT ( 'NONE',  ( 1.033464566929134687, -0.06523048226347956391, 0.4798228346456688831 ) ) ;
#4737 = DIRECTION ( 'NONE',  ( 0.000000000000000000, 0.000000000000000000, 1.000000000000000000 ) ) ;
#4738 = CARTESIAN_POINT ( 'NONE',  ( -0.7185039370078746268, -0.06523048226347956391, 1.124507873908221489 ) ) ;
#4739 = CARTESIAN_POINT ( 'NONE',  ( 0.9500414927467378812, 0.1787899950787401604, 0.5462598424659214080 ) ) ;
#4741 = LINE ( 'NONE', #33791, #6344 ) ;
#4740 = CARTESIAN_POINT ( 'NONE',  ( 0.1574803149606299191, -0.3228346456692913757, -1.928577636452523993E-17 ) ) ;
#4742 = CIRCLE ( 'NONE', #19299, 0.3814023619577306956 ) ;
#4743 = AXIS2_PLACEMENT_3D ( 'NONE', #16569, #12981, #27621 ) ;
#4744 = CARTESIAN_POINT ( 'NONE',  ( 1.033464566929134687, -0.06523048226347956391, 1.966043306979087246 ) ) ;
#4745 = ORIENTED_EDGE ( 'NONE', *, *, #22232, .F. ) ;
#4746 = CARTESIAN_POINT ( 'NONE',  ( -1.033464566929133799, 0.000000000000000000, 1.269685039370078705 ) ) ;
#4747 = CARTESIAN_POINT ( 'NONE',  ( -1.002407869896990045, -0.1264236179284866091, 1.085137795221826629 ) ) ;
#4748 = CARTESIAN_POINT ( 'NONE',  ( 0.7185039370078746268, -0.06523048226347956391, 0.8981299212598431447 ) ) ;
#4749 = CARTESIAN_POINT ( 'NONE',  ( 0.9873396505805591694, 0.1113553986120547346, 1.353346456692913424 ) ) ;
#4750 = EDGE_CURVE ( 'NONE', #18385, #41392, #9600, .T. ) ;
#4751 = DIRECTION ( 'NONE',  ( 0.000000000000000000, 0.000000000000000000, -1.000000000000000000 ) ) ;
#4752 = CARTESIAN_POINT ( 'NONE',  ( -0.8759842519685039353, -0.1574803149606299191, 1.259842519685039353 ) ) ;
#4753 = CARTESIAN_POINT ( 'NONE',  ( -0.1622643153356901069, -0.08956225154872389516, 0.03952951923502038417 ) ) ;
#4754 = ORIENTED_EDGE ( 'NONE', *, *, #23441, .T. ) ;
#4755 = AXIS2_PLACEMENT_3D ( 'NONE', #5649, #20260, #6102 ) ;
#4756 = CARTESIAN_POINT ( 'NONE',  ( 0.1644020957507537628, 0.08115590401245532937, -0.1405661490837558925 ) ) ;
#4757 = CARTESIAN_POINT ( 'NONE',  ( 1.054774247047244540, 0.07405724077823318263, 0.7332677164816707727 ) ) ;
#4758 = EDGE_CURVE ( 'NONE', #27223, #9016, #38819, .T. ) ;
#4759 = ORIENTED_EDGE ( 'NONE', *, *, #6572, .T. ) ;
#4760 = CARTESIAN_POINT ( 'NONE',  ( 1.033464566929133799, 0.000000000000000000, 0.8366141732283465249 ) ) ;
#4761 = CARTESIAN_POINT ( 'NONE',  ( -1.033464566929133799, 0.000000000000000000, 0.4330708660342047489 ) ) ;
#4762 = CARTESIAN_POINT ( 'NONE',  ( 0.1787899950787401604, -1.676181102308441639, 0.07405724077823318263 ) ) ;
#4763 = CARTESIAN_POINT ( 'NONE',  ( -0.07405724077823318263, -0.8789370078202529690, -0.1787899950787401604 ) ) ;
#4764 = CARTESIAN_POINT ( 'NONE',  ( 0.06523048226347956391, -1.275098425196850016, 0.1574803149606297803 ) ) ;
#4765 = CARTESIAN_POINT ( 'NONE',  ( 0.7646288533564489232, -0.1113553986120547346, 1.048228346349165507 ) ) ;
#4766 = CARTESIAN_POINT ( 'NONE',  ( -0.7185039370078739607, 1.928577636452523993E-17, 1.643700787401574992 ) ) ;
#4767 = ORIENTED_EDGE ( 'NONE', *, *, #18776, .T. ) ;
#4768 = ORIENTED_EDGE ( 'NONE', *, *, #26760, .F. ) ;
#4769 = CARTESIAN_POINT ( 'NONE',  ( -0.7495606340400177148, 0.1264236179284866091, 1.774114173174582643 ) ) ;
#4770 = CARTESIAN_POINT ( 'NONE',  ( 1.002407869896990045, -0.1264236179284866091, 1.636318897584031484 ) ) ;
#4771 = ORIENTED_EDGE ( 'NONE', *, *, #4540, .T. ) ;
#4772 = CYLINDRICAL_SURFACE ( 'NONE', #1112, 0.1574803149606299191 ) ;
#4773 = CARTESIAN_POINT ( 'NONE',  ( 0.7495606340400177148, -0.1264236179284866091, 0.3666338582139531677 ) ) ;
#4774 = CARTESIAN_POINT ( 'NONE',  ( -0.9500414927467378812, -0.1787899950787401604, 1.392716535379308285 ) ) ;
#4775 = LINE ( 'NONE', #19403, #21284 ) ;
#4776 = CARTESIAN_POINT ( 'NONE',  ( -0.7495606340400177148, -0.1264236179284866091, 1.227854330654897685 ) ) ;
#4777 = CARTESIAN_POINT ( 'NONE',  ( -0.9500414927467378812, 0.1787899950787401604, 0.07381889758403178958 ) ) ;
#4778 = AXIS2_PLACEMENT_3D ( 'NONE', #37976, #1528, #23830 ) ;
#4779 = CARTESIAN_POINT ( 'NONE',  ( -1.033464566929133799, 0.000000000000000000, 1.653543306979086580 ) ) ;
#4780 = CARTESIAN_POINT ( 'NONE',  ( -1.054774247047244540, -0.07405724077823318263, 1.678149606245448622 ) ) ;
#4781 = CARTESIAN_POINT ( 'NONE',  ( -1.054774247047244540, 0.07405724077823318263, 0.02952755900135457801 ) ) ;
#4782 = CARTESIAN_POINT ( 'NONE',  ( 0.8759842519685039353, 0.000000000000000000, 4.498031496062992574 ) ) ;
#4783 = CARTESIAN_POINT ( 'NONE',  ( -0.9412147342319837628, -0.1574803149606297803, 1.616633858267715551 ) ) ;
#4784 = DIRECTION ( 'NONE',  ( 0.000000000000000000, -1.000000000000000000, 0.000000000000000000 ) ) ;
#4785 = CARTESIAN_POINT ( 'NONE',  ( 1.002407869896990045, -0.1264236179284866091, 1.636318897584031484 ) ) ;
#4786 = CARTESIAN_POINT ( 'NONE',  ( 0.1048411618717816907, -0.09851382789342855162, 0.1042575923466826787 ) ) ;
#4787 = CARTESIAN_POINT ( 'NONE',  ( 0.8070866141732283561, -0.0009842519685049383633, -0.8559055118110230342 ) ) ;
#4788 = EDGE_LOOP ( 'NONE', ( #34300, #11258, #6246, #7072 ) ) ;
#4789 = CIRCLE ( 'NONE', #46111, 0.1574803149606301966 ) ;
#4790 = EDGE_CURVE ( 'NONE', #40254, #11736, #43157, .T. ) ;
#4791 = ORIENTED_EDGE ( 'NONE', *, *, #5136, .T. ) ;
#4792 = ORIENTED_EDGE ( 'NONE', *, *, #11592, .T. ) ;
#4793 = CARTESIAN_POINT ( 'NONE',  ( -1.094772975963752103E-17, -0.9601377952218268508, -0.1787899950787401882 ) ) ;
#4794 = CARTESIAN_POINT ( 'NONE',  ( -0.07405724077823318263, -1.095472440891117838, 0.1787899950787401604 ) ) ;
#4795 = CARTESIAN_POINT ( 'NONE',  ( -0.9873396505805591694, 0.1113553986120547346, 1.274606299212598604 ) ) ;
#4796 = CARTESIAN_POINT ( 'NONE',  ( 0.1270800023317771588, -0.3307524710003684754, -0.1270800023317771588 ) ) ;
#4797 = DIRECTION ( 'NONE',  ( -1.000000000000000000, 0.000000000000000000, 0.000000000000000000 ) ) ;
#4798 = CARTESIAN_POINT ( 'NONE',  ( 0.2133350748051826562, 0.1723249637083595076, -0.3049284531894324579 ) ) ;
#4799 = CARTESIAN_POINT ( 'NONE',  ( -0.7646288533564489232, 0.1113553986120547346, 0.1427165354330708902 ) ) ;
#4801 = EDGE_CURVE ( 'NONE', #39413, #16648, #39040, .T. ) ;
#4800 = CARTESIAN_POINT ( 'NONE',  ( 0.6971942568897637749, 2.189545951927499583E-17, 0.7504921259304880854 ) ) ;
#4802 = VECTOR ( 'NONE', #26824, 39.37007874015748143 ) ;
#4803 = EDGE_CURVE ( 'NONE', #16187, #36149, #6676, .T. ) ;
#4805 = DIRECTION ( 'NONE',  ( -0.4999999999999998890, 0.000000000000000000, -0.8660254037844388186 ) ) ;
#4804 = CARTESIAN_POINT ( 'NONE',  ( 0.02440571223928530292, 0.2814035877312904832, -0.08364281214760876937 ) ) ;
#4806 = CARTESIAN_POINT ( 'NONE',  ( -0.7185039370078739607, 1.928577636452523993E-17, 1.318897637687747926 ) ) ;
#4807 = CARTESIAN_POINT ( 'NONE',  ( 0.9500414927467378812, -0.1787899950787401604, 1.870078740103715331 ) ) ;
#4808 = CARTESIAN_POINT ( 'NONE',  ( 0.9500414927467377701, 0.1787899950787401604, 1.412401574749386990 ) ) ;
#4809 = AXIS2_PLACEMENT_3D ( 'NONE', #31422, #23988, #16554 ) ;
#4810 = ORIENTED_EDGE ( 'NONE', *, *, #9556, .F. ) ;
#4811 = EDGE_CURVE ( 'NONE', #11722, #39584, #46217, .T. ) ;
#4812 = CARTESIAN_POINT ( 'NONE',  ( 0.9412147342319837628, -0.1574803149606297803, 0.08120078740157485320 ) ) ;
#4813 = CARTESIAN_POINT ( 'NONE',  ( 0.2431102362204724532, 2.977241726273585582E-17, 0.000000000000000000 ) ) ;
#4814 = CARTESIAN_POINT ( 'NONE',  ( -0.07405724077823318263, -0.3671259841982050798, -0.1787899950787401604 ) ) ;
#4815 = DIRECTION ( 'NONE',  ( 1.000000000000000000, -0.000000000000000000, 0.000000000000000000 ) ) ;
#4816 = CARTESIAN_POINT ( 'NONE',  ( -1.094772975963752103E-17, -1.230807086560409269, -0.1787899950787401882 ) ) ;
#4817 = CARTESIAN_POINT ( 'NONE',  ( 1.002407869896990045, 0.1264236179284866091, 0.2288385826234019815 ) ) ;
#4818 = CARTESIAN_POINT ( 'NONE',  ( -0.8019270111902717657, -0.1787899950787401604, 1.702755905458047003 ) ) ;
#4819 = ORIENTED_EDGE ( 'NONE', *, *, #46847, .T. ) ;
#4820 = CARTESIAN_POINT ( 'NONE',  ( -1.054774247047244540, 0.07405724077823318263, 1.328740157426552049 ) ) ;
#4821 = CARTESIAN_POINT ( 'NONE',  ( 0.6971942568897648851, 0.07405724077823318263, 1.264763779473795813 ) ) ;
#4822 = CARTESIAN_POINT ( 'NONE',  ( 0.6971942568897626646, 0.07405724077823318263, 0.04429133852891373180 ) ) ;
#4823 = CARTESIAN_POINT ( 'NONE',  ( -0.8019270111902717657, 0.1787899950787401604, 1.176181102308441417 ) ) ;
#4824 = CARTESIAN_POINT ( 'NONE',  ( 0.8759842519685039353, 0.000000000000000000, 4.498031496062992574 ) ) ;
#4825 = CARTESIAN_POINT ( 'NONE',  ( -0.08205013688028725549, -0.09842440306376359915, -0.1588770961503328805 ) ) ;
#4826 = CARTESIAN_POINT ( 'NONE',  ( 0.7185039370078739607, 1.928577636452523993E-17, 0.05905511800270921846 ) ) ;
#4827 = CARTESIAN_POINT ( 'NONE',  ( 1.054774247047244540, 0.07405724077823318263, 0.4232283464029293896 ) ) ;
#4828 = CARTESIAN_POINT ( 'NONE',  ( -0.7495606340400177148, -0.1264236179284866091, 0.3223425196312759144 ) ) ;
#4829 = ORIENTED_EDGE ( 'NONE', *, *, #22956, .T. ) ;
#4830 = ( BOUNDED_CURVE ( )  B_SPLINE_CURVE ( 2, ( #792, #37479, #4628, #19263, #33917, #1040, #15698, #30335, #16848 ),
 .UNSPECIFIED., .F., .T. ) 
 B_SPLINE_CURVE_WITH_KNOTS ( ( 3, 2, 2, 2, 3 ),
 ( 0.5999999999999999778, 0.6025000000000000355, 0.6049999999999999822, 0.6075000000000000400, 0.6099999999999999867 ),
 .UNSPECIFIED. ) 
 CURVE ( )  GEOMETRIC_REPRESENTATION_ITEM ( )  RATIONAL_B_SPLINE_CURVE ( ( 1.000000000000000000, 0.9238795325112869605, 1.000000000000000000, 0.9238795325112869605, 1.000000000000000000, 0.9238795325112869605, 1.000000000000000000, 0.9238795325112829637, 1.000000000000000000 ) ) 
 REPRESENTATION_ITEM ( '' )  ) ;
#4831 = FACE_OUTER_BOUND ( 'NONE', #23943, .T. ) ;
#4832 = ORIENTED_EDGE ( 'NONE', *, *, #8571, .T. ) ;
#4833 = VERTEX_POINT ( 'NONE', #20600 ) ;
#4834 = CARTESIAN_POINT ( 'NONE',  ( -0.8107537697050253289, -0.1574803149606297803, 0.3518700787401576324 ) ) ;
#4835 = CARTESIAN_POINT ( 'NONE',  ( 1.054774247047244540, 0.07405724077823318263, 1.171259842465921741 ) ) ;
#4836 = CARTESIAN_POINT ( 'NONE',  ( -1.054774247047244540, 0.07405724077823318263, 1.953740157426552715 ) ) ;
#4837 = FACE_OUTER_BOUND ( 'NONE', #10620, .T. ) ;
#4838 = EDGE_LOOP ( 'NONE', ( #34045, #33951, #29727, #22816 ) ) ;
#4839 = FACE_OUTER_BOUND ( 'NONE', #33641, .T. ) ;
#4840 = DIRECTION ( 'NONE',  ( 1.000000000000000000, 2.891205793294678326E-16, 0.000000000000000000 ) ) ;
#4841 = CARTESIAN_POINT ( 'NONE',  ( -1.094772975963752103E-17, -1.443529480040261825, -0.1787899950787401882 ) ) ;
#4842 = VERTEX_POINT ( 'NONE', #13649 ) ;
#4843 = CARTESIAN_POINT ( 'NONE',  ( -0.8107537697050254399, 0.1574803149606300301, 1.390255905404285119 ) ) ;
#4844 = CARTESIAN_POINT ( 'NONE',  ( 0.1264236179284866091, -0.4876968503399370380, -0.1264236179284866091 ) ) ;
#4845 = CARTESIAN_POINT ( 'NONE',  ( -0.2610212580023194007, -0.1673090378115814347, 0.8646000909489542918 ) ) ;
#4846 = ORIENTED_EDGE ( 'NONE', *, *, #40501, .F. ) ;
#4847 = AXIS2_PLACEMENT_3D ( 'NONE', #10792, #3805, #15312 ) ;
#4848 = CARTESIAN_POINT ( 'NONE',  ( -0.1008439437003635641, 0.2372714618127385600, -0.3138705397960871446 ) ) ;
#4849 = CARTESIAN_POINT ( 'NONE',  ( 0.9873396505805591694, -0.1113553986120547346, 0.7431102361129447997 ) ) ;
#4850 = ( BOUNDED_CURVE ( )  B_SPLINE_CURVE ( 2, ( #33240, #41470, #5314, #29437, #45325, #8437, #30985, #18353, #11185 ),
 .UNSPECIFIED., .F., .T. ) 
 B_SPLINE_CURVE_WITH_KNOTS ( ( 3, 2, 2, 2, 3 ),
 ( 0.6400000000000000133, 0.6424999999999999600, 0.6450000000000000178, 0.6474999999999999645, 0.6500000000000000222 ),
 .UNSPECIFIED. ) 
 CURVE ( )  GEOMETRIC_REPRESENTATION_ITEM ( )  RATIONAL_B_SPLINE_CURVE ( ( 1.000000000000000000, 0.9238795325112869605, 1.000000000000000000, 0.9238795325112869605, 1.000000000000000000, 0.9238795325112869605, 1.000000000000000000, 0.9238795325112829637, 1.000000000000000000 ) ) 
 REPRESENTATION_ITEM ( '' )  ) ;
#4851 = CARTESIAN_POINT ( 'NONE',  ( -0.8107537697050254399, 0.1574803149606300301, 1.439468503937006760 ) ) ;
#4852 = CARTESIAN_POINT ( 'NONE',  ( 0.6971942568897648851, -0.07405724077823297447, 1.579724409395055318 ) ) ;
#4853 = CARTESIAN_POINT ( 'NONE',  ( 0.6971942568897626646, 0.07405724077823318263, 0.1574803149068664809 ) ) ;
#4854 = ( BOUNDED_CURVE ( )  B_SPLINE_CURVE ( 2, ( #3951, #583, #18575, #26267, #11879, #40130, #15240, #44661, #29429 ),
 .UNSPECIFIED., .F., .T. ) 
 B_SPLINE_CURVE_WITH_KNOTS ( ( 3, 2, 2, 2, 3 ),
 ( 0.03500000000000000333, 0.03749999999999999861, 0.04000000000000000083, 0.04250000000000000305, 0.04499999999999999833 ),
 .UNSPECIFIED. ) 
 CURVE ( )  GEOMETRIC_REPRESENTATION_ITEM ( )  RATIONAL_B_SPLINE_CURVE ( ( 1.000000000000000000, 0.9238795325112869605, 1.000000000000000000, 0.9238795325112869605, 1.000000000000000000, 0.9238795325112869605, 1.000000000000000000, 0.9238795325112869605, 1.000000000000000000 ) ) 
 REPRESENTATION_ITEM ( '' )  ) ;
#4855 = EDGE_CURVE ( 'NONE', #2020, #6624, #40085, .T. ) ;
#4856 = CARTESIAN_POINT ( 'NONE',  ( 0.1787899950787401604, -1.720472440891118726, 0.07405724077823318263 ) ) ;
#4857 = CARTESIAN_POINT ( 'NONE',  ( 0.1784937925128310954, -0.09842519685039369248, -0.001216461463074396381 ) ) ;
#4858 = CARTESIAN_POINT ( 'NONE',  ( -1.054774247047244096, 0.000000000000000000, 0.6569881889226141247 ) ) ;
#4859 = EDGE_CURVE ( 'NONE', #36696, #20228, #11886, .T. ) ;
#4861 = CARTESIAN_POINT ( 'NONE',  ( 1.033464566929133799, 0.000000000000000000, 0.3149606298137326843 ) ) ;
#4860 = CARTESIAN_POINT ( 'NONE',  ( -0.1574803149606297803, -0.7337598425196847352, 0.06523048226347956391 ) ) ;
#4862 = CARTESIAN_POINT ( 'NONE',  ( -0.1270800023317771588, -1.423272156039738112, -0.1270800023317771588 ) ) ;
#4863 = CARTESIAN_POINT ( 'NONE',  ( -0.1574803149606297803, -0.05462598414444141959, 0.06523048226347956391 ) ) ;
#4864 = CARTESIAN_POINT ( 'NONE',  ( 0.2471922904502826257, 0.09255273792768259344, -0.04108768875596677250 ) ) ;
#4865 = CARTESIAN_POINT ( 'NONE',  ( 0.9500414927467378812, -0.1787899950787401604, 1.397637795221827295 ) ) ;
#4866 = CARTESIAN_POINT ( 'NONE',  ( 1.054774247047244096, 0.000000000000000000, 1.793799212544661348 ) ) ;
#4867 = ( REPRESENTATION_RELATIONSHIP ('NONE','NONE', #9609, #19102 ) REPRESENTATION_RELATIONSHIP_WITH_TRANSFORMATION ( #3634 )SHAPE_REPRESENTATION_RELATIONSHIP( ) ) ;
#4869 = VERTEX_POINT ( 'NONE', #36182 ) ;
#4868 = CARTESIAN_POINT ( 'NONE',  ( 0.1574803149606299191, 0.000000000000000000, -0.04012007874015743186 ) ) ;
#4870 = B_SPLINE_CURVE_WITH_KNOTS ( 'NONE', 3,
 ( #24078, #6303, #31507, #46089, #32460, #40532, #17813, #7721, #36733, #26199, #29119, #10881, #25501, #43431, #7269, #3663, #40303, #4119, #40765, #14459, #22105, #29600, #21887, #18286, #3891, #36508, #33170, #39831, #18518, #292, #32691, #14938, #25732, #44142, #33401, #32928, #43910, #21648, #11340, #11112, #25953 ),
 .UNSPECIFIED., .F., .F.,
 ( 4, 1, 1, 1, 1, 1, 1, 2, 2, 1, 1, 1, 1, 2, 2, 2, 1, 1, 1, 1, 2, 2, 1, 1, 1, 1, 1, 2, 2, 4 ),
 ( 0.000000000000000000, 0.1250000000000038858, 0.1875000000000058287, 0.2187500000000068001, 0.2343750000000072164, 0.2421875000000074107, 0.2460937500000075495, 0.2480468750000075773, 0.2500000000000076050, 0.3125000000000083822, 0.3437500000000087153, 0.3593750000000088263, 0.3671875000000089373, 0.3710937500000089373, 0.3750000000000089373, 0.5000000000000056621, 0.5625000000000042188, 0.5937500000000035527, 0.6093750000000032196, 0.6171875000000029976, 0.6210937500000028866, 0.6250000000000027756, 0.6875000000000032196, 0.7187500000000033307, 0.7343750000000035527, 0.7421875000000035527, 0.7460937500000036637, 0.7480468750000035527, 0.7500000000000035527, 1.000000000000000000 ),
 .UNSPECIFIED. ) ;
#4871 = CARTESIAN_POINT ( 'NONE',  ( 0.000000000000000000, 0.000000000000000000, 0.000000000000000000 ) ) ;
#4872 = CARTESIAN_POINT ( 'NONE',  ( 0.3551574803149606385, 0.2362204724409449064, 2.892866454678787531E-17 ) ) ;
#4873 = CARTESIAN_POINT ( 'NONE',  ( -0.07405724077823318263, 0.04133858273092887170, 0.1787899950787401604 ) ) ;
#4874 = CARTESIAN_POINT ( 'NONE',  ( 0.9500414927467378812, -0.1787899950787401604, 0.3690944881352128393 ) ) ;
#4875 = CARTESIAN_POINT ( 'NONE',  ( -0.9873396505805591694, -0.1113553986120547346, 0.7529527559055118058 ) ) ;
#4876 = EDGE_CURVE ( 'NONE', #5551, #2820, #1062, .T. ) ;
#4877 = CARTESIAN_POINT ( 'NONE',  ( -0.7185039370078766252, -0.06523048226348168721, 1.321358267609009207 ) ) ;
#4878 = LINE ( 'NONE', #19504, #35583 ) ;
#4879 = DIRECTION ( 'NONE',  ( 1.000000000000000000, 0.000000000000000000, -0.000000000000000000 ) ) ;
#4880 = MANIFOLD_SOLID_BREP ( 'Handle Arm Right', #31751 ) ;
#4881 = CARTESIAN_POINT ( 'NONE',  ( -0.8019270111902717657, 0.1787899950787401604, 1.333661417269071059 ) ) ;
#4882 = CARTESIAN_POINT ( 'NONE',  ( 0.9873396505805591694, 0.1113553986120547346, 0.8710629920184568276 ) ) ;
#4883 = ORIENTED_EDGE ( 'NONE', *, *, #12877, .T. ) ;
#4884 = CARTESIAN_POINT ( 'NONE',  ( -0.8107537697050254399, 0.1574803149606300301, 1.754429133858266932 ) ) ;
#4885 = CARTESIAN_POINT ( 'NONE',  ( -0.2066929133858267653, -0.3147020779469855145, -1.066138954738185651 ) ) ;
#4886 = VERTEX_POINT ( 'NONE', #4251 ) ;
#4887 = CARTESIAN_POINT ( 'NONE',  ( 0.1270800023317771588, -0.06500443950430531692, 0.1270800023317771588 ) ) ;
#4888 = VECTOR ( 'NONE', #35420, 39.37007874015748143 ) ;
#4889 = CARTESIAN_POINT ( 'NONE',  ( -0.1264236179284866091, -1.260334645615527549, 0.1264236179284866091 ) ) ;
#4890 = CARTESIAN_POINT ( 'NONE',  ( -0.9412147342319837628, -0.1574803149606297803, 1.222933070866141669 ) ) ;
#4891 = CARTESIAN_POINT ( 'NONE',  ( 1.002407869896990045, 0.1264236179284866091, 1.562499999946236118 ) ) ;
#4892 = CARTESIAN_POINT ( 'NONE',  ( -0.9873396505805591694, 0.1113553986120547346, 1.274606299212598604 ) ) ;
#4893 = CARTESIAN_POINT ( 'NONE',  ( -1.033464566929134687, 0.06523048226347956391, 1.144192913278300194 ) ) ;
#4895 = CARTESIAN_POINT ( 'NONE',  ( -0.7646288533564489232, -0.1113553986120547346, 0.4281496062992125595 ) ) ;
#4894 = CARTESIAN_POINT ( 'NONE',  ( 0.1619907858920848209, -0.08803158632533415739, 0.1285577739723440804 ) ) ;
#4896 = DIRECTION ( 'NONE',  ( -1.000000000000000000, -0.000000000000000000, 0.000000000000000000 ) ) ;
#4897 = UNCERTAINTY_MEASURE_WITH_UNIT (LENGTH_MEASURE( 1.000000000000000082E-05 ), #37648, 'distance_accuracy_value', 'NONE') ;
#4898 = ORIENTED_EDGE ( 'NONE', *, *, #3304, .T. ) ;
#4899 = ORIENTED_EDGE ( 'NONE', *, *, #26845, .F. ) ;
#4900 = CARTESIAN_POINT ( 'NONE',  ( 0.9412147342319837628, -0.1574803149606297803, 0.5930118110236221041 ) ) ;
#4901 = AXIS2_PLACEMENT_3D ( 'NONE', #46697, #39274, #32111 ) ;
#4902 = CARTESIAN_POINT ( 'NONE',  ( -0.6971942568897648851, -0.07405724077823297447, 1.579724409395055318 ) ) ;
#4903 = CARTESIAN_POINT ( 'NONE',  ( -0.1113553986120547346, -0.02263779516806350284, -0.1113553986120547346 ) ) ;
#4904 = CARTESIAN_POINT ( 'NONE',  ( -0.8759842519685039353, 0.1787899950787401882, 1.218011810969858111 ) ) ;
#4905 = ORIENTED_EDGE ( 'NONE', *, *, #35980, .T. ) ;
#4906 = CARTESIAN_POINT ( 'NONE',  ( 0.2397010884053811242, 1.205361022782824954E-17, -0.09842519685039370636 ) ) ;
#4907 = CARTESIAN_POINT ( 'NONE',  ( -0.8759842519685039353, -0.1787899950787401882, 0.3321850393163153226 ) ) ;
#4908 = FACE_OUTER_BOUND ( 'NONE', #46312, .T. ) ;
#4909 = CARTESIAN_POINT ( 'NONE',  ( -0.7185039370078739607, 1.928577636452523993E-17, 0.6200787401574803237 ) ) ;
#4910 = CARTESIAN_POINT ( 'NONE',  ( 3.284318927891251994E-17, -0.9120334170481357861, 0.1787899950787401882 ) ) ;
#4911 = VERTEX_POINT ( 'NONE', #39734 ) ;
#4912 = CARTESIAN_POINT ( 'NONE',  ( -0.07405724077823318263, -0.007874015694267993623, -0.1787899950787401604 ) ) ;
#4913 = EDGE_LOOP ( 'NONE', ( #6162, #39201, #38762, #43388 ) ) ;
#4914 = ADVANCED_FACE ( 'NONE', ( #17943 ), #9534, .T. ) ;
#4915 = FACE_OUTER_BOUND ( 'NONE', #37759, .T. ) ;
#4916 = CARTESIAN_POINT ( 'NONE',  ( 0.000000000000000000, -0.5708661417322835607, -6.991093932140394160E-17 ) ) ;
#4917 = ADVANCED_FACE ( 'NONE', ( #33068 ), #29504, .T. ) ;
#4918 = CARTESIAN_POINT ( 'NONE',  ( -0.8759842519685039353, 0.000000000000000000, 0.000000000000000000 ) ) ;
#4919 = VECTOR ( 'NONE', #1557, 39.37007874015748143 ) ;
#4920 = CIRCLE ( 'NONE', #41633, 0.3937007874015748254 ) ;
#4921 = CARTESIAN_POINT ( 'NONE',  ( 0.1264236179284866091, -0.6993110235682834519, 0.1264236179284866091 ) ) ;
#4922 = CARTESIAN_POINT ( 'NONE',  ( -0.8759842519685039353, 0.1787899950787401882, 0.2337598424659216578 ) ) ;
#4923 = CARTESIAN_POINT ( 'NONE',  ( -0.7185039370078746268, -0.06523048226347956391, 0.8587598425196850682 ) ) ;
#4924 = PLANE ( 'NONE',  #29481 ) ;
#4925 = CARTESIAN_POINT ( 'NONE',  ( 0.1270800023317771588, -0.9705162505279271157, 0.1270800023317771588 ) ) ;
#4926 = DIRECTION ( 'NONE',  ( 0.000000000000000000, -1.000000000000000000, 0.000000000000000000 ) ) ;
#4927 = CARTESIAN_POINT ( 'NONE',  ( 0.7495606340400177148, -0.1264236179284866091, 0.9571850393163149340 ) ) ;
#4928 = DIRECTION ( 'NONE',  ( -1.000000000000000000, 0.000000000000000000, 0.000000000000000000 ) ) ;
#4929 = CARTESIAN_POINT ( 'NONE',  ( 0.8759842519685039353, 0.1574803149606299191, 1.515748031496062964 ) ) ;
#4931 = CARTESIAN_POINT ( 'NONE',  ( -0.2362204724409471546, 2.422684756221294029E-15, -1.186023622047243986 ) ) ;
#4930 = CARTESIAN_POINT ( 'NONE',  ( 0.7329509277787201738, 0.07874508389649351181, 1.981681257654730466 ) ) ;
#4932 = CARTESIAN_POINT ( 'NONE',  ( 0.000000000000000000, 1.478656101119254046E-17, 0.1377952755905511861 ) ) ;
#4933 = CARTESIAN_POINT ( 'NONE',  ( 0.1113553986120547346, -0.6722440943806614611, 0.1113553986120547346 ) ) ;
#4934 = CARTESIAN_POINT ( 'NONE',  ( 0.1787899950787401604, 0.06102362210100767403, -0.07405724077823318263 ) ) ;
#4935 = CARTESIAN_POINT ( 'NONE',  ( 0.8759842519685039353, 0.1787899950787401882, 0.9768700786863937502 ) ) ;
#4936 = CARTESIAN_POINT ( 'NONE',  ( 0.8019270111902716547, 0.1787899950787401604, 1.811023621993480548 ) ) ;
#4937 = CARTESIAN_POINT ( 'NONE',  ( 0.1264236179284866091, -0.9699803149068660924, 0.1264236179284866091 ) ) ;
#4938 = CYLINDRICAL_SURFACE ( 'NONE', #26938, 0.009842519685039382085 ) ;
#4939 = VERTEX_POINT ( 'NONE', #33306 ) ;
#4940 = CARTESIAN_POINT ( 'NONE',  ( -0.8759842519685039353, 0.1574803149606299191, 0.8464566929133857665 ) ) ;
#4941 = CARTESIAN_POINT ( 'NONE',  ( 0.1781957201322358353, -0.09842519685039370636, -0.01456528979491370120 ) ) ;
#4942 = CARTESIAN_POINT ( 'NONE',  ( 0.1574803149606300301, -1.614665354223181470, 0.06523048226347956391 ) ) ;
#4943 = CARTESIAN_POINT ( 'NONE',  ( -0.9412147342319837628, -0.1574803149606297803, 0.1107283463491660208 ) ) ;
#4944 = FACE_OUTER_BOUND ( 'NONE', #38741, .T. ) ;
#4945 = CARTESIAN_POINT ( 'NONE',  ( 0.6971942568897648851, -0.07405724077823297447, 1.067913385773007651 ) ) ;
#4946 = CARTESIAN_POINT ( 'NONE',  ( 1.033464566929133799, 1.928577636452524610E-17, 4.498031496062992574 ) ) ;
#4947 = DIRECTION ( 'NONE',  ( 0.000000000000000000, -0.9699617890481186944, -0.2432573283306648515 ) ) ;
#4949 = FACE_OUTER_BOUND ( 'NONE', #20467, .T. ) ;
#4948 = AXIS2_PLACEMENT_3D ( 'NONE', #23717, #5496, #30694 ) ;
#4950 = CARTESIAN_POINT ( 'NONE',  ( -1.054774247047244096, 0.000000000000000000, 0.2583661416785200671 ) ) ;
#4951 = CARTESIAN_POINT ( 'NONE',  ( -1.094772975963752103E-17, -1.550688976324188895, -0.1787899950787401882 ) ) ;
#4952 = AXIS2_PLACEMENT_3D ( 'NONE', #19826, #34454, #34939 ) ;
#4953 = ( GEOMETRIC_REPRESENTATION_CONTEXT ( 3 ) GLOBAL_UNCERTAINTY_ASSIGNED_CONTEXT ( ( #6183 ) ) GLOBAL_UNIT_ASSIGNED_CONTEXT ( ( #1373, #5455, #44977 ) ) REPRESENTATION_CONTEXT ( 'NONE', 'WORKASPACE' ) ) ;
#4954 = CARTESIAN_POINT ( 'NONE',  ( -1.054774247047244540, 0.07405724077823318263, 1.835629921206078485 ) ) ;
#4955 = CARTESIAN_POINT ( 'NONE',  ( -1.054774247047244540, 0.07405724077823318263, 0.9694881889226145688 ) ) ;
#4956 = B_SPLINE_CURVE_WITH_KNOTS ( 'NONE', 3,
 ( #30676, #22501, #19135, #37842, #16048, #1159, #26834, #5000, #45237, #19380, #44526, #12461, #8836, #11742, #1389, #15579, #22982, #41154, #8591, #15101, #4267, #19618, #12210, #30441, #11979, #41391, #37347, #37592, #29980, #37118, #33800, #919, #30217, #26362, #34258, #4500, #41629, #4753, #8117, #23471, #15814, #29746, #40922, #4048, #22742, #33326, #44996, #44291, #8357, #11495, #26115, #18900, #44762, #33554, #672, #15327, #26600, #38073, #38782, #38548, #23941, #31381, #16514, #42806, #28020, #5712, #17207, #9792, #23696, #5228, #5937, #20329, #20559, #5477, #35201, #31846 ),
 .UNSPECIFIED., .F., .F.,
 ( 4, 2, 2, 1, 1, 1, 1, 1, 2, 2, 2, 2, 2, 2, 2, 2, 2, 2, 1, 1, 2, 2, 2, 2, 1, 1, 2, 2, 2, 2, 1, 1, 1, 1, 2, 2, 2, 2, 2, 1, 1, 1, 2, 2, 2, 4 ),
 ( 0.000000000000000000, 0.06249999999999453215, 0.09374999999999182598, 0.1093749999999904104, 0.1171874999999898137, 0.1210937499999895361, 0.1230468749999893002, 0.1240234374999892725, 0.1245117187499892586, 0.1249999999999892308, 0.1874999999999879263, 0.2187499999999873157, 0.2343749999999871214, 0.2421874999999870104, 0.2499999999999868994, 0.3124999999999853451, 0.3437499999999846789, 0.3593749999999843459, 0.3671874999999841238, 0.3710937499999840128, 0.3730468749999839573, 0.3749999999999839018, 0.4374999999999833467, 0.4687499999999831246, 0.4843749999999830136, 0.4921874999999829026, 0.4960937499999828471, 0.4999999999999827915, 0.5624999999999827915, 0.5937499999999826805, 0.6093749999999826805, 0.6171874999999826805, 0.6210937499999826805, 0.6230468749999826805, 0.6240234374999826805, 0.6249999999999826805, 0.6874999999999852340, 0.7187499999999866773, 0.7343749999999872324, 0.7421874999999875655, 0.7460937499999876765, 0.7480468749999877875, 0.7490234374999877875, 0.7499999999999877875, 0.8749999999999938938, 1.000000000000000000 ),
 .UNSPECIFIED. ) ;
#4957 = CARTESIAN_POINT ( 'NONE',  ( -1.002407869896990045, 0.1264236179284866091, 0.5044291338045039375 ) ) ;
#4958 = CARTESIAN_POINT ( 'NONE',  ( 0.2759478392031653460, 0.3740157480314960647, 2.185526306663015728 ) ) ;
#4959 = DIRECTION ( 'NONE',  ( -0.000000000000000000, 1.000000000000000000, -3.995705278811693553E-31 ) ) ;
#4960 = LINE ( 'NONE', #18864, #19567 ) ;
#4961 = CARTESIAN_POINT ( 'NONE',  ( -0.3100393700787401619, 0.000000000000000000, 1.181102362204724310 ) ) ;
#4962 = CARTESIAN_POINT ( 'NONE',  ( 0.1787899950787401604, -0.6241397162607352778, -0.07405724077823318263 ) ) ;
#4963 = CARTESIAN_POINT ( 'NONE',  ( -0.2199481559187673185, -0.08955985715031791750, 0.08004915535381516845 ) ) ;
#4964 = CARTESIAN_POINT ( 'NONE',  ( 0.1574803149606299191, 0.04133858278469235842, -1.928577636452523993E-17 ) ) ;
#4965 = CARTESIAN_POINT ( 'NONE',  ( 0.9412147342319837628, -0.1574803149606297803, 0.4749015748031497064 ) ) ;
#4966 = DIRECTION ( 'NONE',  ( 0.000000000000000000, 0.000000000000000000, -1.000000000000000000 ) ) ;
#4967 = EDGE_CURVE ( 'NONE', #46334, #2521, #21777, .T. ) ;
#4968 = CARTESIAN_POINT ( 'NONE',  ( -0.2362204724409471546, 8.195543980992867555E-16, -0.9891732283464564901 ) ) ;
#4969 = CARTESIAN_POINT ( 'NONE',  ( -0.6971942568897637749, 2.189545951927499583E-17, 0.3961614172690708924 ) ) ;
#4970 = ( BOUNDED_CURVE ( )  B_SPLINE_CURVE ( 2, ( #24433, #6441, #24905, #27833, #2372, #42393, #17007, #38812, #46688 ),
 .UNSPECIFIED., .F., .T. ) 
 B_SPLINE_CURVE_WITH_KNOTS ( ( 3, 2, 2, 2, 3 ),
 ( 0.000000000000000000, 0.002500000000000000052, 0.005000000000000000104, 0.007499999999999998855, 0.01000000000000000021 ),
 .UNSPECIFIED. ) 
 CURVE ( )  GEOMETRIC_REPRESENTATION_ITEM ( )  RATIONAL_B_SPLINE_CURVE ( ( 1.000000000000000000, 0.9238795325112869605, 1.000000000000000000, 0.9238795325112869605, 1.000000000000000000, 0.9238795325112869605, 1.000000000000000000, 0.9238795325112869605, 1.000000000000000000 ) ) 
 REPRESENTATION_ITEM ( '' )  ) ;
#4971 = CARTESIAN_POINT ( 'NONE',  ( -0.1787899950787401604, -1.785557039095380105, 0.07405724077823318263 ) ) ;
#4972 = ADVANCED_FACE ( 'NONE', ( #36875, #11476 ), #40211, .T. ) ;
#4973 = ORIENTED_EDGE ( 'NONE', *, *, #44093, .T. ) ;
#4974 = CARTESIAN_POINT ( 'NONE',  ( 0.2471922599940329923, -0.09336655125506174158, 0.03811991455052975847 ) ) ;
#4975 = EDGE_CURVE ( 'NONE', #11301, #39475, #11250, .T. ) ;
#4976 = CARTESIAN_POINT ( 'NONE',  ( -0.9500414927467377701, -0.1787899950787401604, 1.555118110182457158 ) ) ;
#4977 = ADVANCED_FACE ( 'NONE', ( #11727 ), #31705, .T. ) ;
#4978 = CARTESIAN_POINT ( 'NONE',  ( 0.07405724077823318263, -1.553149606245448178, -0.1787899950787401604 ) ) ;
#4979 = CARTESIAN_POINT ( 'NONE',  ( -0.1787899950787401882, -1.575295275536787276, 0.000000000000000000 ) ) ;
#4980 = DIRECTION ( 'NONE',  ( -1.000000000000000000, 0.000000000000000000, 0.000000000000000000 ) ) ;
#4981 = CARTESIAN_POINT ( 'NONE',  ( 0.1626913500753331410, -0.07997641687420671552, 0.1385231884448369366 ) ) ;
#4982 = CARTESIAN_POINT ( 'NONE',  ( 0.7185039370078746268, 0.06523048226347956391, 0.4995078740157484765 ) ) ;
#4983 = AXIS2_PLACEMENT_3D ( 'NONE', #45204, #30190, #41841 ) ;
#4984 = VECTOR ( 'NONE', #6909, 39.37007874015748143 ) ;
#4985 = CARTESIAN_POINT ( 'NONE',  ( 0.2395294000716133853, 3.218313930830148909E-16, -1.043307086614172707 ) ) ;
#4986 = CARTESIAN_POINT ( 'NONE',  ( -1.033464566929134687, 0.06523048226347956391, 1.183562992018456272 ) ) ;
#4987 = CARTESIAN_POINT ( 'NONE',  ( 1.002407869896990045, -0.1264236179284866091, 0.4945866141194645849 ) ) ;
#4988 = CARTESIAN_POINT ( 'NONE',  ( 0.9500414927467377701, -0.1787899950787401604, 0.05413385821395302888 ) ) ;
#4989 = CARTESIAN_POINT ( 'NONE',  ( 0.06523048226347956391, -0.3941929133858267931, -0.1574803149606300301 ) ) ;
#4990 = CIRCLE ( 'NONE', #21061, 0.5905511811023623769 ) ;
#4991 = CONICAL_SURFACE ( 'NONE', #34891, 0.1377952755905510474, 0.9599310885968920237 ) ;
#4992 = CARTESIAN_POINT ( 'NONE',  ( -0.2066929133858267931, 0.09275486626281861935, -0.1104648588920805335 ) ) ;
#4993 = VERTEX_POINT ( 'NONE', #25860 ) ;
#4994 = CARTESIAN_POINT ( 'NONE',  ( -0.1368215936367279117, -0.09383385973766106281, -0.1150912892199234677 ) ) ;
#4995 = CARTESIAN_POINT ( 'NONE',  ( -0.6971942568897637749, 2.189545951927499583E-17, 1.109744094434425232 ) ) ;
#4996 = CARTESIAN_POINT ( 'NONE',  ( 0.9412147342319837628, -0.1574803149606297803, 1.026082677165353729 ) ) ;
#4997 = DIRECTION ( 'NONE',  ( -1.000000000000000000, 0.000000000000000000, 0.000000000000000000 ) ) ;
#4998 = DIRECTION ( 'NONE',  ( -1.000000000000000000, 0.000000000000000000, 0.000000000000000000 ) ) ;
#4999 = CARTESIAN_POINT ( 'NONE',  ( 0.7646288533564489232, 0.1113553986120547346, 0.6053149605223937524 ) ) ;
#5000 = CARTESIAN_POINT ( 'NONE',  ( -0.1047703448690850969, -0.08956136656883036118, 0.1211223604329432629 ) ) ;
#5001 = CARTESIAN_POINT ( 'NONE',  ( -1.094772975963752103E-17, -0.5221456692375747721, -0.1787899950787401882 ) ) ;
#5002 = ORIENTED_EDGE ( 'NONE', *, *, #3197, .T. ) ;
#5003 = DIRECTION ( 'NONE',  ( 5.724375810226257641E-16, 0.6156614753256588468, 0.7880107536067216811 ) ) ;
#5004 = ORIENTED_EDGE ( 'NONE', *, *, #28278, .F. ) ;
#5005 = CARTESIAN_POINT ( 'NONE',  ( 0.9412147342319837628, -0.1574803149606297803, 0.8292322834645677876 ) ) ;
#5006 = CARTESIAN_POINT ( 'NONE',  ( 0.9412147342319837628, -0.1574803149606297803, 0.9079724409448817202 ) ) ;
#5007 = CARTESIAN_POINT ( 'NONE',  ( -1.094772975963752103E-17, -1.703248031442299304, -0.1787899950787401882 ) ) ;
#5008 = CARTESIAN_POINT ( 'NONE',  ( -0.1787899950787401604, -0.8297244093950564281, 0.07405724077823318263 ) ) ;
#5009 = CARTESIAN_POINT ( 'NONE',  ( 0.06523048226347956391, -1.196358267716536306, 0.1574803149606297803 ) ) ;
#5010 = CARTESIAN_POINT ( 'NONE',  ( 0.7185039370078746268, -0.06523048226347956391, 1.203248031388535200 ) ) ;
#5011 = DIRECTION ( 'NONE',  ( 0.000000000000000000, -0.7880107536067216811, 0.6156614753256587358 ) ) ;
#5012 = ORIENTED_EDGE ( 'NONE', *, *, #46777, .T. ) ;
#5013 = ORIENTED_EDGE ( 'NONE', *, *, #23048, .F. ) ;
#5014 = CARTESIAN_POINT ( 'NONE',  ( -1.054774247047244540, -0.07405724077823318263, 1.796259842465923073 ) ) ;
#5015 = CARTESIAN_POINT ( 'NONE',  ( 0.8759842519685039353, 0.1787899950787401882, 1.808562992072220377 ) ) ;
#5016 = ORIENTED_EDGE ( 'NONE', *, *, #12269, .T. ) ;
#5017 = CARTESIAN_POINT ( 'NONE',  ( -0.1113553986120547346, -1.390748031388535422, 0.1113553986120547346 ) ) ;
#5018 = CARTESIAN_POINT ( 'NONE',  ( -0.8019270111902717657, 0.1787899950787401604, 0.9055118109698585549 ) ) ;
#5019 = CARTESIAN_POINT ( 'NONE',  ( -0.06197108496686676293, -0.2597152231171959147, -0.3085539532670581453 ) ) ;
#5020 = CARTESIAN_POINT ( 'NONE',  ( 0.7495606340400177148, 0.1264236179284866091, 0.3961614172690708924 ) ) ;
#5021 = CARTESIAN_POINT ( 'NONE',  ( -0.6971942568897648851, -0.07405724077823297447, 1.304133858213953667 ) ) ;
#5022 = AXIS2_PLACEMENT_3D ( 'NONE', #20568, #24186, #12707 ) ;
#5023 = FACE_OUTER_BOUND ( 'NONE', #22860, .T. ) ;
#5024 = CARTESIAN_POINT ( 'NONE',  ( -1.054774247047244540, 0.07405724077823318263, 0.1082677164816695514 ) ) ;
#5025 = DIRECTION ( 'NONE',  ( -3.469446951953613794E-15, -1.000000000000000000, 0.000000000000000000 ) ) ;
#5026 = CARTESIAN_POINT ( 'NONE',  ( -0.7495606340400177148, 0.1264236179284866091, 1.813484251914740053 ) ) ;
#5027 = DIRECTION ( 'NONE',  ( -6.938893903907229955E-15, 0.000000000000000000, -1.000000000000000000 ) ) ;
#5028 = CARTESIAN_POINT ( 'NONE',  ( -0.7185039370078746268, 0.06523048226347956391, 1.798720472440944462 ) ) ;
#5029 = CARTESIAN_POINT ( 'NONE',  ( -0.8759842519685039353, -0.1574803149606299191, 0.9448818897637796255 ) ) ;
#5030 = CARTESIAN_POINT ( 'NONE',  ( 0.8759842519685039353, -0.1787899950787401882, 1.552657480261196765 ) ) ;
#5031 = CARTESIAN_POINT ( 'NONE',  ( -0.2006030091703118190, -0.09842519685039370636, -0.1463775445859769597 ) ) ;
#5032 = FACE_OUTER_BOUND ( 'NONE', #38704, .T. ) ;
#5033 = AXIS2_PLACEMENT_3D ( 'NONE', #38406, #23332, #30091 ) ;
#5034 = AXIS2_PLACEMENT_3D ( 'NONE', #41786, #27710, #8985 ) ;
#5035 = EDGE_CURVE ( 'NONE', #11957, #27881, #4029, .T. ) ;
#5036 = VERTEX_POINT ( 'NONE', #40906 ) ;
#5037 = ORIENTED_EDGE ( 'NONE', *, *, #424, .F. ) ;
#5038 = EDGE_CURVE ( 'NONE', #39764, #19512, #8104, .T. ) ;
#5039 = CARTESIAN_POINT ( 'NONE',  ( -0.1264236179284866091, -0.8666338582139527791, 0.1264236179284866091 ) ) ;
#5040 = CARTESIAN_POINT ( 'NONE',  ( 0.1787899950787401604, -1.085629921206079374, 0.07405724077823318263 ) ) ;
#5041 = CARTESIAN_POINT ( 'NONE',  ( -0.7185039370078746268, -0.06523048226347956391, 0.5831692913385827515 ) ) ;
#5042 = ( NAMED_UNIT ( * ) PLANE_ANGLE_UNIT ( ) SI_UNIT ( $, .RADIAN. ) ) ;
#5043 = MANIFOLD_SOLID_BREP ( 'U-Bolt', #7231 ) ;
#5044 = CARTESIAN_POINT ( 'NONE',  ( 3.301370929368692659E-17, -0.3848863292680850257, 0.1797182628040039365 ) ) ;
#5045 = CARTESIAN_POINT ( 'NONE',  ( 0.1574803149606300301, -1.811515747923969410, 0.06523048226347956391 ) ) ;
#5046 = CARTESIAN_POINT ( 'NONE',  ( -0.1476377952755905387, -0.9875035750853327077, -1.463737590216208861 ) ) ;
#5047 = CARTESIAN_POINT ( 'NONE',  ( 0.1787899950787401604, -0.1801181101824570474, -0.07405724077823318263 ) ) ;
#5048 = CIRCLE ( 'NONE', #3558, 0.2471922904502826812 ) ;
#5049 = CARTESIAN_POINT ( 'NONE',  ( -0.3551574803149606385, -2.130889186148732174E-17, 0.000000000000000000 ) ) ;
#5050 = CARTESIAN_POINT ( 'NONE',  ( 0.6971942568897626646, 0.07405724077823318263, 0.9842519684501742638 ) ) ;
#5051 = ( LENGTH_UNIT ( ) NAMED_UNIT ( * ) SI_UNIT ( $, .METRE. ) ) ;
#5052 = DIRECTION ( 'NONE',  ( 0.000000000000000000, 0.000000000000000000, -1.000000000000000000 ) ) ;
#5053 = CARTESIAN_POINT ( 'NONE',  ( 0.9873396505805591694, 0.1113553986120547346, 0.08366141721530767628 ) ) ;
#5054 = CARTESIAN_POINT ( 'NONE',  ( 0.7185039370078739607, 1.928577636452523993E-17, 0.06889763779527559306 ) ) ;
#5055 = CARTESIAN_POINT ( 'NONE',  ( 1.033464566929133799, 0.000000000000000000, 1.584645669291338654 ) ) ;
#5057 = CARTESIAN_POINT ( 'NONE',  ( -0.07405724077823318263, -0.3917322834108032947, 0.1787899950787401604 ) ) ;
#5056 = CARTESIAN_POINT ( 'NONE',  ( 0.06523048226347956391, -0.9749015746956224415, -0.1574803149606300301 ) ) ;
#5058 = DIRECTION ( 'NONE',  ( 0.000000000000000000, 0.000000000000000000, 1.000000000000000000 ) ) ;
#5059 = CARTESIAN_POINT ( 'NONE',  ( -0.1787899950787401604, -1.179133858213953001, 0.07405724077823318263 ) ) ;
#5060 = CARTESIAN_POINT ( 'NONE',  ( 0.9500414927467378812, 0.1787899950787401604, 0.3494094487651343006 ) ) ;
#5061 = EDGE_CURVE ( 'NONE', #36464, #14105, #37111, .T. ) ;
#5062 = CARTESIAN_POINT ( 'NONE',  ( -0.7495606340400177148, 0.1264236179284866091, 1.729822834591905556 ) ) ;
#5063 = ORIENTED_EDGE ( 'NONE', *, *, #24553, .F. ) ;
#5064 = CARTESIAN_POINT ( 'NONE',  ( -0.8019270111902717657, -0.1787899950787401604, 1.235236220418678199 ) ) ;
#5065 = CARTESIAN_POINT ( 'NONE',  ( 0.6971942568897637749, 2.189545951927499583E-17, 1.464074803095842370 ) ) ;
#5066 = CARTESIAN_POINT ( 'NONE',  ( -1.002407869896990045, -0.1264236179284866091, 0.4945866141194645849 ) ) ;
#5067 = CARTESIAN_POINT ( 'NONE',  ( -0.8759842519685039353, 0.1787899950787401882, 1.252460629867496067 ) ) ;
#5068 = CARTESIAN_POINT ( 'NONE',  ( 1.033464566929133799, 0.000000000000000000, 0.6692913384751496553 ) ) ;
#5069 = CARTESIAN_POINT ( 'NONE',  ( -0.07210009817454927916, -0.09842519241363902049, -0.1636076842217463745 ) ) ;
#5070 = CARTESIAN_POINT ( 'NONE',  ( 0.8759842519685039353, 0.1574803149606299191, 1.200787401574803237 ) ) ;
#5071 = CARTESIAN_POINT ( 'NONE',  ( 0.7495606340400177148, 0.1264236179284866091, 0.4749015747493858242 ) ) ;
#5072 = CARTESIAN_POINT ( 'NONE',  ( -1.054774247047244096, 0.000000000000000000, 0.3371062991588349989 ) ) ;
#5073 = CARTESIAN_POINT ( 'NONE',  ( -1.033464566929134687, 0.06523048226347956391, 0.8686023620971983217 ) ) ;
#5074 = ORIENTED_EDGE ( 'NONE', *, *, #19360, .F. ) ;
#5075 = CARTESIAN_POINT ( 'NONE',  ( -0.7646288533564489232, 0.1113553986120547346, 0.3001968503937008093 ) ) ;
#5076 = CARTESIAN_POINT ( 'NONE',  ( 0.7495606340400177148, -0.1264236179284866091, 1.232775590497417362 ) ) ;
#5077 = CARTESIAN_POINT ( 'NONE',  ( -0.8019270111902716547, -0.1787899950787401604, 1.978346456639149098 ) ) ;
#5078 = CARTESIAN_POINT ( 'NONE',  ( -0.9873396505805591694, -0.1113553986120547346, 1.973425196850393970 ) ) ;
#5079 = VERTEX_POINT ( 'NONE', #20073 ) ;
#5080 = DIRECTION ( 'NONE',  ( -1.000000000000000000, 0.000000000000000000, 0.000000000000000000 ) ) ;
#5081 = EDGE_CURVE ( 'NONE', #6761, #11244, #34543, .T. ) ;
#5082 = FACE_OUTER_BOUND ( 'NONE', #14954, .T. ) ;
#5083 = CARTESIAN_POINT ( 'NONE',  ( 3.284318927891251994E-17, -1.384474361930025932, 0.1787899950787401882 ) ) ;
#5084 = EDGE_LOOP ( 'NONE', ( #8206, #18474, #22572, #33078 ) ) ;
#5085 = CARTESIAN_POINT ( 'NONE',  ( -1.033464566929134687, 0.06523048226347956391, 0.1599409447743626866 ) ) ;
#5086 = CARTESIAN_POINT ( 'NONE',  ( -0.1264236179284866091, -0.3597440944344256208, -0.1264236179284866091 ) ) ;
#5087 = CARTESIAN_POINT ( 'NONE',  ( -0.3076751137723113261, -0.03860885780051057786, 1.038887198594754979 ) ) ;
#5088 = CARTESIAN_POINT ( 'NONE',  ( 1.054774247047244096, 0.000000000000000000, 1.281988188922614125 ) ) ;
#5089 = CARTESIAN_POINT ( 'NONE',  ( 0.7646288533564489232, 0.1113553986120547346, 0.8907480314960629642 ) ) ;
#5090 = LINE ( 'NONE', #45093, #36106 ) ;
#5091 = FACE_OUTER_BOUND ( 'NONE', #34210, .T. ) ;
#5092 = CARTESIAN_POINT ( 'NONE',  ( 0.9500414927467378812, 0.1787899950787401604, 1.643700787347811998 ) ) ;
#5093 = CARTESIAN_POINT ( 'NONE',  ( -1.094772975963752103E-17, 0.1312736695660370045, -0.1787899950787401882 ) ) ;
#5094 = CARTESIAN_POINT ( 'NONE',  ( 0.07405724077823318263, -1.784448818843874962, -0.1787899950787401604 ) ) ;
#5095 = CARTESIAN_POINT ( 'NONE',  ( 0.1564304382124598325, -0.09842519685039370636, 0.07442043211813872960 ) ) ;
#5096 = CARTESIAN_POINT ( 'NONE',  ( -0.8759842519685039353, -0.1787899950787401882, 0.6865157479777322935 ) ) ;
#5098 = DIRECTION ( 'NONE',  ( 1.822029033848725028E-16, 0.000000000000000000, 1.000000000000000000 ) ) ;
#5097 = CARTESIAN_POINT ( 'NONE',  ( 0.1574803149606300301, -0.7928149606299216279, -0.06523048226347956391 ) ) ;
#5099 = CARTESIAN_POINT ( 'NONE',  ( -0.07444174185955065859, -1.622583179661785779, -0.1797182628040039087 ) ) ;
#5100 = CARTESIAN_POINT ( 'NONE',  ( 0.7185039370078739607, 1.928577636452523993E-17, 0.2263779527559055260 ) ) ;
#5101 = CARTESIAN_POINT ( 'NONE',  ( 0.2471922904502826535, 0.09275221067063772751, -0.04038095640780214185 ) ) ;
#5102 = CARTESIAN_POINT ( 'NONE',  ( 1.054774247047244540, -0.07405724077823318263, 1.481299212544662680 ) ) ;
#5103 = CARTESIAN_POINT ( 'NONE',  ( 0.8019270111902716547, 0.1787899950787401604, 1.884842519631275026 ) ) ;
#5104 = CARTESIAN_POINT ( 'NONE',  ( 1.054774247047244540, -0.07405724077823318263, 0.2952755904974176948 ) ) ;
#5105 = ORIENTED_EDGE ( 'NONE', *, *, #46473, .T. ) ;
#5107 = ORIENTED_EDGE ( 'NONE', *, *, #46612, .T. ) ;
#5106 = DIRECTION ( 'NONE',  ( 1.822029033848725028E-16, 0.000000000000000000, 1.000000000000000000 ) ) ;
#5108 = DIRECTION ( 'NONE',  ( -0.8191520442889873577, 1.003171929053519323E-16, 0.5735764363510523767 ) ) ;
#5109 = LINE ( 'NONE', #22862, #41211 ) ;
#5111 = CARTESIAN_POINT ( 'NONE',  ( 0.1787899950787401882, 0.05364173233722811102, -2.189545951927503898E-17 ) ) ;
#5110 = CARTESIAN_POINT ( 'NONE',  ( -9.642888182262618425E-18, -0.8543307085538898171, -0.1574803149606299191 ) ) ;
#5112 = CARTESIAN_POINT ( 'NONE',  ( -1.033464566929133799, 0.000000000000000000, 0.1673228346456692994 ) ) ;
#5113 = CARTESIAN_POINT ( 'NONE',  ( 0.7495606340400177148, 0.1264236179284866091, 0.4306102361667086820 ) ) ;
#5114 = ADVANCED_FACE ( 'NONE', ( #30201 ), #32568, .T. ) ;
#5115 = CARTESIAN_POINT ( 'NONE',  ( -1.033464566929133799, 0.000000000000000000, 1.574803149498771537 ) ) ;
#5116 = CARTESIAN_POINT ( 'NONE',  ( 0.8759842519685039353, -0.1574803149606299191, 0.7775590550105826448 ) ) ;
#5117 = ORIENTED_EDGE ( 'NONE', *, *, #23549, .T. ) ;
#5118 = CARTESIAN_POINT ( 'NONE',  ( 0.000000000000000000, 0.1102362204724409434, 0.000000000000000000 ) ) ;
#5119 = CARTESIAN_POINT ( 'NONE',  ( 0.8481319853008726373, 0.1739929071186617493, 0.03937007952913684772 ) ) ;
#5120 = ORIENTED_EDGE ( 'NONE', *, *, #43445, .T. ) ;
#5122 = CARTESIAN_POINT ( 'NONE',  ( 0.1787899950787401882, -1.324311023568283341, -2.189545951927503898E-17 ) ) ;
#5121 = CARTESIAN_POINT ( 'NONE',  ( 0.06523048226347956391, -1.093011810916094451, -0.1574803149606300301 ) ) ;
#5123 = CARTESIAN_POINT ( 'NONE',  ( -0.7185039370078746268, -0.06523048226347956391, 0.5733267715460159675 ) ) ;
#5124 = DIRECTION ( 'NONE',  ( -0.000000000000000000, 1.000000000000000000, -0.000000000000000000 ) ) ;
#5125 = CARTESIAN_POINT ( 'NONE',  ( -0.8759842519685039353, 0.1574803149606299191, 1.240157480314960647 ) ) ;
#5126 = CARTESIAN_POINT ( 'NONE',  ( -1.033464566929133799, 0.000000000000000000, 1.978346456692913646 ) ) ;
#5128 = CARTESIAN_POINT ( 'NONE',  ( -0.7185039370078746268, 0.06523048226347956391, 0.7652559054042838982 ) ) ;
#5127 = CARTESIAN_POINT ( 'NONE',  ( -0.8759842519685039353, 0.000000000000000000, 0.000000000000000000 ) ) ;
#5129 = CARTESIAN_POINT ( 'NONE',  ( 0.8107537697050254399, -0.1574803149606297803, 1.916830708553890483 ) ) ;
#5130 = CARTESIAN_POINT ( 'NONE',  ( 0.7185039370078746268, 0.06523048226347956391, 1.434547243986962428 ) ) ;
#5131 = ORIENTED_EDGE ( 'NONE', *, *, #12269, .F. ) ;
#5132 = VERTEX_POINT ( 'NONE', #37824 ) ;
#5133 = CARTESIAN_POINT ( 'NONE',  ( -0.01960094289347295154, -0.05179116514251731057, -0.2741164612102225950 ) ) ;
#5134 = EDGE_LOOP ( 'NONE', ( #14252, #38748, #44441, #32739, #28557, #35520, #1237, #38379, #3137, #241, #10330, #17989 ) ) ;
#5135 = CARTESIAN_POINT ( 'NONE',  ( 0.9500414927467378812, -0.1787899950787401604, 0.6889763778989935750 ) ) ;
#5136 = EDGE_CURVE ( 'NONE', #40935, #12702, #19361, .T. ) ;
#5137 = CARTESIAN_POINT ( 'NONE',  ( 0.6971942568897648851, -0.07405724077823297447, 0.9547244093950545407 ) ) ;
#5138 = CARTESIAN_POINT ( 'NONE',  ( 0.1113553986120547346, -0.002952755797984771627, 0.1113553986120547346 ) ) ;
#5139 = CARTESIAN_POINT ( 'NONE',  ( -0.6971942568897648851, -0.07405724077823297447, 1.230314960576156746 ) ) ;
#5140 = ORIENTED_EDGE ( 'NONE', *, *, #18243, .T. ) ;
#5141 = AXIS2_PLACEMENT_3D ( 'NONE', #9800, #39013, #35676 ) ;
#5142 = ( BOUNDED_CURVE ( )  B_SPLINE_CURVE ( 2, ( #16486, #13366, #34940, #38976, #46169, #38759, #27993, #5447, #1602 ),
 .UNSPECIFIED., .F., .T. ) 
 B_SPLINE_CURVE_WITH_KNOTS ( ( 3, 2, 2, 2, 3 ),
 ( 0.8699999999999999956, 0.8725000000000000533, 0.8750000000000000000, 0.8774999999999999467, 0.8800000000000000044 ),
 .UNSPECIFIED. ) 
 CURVE ( )  GEOMETRIC_REPRESENTATION_ITEM ( )  RATIONAL_B_SPLINE_CURVE ( ( 1.000000000000000000, 0.9238795325112899581, 1.000000000000000000, 0.9238795325112869605, 1.000000000000000000, 0.9238795325112869605, 1.000000000000000000, 0.9238795325112869605, 1.000000000000000000 ) ) 
 REPRESENTATION_ITEM ( '' )  ) ;
#5143 = ADVANCED_FACE ( 'NONE', ( #16495 ), #27981, .F. ) ;
#5144 = CARTESIAN_POINT ( 'NONE',  ( 0.1184675242425078795, -0.09842519685039370636, 1.713085361781127913 ) ) ;
#5145 = DIRECTION ( 'NONE',  ( 0.000000000000000000, 1.000000000000000000, 0.000000000000000000 ) ) ;
#5146 = ( BOUNDED_CURVE ( )  B_SPLINE_CURVE ( 2, ( #39064, #20858, #2641, #46492, #32137, #6474, #2871, #46730, #9142 ),
 .UNSPECIFIED., .F., .T. ) 
 B_SPLINE_CURVE_WITH_KNOTS ( ( 3, 2, 2, 2, 3 ),
 ( 0.4500000000000000111, 0.4525000000000000133, 0.4550000000000000155, 0.4575000000000000178, 0.4600000000000000200 ),
 .UNSPECIFIED. ) 
 CURVE ( )  GEOMETRIC_REPRESENTATION_ITEM ( )  RATIONAL_B_SPLINE_CURVE ( ( 1.000000000000000000, 0.9238795325112869605, 1.000000000000000000, 0.9238795325112869605, 1.000000000000000000, 0.9238795325112869605, 1.000000000000000000, 0.9238795325112869605, 1.000000000000000000 ) ) 
 REPRESENTATION_ITEM ( '' )  ) ;
#5147 = CARTESIAN_POINT ( 'NONE',  ( 0.8759842519685039353, 0.1574803149606299191, 0.8759842518609765039 ) ) ;
#5148 = CARTESIAN_POINT ( 'NONE',  ( 0.1787899950787401604, -0.9833916847646722026, 0.07405724077823318263 ) ) ;
#5149 = ORIENTED_EDGE ( 'NONE', *, *, #33424, .F. ) ;
#5150 = CARTESIAN_POINT ( 'NONE',  ( 0.1264236179284866091, -0.02509842514308689362, 0.1264236179284866091 ) ) ;
#5151 = ORIENTED_EDGE ( 'NONE', *, *, #40888, .F. ) ;
#5152 = VERTEX_POINT ( 'NONE', #26816 ) ;
#5153 = EDGE_CURVE ( 'NONE', #5859, #27600, #43219, .T. ) ;
#5154 = CARTESIAN_POINT ( 'NONE',  ( -0.7185039370078778465, -0.06523048226348396317, 1.400098425089323140 ) ) ;
#5155 = CARTESIAN_POINT ( 'NONE',  ( 0.7185039370078746268, -0.06523048226347956391, 0.1008858266641264878 ) ) ;
#5156 = PRODUCT ( 'Threaded Bushing', 'Threaded Bushing', '', ( #33903 ) ) ;
#5157 = CARTESIAN_POINT ( 'NONE',  ( -0.1264236179284866091, -0.6402559054580471143, -0.1264236179284866091 ) ) ;
#5158 = CARTESIAN_POINT ( 'NONE',  ( -1.054774247047244540, -0.07405724077823318263, 0.1820866141194649179 ) ) ;
#5159 = CARTESIAN_POINT ( 'NONE',  ( -1.033464566929133799, 0.000000000000000000, 1.072834645669291431 ) ) ;
#5160 = DIRECTION ( 'NONE',  ( -0.000000000000000000, -0.000000000000000000, -1.000000000000000000 ) ) ;
#5161 = CARTESIAN_POINT ( 'NONE',  ( -0.1586641775163213364, 0.4457451269443606368, -1.671447902550282194 ) ) ;
#5162 = CARTESIAN_POINT ( 'NONE',  ( -0.07444174185955065859, -1.110772156039737890, -0.1797182628040039087 ) ) ;
#5163 = CARTESIAN_POINT ( 'NONE',  ( 0.8759842519685039353, 0.1574803149606299191, 0.4133858267716535861 ) ) ;
#5164 = CARTESIAN_POINT ( 'NONE',  ( 1.054774247047244540, -0.07405724077823318263, 0.9694881889226144578 ) ) ;
#5165 = CARTESIAN_POINT ( 'NONE',  ( 1.054774247047244540, -0.07405724077823318263, 0.1377952755367876370 ) ) ;
#5166 = CARTESIAN_POINT ( 'NONE',  ( -1.033464566929134687, 0.06523048226347956391, 0.6323818896562525271 ) ) ;
#5167 = CARTESIAN_POINT ( 'NONE',  ( 0.9873396505805591694, -0.1113553986120547346, 1.540354330708661568 ) ) ;
#5168 = CARTESIAN_POINT ( 'NONE',  ( 0.7252227560879499491, -0.07532008605015085012, 1.984724907739004562 ) ) ;
#5169 = CARTESIAN_POINT ( 'NONE',  ( 0.1574803149606307795, -0.4026036378687909423, -0.9257984838013391116 ) ) ;
#5170 = CARTESIAN_POINT ( 'NONE',  ( -0.06523048226347956391, -0.7337598424121570817, -0.1574803149606300301 ) ) ;
#5171 = AXIS2_PLACEMENT_3D ( 'NONE', #10923, #36067, #17855 ) ;
#5172 = CARTESIAN_POINT ( 'NONE',  ( 0.4736248074375835060, 1.690605217543005745, -0.5092277576975118292 ) ) ;
#5173 = LINE ( 'NONE', #15756, #16894 ) ;
#5174 = CARTESIAN_POINT ( 'NONE',  ( 0.8759842519685039353, -0.1787899950787401882, 0.9571850393163149340 ) ) ;
#5175 = CARTESIAN_POINT ( 'NONE',  ( 0.8759842519685039353, -0.1787899950787401882, 1.867618110182456714 ) ) ;
#5176 = CARTESIAN_POINT ( 'NONE',  ( 1.033464566929134687, 0.06523048226347956391, 0.2780511809948349455 ) ) ;
#5177 = VERTEX_POINT ( 'NONE', #12910 ) ;
#5178 = CARTESIAN_POINT ( 'NONE',  ( 1.033464566929133799, 0.000000000000000000, 1.702755905511810885 ) ) ;
#5179 = CARTESIAN_POINT ( 'NONE',  ( -0.1574803149606300301, -1.713090551073575662, -0.06523048226347956391 ) ) ;
#5180 = VERTEX_POINT ( 'NONE', #38054 ) ;
#5181 = CARTESIAN_POINT ( 'NONE',  ( 0.8759842519685039353, 0.1787899950787401882, 1.173720472387181246 ) ) ;
#5182 = EDGE_CURVE ( 'NONE', #17013, #26517, #16474, .T. ) ;
#5183 = CARTESIAN_POINT ( 'NONE',  ( 0.1121660444095479159, -0.09796987684348244796, 0.2206716537553182755 ) ) ;
#5184 = CARTESIAN_POINT ( 'NONE',  ( -0.1787899950787401604, 0.1151574803687242243, -0.07405724077823318263 ) ) ;
#5185 = CYLINDRICAL_SURFACE ( 'NONE', #16100, 0.1574803149606299191 ) ;
#5186 = EDGE_CURVE ( 'NONE', #38980, #34169, #10341, .T. ) ;
#5187 = CARTESIAN_POINT ( 'NONE',  ( -1.054774247047244540, 0.07405724077823318263, 0.5364173227808821665 ) ) ;
#5188 = CARTESIAN_POINT ( 'NONE',  ( -0.04878249046419594337, 0.07306521771081592176, 0.2572684868648978385 ) ) ;
#5189 = ADVANCED_FACE ( 'NONE', ( #21246 ), #28719, .T. ) ;
#5190 = CARTESIAN_POINT ( 'NONE',  ( -0.1787899950787401882, -1.501476377898992354, 0.000000000000000000 ) ) ;
#5191 = CARTESIAN_POINT ( 'NONE',  ( -1.002407869896990045, -0.1264236179284866091, 1.788877952702141672 ) ) ;
#5192 = ORIENTED_EDGE ( 'NONE', *, *, #4803, .T. ) ;
#5193 = CARTESIAN_POINT ( 'NONE',  ( -0.7495606340400177148, 0.1264236179284866091, 0.4749015747493858242 ) ) ;
#5194 = DIRECTION ( 'NONE',  ( -1.000000000000000000, 0.000000000000000000, 0.000000000000000000 ) ) ;
#5195 = AXIS2_PLACEMENT_3D ( 'NONE', #25872, #29283, #44287 ) ;
#5196 = DIRECTION ( 'NONE',  ( 0.000000000000000000, -0.6156614753256597350, -0.7880107536067206819 ) ) ;
#5197 = CARTESIAN_POINT ( 'NONE',  ( 0.1787899950787401604, -0.5453995587804200129, -0.07405724077823318263 ) ) ;
#5198 = CARTESIAN_POINT ( 'NONE',  ( 0.1875465240539248013, -0.08956051620222618692, -0.06933865474359547643 ) ) ;
#5199 = DIRECTION ( 'NONE',  ( -1.000000000000000000, 0.000000000000000000, 0.000000000000000000 ) ) ;
#5200 = DIRECTION ( 'NONE',  ( 1.822029033848725028E-16, 0.000000000000000000, 1.000000000000000000 ) ) ;
#5201 = CARTESIAN_POINT ( 'NONE',  ( -1.033464566929133799, 1.928577636452524610E-17, 2.869337061179095023E-17 ) ) ;
#5202 = AXIS2_PLACEMENT_3D ( 'NONE', #8256, #4652, #37974 ) ;
#5203 = CARTESIAN_POINT ( 'NONE',  ( -1.002407869896990045, -0.1264236179284866091, 0.4896653542769449086 ) ) ;
#5204 = CARTESIAN_POINT ( 'NONE',  ( 0.1787899950787401882, -1.807702708386720536, -2.189545951927503898E-17 ) ) ;
#5205 = ORIENTED_EDGE ( 'NONE', *, *, #25069, .F. ) ;
#5206 = CARTESIAN_POINT ( 'NONE',  ( -0.6971942568897648851, 0.07405724077823318263, 1.461614173174583753 ) ) ;
#5207 = CARTESIAN_POINT ( 'NONE',  ( 0.1264236179284866091, -1.476870078686393750, -0.1264236179284866091 ) ) ;
#5208 = CARTESIAN_POINT ( 'NONE',  ( 0.1377952755905512139, -1.365923996832131609E-16, -0.9074803149606294195 ) ) ;
#5209 = CARTESIAN_POINT ( 'NONE',  ( 0.1624141299425573837, -0.07987878989917683581, 0.1383517943471609946 ) ) ;
#5210 = CARTESIAN_POINT ( 'NONE',  ( 0.8107537697050253289, -0.1574803149606297803, 0.5093503937007877180 ) ) ;
#5211 = CARTESIAN_POINT ( 'NONE',  ( -0.1797182628040039087, -0.7072288489531255440, 0.07444174185955065859 ) ) ;
#5212 = FACE_OUTER_BOUND ( 'NONE', #36520, .T. ) ;
#5213 = CARTESIAN_POINT ( 'NONE',  ( -0.7185039370078746268, 0.06523048226347956391, 1.277066929026331898 ) ) ;
#5214 = CARTESIAN_POINT ( 'NONE',  ( 0.6971942568897626646, -0.07405724077823297447, 0.5610236219934807700 ) ) ;
#5216 = CARTESIAN_POINT ( 'NONE',  ( 0.7185039370078739607, 1.928577636452523993E-17, 1.092519685039370136 ) ) ;
#5215 = CARTESIAN_POINT ( 'NONE',  ( -0.1574803149606300301, -0.3843503937007873850, -0.06523048226347956391 ) ) ;
#5217 = DIRECTION ( 'NONE',  ( -1.000000000000000000, 0.000000000000000000, 0.000000000000000000 ) ) ;
#5218 = ORIENTED_EDGE ( 'NONE', *, *, #13436, .F. ) ;
#5219 = CARTESIAN_POINT ( 'NONE',  ( 0.1476377952755906220, -0.2274162997038010614, -0.9219983537151217323 ) ) ;
#5220 = CARTESIAN_POINT ( 'NONE',  ( -0.7495606340400177148, 0.1264236179284866091, 1.065452755851747924 ) ) ;
#5221 = CARTESIAN_POINT ( 'NONE',  ( 0.7185039370078739607, 1.928577636452523993E-17, 1.171259842519684957 ) ) ;
#5222 = FACE_OUTER_BOUND ( 'NONE', #34751, .T. ) ;
#5223 = CARTESIAN_POINT ( 'NONE',  ( -0.6195511811023656223, 0.000000000000000000, -1.186023622047243986 ) ) ;
#5225 = FACE_OUTER_BOUND ( 'NONE', #36959, .T. ) ;
#5224 = CARTESIAN_POINT ( 'NONE',  ( -0.6195511811023656223, 0.4133858267716533086, 0.9891732283464566011 ) ) ;
#5226 = VECTOR ( 'NONE', #25768, 39.37007874015748143 ) ;
#5227 = CARTESIAN_POINT ( 'NONE',  ( -0.7185039370078739607, 0.000000000000000000, -2.869337061179095023E-17 ) ) ;
#5228 = CARTESIAN_POINT ( 'NONE',  ( -0.1604156661162643716, -0.08956087497259392072, -0.06661183193370925903 ) ) ;
#5229 = CARTESIAN_POINT ( 'NONE',  ( 0.1264236179284866091, -0.6058070865604094912, -0.1264236179284866091 ) ) ;
#5230 = CARTESIAN_POINT ( 'NONE',  ( 0.7185039370078739607, 1.928577636452523993E-17, 0.9251968502861732668 ) ) ;
#5231 = ORIENTED_EDGE ( 'NONE', *, *, #1719, .T. ) ;
#5232 = CARTESIAN_POINT ( 'NONE',  ( -0.7185039370078739607, 1.928577636452523993E-17, 0.5708661416247566844 ) ) ;
#5233 = CARTESIAN_POINT ( 'NONE',  ( 1.033464566929133799, 0.000000000000000000, 0.8759842519685039353 ) ) ;
#5234 = CARTESIAN_POINT ( 'NONE',  ( 1.002407869896990045, -0.1264236179284866091, 0.7258858267178898149 ) ) ;
#5235 = EDGE_CURVE ( 'NONE', #17977, #3732, #31823, .T. ) ;
#5236 = EDGE_LOOP ( 'NONE', ( #11509, #43297, #18749, #39900 ) ) ;
#5237 = DIRECTION ( 'NONE',  ( -5.464378949326941559E-15, -1.000000000000000000, 0.000000000000000000 ) ) ;
#5238 = CARTESIAN_POINT ( 'NONE',  ( 0.000000000000000000, 0.000000000000000000, -0.1966003937007873570 ) ) ;
#5239 = CARTESIAN_POINT ( 'NONE',  ( 0.1787899950787401604, -1.749999999946236340, -0.07405724077823318263 ) ) ;
#5240 = CARTESIAN_POINT ( 'NONE',  ( 0.1787899950787401604, -0.9675196849856075865, -0.07405724077823318263 ) ) ;
#5242 = VECTOR ( 'NONE', #12954, 39.37007874015748143 ) ;
#5241 = CARTESIAN_POINT ( 'NONE',  ( -9.642888182262618425E-18, -1.415354330708661568, -0.1574803149606299191 ) ) ;
#5243 = CARTESIAN_POINT ( 'NONE',  ( 0.7646288533564489232, -0.1113553986120547346, 1.087598425089322918 ) ) ;
#5244 = EDGE_CURVE ( 'NONE', #40024, #4309, #17214, .T. ) ;
#5245 = LINE ( 'NONE', #41882, #19114 ) ;
#5246 = VERTEX_POINT ( 'NONE', #31593 ) ;
#5247 = ORIENTED_EDGE ( 'NONE', *, *, #4250, .T. ) ;
#5248 = CARTESIAN_POINT ( 'NONE',  ( -0.8759842519685039353, -0.1787899950787401882, 1.828248031442299082 ) ) ;
#5249 = EDGE_LOOP ( 'NONE', ( #9452, #42557, #37488, #38675 ) ) ;
#5250 = EDGE_CURVE ( 'NONE', #17112, #40844, #28118, .T. ) ;
#5251 = CARTESIAN_POINT ( 'NONE',  ( 0.8019270111902717657, -0.1787899950787401604, 1.904527559001354398 ) ) ;
#5252 = EDGE_LOOP ( 'NONE', ( #21164, #13883, #3389, #45534 ) ) ;
#5253 = CARTESIAN_POINT ( 'NONE',  ( 0.1113553986120547346, -0.002952755797984771627, 0.1113553986120547346 ) ) ;
#5254 = CARTESIAN_POINT ( 'NONE',  ( 0.8759842519685039353, 0.1787899950787401882, 0.3912401574265515491 ) ) ;
#5255 = CARTESIAN_POINT ( 'NONE',  ( -0.8019270111902717657, 0.1787899950787401604, 1.412401574749386990 ) ) ;
#5256 = EDGE_CURVE ( 'NONE', #47128, #1718, #46309, .T. ) ;
#5257 = CARTESIAN_POINT ( 'NONE',  ( 0.05814395269904383545, 0.2619241685425472421, -0.3078067560681213566 ) ) ;
#5258 = CARTESIAN_POINT ( 'NONE',  ( -0.7495606340400177148, 0.1264236179284866091, 0.9030511810485984947 ) ) ;
#5259 = CARTESIAN_POINT ( 'NONE',  ( -0.7495606340400177148, -0.1264236179284866091, 0.09104330703285078152 ) ) ;
#5260 = ( BOUNDED_CURVE ( )  B_SPLINE_CURVE ( 2, ( #9765, #47117, #2781, #35642, #39915, #6855, #46403, #17408, #13365 ),
 .UNSPECIFIED., .F., .T. ) 
 B_SPLINE_CURVE_WITH_KNOTS ( ( 3, 2, 2, 2, 3 ),
 ( 0.1499999999999999944, 0.1524999999999999967, 0.1549999999999999989, 0.1575000000000000011, 0.1600000000000000033 ),
 .UNSPECIFIED. ) 
 CURVE ( )  GEOMETRIC_REPRESENTATION_ITEM ( )  RATIONAL_B_SPLINE_CURVE ( ( 1.000000000000000000, 0.9238795325112869605, 1.000000000000000000, 0.9238795325112869605, 1.000000000000000000, 0.9238795325112869605, 1.000000000000000000, 0.9238795325112869605, 1.000000000000000000 ) ) 
 REPRESENTATION_ITEM ( '' )  ) ;
#5261 = CARTESIAN_POINT ( 'NONE',  ( 0.7185039370078739607, 0.000000000000000000, 4.498031496062992574 ) ) ;
#5262 = CARTESIAN_POINT ( 'NONE',  ( -0.7495606340400177148, 0.1264236179284866091, 1.734744094434425232 ) ) ;
#5263 = CARTESIAN_POINT ( 'NONE',  ( -0.8019270111902717657, -0.1787899950787401604, 0.05413385821395302888 ) ) ;
#5264 = DIRECTION ( 'NONE',  ( 0.000000000000000000, 0.000000000000000000, -1.000000000000000000 ) ) ;
#5265 = CARTESIAN_POINT ( 'NONE',  ( -0.9412147342319837628, -0.1574803149606297803, 1.734744094488190003 ) ) ;
#5266 = CARTESIAN_POINT ( 'NONE',  ( 0.8759842519685039353, 0.000000000000000000, 4.498031496062992574 ) ) ;
#5267 = B_SPLINE_CURVE_WITH_KNOTS ( 'NONE', 3,
 ( #21864, #28848, #3644, #18262, #10619, #32908, #25218, #22980, #39809, #25, #19377, #21624, #1157, #14675, #29347, #11091, #25710, #40281, #7468, #18493, #33146 ),
 .UNSPECIFIED., .F., .F.,
 ( 4, 2, 1, 1, 2, 2, 2, 1, 1, 1, 2, 2, 4 ),
 ( 0.000000000000000000, 0.1250000000000051625, 0.1875000000000077161, 0.2187500000000088540, 0.2343750000000091593, 0.2500000000000094369, 0.3750000000000128786, 0.4375000000000147105, 0.4687500000000155431, 0.4843750000000156541, 0.4921875000000158207, 0.5000000000000159872, 1.000000000000000000 ),
 .UNSPECIFIED. ) ;
#5268 = CARTESIAN_POINT ( 'NONE',  ( 0.8759842519685039353, -0.1787899950787401882, 1.670767716481669440 ) ) ;
#5269 = CARTESIAN_POINT ( 'NONE',  ( 0.2073772511631539750, -0.09842519685039548272, 0.004767299578884354530 ) ) ;
#5270 = CARTESIAN_POINT ( 'NONE',  ( 0.6141732283464567121, 0.000000000000000000, 0.08090551181102362266 ) ) ;
#5271 = CIRCLE ( 'NONE', #26704, 0.09842519685039310962 ) ;
#5272 = ORIENTED_EDGE ( 'NONE', *, *, #15550, .T. ) ;
#5273 = AXIS2_PLACEMENT_3D ( 'NONE', #42105, #9312, #23935 ) ;
#5274 = ORIENTED_EDGE ( 'NONE', *, *, #44773, .F. ) ;
#5275 = CARTESIAN_POINT ( 'NONE',  ( 0.1787899950787401604, -1.006889763725763220, -0.07405724077823318263 ) ) ;
#5276 = CIRCLE ( 'NONE', #29028, 0.1574803149606292529 ) ;
#5277 = ( BOUNDED_CURVE ( )  B_SPLINE_CURVE ( 2, ( #1790, #8506, #19998, #16428, #34178, #31056, #27230, #45621, #34882 ),
 .UNSPECIFIED., .F., .F. ) 
 B_SPLINE_CURVE_WITH_KNOTS ( ( 3, 2, 2, 2, 3 ),
 ( 0.1000000000000000056, 0.1024999999999999939, 0.1049999999999999961, 0.1074999999999999983, 0.1100000000000000006 ),
 .UNSPECIFIED. ) 
 CURVE ( )  GEOMETRIC_REPRESENTATION_ITEM ( )  RATIONAL_B_SPLINE_CURVE ( ( 1.000000000000000000, 0.9238795325112869605, 1.000000000000000000, 0.9238795325112869605, 1.000000000000000000, 0.9238795325112869605, 1.000000000000000000, 0.9238795325112869605, 1.000000000000000000 ) ) 
 REPRESENTATION_ITEM ( '' )  ) ;
#5278 = CARTESIAN_POINT ( 'NONE',  ( -0.1264236179284866091, -1.137303149552535420, 0.1264236179284866091 ) ) ;
#5279 = LENGTH_MEASURE_WITH_UNIT ( LENGTH_MEASURE( 0.02539999999999999897 ), #1431 ) ;
#5280 = CARTESIAN_POINT ( 'NONE',  ( 0.07444174185955065859, -0.4217957780869824869, 0.1797182628040039087 ) ) ;
#5281 = VECTOR ( 'NONE', #27506, 39.37007874015748143 ) ;
#5282 = CARTESIAN_POINT ( 'NONE',  ( -9.642888182262618425E-18, 0.001968503937007873988, -0.1574803149606299191 ) ) ;
#5283 = CARTESIAN_POINT ( 'NONE',  ( 0.8759842519685039353, -0.1787899950787401882, 0.9571850393163149340 ) ) ;
#5285 = CARTESIAN_POINT ( 'NONE',  ( 0.1644020957507537628, -0.08115590401245532937, 0.1405661490837558925 ) ) ;
#5284 = PRESENTATION_STYLE_ASSIGNMENT (( #30489 ) ) ;
#5286 = LINE ( 'NONE', #37402, #15486 ) ;
#5287 = CARTESIAN_POINT ( 'NONE',  ( 0.9500414927467378812, 0.1787899950787401604, 1.963582677111591401 ) ) ;
#5288 = CARTESIAN_POINT ( 'NONE',  ( 0.8107537697050253289, 0.1574803149606300301, 0.2189960629921262614 ) ) ;
#5289 = CARTESIAN_POINT ( 'NONE',  ( -0.7185039370078739607, 0.000000000000000000, -2.869337061179095023E-17 ) ) ;
#5290 = CARTESIAN_POINT ( 'NONE',  ( -1.094772975963752103E-17, -0.4876968503399370380, -0.1787899950787401882 ) ) ;
#5291 = CARTESIAN_POINT ( 'NONE',  ( 0.9412147342319837628, -0.1574803149606297803, 0.1205708661417322358 ) ) ;
#5292 = CARTESIAN_POINT ( 'NONE',  ( 0.1787899950787401882, -1.437499999946236340, -2.189545951927503898E-17 ) ) ;
#5293 = EDGE_CURVE ( 'NONE', #955, #22060, #41209, .T. ) ;
#5294 = AXIS2_PLACEMENT_3D ( 'NONE', #3647, #25483, #21871 ) ;
#5295 = CARTESIAN_POINT ( 'NONE',  ( -0.8019270111902717657, -0.1787899950787401604, 1.781496062938362934 ) ) ;
#5296 = VERTEX_POINT ( 'NONE', #38984 ) ;
#5297 = CARTESIAN_POINT ( 'NONE',  ( -0.6971942568897648851, -0.07405724077823297447, 1.230314960576156746 ) ) ;
#5298 = CARTESIAN_POINT ( 'NONE',  ( -0.8759842519685039353, 0.000000000000000000, 0.000000000000000000 ) ) ;
#5299 = CARTESIAN_POINT ( 'NONE',  ( 0.7495606340400177148, 0.1264236179284866091, 1.380413385773007873 ) ) ;
#5300 = CARTESIAN_POINT ( 'NONE',  ( -0.1113553986120547346, -1.243110236112944689, -0.1113553986120547346 ) ) ;
#5301 = CARTESIAN_POINT ( 'NONE',  ( -0.6971942568897637749, 2.189545951927499583E-17, 1.262303149552535420 ) ) ;
#5302 = ADVANCED_FACE ( 'NONE', ( #16955 ), #34099, .T. ) ;
#5303 = CARTESIAN_POINT ( 'NONE',  ( 0.07763954121060755165, -0.09842560762780139250, -0.1611213105868851969 ) ) ;
#5304 = FACE_OUTER_BOUND ( 'NONE', #39541, .T. ) ;
#5305 = CARTESIAN_POINT ( 'NONE',  ( 0.9500414927467377701, 0.1787899950787401604, 0.6249999999462356737 ) ) ;
#5306 = CARTESIAN_POINT ( 'NONE',  ( -1.054774247047244540, 0.07405724077823318263, 0.3789370078202520253 ) ) ;
#5307 = AXIS2_PLACEMENT_3D ( 'NONE', #24089, #24779, #39377 ) ;
#5308 = CARTESIAN_POINT ( 'NONE',  ( 0.7646288533564489232, 0.1113553986120547346, 1.668307086506645609 ) ) ;
#5309 = ORIENTED_EDGE ( 'NONE', *, *, #9903, .T. ) ;
#5310 = CARTESIAN_POINT ( 'NONE',  ( -0.9873396505805591694, 0.1113553986120547346, 0.2903543307086614012 ) ) ;
#5311 = VECTOR ( 'NONE', #47097, 39.37007874015748143 ) ;
#5312 = CARTESIAN_POINT ( 'NONE',  ( 0.9500414927467377701, -0.1787899950787401604, 1.161417322780881278 ) ) ;
#5313 = CARTESIAN_POINT ( 'NONE',  ( -0.9500414927467377701, -0.1787899950787401604, 1.943897637741510254 ) ) ;
#5314 = CARTESIAN_POINT ( 'NONE',  ( 0.9873396505805591694, 0.1113553986120547346, 1.304133858160188897 ) ) ;
#5315 = ORIENTED_EDGE ( 'NONE', *, *, #19796, .F. ) ;
#5316 = CARTESIAN_POINT ( 'NONE',  ( -0.6971942568897626646, 0.07405724077823318263, 0.9104330708123776761 ) ) ;
#5317 = DIRECTION ( 'NONE',  ( -6.679788269418529283E-17, 1.000000000000000000, 0.000000000000000000 ) ) ;
#5318 = CARTESIAN_POINT ( 'NONE',  ( 0.07405724077823318263, -1.564100346181993562, -0.1787899950787401604 ) ) ;
#5319 = VERTEX_POINT ( 'NONE', #9539 ) ;
#5320 = CARTESIAN_POINT ( 'NONE',  ( -0.7646288533564489232, 0.1113553986120547346, 1.392716535325543292 ) ) ;
#5321 = CARTESIAN_POINT ( 'NONE',  ( 0.4934383202099732468, 4.616380251121755931E-17, 0.000000000000000000 ) ) ;
#5322 = CARTESIAN_POINT ( 'NONE',  ( 0.7495606340400177148, -0.1264236179284866091, 1.345964566875370139 ) ) ;
#5323 = CARTESIAN_POINT ( 'NONE',  ( 0.0005737749932554291705, 0.1277779173640709587, 0.05427780112446529276 ) ) ;
#5324 = CARTESIAN_POINT ( 'NONE',  ( 0.8759842519685039353, 0.1574803149606299191, 1.870078740157480324 ) ) ;
#5325 = CARTESIAN_POINT ( 'NONE',  ( 1.054774247047244540, 0.07405724077823318263, 1.599409448765135133 ) ) ;
#5326 = CARTESIAN_POINT ( 'NONE',  ( -0.1787899950787401604, -1.774606299158834277, 0.07405724077823318263 ) ) ;
#5327 = CARTESIAN_POINT ( 'NONE',  ( -0.1787899950787401604, -1.774606299158834277, -0.07405724077823318263 ) ) ;
#5328 = DIRECTION ( 'NONE',  ( 1.000000000000000000, 0.000000000000000000, -1.822029033848725275E-16 ) ) ;
#5329 = CARTESIAN_POINT ( 'NONE',  ( 0.7495606340400177148, -0.1264236179284866091, 0.4404527558517480901 ) ) ;
#5330 = VECTOR ( 'NONE', #16587, 39.37007874015748854 ) ;
#5331 = CARTESIAN_POINT ( 'NONE',  ( -0.6971942568897648851, -0.07405724077823297447, 0.7578740156942688211 ) ) ;
#5333 = CARTESIAN_POINT ( 'NONE',  ( -8.354793841626791791E-17, 0.03219022224904082713, -0.2854330708661417804 ) ) ;
#5332 = CARTESIAN_POINT ( 'NONE',  ( 2.892866454678787531E-17, -0.6870078740157480324, 0.1574803149606299191 ) ) ;
#5335 = CARTESIAN_POINT ( 'NONE',  ( -0.8100458409162250017, -0.1592901343197297148, 1.986959380109183826 ) ) ;
#5334 = CARTESIAN_POINT ( 'NONE',  ( 0.1797182628040039087, -1.593055620606666389, -0.07444174185955065859 ) ) ;
#5336 = DIRECTION ( 'NONE',  ( 1.822029033848725028E-16, 0.000000000000000000, 1.000000000000000000 ) ) ;
#5337 = CARTESIAN_POINT ( 'NONE',  ( 0.1264236179284866091, -0.4089566928596221063, -0.1264236179284866091 ) ) ;
#5338 = FACE_OUTER_BOUND ( 'NONE', #16104, .T. ) ;
#5339 = CARTESIAN_POINT ( 'NONE',  ( 0.9500414927467378812, -0.1787899950787401604, 1.555118110182455382 ) ) ;
#5340 = CARTESIAN_POINT ( 'NONE',  ( 0.8759842519685039353, 0.1787899950787401882, 1.803641732229700700 ) ) ;
#5341 = CARTESIAN_POINT ( 'NONE',  ( 1.054774247047244096, 0.000000000000000000, 0.4552165353793071745 ) ) ;
#5342 = DIRECTION ( 'NONE',  ( 0.000000000000000000, 0.000000000000000000, 1.000000000000000000 ) ) ;
#5343 = CARTESIAN_POINT ( 'NONE',  ( 0.03372458374097370148, 0.6131769916352027838, -0.8165595533554468322 ) ) ;
#5344 = FACE_OUTER_BOUND ( 'NONE', #37131, .T. ) ;
#5345 = CARTESIAN_POINT ( 'NONE',  ( -0.1787899950787401882, 0.1126968504474643862, 0.000000000000000000 ) ) ;
#5346 = CARTESIAN_POINT ( 'NONE',  ( 0.6971942568897626646, -0.07405724077823297447, 0.3986220471903312301 ) ) ;
#5347 = CARTESIAN_POINT ( 'NONE',  ( 0.7582988962546464151, -0.1171207568837268065, 0.03937125541389787514 ) ) ;
#5348 = EDGE_CURVE ( 'NONE', #1520, #5296, #19558, .T. ) ;
#5349 = DIRECTION ( 'NONE',  ( 0.000000000000000000, -1.000000000000000000, 0.000000000000000000 ) ) ;
#5350 = FACE_OUTER_BOUND ( 'NONE', #46134, .T. ) ;
#5351 = MANIFOLD_SOLID_BREP ( 'ISO 4162 M5x10 Hex Flange Bolt', #25620 ) ;
#5352 = CARTESIAN_POINT ( 'NONE',  ( -0.8759842519685039353, -0.1787899950787401882, 1.350885826717889815 ) ) ;
#5353 = CARTESIAN_POINT ( 'NONE',  ( 0.7185039370078739607, 1.928577636452523993E-17, 0.7677165353255432922 ) ) ;
#5354 = VERTEX_POINT ( 'NONE', #29906 ) ;
#5355 = B_SPLINE_CURVE_WITH_KNOTS ( 'NONE', 3,
 ( #14980, #7524, #6812, #32491, #21191, #22143, #28665, #36770, #21683, #35825, #11377, #18550, #29634, #10674 ),
 .UNSPECIFIED., .F., .F.,
 ( 4, 2, 2, 2, 2, 2, 4 ),
 ( 0.000000000000000000, 0.001154605602278699957, 0.001731908403418049936, 0.002309211204557399914, 0.003463816806836099438, 0.004041119607975449633, 0.004618422409114799829 ),
 .UNSPECIFIED. ) ;
#5356 = CARTESIAN_POINT ( 'NONE',  ( -0.8759842519685039353, 0.1574803149606299191, 0.7972440943806614611 ) ) ;
#5357 = CARTESIAN_POINT ( 'NONE',  ( 0.6971942568897626646, 0.07405724077823318263, 0.9891732282926934960 ) ) ;
#5360 = VERTEX_POINT ( 'NONE', #7812 ) ;
#5359 = CARTESIAN_POINT ( 'NONE',  ( 0.1787899950787401604, -1.321850393647023392, -0.07405724077823318263 ) ) ;
#5358 = CARTESIAN_POINT ( 'NONE',  ( -0.1574803149606300301, -1.083169291231055986, -0.06523048226347956391 ) ) ;
#5361 = CARTESIAN_POINT ( 'NONE',  ( -0.7185039370078739607, 1.928577636452523993E-17, 0.6102362203649134287 ) ) ;
#5362 = CARTESIAN_POINT ( 'NONE',  ( -0.7185039370078741827, 0.06523048226347841205, 0.8144685039370075375 ) ) ;
#5363 = CARTESIAN_POINT ( 'NONE',  ( 0.6971942568897648851, -0.07405724077823297447, 1.737204724355685848 ) ) ;
#5364 = CARTESIAN_POINT ( 'NONE',  ( -0.9873396505805591694, -0.1113553986120547346, 1.264763779527559029 ) ) ;
#5365 = EDGE_CURVE ( 'NONE', #40174, #12403, #17417, .T. ) ;
#5367 = CARTESIAN_POINT ( 'NONE',  ( 0.1733357866104494327, -0.5708661417322835607, 1.025733466389925352 ) ) ;
#5366 = CARTESIAN_POINT ( 'NONE',  ( -1.033464566929133799, 1.928577636452524610E-17, 2.869337061179095023E-17 ) ) ;
#5368 = CARTESIAN_POINT ( 'NONE',  ( 0.6971942568897626646, -0.07405724077823297447, 0.1279527558517483676 ) ) ;
#5369 = CARTESIAN_POINT ( 'NONE',  ( 0.9873396505805591694, -0.1113553986120547346, 1.491141732175936818 ) ) ;
#5370 = ORIENTED_EDGE ( 'NONE', *, *, #44949, .F. ) ;
#5371 = ORIENTED_EDGE ( 'NONE', *, *, #30888, .T. ) ;
#5372 = CARTESIAN_POINT ( 'NONE',  ( -0.1121660444094383646, -0.09796987684348240633, -0.2206716537553740642 ) ) ;
#5373 = CARTESIAN_POINT ( 'NONE',  ( -0.7495606340400177148, 0.1264236179284866091, 1.611712598371433103 ) ) ;
#5374 = CARTESIAN_POINT ( 'NONE',  ( 0.1574803149606300301, -0.03494094477436274909, -0.06523048226347956391 ) ) ;
#5375 = CARTESIAN_POINT ( 'NONE',  ( -1.054774247047244540, 0.07405724077823318263, 1.368110236166710125 ) ) ;
#5376 = CIRCLE ( 'NONE', #31510, 0.009842519685039387289 ) ;
#5377 = CONICAL_SURFACE ( 'NONE', #771, 0.09842519685039370636, 0.9599310885968824758 ) ;
#5378 = FACE_OUTER_BOUND ( 'NONE', #29897, .T. ) ;
#5379 = CARTESIAN_POINT ( 'NONE',  ( 1.033464566929134687, 0.06523048226347956391, 1.852854330601134469 ) ) ;
#5380 = FACE_OUTER_BOUND ( 'NONE', #46586, .T. ) ;
#5381 = CARTESIAN_POINT ( 'NONE',  ( 0.1264236179284866091, -1.212230267441836595, -0.1264236179284866091 ) ) ;
#5382 = VERTEX_POINT ( 'NONE', #33014 ) ;
#5383 = CARTESIAN_POINT ( 'NONE',  ( -0.07405724077823318263, -0.03248031490686641154, 0.1787899950787401604 ) ) ;
#5384 = ORIENTED_EDGE ( 'NONE', *, *, #13323, .T. ) ;
#5385 = ORIENTED_EDGE ( 'NONE', *, *, #12905, .T. ) ;
#5386 = CARTESIAN_POINT ( 'NONE',  ( 0.9873396505805591694, 0.1113553986120547346, 1.737204724301921299 ) ) ;
#5387 = EDGE_CURVE ( 'NONE', #44611, #5246, #22575, .T. ) ;
#5388 = DIRECTION ( 'NONE',  ( 0.000000000000000000, 1.000000000000000000, 0.000000000000000000 ) ) ;
#5389 = CARTESIAN_POINT ( 'NONE',  ( 1.033464566929133799, 0.000000000000000000, 1.781496062992125928 ) ) ;
#5390 = CARTESIAN_POINT ( 'NONE',  ( -0.1787899950787401604, -0.5935039369541101895, 0.07405724077823318263 ) ) ;
#5391 = CARTESIAN_POINT ( 'NONE',  ( -1.054774247047244096, 0.000000000000000000, 0.2632874015210397434 ) ) ;
#5392 = CARTESIAN_POINT ( 'NONE',  ( -0.7185039370078746268, -0.06523048226347956391, 0.9768700787401572994 ) ) ;
#5393 = CARTESIAN_POINT ( 'NONE',  ( 0.1270800023317771588, -1.157524124543675148, -0.1270800023317771588 ) ) ;
#5394 = CARTESIAN_POINT ( 'NONE',  ( 0.8107537697050254399, 0.1574803149606300301, 0.4158464566929134798 ) ) ;
#5395 = CARTESIAN_POINT ( 'NONE',  ( 0.6971942568897648851, 0.07405724077823318263, 1.028543307032851795 ) ) ;
#5396 = CARTESIAN_POINT ( 'NONE',  ( 0.8019270111902716547, 0.1787899950787401604, 1.451771653489543290 ) ) ;
#5397 = CARTESIAN_POINT ( 'NONE',  ( 1.033464566929134687, -0.06523048226347956391, 0.2436023622047245041 ) ) ;
#5398 = CARTESIAN_POINT ( 'NONE',  ( 0.9412147342319837628, -0.1574803149606297803, 1.498523622047243764 ) ) ;
#5400 = LINE ( 'NONE', #41329, #7843 ) ;
#5399 = CARTESIAN_POINT ( 'NONE',  ( 0.8282458751120667095, 0.1518331050034476271, 1.979292245347968660 ) ) ;
#5402 = CARTESIAN_POINT ( 'NONE',  ( 0.1638905297737256739, -0.08063388607515166451, -0.1396625121104124179 ) ) ;
#5401 = AXIS2_PLACEMENT_3D ( 'NONE', #42962, #13754, #6791 ) ;
#5403 = CARTESIAN_POINT ( 'NONE',  ( 0.4736248074375433714, 2.559880088878740079, -3.648497683167389649 ) ) ;
#5404 = CARTESIAN_POINT ( 'NONE',  ( 3.284318927891251994E-17, 0.08809055123486594918, 0.1787899950787401882 ) ) ;
#5405 = FACE_BOUND ( 'NONE', #26025, .T. ) ;
#5406 = EDGE_CURVE ( 'NONE', #22273, #22073, #3328, .T. ) ;
#5407 = CARTESIAN_POINT ( 'NONE',  ( 0.9500414927467377701, 0.1787899950787401604, 1.013779527505291878 ) ) ;
#5408 = CARTESIAN_POINT ( 'NONE',  ( 0.7495606340400177148, 0.1264236179284866091, 1.813484251914740053 ) ) ;
#5409 = CARTESIAN_POINT ( 'NONE',  ( 0.8107537697050253289, 0.1574803149606300301, 0.2878937006798746312 ) ) ;
#5410 = ORIENTED_EDGE ( 'NONE', *, *, #13323, .F. ) ;
#5411 = AXIS2_PLACEMENT_3D ( 'NONE', #1162, #1881, #41634 ) ;
#5412 = DIRECTION ( 'NONE',  ( 0.000000000000000000, 0.000000000000000000, 1.000000000000000000 ) ) ;
#5413 = CARTESIAN_POINT ( 'NONE',  ( 1.006022016660639284, 0.1011351315952034868, 0.03936735655933119166 ) ) ;
#5414 = LINE ( 'NONE', #23416, #18322 ) ;
#5415 = CARTESIAN_POINT ( 'NONE',  ( -0.06523048226347956391, -1.718011810916095783, -0.1574803149606300301 ) ) ;
#5416 = CARTESIAN_POINT ( 'NONE',  ( -0.9873396505805591694, 0.1113553986120547346, 0.2805118109160948947 ) ) ;
#5417 = CARTESIAN_POINT ( 'NONE',  ( 0.01035225325188679837, -0.1557259041956392809, 0.005865373059643922728 ) ) ;
#5418 = CARTESIAN_POINT ( 'NONE',  ( 1.054774247047244540, -0.07405724077823318263, 1.279527559001355286 ) ) ;
#5419 = EDGE_CURVE ( 'NONE', #19846, #11651, #28753, .T. ) ;
#5420 = ORIENTED_EDGE ( 'NONE', *, *, #14186, .T. ) ;
#5421 = CARTESIAN_POINT ( 'NONE',  ( 0.9412147342319837628, 0.1574803149606300301, 1.227854330601133359 ) ) ;
#5422 = CARTESIAN_POINT ( 'NONE',  ( 0.1787899950787401604, 0.1003937008411650705, -0.07405724077823318263 ) ) ;
#5423 = CARTESIAN_POINT ( 'NONE',  ( -0.2471922904502826812, 0.03219022224904098672, -0.1427165354330708902 ) ) ;
#5424 = ( BOUNDED_CURVE ( )  B_SPLINE_CURVE ( 2, ( #27176, #20180, #23322, #8688, #27418, #37938, #5089, #8932, #26931 ),
 .UNSPECIFIED., .F., .T. ) 
 B_SPLINE_CURVE_WITH_KNOTS ( ( 3, 2, 2, 2, 3 ),
 ( 0.4400000000000000022, 0.4425000000000000044, 0.4450000000000000067, 0.4475000000000000089, 0.4500000000000000111 ),
 .UNSPECIFIED. ) 
 CURVE ( )  GEOMETRIC_REPRESENTATION_ITEM ( )  RATIONAL_B_SPLINE_CURVE ( ( 1.000000000000000000, 0.9238795325112869605, 1.000000000000000000, 0.9238795325112869605, 1.000000000000000000, 0.9238795325112869605, 1.000000000000000000, 0.9238795325112869605, 1.000000000000000000 ) ) 
 REPRESENTATION_ITEM ( '' )  ) ;
#5425 = CARTESIAN_POINT ( 'NONE',  ( -1.054774247047244096, 0.000000000000000000, 0.6126968503399370380 ) ) ;
#5426 = CARTESIAN_POINT ( 'NONE',  ( 0.9412147342319837628, 0.1574803149606300301, 0.2534448818897638289 ) ) ;
#5427 = DIRECTION ( 'NONE',  ( 1.000000000000000000, -0.000000000000000000, -0.000000000000000000 ) ) ;
#5428 = VERTEX_POINT ( 'NONE', #43320 ) ;
#5430 = CARTESIAN_POINT ( 'NONE',  ( 0.1787899950787401882, -1.521161417269070837, -2.189545951927503898E-17 ) ) ;
#5429 = CARTESIAN_POINT ( 'NONE',  ( -0.06523048226347956391, -0.3794291337507407769, -0.1574803149606300301 ) ) ;
#5431 = CARTESIAN_POINT ( 'NONE',  ( -1.002407869896990045, -0.1264236179284866091, 1.006397637741511808 ) ) ;
#5432 = CARTESIAN_POINT ( 'NONE',  ( -0.6971942568897648851, 0.07405724077823318263, 1.850393700733638624 ) ) ;
#5433 = VERTEX_POINT ( 'NONE', #6898 ) ;
#5434 = CARTESIAN_POINT ( 'NONE',  ( -0.9500414927467378812, -0.1787899950787401604, 0.6102362204186774219 ) ) ;
#5435 = VERTEX_POINT ( 'NONE', #18170 ) ;
#5436 = AXIS2_PLACEMENT_3D ( 'NONE', #5596, #28136, #39118 ) ;
#5437 = CARTESIAN_POINT ( 'NONE',  ( 0.000000000000000000, 0.000000000000000000, -0.2357204724409448504 ) ) ;
#5438 = CARTESIAN_POINT ( 'NONE',  ( 0.7185039370078739607, 1.928577636452523993E-17, 1.801181102362204633 ) ) ;
#5439 = DIRECTION ( 'NONE',  ( 0.000000000000000000, 0.000000000000000000, -1.000000000000000000 ) ) ;
#5440 = CARTESIAN_POINT ( 'NONE',  ( 3.284318927891251994E-17, -0.5577027083867189816, 0.1787899950787401882 ) ) ;
#5441 = CARTESIAN_POINT ( 'NONE',  ( 0.09486442506688562426, -0.08956016536800728844, 0.1938892545125885658 ) ) ;
#5442 = DIRECTION ( 'NONE',  ( 0.000000000000000000, -0.7880107536067203489, 0.6156614753256604011 ) ) ;
#5443 = ORIENTED_EDGE ( 'NONE', *, *, #6158, .T. ) ;
#5444 = VECTOR ( 'NONE', #2498, 39.37007874015748143 ) ;
#5445 = CIRCLE ( 'NONE', #2358, 0.1673228346456689108 ) ;
#5447 = CARTESIAN_POINT ( 'NONE',  ( -1.033464566929134687, -0.06523048226347956391, 1.769192913278299084 ) ) ;
#5446 = VECTOR ( 'NONE', #41680, 39.37007874015748143 ) ;
#5448 = CARTESIAN_POINT ( 'NONE',  ( -0.6971942568897637749, 2.189545951927499583E-17, 0.5142716534895434011 ) ) ;
#5449 = CARTESIAN_POINT ( 'NONE',  ( 1.033464566929133799, 0.000000000000000000, 1.181102362097196989 ) ) ;
#5450 = ORIENTED_EDGE ( 'NONE', *, *, #32997, .T. ) ;
#5451 = DIRECTION ( 'NONE',  ( 1.000000000000000000, 0.000000000000000000, 0.000000000000000000 ) ) ;
#5452 = CARTESIAN_POINT ( 'NONE',  ( -0.6971942568897648851, 0.07405724077823318263, 1.540354330654897685 ) ) ;
#5453 = CARTESIAN_POINT ( 'NONE',  ( 0.07405724077823318263, -1.435039370024976391, -0.1787899950787401604 ) ) ;
#5454 = CARTESIAN_POINT ( 'NONE',  ( 0.4142125984251969206, 0.1870078740157480324, 2.591526198983078750E-17 ) ) ;
#5455 = ( NAMED_UNIT ( * ) PLANE_ANGLE_UNIT ( ) SI_UNIT ( $, .RADIAN. ) ) ;
#5456 = CARTESIAN_POINT ( 'NONE',  ( 0.000000000000000000, 0.000000000000000000, -0.3149606299212598381 ) ) ;
#5457 = ORIENTED_EDGE ( 'NONE', *, *, #1947, .F. ) ;
#5458 = CARTESIAN_POINT ( 'NONE',  ( 3.301370929368692659E-17, -0.6604768804491869538, 0.1797182628040039365 ) ) ;
#5459 = CARTESIAN_POINT ( 'NONE',  ( 0.8759842519685039353, 0.000000000000000000, 4.498031496062992574 ) ) ;
#5460 = CARTESIAN_POINT ( 'NONE',  ( -0.8759842519685039353, -0.1574803149606299191, 1.171259842412157637 ) ) ;
#5461 = EDGE_CURVE ( 'NONE', #5617, #3387, #32751, .T. ) ;
#5462 = CARTESIAN_POINT ( 'NONE',  ( 0.7495606340400177148, 0.1264236179284866091, 0.6323818897100157432 ) ) ;
#5464 = DIRECTION ( 'NONE',  ( 1.000000000000000000, -0.000000000000000000, -0.000000000000000000 ) ) ;
#5463 = CARTESIAN_POINT ( 'NONE',  ( 0.1574803149606300301, -0.3991141732283464694, -0.06523048226347956391 ) ) ;
#5465 = DIRECTION ( 'NONE',  ( -1.000000000000000000, -1.413024824309076326E-14, 1.884033099078770012E-14 ) ) ;
#5466 = ORIENTED_EDGE ( 'NONE', *, *, #16551, .T. ) ;
#5467 = CARTESIAN_POINT ( 'NONE',  ( -0.3161444924769509779, 1.975221432870719385, -0.9622519263226598785 ) ) ;
#5468 = CARTESIAN_POINT ( 'NONE',  ( 0.7646288533564489232, -0.1113553986120547346, 1.136811023622047223 ) ) ;
#5470 = CARTESIAN_POINT ( 'NONE',  ( -0.8904237653908255723, -0.1743634098521867348, 1.988438120113575014 ) ) ;
#5469 = DIRECTION ( 'NONE',  ( 0.000000000000000000, 0.000000000000000000, 1.000000000000000000 ) ) ;
#5471 = CARTESIAN_POINT ( 'NONE',  ( 0.8759842519685039353, 0.000000000000000000, 4.498031496062992574 ) ) ;
#5472 = VECTOR ( 'NONE', #10974, 39.37007874015748143 ) ;
#5473 = EDGE_CURVE ( 'NONE', #32643, #2780, #33026, .T. ) ;
#5475 = CARTESIAN_POINT ( 'NONE',  ( 0.1574803149606300023, 1.117014023967196401, -3.442880580079819008 ) ) ;
#5474 = CARTESIAN_POINT ( 'NONE',  ( 1.033464566929133799, 0.000000000000000000, 0.1673228346456692994 ) ) ;
#5476 = CYLINDRICAL_SURFACE ( 'NONE', #30827, 0.1574803149606299191 ) ;
#5477 = CARTESIAN_POINT ( 'NONE',  ( -0.1321454132681490201, -0.08956771084344543332, -0.1191853298852298265 ) ) ;
#5478 = CARTESIAN_POINT ( 'NONE',  ( -0.07405724077823318263, -0.5196850393163150450, -0.1787899950787401604 ) ) ;
#5479 = CIRCLE ( 'NONE', #39127, 0.3912448816427545051 ) ;
#5480 = CARTESIAN_POINT ( 'NONE',  ( 0.9873396505805591694, -0.1113553986120547346, 0.2805118110236220486 ) ) ;
#5481 = CARTESIAN_POINT ( 'NONE',  ( 0.7495606340400177148, 0.1264236179284866091, 0.7849409448281259305 ) ) ;
#5482 = ORIENTED_EDGE ( 'NONE', *, *, #39785, .F. ) ;
#5483 = CARTESIAN_POINT ( 'NONE',  ( -0.05940473271389184323, 0.07959431159476158812, -0.2511357324426385929 ) ) ;
#5484 = CARTESIAN_POINT ( 'NONE',  ( 1.033464566929134687, -0.06523048226347956391, 0.9128937007874010634 ) ) ;
#5485 = CARTESIAN_POINT ( 'NONE',  ( -0.07405724077823318263, -1.686023621993479882, 0.1787899950787401604 ) ) ;
#5486 = CARTESIAN_POINT ( 'NONE',  ( 0.1264236179284866091, -0.8567913385289133155, 0.1264236179284866091 ) ) ;
#5487 = VECTOR ( 'NONE', #17364, 39.37007874015748854 ) ;
#5488 = CARTESIAN_POINT ( 'NONE',  ( 0.1574803149606299191, -1.425196850393700920, -1.928577636452523993E-17 ) ) ;
#5489 = CARTESIAN_POINT ( 'NONE',  ( 1.033464566929133799, 0.000000000000000000, 1.259842519577511810 ) ) ;
#5490 = CARTESIAN_POINT ( 'NONE',  ( -0.9873396505805591694, 0.1113553986120547346, 1.855314960522393530 ) ) ;
#5491 = VERTEX_POINT ( 'NONE', #36851 ) ;
#5492 = EDGE_LOOP ( 'NONE', ( #18344, #31919, #40127, #24759 ) ) ;
#5493 = CARTESIAN_POINT ( 'NONE',  ( -1.054774247047244540, 0.07405724077823318263, 1.958661417269071947 ) ) ;
#5494 = CARTESIAN_POINT ( 'NONE',  ( 0.9500414927467378812, -0.1787899950787401604, 1.909448818843873186 ) ) ;
#5495 = VERTEX_POINT ( 'NONE', #4005 ) ;
#5496 = DIRECTION ( 'NONE',  ( 4.190354514309263844E-15, -0.9699617890481126992, -0.2432573283306889433 ) ) ;
#5497 = CARTESIAN_POINT ( 'NONE',  ( 0.7495606340400177148, 0.1264236179284866091, 0.4749015747493858242 ) ) ;
#5498 = CARTESIAN_POINT ( 'NONE',  ( -1.054774247047244540, -0.07405724077823318263, 1.397637795221827295 ) ) ;
#5499 = DIRECTION ( 'NONE',  ( 0.000000000000000000, 0.6156614753256605121, 0.7880107536067204599 ) ) ;
#5500 = CARTESIAN_POINT ( 'NONE',  ( -0.7495606340400177148, -0.1264236179284866091, 0.2485236219934806867 ) ) ;
#5501 = CARTESIAN_POINT ( 'NONE',  ( -1.033464566929133799, 0.000000000000000000, 0.5610236220472440971 ) ) ;
#5502 = CARTESIAN_POINT ( 'NONE',  ( -0.6971942568897648851, -0.07405724077823297447, 1.742125984198204858 ) ) ;
#5503 = CARTESIAN_POINT ( 'NONE',  ( -0.6971942568897626646, -0.07405724077823297447, 0.08858267711159097113 ) ) ;
#5504 = CARTESIAN_POINT ( 'NONE',  ( -0.1564664719456511366, 0.09340956239926197224, 0.1950971111691690296 ) ) ;
#5505 = CARTESIAN_POINT ( 'NONE',  ( -0.8759842519685039353, 0.1574803149606299191, 1.791338582677165281 ) ) ;
#5506 = LINE ( 'NONE', #41663, #28999 ) ;
#5507 = CARTESIAN_POINT ( 'NONE',  ( 0.6971942568897637749, 2.189545951927499583E-17, 1.739665354276945131 ) ) ;
#5508 = CARTESIAN_POINT ( 'NONE',  ( 0.1468252362971212699, -0.09842519685039370636, -0.1345159704478356422 ) ) ;
#5509 = DIRECTION ( 'NONE',  ( 0.5735764363510447161, -0.8191520442889925757, 1.003171929053525486E-16 ) ) ;
#5510 = LINE ( 'NONE', #34064, #13428 ) ;
#5511 = AXIS2_PLACEMENT_3D ( 'NONE', #8642, #5527, #42166 ) ;
#5512 = ORIENTED_EDGE ( 'NONE', *, *, #18930, .F. ) ;
#5513 = ORIENTED_EDGE ( 'NONE', *, *, #8435, .T. ) ;
#5514 = AXIS2_PLACEMENT_3D ( 'NONE', #32162, #43872, #39786 ) ;
#5515 = CONICAL_SURFACE ( 'NONE', #6252, 0.2559055118110236116, 1.047197551196597409 ) ;
#5516 = EDGE_CURVE ( 'NONE', #26852, #19285, #33516, .T. ) ;
#5517 = CARTESIAN_POINT ( 'NONE',  ( -0.1264236179284866091, -1.073326771599779628, -0.1264236179284866091 ) ) ;
#5518 = CARTESIAN_POINT ( 'NONE',  ( -1.094772975963752103E-17, -1.191437007820251859, -0.1787899950787401882 ) ) ;
#5519 = CARTESIAN_POINT ( 'NONE',  ( 2.892866454678787531E-17, -0.01771653543307086590, 0.1574803149606299191 ) ) ;
#5520 = CARTESIAN_POINT ( 'NONE',  ( -0.1797182628040039087, -0.5152997150948566141, -0.07444174185955065859 ) ) ;
#5521 = CARTESIAN_POINT ( 'NONE',  ( -0.1574803149606299191, -1.828740157372787278, 0.000000000000000000 ) ) ;
#5522 = EDGE_CURVE ( 'NONE', #5631, #20308, #34561, .T. ) ;
#5523 = CARTESIAN_POINT ( 'NONE',  ( -0.1574803149606300301, 0.009350393700787397108, -0.06523048226347956391 ) ) ;
#5524 = CARTESIAN_POINT ( 'NONE',  ( 0.1787899950787401882, -0.1432086613635592531, -2.189545951927503898E-17 ) ) ;
#5525 = CARTESIAN_POINT ( 'NONE',  ( 1.002407869896990045, 0.1264236179284866091, 0.9719488188438739629 ) ) ;
#5527 = DIRECTION ( 'NONE',  ( 0.000000000000000000, 0.000000000000000000, 1.000000000000000000 ) ) ;
#5526 = CARTESIAN_POINT ( 'NONE',  ( 0.7185039370078739607, 1.928577636452523993E-17, 0.6200787401574803237 ) ) ;
#5528 = CARTESIAN_POINT ( 'NONE',  ( 0.7646288533564489232, -0.1113553986120547346, 0.06397637784522892945 ) ) ;
#5529 = CONICAL_SURFACE ( 'NONE', #32314, 0.2559055118110236116, 1.047197551196597409 ) ;
#5530 = CARTESIAN_POINT ( 'NONE',  ( -0.7197834393077419124, 0.09009865225401414435, 0.03937007874015843040 ) ) ;
#5531 = CARTESIAN_POINT ( 'NONE',  ( 3.284318927891251994E-17, -0.4286417322297008115, 0.1787899950787401882 ) ) ;
#5532 = DIRECTION ( 'NONE',  ( 1.000000000000000000, 0.000000000000000000, 0.000000000000000000 ) ) ;
#5533 = CARTESIAN_POINT ( 'NONE',  ( -0.1787899950787401604, -1.454724409395055096, 0.07405724077823318263 ) ) ;
#5534 = ( BOUNDED_CURVE ( )  B_SPLINE_CURVE ( 2, ( #13560, #17383, #27971, #6598, #32021, #24817, #6829, #32269, #32508 ),
 .UNSPECIFIED., .F., .T. ) 
 B_SPLINE_CURVE_WITH_KNOTS ( ( 3, 2, 2, 2, 3 ),
 ( 0.08999999999999999667, 0.09249999999999999889, 0.09500000000000000111, 0.09750000000000000333, 0.1000000000000000056 ),
 .UNSPECIFIED. ) 
 CURVE ( )  GEOMETRIC_REPRESENTATION_ITEM ( )  RATIONAL_B_SPLINE_CURVE ( ( 1.000000000000000000, 0.9238795325112869605, 1.000000000000000000, 0.9238795325112869605, 1.000000000000000000, 0.9238795325112869605, 1.000000000000000000, 0.9238795325112869605, 1.000000000000000000 ) ) 
 REPRESENTATION_ITEM ( '' )  ) ;
#5535 = AXIS2_PLACEMENT_3D ( 'NONE', #42005, #33936, #12354 ) ;
#5536 = ADVANCED_BREP_SHAPE_REPRESENTATION ( 'Handle Arm Right', ( #4880, #20860 ), #27025 ) ;
#5537 = CARTESIAN_POINT ( 'NONE',  ( -0.6971942568897637749, 2.189545951927499583E-17, 1.892224409395055096 ) ) ;
#5538 = ORIENTED_EDGE ( 'NONE', *, *, #7094, .T. ) ;
#5539 = CARTESIAN_POINT ( 'NONE',  ( -0.9500414927467378812, 0.1787899950787401604, 1.412401574749386990 ) ) ;
#5540 = DIRECTION ( 'NONE',  ( 0.000000000000000000, 2.355041373848520102E-15, -1.000000000000000000 ) ) ;
#5541 = FACE_BOUND ( 'NONE', #38113, .T. ) ;
#5542 = CARTESIAN_POINT ( 'NONE',  ( 0.1113553986120547346, -1.223425196742866206, 0.1113553986120547346 ) ) ;
#5543 = AXIS2_PLACEMENT_3D ( 'NONE', #5321, #30771, #16372 ) ;
#5544 = AXIS2_PLACEMENT_3D ( 'NONE', #26177, #3410, #7943 ) ;
#5545 = CARTESIAN_POINT ( 'NONE',  ( -0.8759842519685039353, -0.1787899950787401882, 1.272145669237574772 ) ) ;
#5546 = CARTESIAN_POINT ( 'NONE',  ( 0.09164215658464343328, -0.09842519685974014665, -0.1535173901171399125 ) ) ;
#5547 = CARTESIAN_POINT ( 'NONE',  ( 0.000000000000000000, 0.000000000000000000, -0.0009999999999999347518 ) ) ;
#5548 = CARTESIAN_POINT ( 'NONE',  ( 0.8759842519685039353, -0.1787899950787401882, 0.5684055117572598403 ) ) ;
#5549 = CARTESIAN_POINT ( 'NONE',  ( -0.6971942568897648851, -0.07405724077823297447, 0.4773622046706456068 ) ) ;
#5550 = FACE_OUTER_BOUND ( 'NONE', #29046, .T. ) ;
#5551 = VERTEX_POINT ( 'NONE', #13241 ) ;
#5552 = PRODUCT ( 'ISO 10513 M8 Lock Nut', 'ISO 10513 M8 Lock Nut', '', ( #18543 ) ) ;
#5553 = CARTESIAN_POINT ( 'NONE',  ( -0.8759842519685039353, 0.1574803149606299191, 0.3740157480314960647 ) ) ;
#5554 = CARTESIAN_POINT ( 'NONE',  ( 1.002407869896990045, 0.1264236179284866091, 1.370570866087968520 ) ) ;
#5555 = CARTESIAN_POINT ( 'NONE',  ( 0.09663292179451181407, -0.09851384716521771612, 0.1970772057663724430 ) ) ;
#5556 = ORIENTED_EDGE ( 'NONE', *, *, #9114, .T. ) ;
#5557 = CARTESIAN_POINT ( 'NONE',  ( -0.8759842519685039353, -0.1574803149606299191, 0.6299212598425196763 ) ) ;
#5558 = CARTESIAN_POINT ( 'NONE',  ( -0.9500414927467378812, 0.1787899950787401604, 0.9793307086076531442 ) ) ;
#5559 = ( BOUNDED_CURVE ( )  B_SPLINE_CURVE ( 2, ( #22000, #18630, #33290, #40651, #4233, #18862, #26796, #45441, #20290 ),
 .UNSPECIFIED., .F., .F. ) 
 B_SPLINE_CURVE_WITH_KNOTS ( ( 3, 2, 2, 2, 3 ),
 ( 0.08500000000000000611, 0.08749999999999999445, 0.08999999999999999667, 0.09249999999999999889, 0.09500000000000000111 ),
 .UNSPECIFIED. ) 
 CURVE ( )  GEOMETRIC_REPRESENTATION_ITEM ( )  RATIONAL_B_SPLINE_CURVE ( ( 1.000000000000000000, 0.9238795325112869605, 1.000000000000000000, 0.9238795325112869605, 1.000000000000000000, 0.9238795325112869605, 1.000000000000000000, 0.9238795325112869605, 1.000000000000000000 ) ) 
 REPRESENTATION_ITEM ( '' )  ) ;
#5560 = CARTESIAN_POINT ( 'NONE',  ( -0.6971942568897626646, -0.07405724077823297447, 0.08366141726907129483 ) ) ;
#5561 = CARTESIAN_POINT ( 'NONE',  ( -0.1264236179284866091, -1.586246015473332882, 0.1264236179284866091 ) ) ;
#5562 = ORIENTED_EDGE ( 'NONE', *, *, #7886, .F. ) ;
#5563 = FACE_OUTER_BOUND ( 'NONE', #13406, .T. ) ;
#5564 = CARTESIAN_POINT ( 'NONE',  ( 3.284318927891251994E-17, -0.5418307086076535883, 0.1787899950787401882 ) ) ;
#5565 = CARTESIAN_POINT ( 'NONE',  ( -0.2644880271752204637, -0.1617936740470132251, 0.8319153819575217934 ) ) ;
#5566 = EDGE_LOOP ( 'NONE', ( #14617, #8675, #21485, #2033, #25518 ) ) ;
#5567 = ADVANCED_FACE ( 'NONE', ( #27404 ), #43992, .F. ) ;
#5568 = CARTESIAN_POINT ( 'NONE',  ( 0.003062405574123812976, 0.1386494127069827775, 0.03544276884527174792 ) ) ;
#5569 = DIRECTION ( 'NONE',  ( 0.000000000000000000, 0.000000000000000000, 1.000000000000000000 ) ) ;
#5570 = ADVANCED_FACE ( 'NONE', ( #20635, #41946 ), #39074, .F. ) ;
#5571 = CARTESIAN_POINT ( 'NONE',  ( -0.07405724077823318263, -0.8198818897100156322, 0.1787899950787401604 ) ) ;
#5572 = CIRCLE ( 'NONE', #4021, 0.1624015748031501782 ) ;
#5573 = FACE_OUTER_BOUND ( 'NONE', #18222, .T. ) ;
#5574 = ADVANCED_FACE ( 'NONE', ( #1712 ), #9399, .T. ) ;
#5575 = CONICAL_SURFACE ( 'NONE', #29350, 0.2471922904502826812, 0.5235987755982992597 ) ;
#5576 = CARTESIAN_POINT ( 'NONE',  ( 3.284318927891251994E-17, -0.04589168476467180707, 0.1787899950787401882 ) ) ;
#5577 = CARTESIAN_POINT ( 'NONE',  ( 0.07405724077823318263, 0.1397637795813224670, -0.1787899950787401604 ) ) ;
#5578 = APPLICATION_PROTOCOL_DEFINITION ( 'draft international standard', 'automotive_design', 1998, #3691 ) ;
#5579 = DIRECTION ( 'NONE',  ( -1.000000000000000000, 0.000000000000000000, 0.000000000000000000 ) ) ;
#5580 = ADVANCED_FACE ( 'NONE', ( #46270 ), #42889, .T. ) ;
#5581 = CARTESIAN_POINT ( 'NONE',  ( 0.8759842519685039353, -0.1787899950787401882, 0.4847440944344252323 ) ) ;
#5582 = CARTESIAN_POINT ( 'NONE',  ( -0.8759842519685039353, 0.1787899950787401882, 0.8636811023084409733 ) ) ;
#5584 = DIRECTION ( 'NONE',  ( -1.000000000000000000, 0.000000000000000000, 7.155734338404321376E-15 ) ) ;
#5583 = CARTESIAN_POINT ( 'NONE',  ( 0.06523048226347956391, -0.8272637795275583628, -0.1574803149606300301 ) ) ;
#5586 = CARTESIAN_POINT ( 'NONE',  ( -0.8485855016175685162, -0.1715156613748270442, 1.987705042127893895 ) ) ;
#5585 = CARTESIAN_POINT ( 'NONE',  ( -0.07444174185955065859, -1.504472943441313770, -0.1797182628040039087 ) ) ;
#5587 = AXIS2_PLACEMENT_3D ( 'NONE', #43394, #39329, #25205 ) ;
#5588 = CARTESIAN_POINT ( 'NONE',  ( 0.6971942568897637749, 2.189545951927499583E-17, 1.503444881836000002 ) ) ;
#5589 = CARTESIAN_POINT ( 'NONE',  ( 0.8019270111902716547, -0.1787899950787401604, 1.899606299158834943 ) ) ;
#5590 = CARTESIAN_POINT ( 'NONE',  ( 1.054774247047244096, 0.000000000000000000, 0.4158464566391496531 ) ) ;
#5591 = CARTESIAN_POINT ( 'NONE',  ( 0.000000000000000000, 0.000000000000000000, -0.3149606299212598381 ) ) ;
#5592 = DIRECTION ( 'NONE',  ( 1.822029033848725028E-16, 0.000000000000000000, 1.000000000000000000 ) ) ;
#5593 = CARTESIAN_POINT ( 'NONE',  ( 0.3604359965418638123, 4.466152701071653354E-17, 0.000000000000000000 ) ) ;
#5594 = CARTESIAN_POINT ( 'NONE',  ( 0.07405724077823318263, 0.006889763833291078637, 0.1787899950787401604 ) ) ;
#5595 = CARTESIAN_POINT ( 'NONE',  ( 0.6971942568897626646, 0.07405724077823318263, 0.5118110235682844511 ) ) ;
#5596 = CARTESIAN_POINT ( 'NONE',  ( 0.000000000000000000, -0.09842519685039370636, 0.000000000000000000 ) ) ;
#5598 = DIRECTION ( 'NONE',  ( 0.000000000000000000, 0.000000000000000000, -1.000000000000000000 ) ) ;
#5597 = CARTESIAN_POINT ( 'NONE',  ( 0.6971942568897637749, 2.189545951927499583E-17, 1.301673228292692830 ) ) ;
#5599 = CARTESIAN_POINT ( 'NONE',  ( 1.033464566929133799, 0.000000000000000000, 0.2066929133858267931 ) ) ;
#5600 = CARTESIAN_POINT ( 'NONE',  ( -0.8019270111902717657, 0.1787899950787401604, 1.491141732229701367 ) ) ;
#5601 = CARTESIAN_POINT ( 'NONE',  ( 1.033464566929133799, 0.000000000000000000, 0.8661417321759370402 ) ) ;
#5602 = EDGE_LOOP ( 'NONE', ( #14159, #21326, #42089, #25238, #11299 ) ) ;
#5603 = CARTESIAN_POINT ( 'NONE',  ( -0.3551574803149606385, 0.2559055118110236116, 3.133938659235350488E-17 ) ) ;
#5604 = CARTESIAN_POINT ( 'NONE',  ( 0.9500414927467378812, 0.1787899950787401604, 1.018700787347811110 ) ) ;
#5605 = ORIENTED_EDGE ( 'NONE', *, *, #3420, .F. ) ;
#5607 = CARTESIAN_POINT ( 'NONE',  ( -0.1264236179284866091, -1.378444881836000002, 0.1264236179284866091 ) ) ;
#5606 = CARTESIAN_POINT ( 'NONE',  ( 2.892866454678787531E-17, -1.110236220364913429, 0.1574803149606299191 ) ) ;
#5608 = CARTESIAN_POINT ( 'NONE',  ( -0.9873396505805591694, 0.1113553986120547346, 0.6348425195775118102 ) ) ;
#5609 = CARTESIAN_POINT ( 'NONE',  ( -1.033464566929134687, 0.06523048226347956391, 1.390255905511810441 ) ) ;
#5610 = AXIS2_PLACEMENT_3D ( 'NONE', #38827, #38354, #24687 ) ;
#5611 = CARTESIAN_POINT ( 'NONE',  ( 1.033464566929133799, 1.928577636452524610E-17, 4.498031496062992574 ) ) ;
#5613 = LINE ( 'NONE', #26736, #46853 ) ;
#5612 = FACE_OUTER_BOUND ( 'NONE', #20383, .T. ) ;
#5614 = CARTESIAN_POINT ( 'NONE',  ( 1.002407869896990045, 0.1264236179284866091, 0.1894685038832444879 ) ) ;
#5615 = CARTESIAN_POINT ( 'NONE',  ( -1.054774247047244540, -0.07405724077823318263, 0.09842519679663024046 ) ) ;
#5616 = CARTESIAN_POINT ( 'NONE',  ( 0.9412147342319837628, 0.1574803149606300301, 1.464074803042079598 ) ) ;
#5617 = VERTEX_POINT ( 'NONE', #25190 ) ;
#5618 = VERTEX_POINT ( 'NONE', #13928 ) ;
#5619 = DIRECTION ( 'NONE',  ( 0.000000000000000000, -1.000000000000000000, 0.000000000000000000 ) ) ;
#5620 = ORIENTED_EDGE ( 'NONE', *, *, #11122, .T. ) ;
#5621 = CARTESIAN_POINT ( 'NONE',  ( 1.054774247047244540, 0.07405724077823318263, 0.9350393700249758355 ) ) ;
#5622 = CARTESIAN_POINT ( 'NONE',  ( -1.054774247047244096, 0.000000000000000000, 1.675688976324189117 ) ) ;
#5623 = CARTESIAN_POINT ( 'NONE',  ( 0.1113553986120547346, -0.2391732282389295028, 0.1113553986120547346 ) ) ;
#5624 = PRODUCT_DEFINITION_FORMATION_WITH_SPECIFIED_SOURCE ( 'ANY', '', #20092, .NOT_KNOWN. ) ;
#5625 = CIRCLE ( 'NONE', #2525, 0.4724409448818896462 ) ;
#5626 = VERTEX_POINT ( 'NONE', #28572 ) ;
#5627 = DIRECTION ( 'NONE',  ( 1.000000000000000000, 0.000000000000000000, -1.822029033848725275E-16 ) ) ;
#5628 = CARTESIAN_POINT ( 'NONE',  ( -0.1264236179284866091, -1.074434991851285437, 0.1264236179284866091 ) ) ;
#5629 = ORIENTED_EDGE ( 'NONE', *, *, #28993, .F. ) ;
#5630 = CARTESIAN_POINT ( 'NONE',  ( 0.1787899950787401604, -0.1407480314422995815, 0.07405724077823318263 ) ) ;
#5631 = VERTEX_POINT ( 'NONE', #3129 ) ;
#5632 = ORIENTED_EDGE ( 'NONE', *, *, #3686, .F. ) ;
#5633 = PLANE ( 'NONE',  #8752 ) ;
#5634 = DIRECTION ( 'NONE',  ( 0.000000000000000000, 1.000000000000000000, 0.000000000000000000 ) ) ;
#5635 = ADVANCED_FACE ( 'NONE', ( #33117 ), #26431, .T. ) ;
#5636 = ADVANCED_BREP_SHAPE_REPRESENTATION ( 'Catch Plate', ( #35488, #20860 ), #39224 ) ;
#5637 = CARTESIAN_POINT ( 'NONE',  ( 1.033464566929134687, -0.06523048226347956391, 1.897145669291339320 ) ) ;
#5638 = CARTESIAN_POINT ( 'NONE',  ( -0.07405724077823318263, -0.6820866141194646959, -0.1787899950787401604 ) ) ;
#5639 = EDGE_CURVE ( 'NONE', #9079, #45828, #21590, .T. ) ;
#5640 = CARTESIAN_POINT ( 'NONE',  ( -0.7495606340400177148, 0.1264236179284866091, 0.2780511810485988278 ) ) ;
#5641 = CARTESIAN_POINT ( 'NONE',  ( -1.033464566929134687, 0.06523048226347956391, 1.075295275590550048 ) ) ;
#5642 = CARTESIAN_POINT ( 'NONE',  ( 3.301370929368692659E-17, -1.211657982811391809, 0.1797182628040039365 ) ) ;
#5643 = CARTESIAN_POINT ( 'NONE',  ( -0.2314997995717629486, 0.1618377606623054299, -0.08364281214763795436 ) ) ;
#5644 = CARTESIAN_POINT ( 'NONE',  ( 0.6971942568897648851, 0.07405724077823318263, 1.107283464513165949 ) ) ;
#5645 = CARTESIAN_POINT ( 'NONE',  ( 0.6971942568897637749, 2.189545951927499583E-17, 0.2386811023084413619 ) ) ;
#5646 = CARTESIAN_POINT ( 'NONE',  ( 1.033464566929133799, 0.000000000000000000, 0.2460629921259842590 ) ) ;
#5647 = CARTESIAN_POINT ( 'NONE',  ( 0.9873396505805591694, 0.1113553986120547346, 1.510826771653543288 ) ) ;
#5649 = CARTESIAN_POINT ( 'NONE',  ( 0.1864803149606299171, 1.086379535891623949, -0.03715491745706165500 ) ) ;
#5648 = CARTESIAN_POINT ( 'NONE',  ( 1.033464566929134687, -0.06523048226347956391, 1.424704724409449064 ) ) ;
#5650 = CARTESIAN_POINT ( 'NONE',  ( 1.033464566929134687, -0.06523048226347956391, 1.454232283357038691 ) ) ;
#5651 = CARTESIAN_POINT ( 'NONE',  ( 0.9412147342319837628, -0.1574803149606297803, 0.4650590550105836440 ) ) ;
#5652 = CARTESIAN_POINT ( 'NONE',  ( -0.9412147342319837628, -0.1574803149606297803, 1.646161417215307843 ) ) ;
#5653 = CARTESIAN_POINT ( 'NONE',  ( 1.229559056033039366E-16, 0.000000000000000000, 0.3937007874015748254 ) ) ;
#5654 = CARTESIAN_POINT ( 'NONE',  ( 0.6971942568897648851, 0.07405724077823318263, 0.9448818897100165204 ) ) ;
#5655 = CARTESIAN_POINT ( 'NONE',  ( 1.002407869896990045, 0.1264236179284866091, 1.961122047190330786 ) ) ;
#5656 = CARTESIAN_POINT ( 'NONE',  ( 0.7185039370078746268, 0.06523048226347956391, 0.3715551180027090727 ) ) ;
#5657 = ORIENTED_EDGE ( 'NONE', *, *, #23720, .T. ) ;
#5658 = AXIS2_PLACEMENT_3D ( 'NONE', #22546, #40967, #25919 ) ;
#5659 = CARTESIAN_POINT ( 'NONE',  ( 0.2362204724409448509, 0.1574803149606299191, -0.9891732283464566011 ) ) ;
#5660 = DIRECTION ( 'NONE',  ( 1.000000000000000000, 0.000000000000000000, 0.000000000000000000 ) ) ;
#5661 = CARTESIAN_POINT ( 'NONE',  ( -0.1113553986120547346, -1.676181102254677091, -0.1113553986120547346 ) ) ;
#5662 = CARTESIAN_POINT ( 'NONE',  ( -0.8107537697050253289, 0.1574803149606300301, 0.2878937006798746312 ) ) ;
#5663 = ORIENTED_EDGE ( 'NONE', *, *, #23020, .T. ) ;
#5664 = CARTESIAN_POINT ( 'NONE',  ( 0.6971942568897637749, 2.189545951927499583E-17, 1.341043307032850462 ) ) ;
#5665 = DIRECTION ( 'NONE',  ( -1.000000000000000000, 0.000000000000000000, 0.000000000000000000 ) ) ;
#5666 = DIMENSIONAL_EXPONENTS ( 1.000000000000000000, 0.000000000000000000, 0.000000000000000000, 0.000000000000000000, 0.000000000000000000, 0.000000000000000000, 0.000000000000000000 ) ;
#5667 = CARTESIAN_POINT ( 'NONE',  ( -0.1787899950787401882, 0.1176181102899840625, 0.000000000000000000 ) ) ;
#5668 = CARTESIAN_POINT ( 'NONE',  ( -0.7185039370078714072, 0.06523048226347728795, 1.877460629921259727 ) ) ;
#5669 = CARTESIAN_POINT ( 'NONE',  ( -1.002407869896990045, -0.1264236179284866091, 0.6471456692375747721 ) ) ;
#5670 = CARTESIAN_POINT ( 'NONE',  ( 0.8107537697050254399, -0.1574803149606297803, 1.365649606191686294 ) ) ;
#5671 = CARTESIAN_POINT ( 'NONE',  ( -0.06218625040858933445, 0.08128102204192425018, 0.2495298224528491315 ) ) ;
#5672 = ORIENTED_EDGE ( 'NONE', *, *, #26289, .F. ) ;
#5673 = ORIENTED_EDGE ( 'NONE', *, *, #42018, .F. ) ;
#5674 = CARTESIAN_POINT ( 'NONE',  ( 0.1787899950787401882, -1.678641732229700922, -2.189545951927503898E-17 ) ) ;
#5675 = CARTESIAN_POINT ( 'NONE',  ( -0.7495606340400177148, -0.1264236179284866091, 1.035925196796629866 ) ) ;
#5676 = CARTESIAN_POINT ( 'NONE',  ( -0.9873396505805591694, -0.1113553986120547346, 0.04429133858267716300 ) ) ;
#5677 = ORIENTED_EDGE ( 'NONE', *, *, #17755, .F. ) ;
#5678 = CARTESIAN_POINT ( 'NONE',  ( -1.002407869896990045, -0.1264236179284866091, 0.7308070865604093802 ) ) ;
#5679 = ORIENTED_EDGE ( 'NONE', *, *, #41245, .F. ) ;
#5680 = DIRECTION ( 'NONE',  ( 0.000000000000000000, -1.000000000000000000, 0.000000000000000000 ) ) ;
#5681 = CARTESIAN_POINT ( 'NONE',  ( 0.001488395362858443375, 0.02696616380223046047, -0.1377975526281502716 ) ) ;
#5682 = CARTESIAN_POINT ( 'NONE',  ( -0.1264236179284866091, -0.6413641257095532566, 0.1264236179284866091 ) ) ;
#5683 = VERTEX_POINT ( 'NONE', #32877 ) ;
#5684 = CARTESIAN_POINT ( 'NONE',  ( -1.033464566929133799, 0.000000000000000000, 0.6692913384751496553 ) ) ;
#5685 = VERTEX_POINT ( 'NONE', #3382 ) ;
#5686 = LINE ( 'NONE', #8802, #12657 ) ;
#5687 = CARTESIAN_POINT ( 'NONE',  ( 0.2519685039370078705, 4.616380251121755931E-17, 0.000000000000000000 ) ) ;
#5688 = CARTESIAN_POINT ( 'NONE',  ( -0.9500414927467378812, 0.1787899950787401604, 0.5413385826234012876 ) ) ;
#5689 = DIRECTION ( 'NONE',  ( 0.000000000000000000, -1.000000000000000000, 0.000000000000000000 ) ) ;
#5690 = ADVANCED_FACE ( 'NONE', ( #32644 ), #14414, .F. ) ;
#5691 = ORIENTED_EDGE ( 'NONE', *, *, #41188, .F. ) ;
#5692 = CARTESIAN_POINT ( 'NONE',  ( 0.000000000000000000, 0.09842519685039370636, 0.000000000000000000 ) ) ;
#5693 = CARTESIAN_POINT ( 'NONE',  ( -1.054774247047244540, 0.07405724077823318263, 1.604330708607653921 ) ) ;
#5694 = EDGE_CURVE ( 'NONE', #16593, #38424, #33353, .T. ) ;
#5695 = CARTESIAN_POINT ( 'NONE',  ( 0.1787899950787401604, -1.518700787347811554, -0.07405724077823318263 ) ) ;
#5696 = LINE ( 'NONE', #31822, #34890 ) ;
#5697 = CARTESIAN_POINT ( 'NONE',  ( -1.033464566929134687, -0.06523048226347956391, 0.1943897636720005040 ) ) ;
#5698 = CARTESIAN_POINT ( 'NONE',  ( 0.07444174185955065859, -0.7367564080082430467, 0.1797182628040039087 ) ) ;
#5699 = LINE ( 'NONE', #26588, #30955 ) ;
#5700 = CARTESIAN_POINT ( 'NONE',  ( -0.8107537697050253289, 0.1574803149606300301, 1.311515747923968744 ) ) ;
#5702 = CARTESIAN_POINT ( 'NONE',  ( 0.2362204724409448509, 0.000000000000000000, -0.9891732283464566011 ) ) ;
#5701 = CARTESIAN_POINT ( 'NONE',  ( 0.06523048226347956391, -0.4335629921259839814, -0.1574803149606300301 ) ) ;
#5703 = LINE ( 'NONE', #1624, #27682 ) ;
#5704 = VECTOR ( 'NONE', #32125, 39.37007874015748143 ) ;
#5705 = CARTESIAN_POINT ( 'NONE',  ( 0.8759842519685039353, 0.1574803149606299191, 1.043307086614173151 ) ) ;
#5706 = CARTESIAN_POINT ( 'NONE',  ( -0.9720330238214066609, -0.1495884858916018134, 1.989995714837735408 ) ) ;
#5707 = CARTESIAN_POINT ( 'NONE',  ( 0.1639941039450801552, -0.08071844585390765270, -0.1398101989048133320 ) ) ;
#5708 = PLANE ( 'NONE',  #6732 ) ;
#5710 = DIRECTION ( 'NONE',  ( 0.5735764363510332808, -0.6455006197386625733, 0.5043203561029951931 ) ) ;
#5709 = DIRECTION ( 'NONE',  ( -0.8191520442889991260, 0.000000000000000000, -0.5735764363510356123 ) ) ;
#5711 = CARTESIAN_POINT ( 'NONE',  ( 0.7185039370078739607, 1.928577636452523993E-17, 1.279527558947590515 ) ) ;
#5712 = CARTESIAN_POINT ( 'NONE',  ( -0.1619057349516830613, -0.08956057142125727066, -0.06208618848698507081 ) ) ;
#5714 = VECTOR ( 'NONE', #13761, 39.37007874015748854 ) ;
#5713 = CARTESIAN_POINT ( 'NONE',  ( 0.1264236179284866091, -0.6156496062454488438, 0.1264236179284866091 ) ) ;
#5715 = FACE_OUTER_BOUND ( 'NONE', #34114, .T. ) ;
#5716 = VERTEX_POINT ( 'NONE', #40952 ) ;
#5717 = AXIS2_PLACEMENT_3D ( 'NONE', #14443, #6526, #25482 ) ;
#5718 = AXIS2_PLACEMENT_3D ( 'NONE', #7993, #41262, #8948 ) ;
#5719 = CARTESIAN_POINT ( 'NONE',  ( 1.002407869896990045, -0.1264236179284866091, 0.7652559054580472253 ) ) ;
#5720 = DIRECTION ( 'NONE',  ( -1.000000000000000000, 0.000000000000000000, 0.000000000000000000 ) ) ;
#5721 = CARTESIAN_POINT ( 'NONE',  ( 0.8759842519685039353, 0.000000000000000000, 4.498031496062992574 ) ) ;
#5722 = CARTESIAN_POINT ( 'NONE',  ( -0.1787899950787401604, -1.651574803095843258, 0.07405724077823318263 ) ) ;
#5723 = CARTESIAN_POINT ( 'NONE',  ( 3.284318927891251994E-17, -0.9798228345919054449, 0.1787899950787401882 ) ) ;
#5724 = CARTESIAN_POINT ( 'NONE',  ( -0.1574803149606297803, -1.403051181102363154, 0.06523048226347956391 ) ) ;
#5725 = CARTESIAN_POINT ( 'NONE',  ( 0.9412147342319837628, -0.1574803149606297803, 1.213090551073576107 ) ) ;
#5726 = CARTESIAN_POINT ( 'NONE',  ( 0.8759842519685039353, -0.1574803149606299191, 1.171259842412157637 ) ) ;
#5727 = UNCERTAINTY_MEASURE_WITH_UNIT (LENGTH_MEASURE( 1.000000000000000082E-05 ), #6167, 'distance_accuracy_value', 'NONE') ;
#5728 = VERTEX_POINT ( 'NONE', #23259 ) ;
#5729 = CARTESIAN_POINT ( 'NONE',  ( -0.9500414927467378812, 0.1787899950787401604, 1.924212598371433325 ) ) ;
#5730 = CARTESIAN_POINT ( 'NONE',  ( 1.054774247047244540, 0.07405724077823318263, 1.801181102308441861 ) ) ;
#5731 = ORIENTED_EDGE ( 'NONE', *, *, #10353, .F. ) ;
#5732 = CARTESIAN_POINT ( 'NONE',  ( -0.1574803149606297803, -1.353838582569638849, 0.06523048226347956391 ) ) ;
#5733 = CARTESIAN_POINT ( 'NONE',  ( 0.9873396505805591694, -0.1113553986120547346, 1.776574803149606252 ) ) ;
#5734 = CARTESIAN_POINT ( 'NONE',  ( -0.8019270111902717657, 0.1787899950787401604, 1.530511810969859443 ) ) ;
#5735 = CARTESIAN_POINT ( 'NONE',  ( 0.09272654090495630053, 0.2419614285902424167, -0.3131151337379057265 ) ) ;
#5736 = CARTESIAN_POINT ( 'NONE',  ( -0.8759842519685039353, -0.1787899950787401882, 0.9571850393163149340 ) ) ;
#5737 = CARTESIAN_POINT ( 'NONE',  ( -0.9500414927467378812, -0.1787899950787401604, 0.2559055117572600624 ) ) ;
#5738 = DIRECTION ( 'NONE',  ( 1.822029033848725028E-16, 0.000000000000000000, 1.000000000000000000 ) ) ;
#5739 = CARTESIAN_POINT ( 'NONE',  ( -0.7495606340400177148, -0.1264236179284866091, 1.665846456639149764 ) ) ;
#5740 = CARTESIAN_POINT ( 'NONE',  ( -1.054774247047244540, -0.07405724077823318263, 0.1427165353793072855 ) ) ;
#5741 = LINE ( 'NONE', #17000, #42505 ) ;
#5742 = CARTESIAN_POINT ( 'NONE',  ( -0.9412147342319837628, -0.1574803149606297803, 1.813484251968503935 ) ) ;
#5743 = DIRECTION ( 'NONE',  ( 8.659560562358463011E-17, 0.7071067811862592478, -0.7071067811868357866 ) ) ;
#5744 = EDGE_CURVE ( 'NONE', #31115, #24872, #37874, .T. ) ;
#5745 = CARTESIAN_POINT ( 'NONE',  ( 0.7495606340400177148, 0.1264236179284866091, 1.734744094434425232 ) ) ;
#5746 = CARTESIAN_POINT ( 'NONE',  ( -0.009585880836737756955, -0.09842519685039370636, -0.1896059596911200962 ) ) ;
#5747 = CARTESIAN_POINT ( 'NONE',  ( 0.2066929133858268486, 0.06245656531175283743, -0.1492449156640649477 ) ) ;
#5748 = ADVANCED_FACE ( 'NONE', ( #11772 ), #37375, .T. ) ;
#5749 = AXIS2_PLACEMENT_3D ( 'NONE', #17965, #22262, #36661 ) ;
#5750 = EDGE_CURVE ( 'NONE', #5132, #42574, #30242, .T. ) ;
#5751 = ORIENTED_EDGE ( 'NONE', *, *, #777, .F. ) ;
#5752 = AXIS2_PLACEMENT_3D ( 'NONE', #39780, #21596, #36232 ) ;
#5753 = ORIENTED_EDGE ( 'NONE', *, *, #23116, .T. ) ;
#5754 = AXIS2_PLACEMENT_3D ( 'NONE', #2192, #3853, #35977 ) ;
#5755 = AXIS2_PLACEMENT_3D ( 'NONE', #8382, #41424, #22289 ) ;
#5756 = ADVANCED_FACE ( 'NONE', ( #12240 ), #12007, .T. ) ;
#5757 = CARTESIAN_POINT ( 'NONE',  ( 0.07405724077823318263, -1.095472440891117838, 0.1787899950787401604 ) ) ;
#5758 = CARTESIAN_POINT ( 'NONE',  ( 0.1787899950787401604, -1.277559055064345861, -0.07405724077823318263 ) ) ;
#5759 = EDGE_CURVE ( 'NONE', #34930, #2118, #40913, .T. ) ;
#5760 = CYLINDRICAL_SURFACE ( 'NONE', #27135, 0.009842519685039387289 ) ;
#5761 = ( LENGTH_UNIT ( ) NAMED_UNIT ( * ) SI_UNIT ( $, .METRE. ) ) ;
#5762 = CARTESIAN_POINT ( 'NONE',  ( 1.054774247047244096, 0.000000000000000000, 0.4158464566391496531 ) ) ;
#5763 = CARTESIAN_POINT ( 'NONE',  ( 0.1797182628040039087, -0.4956146757247781309, 0.07444174185955046430 ) ) ;
#5764 = CARTESIAN_POINT ( 'NONE',  ( -0.8759842519685039353, -0.1574803149606299191, 0.8169291337507401662 ) ) ;
#5765 = CARTESIAN_POINT ( 'NONE',  ( -1.033464566929134687, -0.06523048226347956391, 0.6766732283464570452 ) ) ;
#5766 = CARTESIAN_POINT ( 'NONE',  ( -0.06523048226347956391, -0.03494094488188976416, -0.1574803149606300301 ) ) ;
#5767 = CARTESIAN_POINT ( 'NONE',  ( 1.002407869896990045, 0.1264236179284866091, 0.8538385826234016207 ) ) ;
#5769 = CARTESIAN_POINT ( 'NONE',  ( 0.006378642920439305843, 0.09116121678403278639, 0.1176987636582383229 ) ) ;
#5768 = CARTESIAN_POINT ( 'NONE',  ( 0.1976644210311565564, 0.1813726255708565105, -0.05388431474955820977 ) ) ;
#5770 = CARTESIAN_POINT ( 'NONE',  ( 0.7185039370078739607, 1.928577636452523993E-17, 0.05905511800270921846 ) ) ;
#5771 = AXIS2_PLACEMENT_3D ( 'NONE', #451, #3819, #11268 ) ;
#5772 = DIRECTION ( 'NONE',  ( 1.822029033848725028E-16, 0.000000000000000000, 1.000000000000000000 ) ) ;
#5773 = CARTESIAN_POINT ( 'NONE',  ( -0.07405724077823318263, -0.6033464566391496531, -0.1787899950787401604 ) ) ;
#5774 = CARTESIAN_POINT ( 'NONE',  ( 0.1787899950787401882, -1.398129921206078707, -2.189545951927503898E-17 ) ) ;
#5775 = CYLINDRICAL_SURFACE ( 'NONE', #7049, 0.1574803149606299191 ) ;
#5776 = CARTESIAN_POINT ( 'NONE',  ( -0.8019270111902717657, 0.1787899950787401604, 1.884842519631275026 ) ) ;
#5777 = ORIENTED_EDGE ( 'NONE', *, *, #29916, .F. ) ;
#5778 = AXIS2_PLACEMENT_3D ( 'NONE', #11006, #25624, #40199 ) ;
#5779 = CARTESIAN_POINT ( 'NONE',  ( -0.9500414927467378812, 0.1787899950787401604, 1.530511810969859443 ) ) ;
#5780 = CARTESIAN_POINT ( 'NONE',  ( 0.8759842519685039353, 0.1787899950787401882, 1.375492125930488196 ) ) ;
#5781 = CIRCLE ( 'NONE', #7335, 0.3100393700787401619 ) ;
#5783 = DIRECTION ( 'NONE',  ( 0.000000000000000000, 0.7071067811865965336, 0.7071067811864983899 ) ) ;
#5782 = VECTOR ( 'NONE', #44968, 39.37007874015748143 ) ;
#5784 = CARTESIAN_POINT ( 'NONE',  ( -0.6971942568897637749, 2.189545951927499583E-17, 0.6766732282926929409 ) ) ;
#5785 = CARTESIAN_POINT ( 'NONE',  ( 1.002407869896990045, 0.1264236179284866091, 0.1107283464029293202 ) ) ;
#5786 = CARTESIAN_POINT ( 'NONE',  ( -0.9500414927467378812, 0.1787899950787401604, 1.289370078686393750 ) ) ;
#5787 = EDGE_CURVE ( 'NONE', #426, #38785, #20126, .T. ) ;
#5788 = CARTESIAN_POINT ( 'NONE',  ( 0.1003010584927840482, -0.09843450717735198474, -0.1483099721156116158 ) ) ;
#5789 = CARTESIAN_POINT ( 'NONE',  ( 0.9500414927467377701, 0.1787899950787401604, 0.6643700786863929730 ) ) ;
#5790 = CARTESIAN_POINT ( 'NONE',  ( -0.7495606340400177148, 0.1264236179284866091, 0.5880905511273386566 ) ) ;
#5791 = CARTESIAN_POINT ( 'NONE',  ( 0.2137641352132148842, -0.06208088008958128484, 0.1620118252827001948 ) ) ;
#5792 = CARTESIAN_POINT ( 'NONE',  ( 0.1574803149606299746, 0.3740157480314960647, 1.057384721142220263 ) ) ;
#5793 = ORIENTED_EDGE ( 'NONE', *, *, #16423, .F. ) ;
#5794 = CARTESIAN_POINT ( 'NONE',  ( -1.033464566929134687, 0.06523048226347956391, 0.3272637795275589734 ) ) ;
#5795 = EDGE_CURVE ( 'NONE', #22721, #4172, #5741, .T. ) ;
#5796 = CARTESIAN_POINT ( 'NONE',  ( 1.054774247047244540, -0.07405724077823318263, 1.323818897584032594 ) ) ;
#5797 = CARTESIAN_POINT ( 'NONE',  ( 0.1225873787495714712, -0.09851384768301142680, 0.1799582249796369826 ) ) ;
#5798 = CARTESIAN_POINT ( 'NONE',  ( -0.9873396505805591694, -0.1113553986120547346, 1.845472440837354178 ) ) ;
#5799 = ORIENTED_EDGE ( 'NONE', *, *, #16805, .F. ) ;
#5800 = DIRECTION ( 'NONE',  ( 0.000000000000000000, 0.000000000000000000, -1.000000000000000000 ) ) ;
#5801 = CARTESIAN_POINT ( 'NONE',  ( -0.8759842519685039353, 0.1787899950787401882, 1.021161417269070837 ) ) ;
#5802 = CARTESIAN_POINT ( 'NONE',  ( -0.07405724077823318263, -1.623155464292230565, 0.1787899950787401604 ) ) ;
#5803 = ORIENTED_EDGE ( 'NONE', *, *, #30598, .T. ) ;
#5804 = LINE ( 'NONE', #2198, #15871 ) ;
#5805 = CARTESIAN_POINT ( 'NONE',  ( 0.1264236179284866091, -0.5762795275052914334, 0.1264236179284866091 ) ) ;
#5806 = LINE ( 'NONE', #35751, #39943 ) ;
#5807 = ORIENTED_EDGE ( 'NONE', *, *, #22370, .F. ) ;
#5808 = CIRCLE ( 'NONE', #22648, 0.1787899950787401049 ) ;
#5809 = CARTESIAN_POINT ( 'NONE',  ( -0.06863485658886912810, 0.2558675481231191817, -0.3097625555228274985 ) ) ;
#5810 = LINE ( 'NONE', #19942, #38422 ) ;
#5811 = CARTESIAN_POINT ( 'NONE',  ( -0.07405724077823318263, -0.2883858267178899260, -0.1787899950787401604 ) ) ;
#5812 = CARTESIAN_POINT ( 'NONE',  ( 0.1264236179284866091, -0.7337598424659212970, 0.1264236179284866091 ) ) ;
#5813 = CARTESIAN_POINT ( 'NONE',  ( 0.8759842519685039353, 0.000000000000000000, 4.498031496062992574 ) ) ;
#5814 = CARTESIAN_POINT ( 'NONE',  ( 0.5555748031496103856, 0.7681739484881628943, -0.04983111751016747887 ) ) ;
#5815 = CARTESIAN_POINT ( 'NONE',  ( 0.8759842519685039353, 0.1787899950787401882, 1.567421259788755794 ) ) ;
#5816 = CIRCLE ( 'NONE', #35657, 0.6872114956789353579 ) ;
#5817 = CARTESIAN_POINT ( 'NONE',  ( -0.1264236179284866091, 0.06729729161328090736, 0.1264236179284866091 ) ) ;
#5818 = CARTESIAN_POINT ( 'NONE',  ( -0.07405724077823318263, 0.1053149606836847191, -0.1787899950787401604 ) ) ;
#5819 = CARTESIAN_POINT ( 'NONE',  ( 0.2559055118110235560, -0.02431590950899893341, -0.3149606299212598381 ) ) ;
#5820 = CARTESIAN_POINT ( 'NONE',  ( 0.8019270111902717657, -0.1787899950787401604, 0.4822834645131655606 ) ) ;
#5821 = ( BOUNDED_CURVE ( )  B_SPLINE_CURVE ( 2, ( #15236, #43731, #10934, #29880, #36794, #29181, #40823, #14515, #39892 ),
 .UNSPECIFIED., .F., .T. ) 
 B_SPLINE_CURVE_WITH_KNOTS ( ( 3, 2, 2, 2, 3 ),
 ( 0.6899999999999999467, 0.6925000000000000044, 0.6949999999999999512, 0.6975000000000000089, 0.6999999999999999556 ),
 .UNSPECIFIED. ) 
 CURVE ( )  GEOMETRIC_REPRESENTATION_ITEM ( )  RATIONAL_B_SPLINE_CURVE ( ( 1.000000000000000000, 0.9238795325112899581, 1.000000000000000000, 0.9238795325112869605, 1.000000000000000000, 0.9238795325112869605, 1.000000000000000000, 0.9238795325112829637, 1.000000000000000000 ) ) 
 REPRESENTATION_ITEM ( '' )  ) ;
#5822 = CARTESIAN_POINT ( 'NONE',  ( -0.8759842519685039353, 0.1787899950787401882, 0.7849409448281259305 ) ) ;
#5824 = DIRECTION ( 'NONE',  ( 1.000000000000000000, 0.000000000000000000, 0.000000000000000000 ) ) ;
#5823 = CARTESIAN_POINT ( 'NONE',  ( -0.1113553986120547346, -0.8986220472440945573, -0.1113553986120547346 ) ) ;
#5826 = CARTESIAN_POINT ( 'NONE',  ( -0.7369741704597091436, -0.09768268266897506269, 1.985206247291391390 ) ) ;
#5825 = CARTESIAN_POINT ( 'NONE',  ( -0.1270800023317771588, -1.570909951315328623, 0.1270800023317771588 ) ) ;
#5827 = CARTESIAN_POINT ( 'NONE',  ( 0.07405724077823318263, -0.3818897637257640532, 0.1787899950787401604 ) ) ;
#5828 = CARTESIAN_POINT ( 'NONE',  ( -0.7185039370078746268, 0.06523048226347956391, 1.040846456585385882 ) ) ;
#5829 = CARTESIAN_POINT ( 'NONE',  ( 0.7495606340400177148, 0.1264236179284866091, 1.577263779473795369 ) ) ;
#5830 = LINE ( 'NONE', #20437, #14580 ) ;
#5831 = CARTESIAN_POINT ( 'NONE',  ( 0.9500414927467377701, -0.1787899950787401604, 0.3690944881352128393 ) ) ;
#5832 = DIRECTION ( 'NONE',  ( 3.469446951953626022E-15, 1.000000000000000000, 0.000000000000000000 ) ) ;
#5833 = CARTESIAN_POINT ( 'NONE',  ( 0.9412147342319837628, -0.1574803149606297803, 0.8587598424121577478 ) ) ;
#5834 = CARTESIAN_POINT ( 'NONE',  ( 0.1818270763438056270, -0.1905157801853442356, -0.3106979152243058984 ) ) ;
#5835 = CARTESIAN_POINT ( 'NONE',  ( 0.1264236179284866091, 0.04872047249470835839, 0.1264236179284866091 ) ) ;
#5836 = CARTESIAN_POINT ( 'NONE',  ( 0.07405724077823318263, -0.05216535427694517224, -0.1787899950787401604 ) ) ;
#5837 = CARTESIAN_POINT ( 'NONE',  ( 0.6971942568897626646, -0.07405724077823297447, 0.4379921259304882519 ) ) ;
#5838 = CARTESIAN_POINT ( 'NONE',  ( 0.07405724077823318263, -0.9330708660879686311, 0.1787899950787401604 ) ) ;
#5839 = CARTESIAN_POINT ( 'NONE',  ( 0.7185039370078739607, 1.928577636452523993E-17, 0.06889763779527559306 ) ) ;
#5840 = DIRECTION ( 'NONE',  ( -1.000000000000000000, 0.000000000000000000, 0.000000000000000000 ) ) ;
#5841 = CARTESIAN_POINT ( 'NONE',  ( -0.7495606340400177148, -0.1264236179284866091, 1.424704724355685181 ) ) ;
#5842 = CARTESIAN_POINT ( 'NONE',  ( 0.7646288533564489232, -0.1113553986120547346, 0.8120078739082204899 ) ) ;
#5843 = ORIENTED_EDGE ( 'NONE', *, *, #21607, .T. ) ;
#5844 = CARTESIAN_POINT ( 'NONE',  ( -0.9873396505805591694, 0.1113553986120547346, 0.7923228345381417848 ) ) ;
#5845 = CARTESIAN_POINT ( 'NONE',  ( 0.6971942568897637749, 2.189545951927499583E-17, 0.9916338582139527791 ) ) ;
#5846 = EDGE_LOOP ( 'NONE', ( #25452, #3729, #12691, #15112 ) ) ;
#5847 = CARTESIAN_POINT ( 'NONE',  ( -1.094772975963752103E-17, -1.353838582623401621, -0.1787899950787401882 ) ) ;
#5848 = CARTESIAN_POINT ( 'NONE',  ( -0.8107537697050253289, -0.1574803149606297803, 0.5388779526483779003 ) ) ;
#5849 = DIRECTION ( 'NONE',  ( -1.000000000000000000, 0.000000000000000000, 0.000000000000000000 ) ) ;
#5850 = CARTESIAN_POINT ( 'NONE',  ( 0.8759842519685039353, -0.1787899950787401882, 1.705216535379307174 ) ) ;
#5851 = CARTESIAN_POINT ( 'NONE',  ( -0.7185039370078739607, 1.928577636452523993E-17, 1.446850393700787274 ) ) ;
#5852 = EDGE_CURVE ( 'NONE', #2820, #799, #35748, .T. ) ;
#5853 = CYLINDRICAL_SURFACE ( 'NONE', #22042, 0.09842519685039370636 ) ;
#5855 = DIRECTION ( 'NONE',  ( 0.000000000000000000, 0.000000000000000000, -1.000000000000000000 ) ) ;
#5854 = CARTESIAN_POINT ( 'NONE',  ( 0.1469224761503790389, 0.2106668292956904442, -0.3144321013757216399 ) ) ;
#5856 = CARTESIAN_POINT ( 'NONE',  ( 0.6971942568897637749, 2.189545951927499583E-17, 0.08612204719033110523 ) ) ;
#5857 = CARTESIAN_POINT ( 'NONE',  ( -1.002407869896990045, -0.1264236179284866091, 0.1353346456155277433 ) ) ;
#5858 = CARTESIAN_POINT ( 'NONE',  ( 0.8107537697050253289, 0.1574803149606300301, 1.350885826664126821 ) ) ;
#5859 = VERTEX_POINT ( 'NONE', #28048 ) ;
#5860 = ORIENTED_EDGE ( 'NONE', *, *, #13221, .F. ) ;
#5861 = ( BOUNDED_CURVE ( )  B_SPLINE_CURVE ( 2, ( #10445, #37012, #29413, #28675, #36324, #4166, #7310, #25042, #6820 ),
 .UNSPECIFIED., .F., .T. ) 
 B_SPLINE_CURVE_WITH_KNOTS ( ( 3, 2, 2, 2, 3 ),
 ( 0.9499999999999999556, 0.9525000000000000133, 0.9549999999999999600, 0.9575000000000000178, 0.9599999999999999645 ),
 .UNSPECIFIED. ) 
 CURVE ( )  GEOMETRIC_REPRESENTATION_ITEM ( )  RATIONAL_B_SPLINE_CURVE ( ( 1.000000000000000000, 0.9238795325112939549, 1.000000000000000000, 0.9238795325112869605, 1.000000000000000000, 0.9238795325112869605, 1.000000000000000000, 0.9238795325112869605, 1.000000000000000000 ) ) 
 REPRESENTATION_ITEM ( '' )  ) ;
#5862 = EDGE_CURVE ( 'NONE', #18361, #8850, #42608, .T. ) ;
#5863 = DIRECTION ( 'NONE',  ( 1.000000000000000000, 0.000000000000000000, -1.822029033848725275E-16 ) ) ;
#5864 = VERTEX_POINT ( 'NONE', #2139 ) ;
#5865 = EDGE_CURVE ( 'NONE', #31109, #5618, #25496, .T. ) ;
#5866 = CARTESIAN_POINT ( 'NONE',  ( -0.8019270111902716547, 0.1787899950787401604, 1.766732283410803239 ) ) ;
#5867 = EDGE_CURVE ( 'NONE', #3082, #38318, #2069, .T. ) ;
#5868 = VERTEX_POINT ( 'NONE', #6434 ) ;
#5869 = CARTESIAN_POINT ( 'NONE',  ( -0.2471922904502826257, 0.07945684066377885213, -0.07439773916327591108 ) ) ;
#5870 = DIRECTION ( 'NONE',  ( 0.000000000000000000, 0.000000000000000000, -1.000000000000000000 ) ) ;
#5871 = CARTESIAN_POINT ( 'NONE',  ( 0.1787899950787401882, -1.138411369804041451, -2.189545951927503898E-17 ) ) ;
#5872 = VERTEX_POINT ( 'NONE', #28514 ) ;
#5873 = CARTESIAN_POINT ( 'NONE',  ( 0.1787899950787401604, -0.1801181101824570474, 0.07405724077823318263 ) ) ;
#5874 = VERTEX_POINT ( 'NONE', #10290 ) ;
#5875 = VERTEX_POINT ( 'NONE', #32347 ) ;
#5876 = CARTESIAN_POINT ( 'NONE',  ( -0.2559053909010672312, -0.07743436953536136924, -0.3083471293668692548 ) ) ;
#5877 = DIRECTION ( 'NONE',  ( -0.000000000000000000, -0.000000000000000000, -1.000000000000000000 ) ) ;
#5878 = CARTESIAN_POINT ( 'NONE',  ( 0.8107537697050253289, -0.1574803149606297803, 1.808562992125984703 ) ) ;
#5879 = CARTESIAN_POINT ( 'NONE',  ( 0.1264236179284866091, -0.6205708660879685201, 0.1264236179284866091 ) ) ;
#5880 = EDGE_CURVE ( 'NONE', #46851, #33302, #14964, .T. ) ;
#5881 = CARTESIAN_POINT ( 'NONE',  ( -1.002407869896990045, -0.1264236179284866091, 0.3371062991588349989 ) ) ;
#5882 = CARTESIAN_POINT ( 'NONE',  ( -0.8759842519685039353, -0.1574803149606299191, 1.102362204724409489 ) ) ;
#5883 = CARTESIAN_POINT ( 'NONE',  ( -0.07444174185955065859, -1.150142234779895745, -0.1797182628040039087 ) ) ;
#5884 = CARTESIAN_POINT ( 'NONE',  ( -0.1934636958948592889, 0.1837979153590902914, -0.05069326177273324185 ) ) ;
#5885 = CARTESIAN_POINT ( 'NONE',  ( 1.002407869896990045, 0.1264236179284866091, 1.055610236166708793 ) ) ;
#5886 = CARTESIAN_POINT ( 'NONE',  ( 0.6971942568897648851, 0.07405724077823318263, 1.456692913332062522 ) ) ;
#5887 = CARTESIAN_POINT ( 'NONE',  ( 0.7185039370078746268, -0.06523048226347956391, 0.2288385826771655862 ) ) ;
#5888 = CARTESIAN_POINT ( 'NONE',  ( 0.9873396505805591694, -0.1113553986120547346, 1.697834645669291209 ) ) ;
#5890 = DIRECTION ( 'NONE',  ( 0.000000000000000000, 1.000000000000000000, 0.000000000000000000 ) ) ;
#5889 = CARTESIAN_POINT ( 'NONE',  ( -0.6195511811023656223, 0.9842519685039370358, -0.7135826771653542844 ) ) ;
#5891 = CARTESIAN_POINT ( 'NONE',  ( -0.8107537697050254399, 0.1574803149606300301, 1.557578740157481212 ) ) ;
#5892 = CARTESIAN_POINT ( 'NONE',  ( 0.8019270111902716547, -0.1787899950787401604, 0.9153543306548987957 ) ) ;
#5893 = CARTESIAN_POINT ( 'NONE',  ( 0.6971942568897637749, 2.189545951927499583E-17, 1.975885826717889815 ) ) ;
#5894 = CARTESIAN_POINT ( 'NONE',  ( 0.8759842519685039353, 0.1574803149606299191, 0.2854330707586145710 ) ) ;
#5895 = EDGE_LOOP ( 'NONE', ( #46884, #7248, #20128, #30293 ) ) ;
#5896 = DIRECTION ( 'NONE',  ( -0.000000000000000000, 1.000000000000000000, -0.000000000000000000 ) ) ;
#5897 = CARTESIAN_POINT ( 'NONE',  ( 1.011659506949417420, 0.09243204465627147259, 0.03936570540571364407 ) ) ;
#5898 = CARTESIAN_POINT ( 'NONE',  ( -0.1113553986120547346, -1.666338582569637738, 0.1113553986120547346 ) ) ;
#5899 = CARTESIAN_POINT ( 'NONE',  ( -1.033464566929134687, -0.06523048226347956391, 0.2337598424121580809 ) ) ;
#5900 = CARTESIAN_POINT ( 'NONE',  ( 0.7495606340400177148, -0.1264236179284866091, 1.345964566875370139 ) ) ;
#5901 = CARTESIAN_POINT ( 'NONE',  ( 0.7185039370078739607, 1.928577636452523993E-17, 1.240157480207432883 ) ) ;
#5902 = CARTESIAN_POINT ( 'NONE',  ( -0.1787899950787401882, 0.07824803154982658271, 0.000000000000000000 ) ) ;
#5903 = CARTESIAN_POINT ( 'NONE',  ( -0.8107537697050254399, -0.1574803149606297803, 1.011318897530268712 ) ) ;
#5904 = ADVANCED_FACE ( 'NONE', ( #43561 ), #34231, .T. ) ;
#5905 = DIRECTION ( 'NONE',  ( -0.000000000000000000, 1.000000000000000000, 0.000000000000000000 ) ) ;
#5906 = CARTESIAN_POINT ( 'NONE',  ( -0.7185039370078739607, 1.928577636452523993E-17, 0.2165354329633393804 ) ) ;
#5907 = DIRECTION ( 'NONE',  ( 0.000000000000000000, 0.000000000000000000, 1.000000000000000000 ) ) ;
#5908 = ORIENTED_EDGE ( 'NONE', *, *, #29325, .T. ) ;
#5909 = CARTESIAN_POINT ( 'NONE',  ( 0.1264236179284866091, -1.752460629867496067, -0.1264236179284866091 ) ) ;
#5910 = CARTESIAN_POINT ( 'NONE',  ( -1.054774247047244540, -0.07405724077823318263, 1.008858267662772423 ) ) ;
#5911 = CARTESIAN_POINT ( 'NONE',  ( -0.6971942568897648851, -0.07405724077823297447, 1.973425196796630088 ) ) ;
#5912 = EDGE_LOOP ( 'NONE', ( #30515, #10422, #17857, #42784, #24375, #36154, #43440, #45182 ) ) ;
#5913 = EDGE_CURVE ( 'NONE', #14452, #1242, #11460, .T. ) ;
#5914 = CARTESIAN_POINT ( 'NONE',  ( -0.8019270111902717657, 0.1787899950787401604, 0.7086614172690703928 ) ) ;
#5915 = CARTESIAN_POINT ( 'NONE',  ( 0.4509871776442260227, 4.466152701071653354E-17, 0.000000000000000000 ) ) ;
#5916 = CARTESIAN_POINT ( 'NONE',  ( 0.003880704729684991260, 0.04358867701646648718, -0.1377950254940095709 ) ) ;
#5917 = VERTEX_POINT ( 'NONE', #881 ) ;
#5918 = CARTESIAN_POINT ( 'NONE',  ( -0.3690944881889761109, 0.1864803149606353017, 0.7480314960629921295 ) ) ;
#5919 = ORIENTED_EDGE ( 'NONE', *, *, #4524, .T. ) ;
#5920 = CARTESIAN_POINT ( 'NONE',  ( -0.4338976377952755703, -2.656856766417909227E-17, 0.000000000000000000 ) ) ;
#5921 = CARTESIAN_POINT ( 'NONE',  ( -0.6971942568897626646, 0.07405724077823318263, 0.6692913385289144257 ) ) ;
#5922 = CARTESIAN_POINT ( 'NONE',  ( 1.033464566929133799, 0.000000000000000000, 1.338582677057826853 ) ) ;
#5923 = CARTESIAN_POINT ( 'NONE',  ( -0.6971942568897648851, 0.07405724077823318263, 1.658464566875369472 ) ) ;
#5924 = CARTESIAN_POINT ( 'NONE',  ( -0.1968503937007874127, -0.5192708129487058066, -0.8938220056861535534 ) ) ;
#5925 = CARTESIAN_POINT ( 'NONE',  ( -0.8107537697050254399, 0.1574803149606300301, 0.4945866141732282451 ) ) ;
#5926 = LINE ( 'NONE', #13373, #6286 ) ;
#5927 = EDGE_LOOP ( 'NONE', ( #362, #35144, #21456, #1197 ) ) ;
#5928 = FACE_OUTER_BOUND ( 'NONE', #1151, .T. ) ;
#5929 = CARTESIAN_POINT ( 'NONE',  ( -0.9873396505805591694, 0.1113553986120547346, 1.264763779420031486 ) ) ;
#5931 = CARTESIAN_POINT ( 'NONE',  ( 0.000000000000000000, 0.1200787401574803237, 0.000000000000000000 ) ) ;
#5930 = CARTESIAN_POINT ( 'NONE',  ( 0.06523048226347956391, -0.4876968503937005872, 0.1574803149606297803 ) ) ;
#5932 = CARTESIAN_POINT ( 'NONE',  ( -0.8107537697050254399, 0.1574803149606300301, 0.4158464566929134798 ) ) ;
#5933 = CARTESIAN_POINT ( 'NONE',  ( 0.1113553986120547346, 0.02657480314960630058, 0.1113553986120547346 ) ) ;
#5934 = CARTESIAN_POINT ( 'NONE',  ( 0.7646288533564489232, 0.1113553986120547346, 1.126968503937007871 ) ) ;
#5935 = DIRECTION ( 'NONE',  ( 0.000000000000000000, -0.7880107536067214591, 0.6156614753256588468 ) ) ;
#5936 = CARTESIAN_POINT ( 'NONE',  ( 0.9412147342319837628, -0.1574803149606297803, 0.5831692912310552090 ) ) ;
#5937 = CARTESIAN_POINT ( 'NONE',  ( -0.1603352656429097856, -0.08956088745009382901, -0.06684612809662447697 ) ) ;
#5938 = PRODUCT_DEFINITION_SHAPE ( 'NONE', 'NONE',  #33920 ) ;
#5939 = CARTESIAN_POINT ( 'NONE',  ( 0.1787899950787401604, -0.5295275590013543976, -0.07405724077823318263 ) ) ;
#5940 = CARTESIAN_POINT ( 'NONE',  ( 1.033464566929133799, 1.928577636452524610E-17, 4.498031496062992574 ) ) ;
#5941 = ORIENTED_EDGE ( 'NONE', *, *, #12634, .F. ) ;
#5942 = CARTESIAN_POINT ( 'NONE',  ( -0.8107537697050254399, -0.1574803149606297803, 1.060531496062992352 ) ) ;
#5943 = FACE_OUTER_BOUND ( 'NONE', #597, .T. ) ;
#5944 = CARTESIAN_POINT ( 'NONE',  ( 0.9500414927467378812, 0.1787899950787401604, 0.8562992125446617919 ) ) ;
#5945 = CARTESIAN_POINT ( 'NONE',  ( 0.9873396505805591694, -0.1113553986120547346, 1.461614173228346525 ) ) ;
#5946 = CARTESIAN_POINT ( 'NONE',  ( 1.033464566929134687, -0.06523048226347956391, 0.7062007872940467834 ) ) ;
#5947 = CARTESIAN_POINT ( 'NONE',  ( 0.1270800023317771588, 0.06294831640120648886, -0.1270800023317771588 ) ) ;
#5948 = CARTESIAN_POINT ( 'NONE',  ( -0.07405724077823318263, -1.100393700733639069, 0.1787899950787401604 ) ) ;
#5949 = CARTESIAN_POINT ( 'NONE',  ( 0.06523048226347956391, -1.378444881889764551, -0.1574803149606300301 ) ) ;
#5950 = SHAPE_REPRESENTATION ( 'Link Bar', ( #20860 ), #6323 ) ;
#5951 = CARTESIAN_POINT ( 'NONE',  ( -0.7185039370078746268, 0.06523048226347956391, 1.405019685039369914 ) ) ;
#5952 = EDGE_CURVE ( 'NONE', #8391, #34753, #14668, .T. ) ;
#5953 = CIRCLE ( 'NONE', #39609, 0.1574803149606299191 ) ;
#5954 = ORIENTED_EDGE ( 'NONE', *, *, #753, .F. ) ;
#5955 = CARTESIAN_POINT ( 'NONE',  ( -0.9500414927467378812, -0.1787899950787401604, 1.988188976324187562 ) ) ;
#5956 = CARTESIAN_POINT ( 'NONE',  ( 0.8759842519685039353, 0.1787899950787401882, 1.847933070812378009 ) ) ;
#5957 = ORIENTED_EDGE ( 'NONE', *, *, #25512, .T. ) ;
#5958 = CARTESIAN_POINT ( 'NONE',  ( 0.8759842519685039353, 0.000000000000000000, 4.498031496062992574 ) ) ;
#5959 = CARTESIAN_POINT ( 'NONE',  ( -0.6971942568897637749, 2.189545951927499583E-17, 1.498523621993480326 ) ) ;
#5960 = CARTESIAN_POINT ( 'NONE',  ( -0.1296641775163210608, 1.495705267341510769, -0.3569552279982081133 ) ) ;
#5961 = EDGE_CURVE ( 'NONE', #47215, #32278, #4960, .T. ) ;
#5962 = AXIS2_PLACEMENT_3D ( 'NONE', #40068, #25952, #17812 ) ;
#5963 = CARTESIAN_POINT ( 'NONE',  ( -0.6971942568897637749, 2.189545951927499583E-17, 0.2829724408911185041 ) ) ;
#5964 = CARTESIAN_POINT ( 'NONE',  ( 0.2362204724409449064, -0.5708661417322835607, 0.9783464566929134243 ) ) ;
#5965 = CARTESIAN_POINT ( 'NONE',  ( -0.6971942568897637749, 2.189545951927499583E-17, 1.936515747977732405 ) ) ;
#5966 = CARTESIAN_POINT ( 'NONE',  ( 0.05636151600968929837, -0.07780576619186881093, -0.2528927375204811923 ) ) ;
#5967 = CARTESIAN_POINT ( 'NONE',  ( -0.8759842519685039353, -0.1574803149606299191, 1.811023622047244208 ) ) ;
#5968 = DIRECTION ( 'NONE',  ( 0.000000000000000000, 0.000000000000000000, -1.000000000000000000 ) ) ;
#5969 = CARTESIAN_POINT ( 'NONE',  ( -0.1264236179284866091, -0.2575058579930181168, -0.1264236179284866091 ) ) ;
#5970 = CARTESIAN_POINT ( 'NONE',  ( -0.06937174427877500216, -0.09842519685039370636, -0.1728322085960811161 ) ) ;
#5971 = CARTESIAN_POINT ( 'NONE',  ( -0.7646288533564489232, -0.1113553986120547346, 1.491141732283464583 ) ) ;
#5972 = CARTESIAN_POINT ( 'NONE',  ( 0.1574803149606299746, 0.1473293504822046074, -0.9532488779249699284 ) ) ;
#5973 = VERTEX_POINT ( 'NONE', #44730 ) ;
#5974 = CARTESIAN_POINT ( 'NONE',  ( -1.054774247047244540, -0.07405724077823318263, 1.245078740103716886 ) ) ;
#5975 = ORIENTED_EDGE ( 'NONE', *, *, #32989, .T. ) ;
#5976 = CARTESIAN_POINT ( 'NONE',  ( -0.1264236179284866091, -1.024114173174582643, 0.1264236179284866091 ) ) ;
#5977 = ADVANCED_FACE ( 'NONE', ( #11706, #44963, #26331, #40892, #22950 ), #18632, .T. ) ;
#5978 = CARTESIAN_POINT ( 'NONE',  ( 0.1787899950787401882, -1.240649606245448622, -2.189545951927503898E-17 ) ) ;
#5979 = CIRCLE ( 'NONE', #45788, 0.4724409448818899238 ) ;
#5980 = CARTESIAN_POINT ( 'NONE',  ( -1.033464566929134687, -0.06523048226347956391, 1.375492125876724980 ) ) ;
#5981 = CARTESIAN_POINT ( 'NONE',  ( 1.002407869896990045, 0.1264236179284866091, 0.4207677164816693294 ) ) ;
#5982 = CARTESIAN_POINT ( 'NONE',  ( -0.1270800023317771588, -0.5177603450161165632, -0.1270800023317771588 ) ) ;
#5983 = LINE ( 'NONE', #35705, #10973 ) ;
#5984 = CARTESIAN_POINT ( 'NONE',  ( -1.033464566929134687, 0.06523048226347956391, 0.8292322833570401341 ) ) ;
#5985 = CARTESIAN_POINT ( 'NONE',  ( -1.033464566929133799, 0.000000000000000000, 0.7185039370078739607 ) ) ;
#5986 = CARTESIAN_POINT ( 'NONE',  ( -0.1574803149606299191, -0.06692913385826770867, 0.000000000000000000 ) ) ;
#5987 = CARTESIAN_POINT ( 'NONE',  ( 1.002407869896990045, 0.1264236179284866091, 0.8932086613635591421 ) ) ;
#5989 = CARTESIAN_POINT ( 'NONE',  ( 0.4620708661417351482, 0.8070866141732281340, 0.5854071585544579071 ) ) ;
#5988 = AXIS2_PLACEMENT_3D ( 'NONE', #23729, #4784, #19885 ) ;
#5990 = CARTESIAN_POINT ( 'NONE',  ( -0.5555748031496045014, 0.6449983665207589256, -0.7480314960629921295 ) ) ;
#5991 = CARTESIAN_POINT ( 'NONE',  ( 1.033464566929134687, 0.06523048226347956391, 0.08120078729404769935 ) ) ;
#5992 = ADVANCED_FACE ( 'NONE', ( #7610 ), #4991, .F. ) ;
#5993 = VERTEX_POINT ( 'NONE', #29714 ) ;
#5994 = CARTESIAN_POINT ( 'NONE',  ( 0.9412147342319837628, 0.1574803149606300301, 0.7160433069790875793 ) ) ;
#5995 = CARTESIAN_POINT ( 'NONE',  ( 0.1787899950787401882, -0.6550196849856062542, -2.189545951927503898E-17 ) ) ;
#5996 = ADVANCED_FACE ( 'NONE', ( #8559 ), #22468, .T. ) ;
#5997 = CARTESIAN_POINT ( 'NONE',  ( 0.07405724077823318263, -1.469488188922614791, -0.1787899950787401604 ) ) ;
#5998 = CARTESIAN_POINT ( 'NONE',  ( 1.002407869896990045, -0.1264236179284866091, 0.3371062991588349989 ) ) ;
#5999 = EDGE_CURVE ( 'NONE', #3498, #763, #329, .T. ) ;
#6000 = CARTESIAN_POINT ( 'NONE',  ( -0.8759842519685039353, 0.1787899950787401882, 1.843011810969858333 ) ) ;
#6001 = ORIENTED_EDGE ( 'NONE', *, *, #8765, .T. ) ;
#6002 = CARTESIAN_POINT ( 'NONE',  ( -1.054774247047244540, -0.07405724077823318263, 1.481299212544662680 ) ) ;
#6003 = CARTESIAN_POINT ( 'NONE',  ( 1.054774247047244540, 0.07405724077823318263, 1.407480314906865981 ) ) ;
#6004 = DIRECTION ( 'NONE',  ( -1.000000000000000000, -0.000000000000000000, 0.000000000000000000 ) ) ;
#6005 = CARTESIAN_POINT ( 'NONE',  ( -0.8019270111902717657, 0.1787899950787401604, 0.6692913385289144257 ) ) ;
#6006 = CARTESIAN_POINT ( 'NONE',  ( 0.6971942568897626646, -0.07405724077823297447, 0.1279527558517483676 ) ) ;
#6007 = DIRECTION ( 'NONE',  ( -1.000000000000000000, 0.000000000000000000, 0.000000000000000000 ) ) ;
#6008 = PRESENTATION_STYLE_ASSIGNMENT (( #9146 ) ) ;
#6009 = CARTESIAN_POINT ( 'NONE',  ( 1.054774247047244096, 0.000000000000000000, 0.6176181101824566033 ) ) ;
#6010 = CARTESIAN_POINT ( 'NONE',  ( -0.8759842519685039353, 0.1787899950787401882, 0.5437992125446614589 ) ) ;
#6011 = EDGE_CURVE ( 'NONE', #43147, #15333, #1362, .T. ) ;
#6012 = CARTESIAN_POINT ( 'NONE',  ( 0.1594432092295600123, -0.09246610911307991121, 0.1933784749626996369 ) ) ;
#6013 = VECTOR ( 'NONE', #21923, 39.37007874015748143 ) ;
#6014 = VERTEX_POINT ( 'NONE', #27044 ) ;
#6015 = CARTESIAN_POINT ( 'NONE',  ( -0.7185039370078746268, -0.06523048226347956391, 0.5044291338582675976 ) ) ;
#6016 = CARTESIAN_POINT ( 'NONE',  ( 1.054774247047244540, 0.07405724077823318263, 1.249999999946235896 ) ) ;
#6017 = CARTESIAN_POINT ( 'NONE',  ( 0.2010203987887842214, -0.09851384488251044291, -0.04151172976903000356 ) ) ;
#6018 = ORIENTED_EDGE ( 'NONE', *, *, #41186, .F. ) ;
#6019 = CARTESIAN_POINT ( 'NONE',  ( 0.2871444924769520068, 1.495705267341507883, -0.3569552279982047271 ) ) ;
#6020 = CARTESIAN_POINT ( 'NONE',  ( -0.8019270111902717657, 0.1787899950787401604, 0.9842519684501742638 ) ) ;
#6021 = AXIS2_PLACEMENT_3D ( 'NONE', #45675, #23431, #22951 ) ;
#6022 = CARTESIAN_POINT ( 'NONE',  ( -0.07405724077823318263, -1.559179086339476550, -0.1787899950787401604 ) ) ;
#6023 = ORIENTED_EDGE ( 'NONE', *, *, #9749, .T. ) ;
#6024 = DIRECTION ( 'NONE',  ( 0.000000000000000000, 0.000000000000000000, -1.000000000000000000 ) ) ;
#6025 = CARTESIAN_POINT ( 'NONE',  ( 0.07405724077823318263, -0.5639763778989922427, -0.1787899950787401604 ) ) ;
#6026 = CYLINDRICAL_SURFACE ( 'NONE', #17014, 0.1574803149606299191 ) ;
#6027 = DIRECTION ( 'NONE',  ( 0.000000000000000000, 1.000000000000000000, 0.000000000000000000 ) ) ;
#6028 = CARTESIAN_POINT ( 'NONE',  ( 0.1787899950787401604, -0.7312992125446612368, 0.07405724077823318263 ) ) ;
#6029 = DIRECTION ( 'NONE',  ( 0.000000000000000000, 0.000000000000000000, 1.000000000000000000 ) ) ;
#6030 = CARTESIAN_POINT ( 'NONE',  ( -0.7185039370078739607, 1.928577636452523993E-17, 0.9645669290263307882 ) ) ;
#6031 = CARTESIAN_POINT ( 'NONE',  ( 0.1264236179284866091, 0.008242173503044743221, -0.1264236179284866091 ) ) ;
#6032 = CARTESIAN_POINT ( 'NONE',  ( 0.1264236179284866091, 0.08809055123486594918, 0.1264236179284866091 ) ) ;
#6033 = ITEM_DEFINED_TRANSFORMATION ( 'NONE', 'NONE', #40786,  #20860 ) ;
#6034 = EDGE_CURVE ( 'NONE', #15025, #33889, #41592, .T. ) ;
#6035 = DIRECTION ( 'NONE',  ( 0.000000000000000000, -1.000000000000000000, 0.000000000000000000 ) ) ;
#6036 = CARTESIAN_POINT ( 'NONE',  ( 0.8759842519685039353, -0.1787899950787401882, 0.5241141731745827537 ) ) ;
#6037 = CARTESIAN_POINT ( 'NONE',  ( -1.054774247047244540, 0.07405724077823318263, 0.8169291338045038264 ) ) ;
#6038 = VECTOR ( 'NONE', #12574, 39.37007874015748143 ) ;
#6040 = FACE_OUTER_BOUND ( 'NONE', #19507, .T. ) ;
#6039 = CARTESIAN_POINT ( 'NONE',  ( 0.1574803149606299191, -0.9133858267716534751, -1.928577636452523993E-17 ) ) ;
#6041 = CARTESIAN_POINT ( 'NONE',  ( 3.301370929368692659E-17, -1.723469006433439032, 0.1797182628040039365 ) ) ;
#6042 = CARTESIAN_POINT ( 'NONE',  ( 1.054774247047244540, -0.07405724077823318263, 1.520669291284818758 ) ) ;
#6044 = DIRECTION ( 'NONE',  ( 1.000000000000000000, -0.000000000000000000, -0.000000000000000000 ) ) ;
#6043 = CARTESIAN_POINT ( 'NONE',  ( 0.1564664719456493325, 0.09340956239926197224, -0.1950971111691700843 ) ) ;
#6045 = CARTESIAN_POINT ( 'NONE',  ( 0.7495606340400177148, -0.1264236179284866091, 0.4404527558517480901 ) ) ;
#6046 = EDGE_CURVE ( 'NONE', #398, #11324, #8214, .T. ) ;
#6047 = EDGE_LOOP ( 'NONE', ( #7657, #28457, #38794, #28639, #23318 ) ) ;
#6048 = CARTESIAN_POINT ( 'NONE',  ( -0.2471922904502826812, -0.03219022224904098672, -0.1427165354330708902 ) ) ;
#6049 = DIRECTION ( 'NONE',  ( 0.000000000000000000, 0.000000000000000000, -1.000000000000000000 ) ) ;
#6050 = CARTESIAN_POINT ( 'NONE',  ( 0.8070866141732283561, -0.0009842519685049383633, 0.7574803149606299524 ) ) ;
#6052 = CARTESIAN_POINT ( 'NONE',  ( -0.1264236179284866091, -0.1186023621509608300, 0.1264236179284866091 ) ) ;
#6051 = CARTESIAN_POINT ( 'NONE',  ( -0.1113553986120547346, -0.8789370077664881986, 0.1113553986120547346 ) ) ;
#6053 = VECTOR ( 'NONE', #23843, 39.37007874015748143 ) ;
#6054 = CARTESIAN_POINT ( 'NONE',  ( 0.9500414927467378812, -0.1787899950787401604, 0.4478346456155276045 ) ) ;
#6055 = CARTESIAN_POINT ( 'NONE',  ( -0.1264236179284866091, -0.9896653542769447975, -0.1264236179284866091 ) ) ;
#6056 = CARTESIAN_POINT ( 'NONE',  ( -1.033464566929134687, -0.06523048226347956391, 0.9424212597349931331 ) ) ;
#6057 = CARTESIAN_POINT ( 'NONE',  ( -0.6971942568897648851, -0.07405724077823297447, 1.382874015694268044 ) ) ;
#6058 = ORIENTED_EDGE ( 'NONE', *, *, #28100, .T. ) ;
#6059 = CONICAL_SURFACE ( 'NONE', #23667, 0.2559055118110236116, 1.047197551196597409 ) ;
#6060 = CARTESIAN_POINT ( 'NONE',  ( 0.7495606340400177148, 0.1264236179284866091, 0.9473425196312755814 ) ) ;
#6061 = VERTEX_POINT ( 'NONE', #47361 ) ;
#6062 = CARTESIAN_POINT ( 'NONE',  ( 0.1264236179284866091, -1.358759842465921297, -0.1264236179284866091 ) ) ;
#6063 = CARTESIAN_POINT ( 'NONE',  ( -0.8107537697050253289, 0.1574803149606300301, 0.5241141731208195376 ) ) ;
#6064 = CARTESIAN_POINT ( 'NONE',  ( 0.7185039370078739607, 1.928577636452523993E-17, 1.801181102362204633 ) ) ;
#6065 = CARTESIAN_POINT ( 'NONE',  ( -0.8107537697050253289, 0.1574803149606300301, 1.439468503937006538 ) ) ;
#6066 = CARTESIAN_POINT ( 'NONE',  ( -0.6971942568897626646, -0.07405724077823297447, 0.8710629920722218200 ) ) ;
#6067 = DIRECTION ( 'NONE',  ( 1.000000000000000000, 0.000000000000000000, 0.000000000000000000 ) ) ;
#6068 = CARTESIAN_POINT ( 'NONE',  ( -0.7250449425850237217, -0.07798161211236025181, 0.03937007874015843734 ) ) ;
#6069 = CARTESIAN_POINT ( 'NONE',  ( 0.9500414927467377701, 0.1787899950787401604, 0.1131889763241892000 ) ) ;
#6070 = EDGE_CURVE ( 'NONE', #1625, #35241, #29694, .T. ) ;
#6071 = CARTESIAN_POINT ( 'NONE',  ( 0.7646288533564489232, 0.1113553986120547346, 1.392716535325543292 ) ) ;
#6072 = ORIENTED_EDGE ( 'NONE', *, *, #17257, .F. ) ;
#6073 = ORIENTED_EDGE ( 'NONE', *, *, #44618, .T. ) ;
#6074 = CARTESIAN_POINT ( 'NONE',  ( -0.8759842519685039353, 0.1787899950787401882, 1.724901574749385880 ) ) ;
#6075 = VERTEX_POINT ( 'NONE', #25321 ) ;
#6076 = DIRECTION ( 'NONE',  ( 0.000000000000000000, -1.000000000000000000, 0.000000000000000000 ) ) ;
#6077 = VECTOR ( 'NONE', #30271, 39.37007874015748143 ) ;
#6078 = CARTESIAN_POINT ( 'NONE',  ( 0.1574803149606299746, 0.6926248950869623444, -0.5411378750921671532 ) ) ;
#6079 = CARTESIAN_POINT ( 'NONE',  ( 3.284318927891251994E-17, -1.108883810748923171, 0.1787899950787401882 ) ) ;
#6080 = VERTEX_POINT ( 'NONE', #9989 ) ;
#6081 = CARTESIAN_POINT ( 'NONE',  ( -0.07405724077823318263, -0.1505905511273389341, 0.1787899950787401604 ) ) ;
#6082 = ORIENTED_EDGE ( 'NONE', *, *, #34470, .F. ) ;
#6083 = VERTEX_POINT ( 'NONE', #17643 ) ;
#6084 = AXIS2_PLACEMENT_3D ( 'NONE', #9396, #46266, #20160 ) ;
#6085 = CARTESIAN_POINT ( 'NONE',  ( -0.9873396505805591694, -0.1113553986120547346, 0.4281496061916850726 ) ) ;
#6086 = ( BOUNDED_SURFACE ( )  B_SPLINE_SURFACE ( 1, 2, ( 
 ( #41107, #12158, #39997, #4700, #41341, #33980, #14623, #19331, #26782, #14390, #11042, #6945, #11928, #7422, #1107, #30398, #36666, #29040, #3824, #18444, #10810, #33752, #37791, #34214, #25423, #863, #23174, #19570, #15766, #4943, #1344, #15998, #22930, #47451, #30622, #12408, #29293, #45186, #15523, #26547, #8299, #27029, #17969, #7190, #21567, #36205, #32623, #3357, #43841, #36443, #21815, #3595, #18215, #32857, #30165, #42532, #45656, #31095, #20035, #46377, #19800, #23881, #8781, #34918, #16230, #27966, #35146, #23418, #13338, #24351, #38949, #34676, #12874, #38730, #38020, #9262, #31559, #13557, #9735, #5899, #34432, #41578, #16459, #23641, #30864, #1579, #45426, #2289, #12643, #6114, #27508, #42059, #1823, #27269, #41818, #38493, #38254, #2062, #5416, #20739, #16919, #5662, #35381, #2526, #17152, #20270, #16694, #20511, #31322, #45899, #46141, #13114, #31793, #27747, #42312, #9504, #24126, #14035, #39179, #24813, #20967, #3483, #6594, #9970, #46844, #7318, #42751, #2756, #2988, #3231, #3717, #28681, #25297, #32017, #10691, #39886, #39412, #7071, #17862, #21698, #25550, #43249, #36074, #13788, #36331, #32503, #18098, #40122, #32742, #18338, #10450, #21207, #25050, #102, #28435, #35839, #47338, #14510, #42999, #29174, #39644, #28193, #14280, #43726, #10210, #10929, #21937, #36557, #17620, #24582, #6352, #35613, #32265, #17379, #47086, #6825, #21445, #28920, #43484, #26008, #33930, #40587, #37022, #19980, #31501, #27920, #19748, #16411, #35092, #13287, #31268, #24072, #2240, #42483, #16638, #41766, #9687, #6063, #8968, #46084, #12823, #20216, #38440, #5848, #12347, #1522, #38681, #45376, #45847, #20689, #12592, #27215, #2011, #16175, #30808, #20457, #31037, #5123, #26967, #1290, #15945, #24300, #34383, #42000, #34864, #38902, #30570, #34620, #45131, #23587, #38199, #13054, #5361, #1770, #45604, #27456, #41522, #8726, #23362, #9204, #37970, #23823, #5608, #27691, #42255, #9456, #28378, #6298, #21153, #7016, #31737, #20921, #42700, #10397, #39596, #3428, #24763, #39361, #3178, #9919, #17566, #2706, #17807, #47035, #28867, #32456, #14225, #32204, #43425, #6541, #25001, #31968, #35563, #2929, #17334, #10634, #25239, #46791, #46326, #39826, #46553, #36276, #2469, #42945, #13978, #2384, #12967, #34782, #38346, #20839, #2618, #30717, #1923, #45758, #42158, #27128, #35249, #12505, #17020, #31423, #35478, #16555, #20604, #9366, #46230, #24225, #23989, #35009, #13434, #45289, #23518, #31184, #41678, #8883, #38588, #31657, #5764, #38121, #16330, #20369, #19897, #5984, #28064, #45519, #42627, #2157, #9836, #12741, #16784, #34527, #24444, #46000, #39044, #1684, #13208, #27842, #27372, #42403, #6210, #41914, #9125, #43579, #25147, #39980, #3091, #3343, #10307, #21069, #46945, #35706, #18198, #7173, #28780, #46468, #43820, #46700, #36186, #14603, #25638, #6925, #36422, #14136, #21303, #24920, #22020, #36646, #13652, #35931, #43346, #10549, #28289, #21797, #42852, #3580, #17948, #10061, #39512, #32838, #39737, #47432, #10793, #21548, #32606, #40214, #39277, #28533, #17716, #6686, #47194, #14375, #29021, #25403, #11254, #36880, #29967, #196, #26589, #44750, #18653, #22969, #33544, #19364, #33312, #37105, #40446, #30430, #659, #34019, #44055, #15313, #436, #33788, #23215, #15088, #29735, #4485, #4034, #44276, #8342, #18889, #7632, #14844, #8577, #3806, #1144, #22248, #44514, #22730, #41143, #18423, #22487, #37577, #11480, #26102, #904, #40674, #7871, #11731, #4254, #33071, #29509, #4738, #26350, #15802, #44982, #40910, #25864, #8108, #37336, #19124, #15566, #30205, #12194, #11968, #26820, #41377, #38531, #34953, #28005, #23681, #5460, #2097, #30661, #9062, #16958, #4986, #12443, #12682, #12915, #13376, #38291, #16727, #41614, #20313, #31363, #34469, #45943, #27545, #13154, #2331, #20076, #45695, #23455, #27787, #42097, #42348, #31598, #9544, #42570, #34722, #1619, #1861, #9779, #8820, #16269, #24166, #38768, #38058, #5929, #16499, #37829, #23923, #20546, #5213, #46179, #19606, #34247, #45458, #1376, #16033, #45221, #41858, #27065, #9302, #31129, #19841, #30901, #5700, #27308, #39457, #6633, #28229, #21252, #7116, #3526, #42792, #35877, #10737, #36371, #6868, #47136, #25345, #18139, #39681, #17422, #32783, #29219, #32059, #21739, #3030, #43293, #14076, #28966, #35421, #24621, #14321, #21489, #2558, #24389, #46647, #6397, #46413, #31826, #13592, #32548, #10008, #39929, #28475, #17661, #2793, #38988, #39221, #46888, #6156, #28724, #21008, #47377, #17900, #35655, #43523, #14549, #10493, #25091, #36121, #3276, #40160, #26050, #845, #30381, #26529, #140, #7581, #7359, #15037, #44228, #21971, #22194, #3753, #33735, #36830, #36596, #44001, #8050, #44689, #37279, #18599, #22678, #15505, #18376, #29686, #10969, #607, #40623, #40855, #11906, #7817, #33018, #22433, #37053, #14793, #4206, #41089, #37526, #29454, #18836, #8286, #22912, #4434, #4682, #19312, #1088, #26298, #3981, #15747, #25587, #33261, #11203, #33491, #29911, #15264, #25816, #40392, #385, #11674, #19066, #29151, #37470, #41810, #12633, #41565, #15988, #8771, #1332, #30611, #45176, #38244, #9010, #1814, #12396, #12864, #27499, #23870, #38481, #5652, #20262, #2051, #20730, #25285, #36318, #3473, #46598, #24803, #3218, #35371, #21196, #43471, #25542, #21688, #42743, #2741, #2513, #10196, #39401, #17139, #17369, #46366, #28908, #32005, #31783, #6583, #32731, #13546, #28182, #28422, #28669, #29158, #35829, #17848, #9958, #36062, #32494, #13777, #47076, #43236, #14269, #18085, #2976, #14022, #39170, #10678, #10439, #39874, #47324, #7061, #43715, #17609, #42989, #32255, #10919, #24570, #46833, #14497, #6104, #6342, #20956, #25038, #35602, #39632, #6815, #21434, #11770, #26389, #44321, #25678, #4294, #26143, #25442, #21588, #11291, #32875, #29313, #7211, #3844, #699, #3380, #40015, #47228, #7671, #4076, #44552, #40253, #22059, #18690, #14412, #14884, #3614, #33349, #40714, #22528, #15127, #472, #29544, #29772, #7441, #40486, #17860, #43618, #36684, #10826, #7913, #11524, #18465, #17988, #18926, #21833, #25903, #33586, #15357, #44096, #37145, #33115, #11061, #14642, #6966, #32642, #29062, #240, #22287, #36923, #36458, #30007, #18232, #43860, #41660, #31169, #34059, #30940, #19648, #9106, #34511, #8621, #45267, #23726, #45742, #33825, #12239, #8143, #12951, #1187, #45500, #26863 ),
 ( #12006, #4781, #38101, #23498, #44791, #27354, #41423, #40949, #27113, #12725, #26626, #5263, #41897, #19882, #15846, #1664, #38331, #945, #45024, #4530, #30702, #23258, #16311, #15604, #8866, #5503, #19168, #37873, #34293, #20116, #30241, #1418, #37623, #34763, #1906, #16542, #41179, #8381, #16077, #23011, #12488, #19407, #30469, #35231, #28271, #42834, #24899, #5740, #2827, #3008, #33241, #25071, #7341, #18582, #366, #10949, #40373, #3507, #25320, #28945, #26028, #40603, #21230, #39907, #36352, #32763, #17642, #25799, #32288, #7560, #21954, #46867, #14301, #11188, #47360, #36809, #14772, #29198, #25569, #3965, #14053, #43272, #7095, #10474, #39662, #43506, #22173, #21721, #6846, #3255, #43748, #17879, #43983, #15020, #32523, #29672, #3737, #44210, #10714, #18357, #33000, #45150, #26510, #34179, #33473, #41071, #8029, #44912, #23382, #22661, #19048, #15728, #26278, #11656, #37752, #11887, #44437, #18817, #8743, #7799, #30587, #40838, #37508, #1069, #4907, #22415, #44671, #19528, #33716, #823, #26745, #15487, #30130, #8268, #22895, #37039, #4189, #26991, #4664, #591, #41540, #19291, #15248, #41304, #33948, #30366, #12124, #23136, #29893, #32443, #21631, #36265, #18269, #11559, #40751, #33156, #22566, #17796, #47021, #18499, #10865, #28856, #43416, #25485, #39815, #14681, #36717, #40287, #7004, #3416, #18032, #32678, #277, #47265, #29100, #40051, #7251, #21873, #3649, #32912, #32, #43897, #11095, #25718, #7472, #3880, #14922, #29587, #44128, #26432, #5066, #33869, #12761, #34549, #40997, #30972, #38369, #20155, #34100, #30504, #1700, #8183, #1457, #27391, #37420, #34802, #988, #8420, #19210, #15880, #30739, #30283, #37668, #44834, #1948, #1226, #26667, #45308, #16578, #41217, #12529, #41704, #20859, #21331, #31679, #42878, #2177, #10089, #24700, #9626, #39301, #35502, #6476, #43131, #46259, #6234, #31439, #21096, #2642, #35734, #10335, #2872, #35962, #13456, #24243, #28084, #3120, #16800, #38840, #17507, #32138, #46021, #46732, #42646, #17747, #31911, #13916, #13230, #28562, #24947, #39543, #6005, #6716, #45780, #5784, #2408, #12989, #17276, #9858, #27629, #42182, #24469, #38607, #39065, #46494, #27862, #13673, #24007, #20389, #35029, #20626, #35272, #7660, #18681, #44311, #227, #25433, #11513, #37135, #40008, #29763, #43851, #3835, #22051, #36913, #43371, #32633, #22277, #29535, #10583, #32394, #7202, #14403, #6957, #28810, #39766, #40476, #25181, #33340, #36452, #21824, #10820, #4285, #21577, #14634, #46972, #25670, #36218, #464, #25894, #14165, #4066, #15117, #26136, #3607, #18227, #44086, #3371, #42310, #40704, #17980, #7903, #47221, #29052, #43610, #32867, #29303, #11054, #40245, #7432, #22519, #36676, #18457, #33105, #14875, #11284, #40940, #41171, #37864, #9095, #15836, #27102, #4519, #27344, #33576, #23000, #29999, #5018, #44543, #19155, #45016, #34281, #935, #12229, #20525, #42548, #24594, #2540, #2771, #27763, #9276, #45913, #17395, #31105, #23896, #9751, #24365, #45668, #46392, #42324, #32034, #46156, #31807, #12886, #38963, #13569, #6128, #20282, #20752, #28205, #20049, #9518, #12656, #2304, #24142, #35395, #42768, #38746, #5431, #5910, #35160, #27519, #16932, #39192, #6367, #42073, #13351, #35629, #27283, #38504, #5675, #27979, #34928, #2076, #41831, #9034, #23656, #38266, #34691, #1834, #14765, #17637, #39902, #18115, #36572, #3958, #17875, #3731, #14048, #28696, #29194, #43264, #46861, #43500, #10468, #18580, #46624, #18351, #32519, #43978, #32995, #25065, #13808, #32758, #39657, #21461, #6840, #10710, #40367, #43017, #36092, #39432, #47355, #43741, #36805, #47105, #14295, #10946, #6611, #7090, #3249, #25565, #118, #29435, #7334, #40137, #21715, #21950, #28939, #14528, #25315, #3003, #36347, #11182, #25795, #7556, #22166, #10224, #24830, #21225, #4662, #30582, #45146, #22891, #4904, #15483, #37262, #40836, #23378, #5139, #33238, #4415, #821, #44667, #29668, #37746, #15015, #19525, #33943, #37985, #26273, #23132, #11883, #1307, #26742, #30127, #37504, #15962, #365, #26024, #19045, #44207, #11406, #8028, #34174, #33712, #40599, #18812, #41068, #7793, #8502, #41301, #589, #12366, #8266, #26984, #29890, #1066, #22410, #41535, #15724, #8742, #37036, #30360, #44435, #4185, #11650, #44908, #12121, #22657, #6724, #39073, #10591, #6484, #10344, #5375, #17514, #21340, #46740, #42654, #32149, #24953, #27228, #24481, #19765, #10099, #20869, #2878, #43138, #6245, #12607, #35513, #2651, #23603, #17284, #3127, #46980, #38215, #46501, #35971, #32404, #13927, #39551, #17758, #14173, #35742, #13463, #28818, #25188, #9868, #43381, #28321, #39310, #24709, #39775, #30822, #19996, #34398, #28571, #45392, #1538, #42888, #2417, #41781, #16191, #8982, #35280, #17047, #31688, #21104, #46268, #14883, #41178, #14641, #18689, #3613, #29771, #11060, #22766, #30006, #18231, #8142, #19167, #33824, #29543, #7670, #33585, #32874, #4075, #26388, #8380, #4529, #25677, #33114, #18603, #40485, #22286, #29312, #239, #43859, #11769, #44095, #40252, #36922, #15603, #7440, #22058, #11290, #11523, #12005, #33348, #698, #36683, #18925, #15356, #25902, #44551, #26142, #40948, #944, #471, #44320, #3843, #37373, #40713, #30240, #44790, #26625, #36457, #15126, #7912, #22527, #18464, #37144, #4293, #42138, #5739, #20356, #16076, #41659, #20115, #4780, #38100, #12950, #42385, #38572, #12238, #19647, #19406, #27112, #8865, #34058, #34292, #15845, #45741, #1417, #1186, #23497, #2138, #37622, #45023, #45266, #45499, #45980, #5262, #34762, #26862, #5502, #1905, #30701, #16541, #12724, #31168, #34993, #19881, #30939, #8620, #27589, #27353, #9348, #16765, #23968, #13189, #34510, #12487, #1663, #27825, #41422, #16310, #31405, #23010, #23257, #30468, #41896, #37872, #9105, #5026, #23725, #38330, #43329, #35911, #17233, #6669, #14116, #16999, #13631, #9584, #46682, #10046, #39495, #32346, #28270, #2363, #24663, #42833, #13415, #39258, #39718, #36163, #28047, #6433, #10530, #21525, #21286, #46927, #25127, #3317, #24898, #2600, #17930, #14355, #31869, #6903, #21049, #28513, #13871, #28759, #20584, #9821, #32585, #3068, #35230, #24203, #46449, #39027, #31639, #5965, #46215, #17698, #42607, #47171, #35691, #2826, #35458, #29002, #24426, #17460, #38806, #32093, #6195, #20819, #43086, #10289, #638, #7151, #43800, #33522, #40652, #21774, #43560, #18405 ) ),
 .UNSPECIFIED., .F., .F., .T. ) 
 B_SPLINE_SURFACE_WITH_KNOTS ( ( 2, 2 ),
 ( 3, 2, 2, 2, 2, 2, 2, 2, 2, 2, 2, 2, 2, 2, 2, 2, 2, 2, 2, 2, 2, 2, 2, 2, 2, 2, 2, 2, 2, 2, 2, 2, 2, 2, 2, 2, 2, 2, 2, 2, 2, 2, 2, 2, 2, 2, 2, 2, 2, 2, 2, 2, 2, 2, 2, 2, 2, 2, 2, 2, 2, 2, 2, 2, 2, 2, 2, 2, 2, 2, 2, 2, 2, 2, 2, 2, 2, 2, 2, 2, 2, 2, 2, 2, 2, 2, 2, 2, 2, 2, 2, 2, 2, 2, 2, 2, 2, 2, 2, 2, 2, 2, 2, 2, 2, 2, 2, 2, 2, 2, 2, 2, 2, 2, 2, 2, 2, 2, 2, 2, 2, 2, 2, 2, 2, 2, 2, 2, 2, 2, 2, 2, 2, 2, 2, 2, 2, 2, 2, 2, 2, 2, 2, 2, 2, 2, 2, 2, 2, 2, 2, 2, 2, 2, 2, 2, 2, 2, 2, 2, 2, 2, 2, 2, 2, 2, 2, 2, 2, 2, 2, 2, 2, 2, 2, 2, 2, 2, 2, 2, 2, 2, 2, 2, 2, 2, 2, 2, 2, 2, 2, 2, 2, 2, 2, 2, 2, 2, 2, 2, 2, 2, 2, 2, 2, 2, 2, 2, 2, 2, 2, 2, 2, 2, 2, 2, 2, 2, 2, 2, 2, 2, 2, 2, 2, 2, 2, 2, 2, 2, 2, 2, 2, 2, 2, 2, 2, 2, 2, 2, 2, 2, 2, 2, 2, 2, 2, 2, 2, 2, 2, 2, 2, 2, 2, 2, 2, 2, 2, 2, 2, 2, 2, 2, 2, 2, 2, 2, 2, 2, 2, 2, 2, 2, 2, 2, 2, 2, 2, 2, 2, 2, 2, 2, 2, 2, 2, 2, 2, 2, 2, 2, 2, 2, 2, 2, 2, 2, 2, 2, 2, 2, 2, 2, 2, 2, 2, 2, 2, 2, 2, 2, 2, 2, 2, 2, 2, 2, 2, 2, 2, 2, 2, 2, 2, 2, 2, 2, 2, 2, 2, 2, 2, 2, 2, 2, 2, 2, 2, 2, 2, 2, 2, 2, 2, 2, 2, 2, 2, 2, 2, 2, 2, 2, 2, 2, 2, 2, 2, 2, 2, 2, 2, 2, 2, 2, 2, 2, 2, 2, 2, 2, 2, 2, 2, 2, 2, 2, 2, 2, 2, 2, 2, 2, 2, 2, 2, 2, 2, 2, 2, 2, 2, 2, 2, 2, 2, 2, 2, 2, 3 ),
 ( 0.000000000000000000, 1.000000000000000000 ),
 ( 0.000000000000000000, 0.002500000000000000052, 0.005000000000000000104, 0.007499999999999999722, 0.01000000000000000021, 0.01250000000000000069, 0.01499999999999999944, 0.01750000000000000167, 0.02000000000000000042, 0.02249999999999999917, 0.02500000000000000139, 0.02750000000000000014, 0.02999999999999999889, 0.03250000000000000111, 0.03500000000000000333, 0.03749999999999999861, 0.04000000000000000083, 0.04250000000000000305, 0.04499999999999999833, 0.04750000000000000056, 0.05000000000000000278, 0.05249999999999999806, 0.05500000000000000028, 0.05750000000000000250, 0.05999999999999999778, 0.06250000000000000000, 0.06500000000000000222, 0.06750000000000000444, 0.07000000000000000666, 0.07249999999999999500, 0.07499999999999999722, 0.07749999999999999944, 0.08000000000000000167, 0.08250000000000000389, 0.08500000000000000611, 0.08749999999999999445, 0.08999999999999999667, 0.09249999999999999889, 0.09500000000000000111, 0.09750000000000000333, 0.1000000000000000056, 0.1024999999999999939, 0.1049999999999999961, 0.1074999999999999983, 0.1100000000000000006, 0.1125000000000000028, 0.1150000000000000050, 0.1174999999999999933, 0.1199999999999999956, 0.1224999999999999978, 0.1250000000000000000, 0.1275000000000000022, 0.1300000000000000044, 0.1325000000000000067, 0.1350000000000000089, 0.1375000000000000111, 0.1400000000000000133, 0.1424999999999999878, 0.1449999999999999900, 0.1474999999999999922, 0.1499999999999999944, 0.1524999999999999967, 0.1549999999999999989, 0.1575000000000000011, 0.1600000000000000033, 0.1625000000000000056, 0.1650000000000000078, 0.1675000000000000100, 0.1700000000000000122, 0.1724999999999999867, 0.1749999999999999889, 0.1774999999999999911, 0.1799999999999999933, 0.1824999999999999956, 0.1849999999999999978, 0.1875000000000000000, 0.1900000000000000022, 0.1925000000000000044, 0.1950000000000000067, 0.1975000000000000089, 0.2000000000000000111, 0.2025000000000000133, 0.2049999999999999878, 0.2074999999999999900, 0.2099999999999999922, 0.2124999999999999944, 0.2149999999999999967, 0.2174999999999999989, 0.2200000000000000011, 0.2225000000000000033, 0.2250000000000000056, 0.2275000000000000078, 0.2300000000000000100, 0.2325000000000000122, 0.2349999999999999867, 0.2374999999999999889, 0.2399999999999999911, 0.2424999999999999933, 0.2449999999999999956, 0.2474999999999999978, 0.2500000000000000000, 0.2525000000000000022, 0.2550000000000000044, 0.2575000000000000067, 0.2600000000000000089, 0.2625000000000000111, 0.2650000000000000133, 0.2675000000000000155, 0.2700000000000000178, 0.2725000000000000200, 0.2750000000000000222, 0.2775000000000000244, 0.2800000000000000266, 0.2824999999999999734, 0.2849999999999999756, 0.2874999999999999778, 0.2899999999999999800, 0.2924999999999999822, 0.2949999999999999845, 0.2974999999999999867, 0.2999999999999999889, 0.3024999999999999911, 0.3049999999999999933, 0.3074999999999999956, 0.3099999999999999978, 0.3125000000000000000, 0.3150000000000000022, 0.3175000000000000044, 0.3200000000000000067, 0.3225000000000000089, 0.3250000000000000111, 0.3275000000000000133, 0.3300000000000000155, 0.3325000000000000178, 0.3350000000000000200, 0.3375000000000000222, 0.3400000000000000244, 0.3425000000000000266, 0.3449999999999999734, 0.3474999999999999756, 0.3499999999999999778, 0.3524999999999999800, 0.3549999999999999822, 0.3574999999999999845, 0.3599999999999999867, 0.3624999999999999889, 0.3649999999999999911, 0.3674999999999999933, 0.3699999999999999956, 0.3724999999999999978, 0.3750000000000000000, 0.3775000000000000022, 0.3800000000000000044, 0.3825000000000000067, 0.3850000000000000089, 0.3875000000000000111, 0.3900000000000000133, 0.3925000000000000155, 0.3950000000000000178, 0.3975000000000000200, 0.4000000000000000222, 0.4025000000000000244, 0.4050000000000000266, 0.4074999999999999734, 0.4099999999999999756, 0.4124999999999999778, 0.4149999999999999800, 0.4174999999999999822, 0.4199999999999999845, 0.4224999999999999867, 0.4249999999999999889, 0.4274999999999999911, 0.4299999999999999933, 0.4324999999999999956, 0.4349999999999999978, 0.4375000000000000000, 0.4400000000000000022, 0.4425000000000000044, 0.4450000000000000067, 0.4475000000000000089, 0.4500000000000000111, 0.4525000000000000133, 0.4550000000000000155, 0.4575000000000000178, 0.4600000000000000200, 0.4625000000000000222, 0.4650000000000000244, 0.4675000000000000266, 0.4699999999999999734, 0.4724999999999999756, 0.4749999999999999778, 0.4774999999999999800, 0.4799999999999999822, 0.4824999999999999845, 0.4849999999999999867, 0.4874999999999999889, 0.4899999999999999911, 0.4924999999999999933, 0.4949999999999999956, 0.4974999999999999978, 0.5000000000000000000, 0.5024999999999999467, 0.5050000000000000044, 0.5074999999999999512, 0.5100000000000000089, 0.5124999999999999556, 0.5150000000000000133, 0.5174999999999999600, 0.5200000000000000178, 0.5224999999999999645, 0.5250000000000000222, 0.5274999999999999689, 0.5300000000000000266, 0.5324999999999999734, 0.5350000000000000311, 0.5374999999999999778, 0.5400000000000000355, 0.5424999999999999822, 0.5450000000000000400, 0.5474999999999999867, 0.5500000000000000444, 0.5524999999999999911, 0.5550000000000000488, 0.5574999999999999956, 0.5600000000000000533, 0.5625000000000000000, 0.5649999999999999467, 0.5675000000000000044, 0.5699999999999999512, 0.5725000000000000089, 0.5749999999999999556, 0.5775000000000000133, 0.5799999999999999600, 0.5825000000000000178, 0.5849999999999999645, 0.5875000000000000222, 0.5899999999999999689, 0.5925000000000000266, 0.5949999999999999734, 0.5975000000000000311, 0.5999999999999999778, 0.6025000000000000355, 0.6049999999999999822, 0.6075000000000000400, 0.6099999999999999867, 0.6125000000000000444, 0.6149999999999999911, 0.6175000000000000488, 0.6199999999999999956, 0.6225000000000000533, 0.6250000000000000000, 0.6274999999999999467, 0.6300000000000000044, 0.6324999999999999512, 0.6350000000000000089, 0.6374999999999999556, 0.6400000000000000133, 0.6424999999999999600, 0.6450000000000000178, 0.6474999999999999645, 0.6500000000000000222, 0.6524999999999999689, 0.6550000000000000266, 0.6574999999999999734, 0.6600000000000000311, 0.6624999999999999778, 0.6650000000000000355, 0.6674999999999999822, 0.6700000000000000400, 0.6724999999999999867, 0.6750000000000000444, 0.6774999999999999911, 0.6800000000000000488, 0.6824999999999999956, 0.6850000000000000533, 0.6875000000000000000, 0.6899999999999999467, 0.6925000000000000044, 0.6949999999999999512, 0.6975000000000000089, 0.6999999999999999556, 0.7025000000000000133, 0.7049999999999999600, 0.7075000000000000178, 0.7099999999999999645, 0.7125000000000000222, 0.7149999999999999689, 0.7175000000000000266, 0.7199999999999999734, 0.7225000000000000311, 0.7249999999999999778, 0.7275000000000000355, 0.7299999999999999822, 0.7325000000000000400, 0.7349999999999999867, 0.7375000000000000444, 0.7399999999999999911, 0.7425000000000000488, 0.7449999999999999956, 0.7475000000000000533, 0.7500000000000000000, 0.7524999999999999467, 0.7550000000000000044, 0.7574999999999999512, 0.7600000000000000089, 0.7624999999999999556, 0.7650000000000000133, 0.7674999999999999600, 0.7700000000000000178, 0.7724999999999999645, 0.7750000000000000222, 0.7774999999999999689, 0.7800000000000000266, 0.7824999999999999734, 0.7850000000000000311, 0.7874999999999999778, 0.7900000000000000355, 0.7924999999999999822, 0.7950000000000000400, 0.7974999999999999867, 0.8000000000000000444, 0.8024999999999999911, 0.8050000000000000488, 0.8074999999999999956, 0.8100000000000000533, 0.8125000000000000000, 0.8149999999999999467, 0.8175000000000000044, 0.8199999999999999512, 0.8225000000000000089, 0.8249999999999999556, 0.8275000000000000133, 0.8299999999999999600, 0.8325000000000000178, 0.8349999999999999645, 0.8375000000000000222, 0.8399999999999999689, 0.8425000000000000266, 0.8449999999999999734, 0.8475000000000000311, 0.8499999999999999778, 0.8525000000000000355, 0.8549999999999999822, 0.8575000000000000400, 0.8599999999999999867, 0.8625000000000000444, 0.8649999999999999911, 0.8675000000000000488, 0.8699999999999999956, 0.8725000000000000533, 0.8750000000000000000, 0.8774999999999999467, 0.8800000000000000044, 0.8824999999999999512, 0.8850000000000000089, 0.8874999999999999556, 0.8900000000000000133, 0.8924999999999999600, 0.8950000000000000178, 0.8974999999999999645, 0.9000000000000000222, 0.9024999999999999689, 0.9050000000000000266, 0.9074999999999999734, 0.9100000000000000311, 0.9124999999999999778, 0.9150000000000000355, 0.9174999999999999822, 0.9200000000000000400, 0.9224999999999999867, 0.9250000000000000444, 0.9274999999999999911, 0.9300000000000000488, 0.9324999999999999956, 0.9350000000000000533, 0.9375000000000000000, 0.9399999999999999467, 0.9425000000000000044, 0.9449999999999999512, 0.9475000000000000089, 0.9499999999999999556, 0.9525000000000000133, 0.9549999999999999600, 0.9575000000000000178, 0.9599999999999999645, 0.9625000000000000222, 0.9649999999999999689, 0.9675000000000000266, 0.9699999999999999734, 0.9725000000000000311, 0.9749999999999999778, 0.9775000000000000355, 0.9799999999999999822, 0.9825000000000000400, 0.9849999999999999867, 0.9875000000000000444, 0.9899999999999999911, 0.9925000000000000488, 0.9949999999999999956, 0.9975000000000000533, 1.000000000000000000 ),
 .UNSPECIFIED. ) 
 GEOMETRIC_REPRESENTATION_ITEM ( )  RATIONAL_B_SPLINE_SURFACE ( (
 ( 1.000000000000000000, 0.9238795325112869605, 1.000000000000000000, 0.9238795325112869605, 1.000000000000000000, 0.9238795325112869605, 1.000000000000000000, 0.9238795325112869605, 1.000000000000000000, 0.9238795325112869605, 1.000000000000000000, 0.9238795325112869605, 1.000000000000000000, 0.9238795325112869605, 1.000000000000000000, 0.9238795325112869605, 1.000000000000000000, 0.9238795325112869605, 1.000000000000000000, 0.9238795325112869605, 1.000000000000000000, 0.9238795325112869605, 1.000000000000000000, 0.9238795325112869605, 1.000000000000000000, 0.9238795325112869605, 1.000000000000000000, 0.9238795325112869605, 1.000000000000000000, 0.9238795325112869605, 1.000000000000000000, 0.9238795325112869605, 1.000000000000000000, 0.9238795325112869605, 1.000000000000000000, 0.9238795325112869605, 1.000000000000000000, 0.9238795325112869605, 1.000000000000000000, 0.9238795325112869605, 1.000000000000000000, 0.9238795325112869605, 1.000000000000000000, 0.9238795325112869605, 1.000000000000000000, 0.9238795325112869605, 1.000000000000000000, 0.9238795325112869605, 1.000000000000000000, 0.9238795325112869605, 1.000000000000000000, 0.9238795325112869605, 1.000000000000000000, 0.9238795325112869605, 1.000000000000000000, 0.9238795325112869605, 1.000000000000000000, 0.9238795325112869605, 1.000000000000000000, 0.9238795325112869605, 1.000000000000000000, 0.9238795325112869605, 1.000000000000000000, 0.9238795325112869605, 1.000000000000000000, 0.9238795325112869605, 1.000000000000000000, 0.9238795325112869605, 1.000000000000000000, 0.9238795325112869605, 1.000000000000000000, 0.9238795325112869605, 1.000000000000000000, 0.9238795325112869605, 1.000000000000000000, 0.9238795325112869605, 1.000000000000000000, 0.9238795325112869605, 1.000000000000000000, 0.9238795325112869605, 1.000000000000000000, 0.9238795325112869605, 1.000000000000000000, 0.9238795325112869605, 1.000000000000000000, 0.9238795325112869605, 1.000000000000000000, 0.9238795325112869605, 1.000000000000000000, 0.9238795325112869605, 1.000000000000000000, 0.9238795325112869605, 1.000000000000000000, 0.9238795325112869605, 1.000000000000000000, 0.9238795325112869605, 1.000000000000000000, 0.9238795325112869605, 1.000000000000000000, 0.9238795325112869605, 1.000000000000000000, 0.9238795325112869605, 1.000000000000000000, 0.9238795325112869605, 1.000000000000000000, 0.9238795325112869605, 1.000000000000000000, 0.9238795325112869605, 1.000000000000000000, 0.9238795325112869605, 1.000000000000000000, 0.9238795325112869605, 1.000000000000000000, 0.9238795325112869605, 1.000000000000000000, 0.9238795325112869605, 1.000000000000000000, 0.9238795325112869605, 1.000000000000000000, 0.9238795325112869605, 1.000000000000000000, 0.9238795325112869605, 1.000000000000000000, 0.9238795325112869605, 1.000000000000000000, 0.9238795325112869605, 1.000000000000000000, 0.9238795325112869605, 1.000000000000000000, 0.9238795325112869605, 1.000000000000000000, 0.9238795325112869605, 1.000000000000000000, 0.9238795325112869605, 1.000000000000000000, 0.9238795325112869605, 1.000000000000000000, 0.9238795325112869605, 1.000000000000000000, 0.9238795325112869605, 1.000000000000000000, 0.9238795325112869605, 1.000000000000000000, 0.9238795325112869605, 1.000000000000000000, 0.9238795325112869605, 1.000000000000000000, 0.9238795325112869605, 1.000000000000000000, 0.9238795325112869605, 1.000000000000000000, 0.9238795325112869605, 1.000000000000000000, 0.9238795325112869605, 1.000000000000000000, 0.9238795325112869605, 1.000000000000000000, 0.9238795325112869605, 1.000000000000000000, 0.9238795325112869605, 1.000000000000000000, 0.9238795325112869605, 1.000000000000000000, 0.9238795325112869605, 1.000000000000000000, 0.9238795325112869605, 1.000000000000000000, 0.9238795325112869605, 1.000000000000000000, 0.9238795325112869605, 1.000000000000000000, 0.9238795325112869605, 1.000000000000000000, 0.9238795325112869605, 1.000000000000000000, 0.9238795325112869605, 1.000000000000000000, 0.9238795325112869605, 1.000000000000000000, 0.9238795325112869605, 1.000000000000000000, 0.9238795325112869605, 1.000000000000000000, 0.9238795325112869605, 1.000000000000000000, 0.9238795325112869605, 1.000000000000000000, 0.9238795325112869605, 1.000000000000000000, 0.9238795325112869605, 1.000000000000000000, 0.9238795325112869605, 1.000000000000000000, 0.9238795325112869605, 1.000000000000000000, 0.9238795325112869605, 1.000000000000000000, 0.9238795325112869605, 1.000000000000000000, 0.9238795325112869605, 1.000000000000000000, 0.9238795325112869605, 1.000000000000000000, 0.9238795325112869605, 1.000000000000000000, 0.9238795325112869605, 1.000000000000000000, 0.9238795325112869605, 1.000000000000000000, 0.9238795325112869605, 1.000000000000000000, 0.9238795325112869605, 1.000000000000000000, 0.9238795325112869605, 1.000000000000000000, 0.9238795325112869605, 1.000000000000000000, 0.9238795325112869605, 1.000000000000000000, 0.9238795325112869605, 1.000000000000000000, 0.9238795325112869605, 1.000000000000000000, 0.9238795325112869605, 1.000000000000000000, 0.9238795325112869605, 1.000000000000000000, 0.9238795325112869605, 1.000000000000000000, 0.9238795325112869605, 1.000000000000000000, 0.9238795325112869605, 1.000000000000000000, 0.9238795325112869605, 1.000000000000000000, 0.9238795325112869605, 1.000000000000000000, 0.9238795325112869605, 1.000000000000000000, 0.9238795325112869605, 1.000000000000000000, 0.9238795325112869605, 1.000000000000000000, 0.9238795325112869605, 1.000000000000000000, 0.9238795325112869605, 1.000000000000000000, 0.9238795325112869605, 1.000000000000000000, 0.9238795325112869605, 1.000000000000000000, 0.9238795325112869605, 1.000000000000000000, 0.9238795325112869605, 1.000000000000000000, 0.9238795325112869605, 1.000000000000000000, 0.9238795325112869605, 1.000000000000000000, 0.9238795325112869605, 1.000000000000000000, 0.9238795325112869605, 1.000000000000000000, 0.9238795325112869605, 1.000000000000000000, 0.9238795325112869605, 1.000000000000000000, 0.9238795325112869605, 1.000000000000000000, 0.9238795325112869605, 1.000000000000000000, 0.9238795325112869605, 1.000000000000000000, 0.9238795325112869605, 1.000000000000000000, 0.9238795325112869605, 1.000000000000000000, 0.9238795325112869605, 1.000000000000000000, 0.9238795325112869605, 1.000000000000000000, 0.9238795325112869605, 1.000000000000000000, 0.9238795325112869605, 1.000000000000000000, 0.9238795325112869605, 1.000000000000000000, 0.9238795325112869605, 1.000000000000000000, 0.9238795325112869605, 1.000000000000000000, 0.9238795325112869605, 1.000000000000000000, 0.9238795325112869605, 1.000000000000000000, 0.9238795325112869605, 1.000000000000000000, 0.9238795325112869605, 1.000000000000000000, 0.9238795325112869605, 1.000000000000000000, 0.9238795325112869605, 1.000000000000000000, 0.9238795325112869605, 1.000000000000000000, 0.9238795325112869605, 1.000000000000000000, 0.9238795325112869605, 1.000000000000000000, 0.9238795325112869605, 1.000000000000000000, 0.9238795325112869605, 1.000000000000000000, 0.9238795325112869605, 1.000000000000000000, 0.9238795325112869605, 1.000000000000000000, 0.9238795325112869605, 1.000000000000000000, 0.9238795325112869605, 1.000000000000000000, 0.9238795325112869605, 1.000000000000000000, 0.9238795325112869605, 1.000000000000000000, 0.9238795325112869605, 1.000000000000000000, 0.9238795325112869605, 1.000000000000000000, 0.9238795325112869605, 1.000000000000000000, 0.9238795325112869605, 1.000000000000000000, 0.9238795325112869605, 1.000000000000000000, 0.9238795325112869605, 1.000000000000000000, 0.9238795325112869605, 1.000000000000000000, 0.9238795325112869605, 1.000000000000000000, 0.9238795325112869605, 1.000000000000000000, 0.9238795325112869605, 1.000000000000000000, 0.9238795325112869605, 1.000000000000000000, 0.9238795325112869605, 1.000000000000000000, 0.9238795325112869605, 1.000000000000000000, 0.9238795325112869605, 1.000000000000000000, 0.9238795325112869605, 1.000000000000000000, 0.9238795325112869605, 1.000000000000000000, 0.9238795325112869605, 1.000000000000000000, 0.9238795325112869605, 1.000000000000000000, 0.9238795325112869605, 1.000000000000000000, 0.9238795325112869605, 1.000000000000000000, 0.9238795325112869605, 1.000000000000000000, 0.9238795325112869605, 1.000000000000000000, 0.9238795325112869605, 1.000000000000000000, 0.9238795325112869605, 1.000000000000000000, 0.9238795325112869605, 1.000000000000000000, 0.9238795325112869605, 1.000000000000000000, 0.9238795325112869605, 1.000000000000000000, 0.9238795325112869605, 1.000000000000000000, 0.9238795325112869605, 1.000000000000000000, 0.9238795325112869605, 1.000000000000000000, 0.9238795325112869605, 1.000000000000000000, 0.9238795325112869605, 1.000000000000000000, 0.9238795325112869605, 1.000000000000000000, 0.9238795325112869605, 1.000000000000000000, 0.9238795325112869605, 1.000000000000000000, 0.9238795325112869605, 1.000000000000000000, 0.9238795325112869605, 1.000000000000000000, 0.9238795325112869605, 1.000000000000000000, 0.9238795325112869605, 1.000000000000000000, 0.9238795325112869605, 1.000000000000000000, 0.9238795325112869605, 1.000000000000000000, 0.9238795325112869605, 1.000000000000000000, 0.9238795325112869605, 1.000000000000000000, 0.9238795325112869605, 1.000000000000000000, 0.9238795325112869605, 1.000000000000000000, 0.9238795325112869605, 1.000000000000000000, 0.9238795325112869605, 1.000000000000000000, 0.9238795325112869605, 1.000000000000000000, 0.9238795325112869605, 1.000000000000000000, 0.9238795325112869605, 1.000000000000000000, 0.9238795325112869605, 1.000000000000000000, 0.9238795325112869605, 1.000000000000000000, 0.9238795325112869605, 1.000000000000000000, 0.9238795325112869605, 1.000000000000000000, 0.9238795325112869605, 1.000000000000000000, 0.9238795325112869605, 1.000000000000000000, 0.9238795325112869605, 1.000000000000000000, 0.9238795325112869605, 1.000000000000000000, 0.9238795325112869605, 1.000000000000000000, 0.9238795325112869605, 1.000000000000000000, 0.9238795325112869605, 1.000000000000000000, 0.9238795325112869605, 1.000000000000000000, 0.9238795325112869605, 1.000000000000000000, 0.9238795325112869605, 1.000000000000000000, 0.9238795325112869605, 1.000000000000000000, 0.9238795325112869605, 1.000000000000000000, 0.9238795325112869605, 1.000000000000000000, 0.9238795325112869605, 1.000000000000000000, 0.9238795325112869605, 1.000000000000000000, 0.9238795325112869605, 1.000000000000000000, 0.9238795325112869605, 1.000000000000000000, 0.9238795325112869605, 1.000000000000000000, 0.9238795325112869605, 1.000000000000000000, 0.9238795325112869605, 1.000000000000000000, 0.9238795325112869605, 1.000000000000000000, 0.9238795325112869605, 1.000000000000000000, 0.9238795325112869605, 1.000000000000000000, 0.9238795325112869605, 1.000000000000000000, 0.9238795325112869605, 1.000000000000000000, 0.9238795325112869605, 1.000000000000000000, 0.9238795325112869605, 1.000000000000000000, 0.9238795325112869605, 1.000000000000000000, 0.9238795325112869605, 1.000000000000000000, 0.9238795325112869605, 1.000000000000000000, 0.9238795325112869605, 1.000000000000000000, 0.9238795325112869605, 1.000000000000000000, 0.9238795325112869605, 1.000000000000000000, 0.9238795325112869605, 1.000000000000000000, 0.9238795325112869605, 1.000000000000000000, 0.9238795325112869605, 1.000000000000000000, 0.9238795325112869605, 1.000000000000000000, 0.9238795325112869605, 1.000000000000000000, 0.9238795325112869605, 1.000000000000000000, 0.9238795325112869605, 1.000000000000000000, 0.9238795325112869605, 1.000000000000000000, 0.9238795325112869605, 1.000000000000000000, 0.9238795325112869605, 1.000000000000000000, 0.9238795325112869605, 1.000000000000000000, 0.9238795325112869605, 1.000000000000000000, 0.9238795325112869605, 1.000000000000000000, 0.9238795325112869605, 1.000000000000000000, 0.9238795325112869605, 1.000000000000000000, 0.9238795325112869605, 1.000000000000000000, 0.9238795325112869605, 1.000000000000000000, 0.9238795325112869605, 1.000000000000000000, 0.9238795325112869605, 1.000000000000000000, 0.9238795325112869605, 1.000000000000000000, 0.9238795325112869605, 1.000000000000000000, 0.9238795325112869605, 1.000000000000000000, 0.9238795325112869605, 1.000000000000000000, 0.9238795325112869605, 1.000000000000000000, 0.9238795325112869605, 1.000000000000000000, 0.9238795325112869605, 1.000000000000000000, 0.9238795325112869605, 1.000000000000000000, 0.9238795325112869605, 1.000000000000000000, 0.9238795325112869605, 1.000000000000000000, 0.9238795325112869605, 1.000000000000000000, 0.9238795325112869605, 1.000000000000000000, 0.9238795325112869605, 1.000000000000000000, 0.9238795325112869605, 1.000000000000000000, 0.9238795325112869605, 1.000000000000000000, 0.9238795325112869605, 1.000000000000000000, 0.9238795325112869605, 1.000000000000000000, 0.9238795325112869605, 1.000000000000000000, 0.9238795325112869605, 1.000000000000000000, 0.9238795325112869605, 1.000000000000000000, 0.9238795325112869605, 1.000000000000000000, 0.9238795325112869605, 1.000000000000000000, 0.9238795325112869605, 1.000000000000000000, 0.9238795325112869605, 1.000000000000000000, 0.9238795325112869605, 1.000000000000000000, 0.9238795325112869605, 1.000000000000000000, 0.9238795325112869605, 1.000000000000000000, 0.9238795325112869605, 1.000000000000000000, 0.9238795325112869605, 1.000000000000000000, 0.9238795325112869605, 1.000000000000000000, 0.9238795325112869605, 1.000000000000000000, 0.9238795325112869605, 1.000000000000000000, 0.9238795325112869605, 1.000000000000000000, 0.9238795325112869605, 1.000000000000000000, 0.9238795325112869605, 1.000000000000000000, 0.9238795325112869605, 1.000000000000000000, 0.9238795325112869605, 1.000000000000000000, 0.9238795325112869605, 1.000000000000000000, 0.9238795325112869605, 1.000000000000000000, 0.9238795325112869605, 1.000000000000000000, 0.9238795325112869605, 1.000000000000000000, 0.9238795325112869605, 1.000000000000000000, 0.9238795325112869605, 1.000000000000000000, 0.9238795325112869605, 1.000000000000000000, 0.9238795325112869605, 1.000000000000000000, 0.9238795325112869605, 1.000000000000000000, 0.9238795325112869605, 1.000000000000000000, 0.9238795325112869605, 1.000000000000000000, 0.9238795325112869605, 1.000000000000000000, 0.9238795325112869605, 1.000000000000000000, 0.9238795325112869605, 1.000000000000000000, 0.9238795325112869605, 1.000000000000000000, 0.9238795325112869605, 1.000000000000000000, 0.9238795325112869605, 1.000000000000000000, 0.9238795325112869605, 1.000000000000000000, 0.9238795325112869605, 1.000000000000000000, 0.9238795325112869605, 1.000000000000000000, 0.9238795325112869605, 1.000000000000000000, 0.9238795325112869605, 1.000000000000000000, 0.9238795325112869605, 1.000000000000000000, 0.9238795325112869605, 1.000000000000000000, 0.9238795325112869605, 1.000000000000000000, 0.9238795325112869605, 1.000000000000000000, 0.9238795325112869605, 1.000000000000000000, 0.9238795325112869605, 1.000000000000000000, 0.9238795325112869605, 1.000000000000000000, 0.9238795325112869605, 1.000000000000000000, 0.9238795325112869605, 1.000000000000000000, 0.9238795325112869605, 1.000000000000000000, 0.9238795325112869605, 1.000000000000000000, 0.9238795325112869605, 1.000000000000000000, 0.9238795325112869605, 1.000000000000000000, 0.9238795325112869605, 1.000000000000000000, 0.9238795325112869605, 1.000000000000000000, 0.9238795325112869605, 1.000000000000000000, 0.9238795325112869605, 1.000000000000000000, 0.9238795325112869605, 1.000000000000000000, 0.9238795325112869605, 1.000000000000000000, 0.9238795325112869605, 1.000000000000000000, 0.9238795325112869605, 1.000000000000000000, 0.9238795325112869605, 1.000000000000000000, 0.9238795325112869605, 1.000000000000000000, 0.9238795325112869605, 1.000000000000000000, 0.9238795325112869605, 1.000000000000000000, 0.9238795325112869605, 1.000000000000000000, 0.9238795325112869605, 1.000000000000000000, 0.9238795325112869605, 1.000000000000000000, 0.9238795325112869605, 1.000000000000000000, 0.9238795325112869605, 1.000000000000000000, 0.9238795325112869605, 1.000000000000000000, 0.9238795325112869605, 1.000000000000000000, 0.9238795325112869605, 1.000000000000000000, 0.9238795325112869605, 1.000000000000000000, 0.9238795325112869605, 1.000000000000000000, 0.9238795325112869605, 1.000000000000000000, 0.9238795325112869605, 1.000000000000000000, 0.9238795325112869605, 1.000000000000000000, 0.9238795325112869605, 1.000000000000000000, 0.9238795325112869605, 1.000000000000000000, 0.9238795325112869605, 1.000000000000000000, 0.9238795325112869605, 1.000000000000000000, 0.9238795325112869605, 1.000000000000000000, 0.9238795325112869605, 1.000000000000000000, 0.9238795325112869605, 1.000000000000000000, 0.9238795325112869605, 1.000000000000000000, 0.9238795325112869605, 1.000000000000000000, 0.9238795325112869605, 1.000000000000000000, 0.9238795325112869605, 1.000000000000000000, 0.9238795325112869605, 1.000000000000000000, 0.9238795325112869605, 1.000000000000000000, 0.9238795325112869605, 1.000000000000000000, 0.9238795325112869605, 1.000000000000000000, 0.9238795325112869605, 1.000000000000000000, 0.9238795325112869605, 1.000000000000000000, 0.9238795325112869605, 1.000000000000000000, 0.9238795325112869605, 1.000000000000000000, 0.9238795325112869605, 1.000000000000000000, 0.9238795325112869605, 1.000000000000000000, 0.9238795325112869605, 1.000000000000000000, 0.9238795325112869605, 1.000000000000000000, 0.9238795325112869605, 1.000000000000000000, 0.9238795325112869605, 1.000000000000000000, 0.9238795325112869605, 1.000000000000000000, 0.9238795325112869605, 1.000000000000000000, 0.9238795325112869605, 1.000000000000000000, 0.9238795325112869605, 1.000000000000000000, 0.9238795325112869605, 1.000000000000000000, 0.9238795325112869605, 1.000000000000000000, 0.9238795325112869605, 1.000000000000000000, 0.9238795325112869605, 1.000000000000000000, 0.9238795325112869605, 1.000000000000000000, 0.9238795325112869605, 1.000000000000000000),
 ( 1.000000000000000000, 0.9238795325112869605, 1.000000000000000000, 0.9238795325112869605, 1.000000000000000000, 0.9238795325112869605, 1.000000000000000000, 0.9238795325112869605, 1.000000000000000000, 0.9238795325112869605, 1.000000000000000000, 0.9238795325112869605, 1.000000000000000000, 0.9238795325112869605, 1.000000000000000000, 0.9238795325112869605, 1.000000000000000000, 0.9238795325112869605, 1.000000000000000000, 0.9238795325112869605, 1.000000000000000000, 0.9238795325112869605, 1.000000000000000000, 0.9238795325112869605, 1.000000000000000000, 0.9238795325112869605, 1.000000000000000000, 0.9238795325112869605, 1.000000000000000000, 0.9238795325112869605, 1.000000000000000000, 0.9238795325112869605, 1.000000000000000000, 0.9238795325112869605, 1.000000000000000000, 0.9238795325112869605, 1.000000000000000000, 0.9238795325112869605, 1.000000000000000000, 0.9238795325112869605, 1.000000000000000000, 0.9238795325112869605, 1.000000000000000000, 0.9238795325112869605, 1.000000000000000000, 0.9238795325112869605, 1.000000000000000000, 0.9238795325112869605, 1.000000000000000000, 0.9238795325112869605, 1.000000000000000000, 0.9238795325112869605, 1.000000000000000000, 0.9238795325112869605, 1.000000000000000000, 0.9238795325112869605, 1.000000000000000000, 0.9238795325112869605, 1.000000000000000000, 0.9238795325112869605, 1.000000000000000000, 0.9238795325112869605, 1.000000000000000000, 0.9238795325112869605, 1.000000000000000000, 0.9238795325112869605, 1.000000000000000000, 0.9238795325112869605, 1.000000000000000000, 0.9238795325112869605, 1.000000000000000000, 0.9238795325112869605, 1.000000000000000000, 0.9238795325112869605, 1.000000000000000000, 0.9238795325112869605, 1.000000000000000000, 0.9238795325112869605, 1.000000000000000000, 0.9238795325112869605, 1.000000000000000000, 0.9238795325112869605, 1.000000000000000000, 0.9238795325112869605, 1.000000000000000000, 0.9238795325112869605, 1.000000000000000000, 0.9238795325112869605, 1.000000000000000000, 0.9238795325112869605, 1.000000000000000000, 0.9238795325112869605, 1.000000000000000000, 0.9238795325112869605, 1.000000000000000000, 0.9238795325112869605, 1.000000000000000000, 0.9238795325112869605, 1.000000000000000000, 0.9238795325112869605, 1.000000000000000000, 0.9238795325112869605, 1.000000000000000000, 0.9238795325112869605, 1.000000000000000000, 0.9238795325112869605, 1.000000000000000000, 0.9238795325112869605, 1.000000000000000000, 0.9238795325112869605, 1.000000000000000000, 0.9238795325112869605, 1.000000000000000000, 0.9238795325112869605, 1.000000000000000000, 0.9238795325112869605, 1.000000000000000000, 0.9238795325112869605, 1.000000000000000000, 0.9238795325112869605, 1.000000000000000000, 0.9238795325112869605, 1.000000000000000000, 0.9238795325112869605, 1.000000000000000000, 0.9238795325112869605, 1.000000000000000000, 0.9238795325112869605, 1.000000000000000000, 0.9238795325112869605, 1.000000000000000000, 0.9238795325112869605, 1.000000000000000000, 0.9238795325112869605, 1.000000000000000000, 0.9238795325112869605, 1.000000000000000000, 0.9238795325112869605, 1.000000000000000000, 0.9238795325112869605, 1.000000000000000000, 0.9238795325112869605, 1.000000000000000000, 0.9238795325112869605, 1.000000000000000000, 0.9238795325112869605, 1.000000000000000000, 0.9238795325112869605, 1.000000000000000000, 0.9238795325112869605, 1.000000000000000000, 0.9238795325112869605, 1.000000000000000000, 0.9238795325112869605, 1.000000000000000000, 0.9238795325112869605, 1.000000000000000000, 0.9238795325112869605, 1.000000000000000000, 0.9238795325112869605, 1.000000000000000000, 0.9238795325112869605, 1.000000000000000000, 0.9238795325112869605, 1.000000000000000000, 0.9238795325112869605, 1.000000000000000000, 0.9238795325112869605, 1.000000000000000000, 0.9238795325112869605, 1.000000000000000000, 0.9238795325112869605, 1.000000000000000000, 0.9238795325112869605, 1.000000000000000000, 0.9238795325112869605, 1.000000000000000000, 0.9238795325112869605, 1.000000000000000000, 0.9238795325112869605, 1.000000000000000000, 0.9238795325112869605, 1.000000000000000000, 0.9238795325112869605, 1.000000000000000000, 0.9238795325112869605, 1.000000000000000000, 0.9238795325112869605, 1.000000000000000000, 0.9238795325112869605, 1.000000000000000000, 0.9238795325112869605, 1.000000000000000000, 0.9238795325112869605, 1.000000000000000000, 0.9238795325112869605, 1.000000000000000000, 0.9238795325112869605, 1.000000000000000000, 0.9238795325112869605, 1.000000000000000000, 0.9238795325112869605, 1.000000000000000000, 0.9238795325112869605, 1.000000000000000000, 0.9238795325112869605, 1.000000000000000000, 0.9238795325112869605, 1.000000000000000000, 0.9238795325112869605, 1.000000000000000000, 0.9238795325112869605, 1.000000000000000000, 0.9238795325112869605, 1.000000000000000000, 0.9238795325112869605, 1.000000000000000000, 0.9238795325112869605, 1.000000000000000000, 0.9238795325112869605, 1.000000000000000000, 0.9238795325112869605, 1.000000000000000000, 0.9238795325112869605, 1.000000000000000000, 0.9238795325112869605, 1.000000000000000000, 0.9238795325112869605, 1.000000000000000000, 0.9238795325112869605, 1.000000000000000000, 0.9238795325112869605, 1.000000000000000000, 0.9238795325112869605, 1.000000000000000000, 0.9238795325112869605, 1.000000000000000000, 0.9238795325112869605, 1.000000000000000000, 0.9238795325112869605, 1.000000000000000000, 0.9238795325112869605, 1.000000000000000000, 0.9238795325112869605, 1.000000000000000000, 0.9238795325112869605, 1.000000000000000000, 0.9238795325112869605, 1.000000000000000000, 0.9238795325112869605, 1.000000000000000000, 0.9238795325112869605, 1.000000000000000000, 0.9238795325112869605, 1.000000000000000000, 0.9238795325112869605, 1.000000000000000000, 0.9238795325112869605, 1.000000000000000000, 0.9238795325112869605, 1.000000000000000000, 0.9238795325112869605, 1.000000000000000000, 0.9238795325112869605, 1.000000000000000000, 0.9238795325112869605, 1.000000000000000000, 0.9238795325112869605, 1.000000000000000000, 0.9238795325112869605, 1.000000000000000000, 0.9238795325112869605, 1.000000000000000000, 0.9238795325112869605, 1.000000000000000000, 0.9238795325112869605, 1.000000000000000000, 0.9238795325112869605, 1.000000000000000000, 0.9238795325112869605, 1.000000000000000000, 0.9238795325112869605, 1.000000000000000000, 0.9238795325112869605, 1.000000000000000000, 0.9238795325112869605, 1.000000000000000000, 0.9238795325112869605, 1.000000000000000000, 0.9238795325112869605, 1.000000000000000000, 0.9238795325112869605, 1.000000000000000000, 0.9238795325112869605, 1.000000000000000000, 0.9238795325112869605, 1.000000000000000000, 0.9238795325112869605, 1.000000000000000000, 0.9238795325112869605, 1.000000000000000000, 0.9238795325112869605, 1.000000000000000000, 0.9238795325112869605, 1.000000000000000000, 0.9238795325112869605, 1.000000000000000000, 0.9238795325112869605, 1.000000000000000000, 0.9238795325112869605, 1.000000000000000000, 0.9238795325112869605, 1.000000000000000000, 0.9238795325112869605, 1.000000000000000000, 0.9238795325112869605, 1.000000000000000000, 0.9238795325112869605, 1.000000000000000000, 0.9238795325112869605, 1.000000000000000000, 0.9238795325112869605, 1.000000000000000000, 0.9238795325112869605, 1.000000000000000000, 0.9238795325112869605, 1.000000000000000000, 0.9238795325112869605, 1.000000000000000000, 0.9238795325112869605, 1.000000000000000000, 0.9238795325112869605, 1.000000000000000000, 0.9238795325112869605, 1.000000000000000000, 0.9238795325112869605, 1.000000000000000000, 0.9238795325112869605, 1.000000000000000000, 0.9238795325112869605, 1.000000000000000000, 0.9238795325112869605, 1.000000000000000000, 0.9238795325112869605, 1.000000000000000000, 0.9238795325112869605, 1.000000000000000000, 0.9238795325112869605, 1.000000000000000000, 0.9238795325112869605, 1.000000000000000000, 0.9238795325112869605, 1.000000000000000000, 0.9238795325112869605, 1.000000000000000000, 0.9238795325112869605, 1.000000000000000000, 0.9238795325112869605, 1.000000000000000000, 0.9238795325112869605, 1.000000000000000000, 0.9238795325112869605, 1.000000000000000000, 0.9238795325112869605, 1.000000000000000000, 0.9238795325112869605, 1.000000000000000000, 0.9238795325112869605, 1.000000000000000000, 0.9238795325112869605, 1.000000000000000000, 0.9238795325112869605, 1.000000000000000000, 0.9238795325112869605, 1.000000000000000000, 0.9238795325112869605, 1.000000000000000000, 0.9238795325112869605, 1.000000000000000000, 0.9238795325112869605, 1.000000000000000000, 0.9238795325112869605, 1.000000000000000000, 0.9238795325112869605, 1.000000000000000000, 0.9238795325112869605, 1.000000000000000000, 0.9238795325112869605, 1.000000000000000000, 0.9238795325112869605, 1.000000000000000000, 0.9238795325112869605, 1.000000000000000000, 0.9238795325112869605, 1.000000000000000000, 0.9238795325112869605, 1.000000000000000000, 0.9238795325112869605, 1.000000000000000000, 0.9238795325112869605, 1.000000000000000000, 0.9238795325112869605, 1.000000000000000000, 0.9238795325112869605, 1.000000000000000000, 0.9238795325112869605, 1.000000000000000000, 0.9238795325112869605, 1.000000000000000000, 0.9238795325112869605, 1.000000000000000000, 0.9238795325112869605, 1.000000000000000000, 0.9238795325112869605, 1.000000000000000000, 0.9238795325112869605, 1.000000000000000000, 0.9238795325112869605, 1.000000000000000000, 0.9238795325112869605, 1.000000000000000000, 0.9238795325112869605, 1.000000000000000000, 0.9238795325112869605, 1.000000000000000000, 0.9238795325112869605, 1.000000000000000000, 0.9238795325112869605, 1.000000000000000000, 0.9238795325112869605, 1.000000000000000000, 0.9238795325112869605, 1.000000000000000000, 0.9238795325112869605, 1.000000000000000000, 0.9238795325112869605, 1.000000000000000000, 0.9238795325112869605, 1.000000000000000000, 0.9238795325112869605, 1.000000000000000000, 0.9238795325112869605, 1.000000000000000000, 0.9238795325112869605, 1.000000000000000000, 0.9238795325112869605, 1.000000000000000000, 0.9238795325112869605, 1.000000000000000000, 0.9238795325112869605, 1.000000000000000000, 0.9238795325112869605, 1.000000000000000000, 0.9238795325112869605, 1.000000000000000000, 0.9238795325112869605, 1.000000000000000000, 0.9238795325112869605, 1.000000000000000000, 0.9238795325112869605, 1.000000000000000000, 0.9238795325112869605, 1.000000000000000000, 0.9238795325112869605, 1.000000000000000000, 0.9238795325112869605, 1.000000000000000000, 0.9238795325112869605, 1.000000000000000000, 0.9238795325112869605, 1.000000000000000000, 0.9238795325112869605, 1.000000000000000000, 0.9238795325112869605, 1.000000000000000000, 0.9238795325112869605, 1.000000000000000000, 0.9238795325112869605, 1.000000000000000000, 0.9238795325112869605, 1.000000000000000000, 0.9238795325112869605, 1.000000000000000000, 0.9238795325112869605, 1.000000000000000000, 0.9238795325112869605, 1.000000000000000000, 0.9238795325112869605, 1.000000000000000000, 0.9238795325112869605, 1.000000000000000000, 0.9238795325112869605, 1.000000000000000000, 0.9238795325112869605, 1.000000000000000000, 0.9238795325112869605, 1.000000000000000000, 0.9238795325112869605, 1.000000000000000000, 0.9238795325112869605, 1.000000000000000000, 0.9238795325112869605, 1.000000000000000000, 0.9238795325112869605, 1.000000000000000000, 0.9238795325112869605, 1.000000000000000000, 0.9238795325112869605, 1.000000000000000000, 0.9238795325112869605, 1.000000000000000000, 0.9238795325112869605, 1.000000000000000000, 0.9238795325112869605, 1.000000000000000000, 0.9238795325112869605, 1.000000000000000000, 0.9238795325112869605, 1.000000000000000000, 0.9238795325112869605, 1.000000000000000000, 0.9238795325112869605, 1.000000000000000000, 0.9238795325112869605, 1.000000000000000000, 0.9238795325112869605, 1.000000000000000000, 0.9238795325112869605, 1.000000000000000000, 0.9238795325112869605, 1.000000000000000000, 0.9238795325112869605, 1.000000000000000000, 0.9238795325112869605, 1.000000000000000000, 0.9238795325112869605, 1.000000000000000000, 0.9238795325112869605, 1.000000000000000000, 0.9238795325112869605, 1.000000000000000000, 0.9238795325112869605, 1.000000000000000000, 0.9238795325112869605, 1.000000000000000000, 0.9238795325112869605, 1.000000000000000000, 0.9238795325112869605, 1.000000000000000000, 0.9238795325112869605, 1.000000000000000000, 0.9238795325112869605, 1.000000000000000000, 0.9238795325112869605, 1.000000000000000000, 0.9238795325112869605, 1.000000000000000000, 0.9238795325112869605, 1.000000000000000000, 0.9238795325112869605, 1.000000000000000000, 0.9238795325112869605, 1.000000000000000000, 0.9238795325112869605, 1.000000000000000000, 0.9238795325112869605, 1.000000000000000000, 0.9238795325112869605, 1.000000000000000000, 0.9238795325112869605, 1.000000000000000000, 0.9238795325112869605, 1.000000000000000000, 0.9238795325112869605, 1.000000000000000000, 0.9238795325112869605, 1.000000000000000000, 0.9238795325112869605, 1.000000000000000000, 0.9238795325112869605, 1.000000000000000000, 0.9238795325112869605, 1.000000000000000000, 0.9238795325112869605, 1.000000000000000000, 0.9238795325112869605, 1.000000000000000000, 0.9238795325112869605, 1.000000000000000000, 0.9238795325112869605, 1.000000000000000000, 0.9238795325112869605, 1.000000000000000000, 0.9238795325112869605, 1.000000000000000000, 0.9238795325112869605, 1.000000000000000000, 0.9238795325112869605, 1.000000000000000000, 0.9238795325112869605, 1.000000000000000000, 0.9238795325112869605, 1.000000000000000000, 0.9238795325112869605, 1.000000000000000000, 0.9238795325112869605, 1.000000000000000000, 0.9238795325112869605, 1.000000000000000000, 0.9238795325112869605, 1.000000000000000000, 0.9238795325112869605, 1.000000000000000000, 0.9238795325112869605, 1.000000000000000000, 0.9238795325112869605, 1.000000000000000000, 0.9238795325112869605, 1.000000000000000000, 0.9238795325112869605, 1.000000000000000000, 0.9238795325112869605, 1.000000000000000000, 0.9238795325112869605, 1.000000000000000000, 0.9238795325112869605, 1.000000000000000000, 0.9238795325112869605, 1.000000000000000000, 0.9238795325112869605, 1.000000000000000000, 0.9238795325112869605, 1.000000000000000000, 0.9238795325112869605, 1.000000000000000000, 0.9238795325112869605, 1.000000000000000000, 0.9238795325112869605, 1.000000000000000000, 0.9238795325112869605, 1.000000000000000000, 0.9238795325112869605, 1.000000000000000000, 0.9238795325112869605, 1.000000000000000000, 0.9238795325112869605, 1.000000000000000000, 0.9238795325112869605, 1.000000000000000000, 0.9238795325112869605, 1.000000000000000000, 0.9238795325112869605, 1.000000000000000000, 0.9238795325112869605, 1.000000000000000000, 0.9238795325112869605, 1.000000000000000000, 0.9238795325112869605, 1.000000000000000000, 0.9238795325112869605, 1.000000000000000000, 0.9238795325112869605, 1.000000000000000000, 0.9238795325112869605, 1.000000000000000000, 0.9238795325112869605, 1.000000000000000000, 0.9238795325112869605, 1.000000000000000000, 0.9238795325112869605, 1.000000000000000000, 0.9238795325112869605, 1.000000000000000000, 0.9238795325112869605, 1.000000000000000000, 0.9238795325112869605, 1.000000000000000000, 0.9238795325112869605, 1.000000000000000000, 0.9238795325112869605, 1.000000000000000000, 0.9238795325112869605, 1.000000000000000000, 0.9238795325112869605, 1.000000000000000000, 0.9238795325112869605, 1.000000000000000000, 0.9238795325112869605, 1.000000000000000000, 0.9238795325112869605, 1.000000000000000000, 0.9238795325112869605, 1.000000000000000000, 0.9238795325112869605, 1.000000000000000000, 0.9238795325112869605, 1.000000000000000000, 0.9238795325112869605, 1.000000000000000000, 0.9238795325112869605, 1.000000000000000000, 0.9238795325112869605, 1.000000000000000000, 0.9238795325112869605, 1.000000000000000000, 0.9238795325112869605, 1.000000000000000000, 0.9238795325112869605, 1.000000000000000000, 0.9238795325112869605, 1.000000000000000000, 0.9238795325112869605, 1.000000000000000000, 0.9238795325112869605, 1.000000000000000000, 0.9238795325112869605, 1.000000000000000000, 0.9238795325112869605, 1.000000000000000000, 0.9238795325112869605, 1.000000000000000000, 0.9238795325112869605, 1.000000000000000000, 0.9238795325112869605, 1.000000000000000000, 0.9238795325112869605, 1.000000000000000000, 0.9238795325112869605, 1.000000000000000000, 0.9238795325112869605, 1.000000000000000000, 0.9238795325112869605, 1.000000000000000000, 0.9238795325112869605, 1.000000000000000000, 0.9238795325112869605, 1.000000000000000000, 0.9238795325112869605, 1.000000000000000000, 0.9238795325112869605, 1.000000000000000000, 0.9238795325112869605, 1.000000000000000000, 0.9238795325112869605, 1.000000000000000000, 0.9238795325112869605, 1.000000000000000000, 0.9238795325112869605, 1.000000000000000000, 0.9238795325112869605, 1.000000000000000000, 0.9238795325112869605, 1.000000000000000000, 0.9238795325112869605, 1.000000000000000000, 0.9238795325112869605, 1.000000000000000000, 0.9238795325112869605, 1.000000000000000000, 0.9238795325112869605, 1.000000000000000000, 0.9238795325112869605, 1.000000000000000000, 0.9238795325112869605, 1.000000000000000000, 0.9238795325112869605, 1.000000000000000000, 0.9238795325112869605, 1.000000000000000000, 0.9238795325112869605, 1.000000000000000000, 0.9238795325112869605, 1.000000000000000000, 0.9238795325112869605, 1.000000000000000000, 0.9238795325112869605, 1.000000000000000000, 0.9238795325112869605, 1.000000000000000000, 0.9238795325112869605, 1.000000000000000000, 0.9238795325112869605, 1.000000000000000000, 0.9238795325112869605, 1.000000000000000000, 0.9238795325112869605, 1.000000000000000000, 0.9238795325112869605, 1.000000000000000000, 0.9238795325112869605, 1.000000000000000000, 0.9238795325112869605, 1.000000000000000000, 0.9238795325112869605, 1.000000000000000000, 0.9238795325112869605, 1.000000000000000000, 0.9238795325112869605, 1.000000000000000000, 0.9238795325112869605, 1.000000000000000000) ) ) 
 REPRESENTATION_ITEM ( '' )  SURFACE ( )  ) ;
#6087 = CARTESIAN_POINT ( 'NONE',  ( 0.9412147342319837628, -0.1574803149606297803, 1.774114173228345859 ) ) ;
#6088 = AXIS2_PLACEMENT_3D ( 'NONE', #45143, #19284, #1534 ) ;
#6089 = CARTESIAN_POINT ( 'NONE',  ( 0.1797182628040039087, -0.1412839670633605771, 0.07444174185955046430 ) ) ;
#6090 = CARTESIAN_POINT ( 'NONE',  ( 3.284318927891251994E-17, -0.7829724408911181710, 0.1787899950787401882 ) ) ;
#6091 = EDGE_CURVE ( 'NONE', #45437, #40610, #36353, .T. ) ;
#6092 = ADVANCED_FACE ( 'NONE', ( #17880 ), #14302, .T. ) ;
#6093 = CARTESIAN_POINT ( 'NONE',  ( 0.1270800023317771588, -1.236264282023989969, -0.1270800023317771588 ) ) ;
#6094 = CARTESIAN_POINT ( 'NONE',  ( -0.09240388072374362827, 0.2421448268523877234, -0.03441347972012046702 ) ) ;
#6095 = CARTESIAN_POINT ( 'NONE',  ( 0.8019270111902717657, 0.1787899950787401604, 1.062992125930488418 ) ) ;
#6096 = CARTESIAN_POINT ( 'NONE',  ( 1.002407869896990045, -0.1264236179284866091, 1.552657480261196765 ) ) ;
#6097 = CARTESIAN_POINT ( 'NONE',  ( 0.7495606340400177148, 0.1264236179284866091, 0.1943897637257641919 ) ) ;
#6098 = ADVANCED_FACE ( 'NONE', ( #43507 ), #24836, .T. ) ;
#6099 = LINE ( 'NONE', #6337, #45249 ) ;
#6100 = CARTESIAN_POINT ( 'NONE',  ( 1.033464566929134687, 0.06523048226347956391, 1.665846456692914312 ) ) ;
#6102 = DIRECTION ( 'NONE',  ( -0.8191520442889957954, 0.4519843998600397428, -0.3531289150159173662 ) ) ;
#6101 = CARTESIAN_POINT ( 'NONE',  ( 0.7185039370078739607, 1.928577636452523993E-17, 1.407480314960629864 ) ) ;
#6103 = CARTESIAN_POINT ( 'NONE',  ( 0.2944196465027555387, 4.766607801171850497E-17, 0.000000000000000000 ) ) ;
#6104 = CARTESIAN_POINT ( 'NONE',  ( -0.7185039370078739607, 1.928577636452523993E-17, 1.791338582569637738 ) ) ;
#6105 = CARTESIAN_POINT ( 'NONE',  ( -0.07405724077823318263, -0.007874015694267993623, -0.1787899950787401604 ) ) ;
#6106 = ( BOUNDED_CURVE ( )  B_SPLINE_CURVE ( 2, ( #26972, #31040, #41524, #23366, #8730, #19752, #45608, #12826, #27458 ),
 .UNSPECIFIED., .F., .T. ) 
 B_SPLINE_CURVE_WITH_KNOTS ( ( 3, 2, 2, 2, 3 ),
 ( 0.5100000000000000089, 0.5124999999999999556, 0.5150000000000000133, 0.5174999999999999600, 0.5200000000000000178 ),
 .UNSPECIFIED. ) 
 CURVE ( )  GEOMETRIC_REPRESENTATION_ITEM ( )  RATIONAL_B_SPLINE_CURVE ( ( 1.000000000000000000, 0.9238795325112869605, 1.000000000000000000, 0.9238795325112869605, 1.000000000000000000, 0.9238795325112869605, 1.000000000000000000, 0.9238795325112869605, 1.000000000000000000 ) ) 
 REPRESENTATION_ITEM ( '' )  ) ;
#6107 = CARTESIAN_POINT ( 'NONE',  ( 0.8759842519685039353, -0.1574803149606299191, 1.653543307086614345 ) ) ;
#6108 = CARTESIAN_POINT ( 'NONE',  ( 0.6971942568897637749, 2.189545951927499583E-17, 1.104822834591905556 ) ) ;
#6109 = CIRCLE ( 'NONE', #36747, 0.2471922904502826812 ) ;
#6110 = LINE ( 'NONE', #20734, #24316 ) ;
#6111 = CARTESIAN_POINT ( 'NONE',  ( 0.7646288533564489232, -0.1113553986120547346, 0.3395669290263311213 ) ) ;
#6112 = VERTEX_POINT ( 'NONE', #46868 ) ;
#6113 = CARTESIAN_POINT ( 'NONE',  ( 1.054774247047244540, -0.07405724077823318263, 1.993110236166711013 ) ) ;
#6114 = CARTESIAN_POINT ( 'NONE',  ( -0.7185039370078746268, -0.06523048226347956391, 0.2583661416247562959 ) ) ;
#6115 = EDGE_LOOP ( 'NONE', ( #13999, #18124, #21961, #42666 ) ) ;
#6116 = CARTESIAN_POINT ( 'NONE',  ( 0.9500414927467378812, -0.1787899950787401604, 1.274606299158834277 ) ) ;
#6118 = DIRECTION ( 'NONE',  ( 0.000000000000000000, 0.000000000000000000, -1.000000000000000000 ) ) ;
#6117 = DIRECTION ( 'NONE',  ( 0.000000000000000000, -0.9771240687918510970, -0.2126700594528006527 ) ) ;
#6120 = AXIS2_PLACEMENT_3D ( 'NONE', #33768, #7849, #11000 ) ;
#6119 = CARTESIAN_POINT ( 'NONE',  ( 0.1787899950787401604, -0.06200787396198446239, 0.07405724077823318263 ) ) ;
#6121 = CARTESIAN_POINT ( 'NONE',  ( -1.033464566929133799, 0.000000000000000000, 1.023622047136567126 ) ) ;
#6122 = DIRECTION ( 'NONE',  ( 0.8191520442889914655, 1.003171929053524500E-16, -0.5735764363510464925 ) ) ;
#6123 = EDGE_LOOP ( 'NONE', ( #40691, #27689, #20849, #42886 ) ) ;
#6124 = VERTEX_POINT ( 'NONE', #43273 ) ;
#6125 = CARTESIAN_POINT ( 'NONE',  ( -0.8759842519685039353, -0.1787899950787401882, 1.350885826717889815 ) ) ;
#6127 = CARTESIAN_POINT ( 'NONE',  ( -1.094772975963752103E-17, -1.668799212544661348, -0.1787899950787401882 ) ) ;
#6126 = CARTESIAN_POINT ( 'NONE',  ( 0.06523048226347956391, -0.3991141731208192045, 0.1574803149606297803 ) ) ;
#6128 = CARTESIAN_POINT ( 'NONE',  ( -1.002407869896990045, 0.1264236179284866091, 0.9768700786863937502 ) ) ;
#6129 = CARTESIAN_POINT ( 'NONE',  ( -0.7185039370078746268, 0.06523048226347956391, 0.02706692913385832025 ) ) ;
#6130 = VERTEX_POINT ( 'NONE', #25072 ) ;
#6131 = CARTESIAN_POINT ( 'NONE',  ( -1.002407869896990045, -0.1264236179284866091, 1.001476377898992132 ) ) ;
#6132 = APPLICATION_CONTEXT ( 'automotive_design' ) ;
#6133 = CARTESIAN_POINT ( 'NONE',  ( -0.8019270111902717657, -0.1787899950787401604, 0.6446850393163160442 ) ) ;
#6134 = CARTESIAN_POINT ( 'NONE',  ( -0.9873396505805591694, 0.1113553986120547346, 0.08366141721530767628 ) ) ;
#6135 = ORIENTED_EDGE ( 'NONE', *, *, #17009, .T. ) ;
#6136 = CARTESIAN_POINT ( 'NONE',  ( -0.02422842392870433459, -0.08956072386513425077, -0.1835680598173657641 ) ) ;
#6137 = CYLINDRICAL_SURFACE ( 'NONE', #33351, 0.4404574800679669777 ) ;
#6138 = EDGE_LOOP ( 'NONE', ( #6952, #31631, #22767, #34065, #20754 ) ) ;
#6139 = DIRECTION ( 'NONE',  ( -1.000000000000000000, 0.000000000000000000, 0.000000000000000000 ) ) ;
#6140 = CARTESIAN_POINT ( 'NONE',  ( 0.3906197235759846786, 4.466152701071653354E-17, 0.000000000000000000 ) ) ;
#6141 = CARTESIAN_POINT ( 'NONE',  ( -0.9500414927467378812, -0.1787899950787401604, 0.5659448818360001132 ) ) ;
#6142 = CARTESIAN_POINT ( 'NONE',  ( 0.9873396505805591694, 0.1113553986120547346, 1.343503936900346529 ) ) ;
#6144 = ORIENTED_EDGE ( 'NONE', *, *, #24253, .T. ) ;
#6143 = AXIS2_PLACEMENT_3D ( 'NONE', #30741, #991, #12283 ) ;
#6145 = CARTESIAN_POINT ( 'NONE',  ( -0.8019270111902716547, 0.1787899950787401604, 1.732283464513166615 ) ) ;
#6146 = AXIS2_PLACEMENT_3D ( 'NONE', #1505, #26951, #5342 ) ;
#6147 = EDGE_CURVE ( 'NONE', #36995, #3438, #34129, .T. ) ;
#6148 = CIRCLE ( 'NONE', #39801, 0.09842519685039310962 ) ;
#6149 = CARTESIAN_POINT ( 'NONE',  ( 0.1574803149606300023, 0.000000000000000000, 0.000000000000000000 ) ) ;
#6150 = ADVANCED_FACE ( 'NONE', ( #36097 ), #26746, .T. ) ;
#6151 = DIRECTION ( 'NONE',  ( 1.000000000000000000, 0.000000000000000000, 0.000000000000000000 ) ) ;
#6152 = PLANE ( 'NONE',  #43018 ) ;
#6153 = ORIENTED_EDGE ( 'NONE', *, *, #39860, .F. ) ;
#6154 = CARTESIAN_POINT ( 'NONE',  ( 0.9412147342319837628, 0.1574803149606300301, 0.6077755905511815770 ) ) ;
#6155 = CARTESIAN_POINT ( 'NONE',  ( 0.2471922904502826812, 0.09842519685039370636, -5.914624404477007554E-17 ) ) ;
#6156 = CARTESIAN_POINT ( 'NONE',  ( -0.9412147342319837628, 0.1574803149606300301, 1.424704724301921743 ) ) ;
#6157 = CARTESIAN_POINT ( 'NONE',  ( 0.8759842519685039353, -0.1787899950787401882, 0.6471456692375747721 ) ) ;
#6158 = EDGE_CURVE ( 'NONE', #27709, #31512, #367, .T. ) ;
#6160 = CARTESIAN_POINT ( 'NONE',  ( -0.7185039370078739607, 1.928577636452523993E-17, 0.6889763778452283605 ) ) ;
#6159 = CARTESIAN_POINT ( 'NONE',  ( 0.1574803149606300301, -0.6402559055118107745, 0.06523048226347956391 ) ) ;
#6161 = CARTESIAN_POINT ( 'NONE',  ( 0.8759842519685039353, 0.1574803149606299191, 1.624015747923968522 ) ) ;
#6162 = ORIENTED_EDGE ( 'NONE', *, *, #37493, .F. ) ;
#6163 = EDGE_CURVE ( 'NONE', #14042, #5036, #40960, .T. ) ;
#6164 = CARTESIAN_POINT ( 'NONE',  ( 0.000000000000000000, 0.000000000000000000, -0.2103840066576717072 ) ) ;
#6165 = CARTESIAN_POINT ( 'NONE',  ( 0.7185039370078746268, 0.06523048226347956391, 1.286909448818898127 ) ) ;
#6167 = ( CONVERSION_BASED_UNIT ( 'INCH', #39466 ) LENGTH_UNIT ( ) NAMED_UNIT ( #22776 ) ) ;
#6166 = CARTESIAN_POINT ( 'NONE',  ( -0.2824199087359777760, 1.411419074098319903, -0.2911036367043356443 ) ) ;
#6168 = CARTESIAN_POINT ( 'NONE',  ( 0.9412147342319837628, -0.1574803149606297803, 1.970964566929134021 ) ) ;
#6169 = CARTESIAN_POINT ( 'NONE',  ( 2.892866454678787531E-17, -0.5984251967428660945, 0.1574803149606299191 ) ) ;
#6170 = ORIENTED_EDGE ( 'NONE', *, *, #17127, .F. ) ;
#6172 = CARTESIAN_POINT ( 'NONE',  ( 0.000000000000000000, 0.000000000000000000, 0.000000000000000000 ) ) ;
#6171 = CARTESIAN_POINT ( 'NONE',  ( 0.8019270111902716547, -0.1787899950787401604, 0.6397637794737947026 ) ) ;
#6173 = CARTESIAN_POINT ( 'NONE',  ( -0.07405724077823318263, -0.6377952755367874982, -0.1787899950787401604 ) ) ;
#6174 = EDGE_LOOP ( 'NONE', ( #2173, #15667, #25106, #39078, #21116 ) ) ;
#6175 = CARTESIAN_POINT ( 'NONE',  ( 0.001477421097710441547, 0.1058998750574050018, -0.09216900433233464474 ) ) ;
#6176 = CARTESIAN_POINT ( 'NONE',  ( 1.002407869896990045, -0.1264236179284866091, 0.8833661416785196785 ) ) ;
#6177 = CARTESIAN_POINT ( 'NONE',  ( -0.8759842519685039353, 0.000000000000000000, 0.000000000000000000 ) ) ;
#6178 = CARTESIAN_POINT ( 'NONE',  ( 3.301370929368692659E-17, 0.1269246943539624195, 0.1797182628040039365 ) ) ;
#6179 = CARTESIAN_POINT ( 'NONE',  ( 0.1264236179284866091, -1.083169291284818980, -0.1264236179284866091 ) ) ;
#6180 = CARTESIAN_POINT ( 'NONE',  ( 2.892866454678787531E-17, -1.395669291338582862, 0.1574803149606299191 ) ) ;
#6181 = CARTESIAN_POINT ( 'NONE',  ( 1.033464566929133799, 0.000000000000000000, 1.220472440837354400 ) ) ;
#6182 = CARTESIAN_POINT ( 'NONE',  ( -0.8107537697050254399, 0.1574803149606300301, 1.862696850286174710 ) ) ;
#6183 = UNCERTAINTY_MEASURE_WITH_UNIT (LENGTH_MEASURE( 1.000000000000000082E-05 ), #1373, 'distance_accuracy_value', 'NONE') ;
#6184 = CARTESIAN_POINT ( 'NONE',  ( -1.002407869896990045, -0.1264236179284866091, 1.872539370024976391 ) ) ;
#6185 = CARTESIAN_POINT ( 'NONE',  ( 0.6971942568897648851, -0.07405724077823297447, 1.938976377898990799 ) ) ;
#6186 = ORIENTED_EDGE ( 'NONE', *, *, #12845, .F. ) ;
#6187 = CARTESIAN_POINT ( 'NONE',  ( -0.9412147342319837628, -0.1574803149606297803, 1.852854330708662012 ) ) ;
#6188 = AXIS2_PLACEMENT_3D ( 'NONE', #9502, #46136, #27264 ) ;
#6189 = CARTESIAN_POINT ( 'NONE',  ( -1.002407869896990045, -0.1264236179284866091, 1.592027559001354398 ) ) ;
#6190 = CARTESIAN_POINT ( 'NONE',  ( 0.1279527559055118058, 0.2216206741968047289, -0.3149606299212598381 ) ) ;
#6191 = CARTESIAN_POINT ( 'NONE',  ( -0.9500414927467378812, -0.1787899950787401604, 0.9990157479777320715 ) ) ;
#6192 = VECTOR ( 'NONE', #29515, 39.37007874015748143 ) ;
#6193 = CARTESIAN_POINT ( 'NONE',  ( -1.002407869896990045, -0.1264236179284866091, 0.1796259841982051075 ) ) ;
#6194 = CARTESIAN_POINT ( 'NONE',  ( -0.2471922904502826535, 0.09842519685039370636, 0.01310751975302586886 ) ) ;
#6195 = CARTESIAN_POINT ( 'NONE',  ( -0.8019270111902717657, 0.1787899950787401604, 1.968503936954110189 ) ) ;
#6196 = CARTESIAN_POINT ( 'NONE',  ( -0.1888124183976708226, 0.07899857248962416367, 0.1764221702779021350 ) ) ;
#6197 = CARTESIAN_POINT ( 'NONE',  ( -0.9412147342319837628, -0.1574803149606297803, 1.931594488188976166 ) ) ;
#6198 = CARTESIAN_POINT ( 'NONE',  ( -0.7185039370078739607, 1.928577636452523993E-17, 1.879921259842519676 ) ) ;
#6199 = CARTESIAN_POINT ( 'NONE',  ( 0.008044285442517225965, -0.09842519685039370636, 0.2239033890101252144 ) ) ;
#6200 = DIRECTION ( 'NONE',  ( -1.000000000000000000, -0.000000000000000000, -0.000000000000000000 ) ) ;
#6201 = ORIENTED_EDGE ( 'NONE', *, *, #1444, .F. ) ;
#6202 = ORIENTED_EDGE ( 'NONE', *, *, #34576, .F. ) ;
#6203 = CARTESIAN_POINT ( 'NONE',  ( 0.1787899950787401882, -1.009350393647023614, -2.189545951927503898E-17 ) ) ;
#6204 = CARTESIAN_POINT ( 'NONE',  ( 0.1787899950787401604, -1.243110236166709459, 0.07405724077823318263 ) ) ;
#6205 = EDGE_CURVE ( 'NONE', #22637, #43357, #7336, .T. ) ;
#6206 = DIRECTION ( 'NONE',  ( -0.000000000000000000, -0.000000000000000000, 1.000000000000000000 ) ) ;
#6207 = ( LENGTH_UNIT ( ) NAMED_UNIT ( * ) SI_UNIT ( $, .METRE. ) ) ;
#6208 = CARTESIAN_POINT ( 'NONE',  ( -1.100456976456230270E-17, -0.5620516835987936499, -0.1797182628040039365 ) ) ;
#6209 = DIRECTION ( 'NONE',  ( 0.000000000000000000, 0.000000000000000000, -1.000000000000000000 ) ) ;
#6210 = CARTESIAN_POINT ( 'NONE',  ( -0.9873396505805591694, 0.1113553986120547346, 0.8710629920184568276 ) ) ;
#6211 = CARTESIAN_POINT ( 'NONE',  ( -0.9412147342319837628, -0.1574803149606297803, 0.7504921259842516346 ) ) ;
#6212 = CARTESIAN_POINT ( 'NONE',  ( -0.1574803149606299191, -0.02755905511811023584, 0.000000000000000000 ) ) ;
#6213 = VECTOR ( 'NONE', #36585, 39.37007874015748143 ) ;
#6214 = PRESENTATION_LAYER_ASSIGNMENT (  '', '', ( #33047 ) ) ;
#6215 = EDGE_CURVE ( 'NONE', #23237, #38700, #29554, .T. ) ;
#6216 = CARTESIAN_POINT ( 'NONE',  ( 0.7185039370078739607, 1.928577636452523993E-17, 0.7775590551181102983 ) ) ;
#6217 = TOROIDAL_SURFACE ( 'NONE', #24609, 0.3444881889763780070, 0.1574803149606299191 ) ;
#6218 = CARTESIAN_POINT ( 'NONE',  ( 0.1528603379501230763, -0.2072402749984882109, -0.03001342526389988788 ) ) ;
#6219 = CARTESIAN_POINT ( 'NONE',  ( 0.4811709046783464450, -0.09842519685039370636, 0.000000000000000000 ) ) ;
#6220 = ( BOUNDED_CURVE ( )  B_SPLINE_CURVE ( 2, ( #6630, #3026, #35181, #42344, #28226, #42789, #31594, #2327, #12385 ),
 .UNSPECIFIED., .F., .F. ) 
 B_SPLINE_CURVE_WITH_KNOTS ( ( 3, 2, 2, 2, 3 ),
 ( 0.3200000000000000067, 0.3225000000000000089, 0.3250000000000000111, 0.3275000000000000133, 0.3300000000000000155 ),
 .UNSPECIFIED. ) 
 CURVE ( )  GEOMETRIC_REPRESENTATION_ITEM ( )  RATIONAL_B_SPLINE_CURVE ( ( 1.000000000000000000, 0.9238795325112869605, 1.000000000000000000, 0.9238795325112869605, 1.000000000000000000, 0.9238795325112869605, 1.000000000000000000, 0.9238795325112869605, 1.000000000000000000 ) ) 
 REPRESENTATION_ITEM ( '' )  ) ;
#6222 = CARTESIAN_POINT ( 'NONE',  ( 0.1599045142068430958, -0.09467125711648119446, -0.1169792578046013332 ) ) ;
#6221 = CARTESIAN_POINT ( 'NONE',  ( 0.2170082705493531494, 0.1702044488443620607, -0.06846571731933490113 ) ) ;
#6223 = CARTESIAN_POINT ( 'NONE',  ( 0.8107537697050253289, 0.1574803149606300301, 0.2091535431995598104 ) ) ;
#6224 = ORIENTED_EDGE ( 'NONE', *, *, #45038, .F. ) ;
#6225 = CARTESIAN_POINT ( 'NONE',  ( 0.4620708661417355922, 0.9842519685039372579, -1.186023622047244430 ) ) ;
#6226 = DIRECTION ( 'NONE',  ( 0.000000000000000000, -1.000000000000000000, 0.000000000000000000 ) ) ;
#6227 = CARTESIAN_POINT ( 'NONE',  ( -0.07405724077823318263, -0.5492125983714331028, 0.1787899950787401604 ) ) ;
#6228 = CARTESIAN_POINT ( 'NONE',  ( 0.1264236179284866091, -1.393208661363559031, -0.1264236179284866091 ) ) ;
#6229 = CARTESIAN_POINT ( 'NONE',  ( -0.6971942568897637749, 2.189545951927499583E-17, 1.852854330654897685 ) ) ;
#6230 = ORIENTED_EDGE ( 'NONE', *, *, #29273, .F. ) ;
#6231 = CARTESIAN_POINT ( 'NONE',  ( -1.002407869896990045, -0.1264236179284866091, 1.518208661363559031 ) ) ;
#6232 = CARTESIAN_POINT ( 'NONE',  ( 1.054774247047244540, -0.07405724077823318263, 1.599409448765135133 ) ) ;
#6233 = CARTESIAN_POINT ( 'NONE',  ( -0.1574803149606299191, -1.277559055010582645, 0.000000000000000000 ) ) ;
#6234 = CARTESIAN_POINT ( 'NONE',  ( -0.8019270111902717657, -0.1787899950787401604, 0.6053149605761579677 ) ) ;
#6235 = CARTESIAN_POINT ( 'NONE',  ( 0.6971942568897637749, 2.189545951927499583E-17, 0.2042322834108035723 ) ) ;
#6236 = LINE ( 'NONE', #35273, #14392 ) ;
#6237 = ( LENGTH_UNIT ( ) NAMED_UNIT ( * ) SI_UNIT ( $, .METRE. ) ) ;
#6238 = CARTESIAN_POINT ( 'NONE',  ( 0.8019270111902716547, 0.1787899950787401604, 0.6299212597887560161 ) ) ;
#6239 = CARTESIAN_POINT ( 'NONE',  ( -0.8019270111902716547, 0.1787899950787401604, 0.5068897637257642197 ) ) ;
#6240 = ADVANCED_FACE ( 'NONE', ( #33474 ), #40604, .F. ) ;
#6241 = CARTESIAN_POINT ( 'NONE',  ( 0.9873396505805591694, -0.1113553986120547346, 0.6348425196850393526 ) ) ;
#6242 = VECTOR ( 'NONE', #22207, 39.37007874015748143 ) ;
#6243 = CARTESIAN_POINT ( 'NONE',  ( 0.1574803149606300301, -0.08415354330708660346, -0.06523048226347956391 ) ) ;
#6244 = ORIENTED_EDGE ( 'NONE', *, *, #43925, .T. ) ;
#6245 = CARTESIAN_POINT ( 'NONE',  ( -1.054774247047244540, -0.07405724077823318263, 1.402559055064346971 ) ) ;
#6246 = ORIENTED_EDGE ( 'NONE', *, *, #15494, .T. ) ;
#6247 = CARTESIAN_POINT ( 'NONE',  ( -0.8107537697050253289, 0.1574803149606300301, 0.4552165354330702240 ) ) ;
#6248 = CARTESIAN_POINT ( 'NONE',  ( 0.9500414927467377701, -0.1787899950787401604, 1.279527559001355730 ) ) ;
#6249 = CARTESIAN_POINT ( 'NONE',  ( -0.05398180662860094930, -0.09851384891491477003, 0.2205059587191452730 ) ) ;
#6250 = VECTOR ( 'NONE', #3143, 39.37007874015748143 ) ;
#6251 = ORIENTED_EDGE ( 'NONE', *, *, #19100, .T. ) ;
#6252 = AXIS2_PLACEMENT_3D ( 'NONE', #21983, #32560, #29233 ) ;
#6253 = CARTESIAN_POINT ( 'NONE',  ( -0.1264236179284866091, -1.635458613898529645, -0.1264236179284866091 ) ) ;
#6254 = ORIENTED_EDGE ( 'NONE', *, *, #27428, .T. ) ;
#6255 = CARTESIAN_POINT ( 'NONE',  ( -0.1787899950787401882, -0.6304133857730078727, 0.000000000000000000 ) ) ;
#6256 = CARTESIAN_POINT ( 'NONE',  ( 0.9873396505805591694, -0.1113553986120547346, 1.619094488188976388 ) ) ;
#6257 = CARTESIAN_POINT ( 'NONE',  ( 0.8759842519685039353, 0.000000000000000000, 4.498031496062992574 ) ) ;
#6258 = ORIENTED_EDGE ( 'NONE', *, *, #8880, .T. ) ;
#6259 = EDGE_CURVE ( 'NONE', #11279, #44249, #37154, .T. ) ;
#6260 = EDGE_CURVE ( 'NONE', #31847, #38785, #36810, .T. ) ;
#6261 = CARTESIAN_POINT ( 'NONE',  ( 0.1787899950787401604, -0.3425196849856064762, 0.07405724077823318263 ) ) ;
#6262 = CARTESIAN_POINT ( 'NONE',  ( 0.1787899950787401604, -0.8051181101824581576, -0.07405724077823318263 ) ) ;
#6263 = ADVANCED_FACE ( 'NONE', ( #22896 ), #21955, .F. ) ;
#6264 = FACE_OUTER_BOUND ( 'NONE', #33801, .T. ) ;
#6265 = CARTESIAN_POINT ( 'NONE',  ( -0.8759842519685039353, -0.1574803149606299191, 0.9744094487113701408 ) ) ;
#6266 = CARTESIAN_POINT ( 'NONE',  ( 0.1787899950787401604, -0.03358853515837262327, -0.07405724077823318263 ) ) ;
#6267 = CARTESIAN_POINT ( 'NONE',  ( 0.1264236179284866091, 0.05856299217974780119, -0.1264236179284866091 ) ) ;
#6268 = CARTESIAN_POINT ( 'NONE',  ( -0.03598878106637547203, -0.09842522444525984848, 0.1542999736886214723 ) ) ;
#6269 = AXIS2_PLACEMENT_3D ( 'NONE', #11085, #21373, #33141 ) ;
#6270 = EDGE_CURVE ( 'NONE', #22975, #5495, #40297, .T. ) ;
#6271 = CARTESIAN_POINT ( 'NONE',  ( 0.6971942568897626646, 0.07405724077823318263, 0.5118110235682844511 ) ) ;
#6272 = DIMENSIONAL_EXPONENTS ( 1.000000000000000000, 0.000000000000000000, 0.000000000000000000, 0.000000000000000000, 0.000000000000000000, 0.000000000000000000, 0.000000000000000000 ) ;
#6273 = CARTESIAN_POINT ( 'NONE',  ( -0.6971942568897648851, -0.07405724077823297447, 0.7972440944344248992 ) ) ;
#6275 = CARTESIAN_POINT ( 'NONE',  ( 0.8107537697050254399, 0.1574803149606300301, 1.124507874015748810 ) ) ;
#6274 = CARTESIAN_POINT ( 'NONE',  ( -0.1113553986120547346, -0.8494094488188976833, 0.1113553986120547346 ) ) ;
#6277 = CARTESIAN_POINT ( 'NONE',  ( -0.7725776124789660582, -0.1361825328364024978, 1.986138947217436668 ) ) ;
#6276 = CARTESIAN_POINT ( 'NONE',  ( -0.1797182628040039365, -1.772681604858638016, 0.000000000000000000 ) ) ;
#6278 = CARTESIAN_POINT ( 'NONE',  ( -0.1574803149606299191, -0.4901574802074331050, 0.000000000000000000 ) ) ;
#6279 = CARTESIAN_POINT ( 'NONE',  ( -0.1787899950787401604, -0.3523622046706461619, 0.07405724077823318263 ) ) ;
#6280 = CARTESIAN_POINT ( 'NONE',  ( -0.8759842519685039353, -0.1574803149606299191, 1.249999999892472236 ) ) ;
#6281 = CARTESIAN_POINT ( 'NONE',  ( 0.8759842519685039353, -0.1787899950787401882, 1.710137795221826851 ) ) ;
#6283 = CARTESIAN_POINT ( 'NONE',  ( 0.2559055118110235560, 0.07179175674853267852, -0.3092570035108861415 ) ) ;
#6282 = DIRECTION ( 'NONE',  ( 0.000000000000000000, 0.000000000000000000, 1.000000000000000000 ) ) ;
#6284 = CARTESIAN_POINT ( 'NONE',  ( 0.8019270111902716547, 0.1787899950787401604, 0.3887795275052913224 ) ) ;
#6285 = ORIENTED_EDGE ( 'NONE', *, *, #19244, .T. ) ;
#6286 = VECTOR ( 'NONE', #45938, 39.37007874015748143 ) ;
#6287 = AXIS2_PLACEMENT_3D ( 'NONE', #17800, #38894, #21148 ) ;
#6288 = ORIENTED_EDGE ( 'NONE', *, *, #34010, .F. ) ;
#6289 = DIRECTION ( 'NONE',  ( 0.000000000000000000, 1.000000000000000000, 0.000000000000000000 ) ) ;
#6290 = CARTESIAN_POINT ( 'NONE',  ( 0.1939344384855389569, -0.1835261454400549941, -0.3085539532670578677 ) ) ;
#6291 = CARTESIAN_POINT ( 'NONE',  ( -0.1787899950787401604, -0.04724409443442544737, -0.07405724077823318263 ) ) ;
#6292 = CARTESIAN_POINT ( 'NONE',  ( 1.002407869896990045, -0.1264236179284866091, 0.6471456692375747721 ) ) ;
#6293 = DIRECTION ( 'NONE',  ( 1.000000000000000000, 0.000000000000000000, 0.000000000000000000 ) ) ;
#6294 = CARTESIAN_POINT ( 'NONE',  ( -0.9412147342319837628, -0.1574803149606297803, 0.9374999998924736788 ) ) ;
#6295 = CARTESIAN_POINT ( 'NONE',  ( -0.9500414927467378812, -0.1787899950787401604, 1.432086614119464141 ) ) ;
#6296 = CARTESIAN_POINT ( 'NONE',  ( -0.2618967166504349575, -0.1659366058165109570, -0.8537719073895772004 ) ) ;
#6297 = CARTESIAN_POINT ( 'NONE',  ( 1.054774247047244540, 0.07405724077823318263, 1.013779527505291878 ) ) ;
#6298 = CARTESIAN_POINT ( 'NONE',  ( -0.7185039370078746268, 0.06523048226347956391, 0.6471456691838121111 ) ) ;
#6299 = CARTESIAN_POINT ( 'NONE',  ( 0.6971942568897648851, 0.07405724077823318263, 1.811023621993480548 ) ) ;
#6300 = CARTESIAN_POINT ( 'NONE',  ( -0.8107537697050253289, -0.1574803149606297803, 1.375492125984252523 ) ) ;
#6301 = CARTESIAN_POINT ( 'NONE',  ( -1.054774247047244540, -0.07405724077823318263, 0.8858267715997791836 ) ) ;
#6302 = DIRECTION ( 'NONE',  ( 1.000000000000000000, -3.469446951953614583E-15, -1.151683635503274272E-16 ) ) ;
#6303 = CARTESIAN_POINT ( 'NONE',  ( -0.009895589093224880714, -0.2897810112356447587, -0.09996720075265054517 ) ) ;
#6304 = CARTESIAN_POINT ( 'NONE',  ( 1.054774247047244540, 0.07405724077823318263, 0.1082677164816695514 ) ) ;
#6305 = CARTESIAN_POINT ( 'NONE',  ( 0.8759842519685039353, 0.1574803149606299191, 1.545275590443653480 ) ) ;
#6306 = VERTEX_POINT ( 'NONE', #33949 ) ;
#6307 = EDGE_CURVE ( 'NONE', #44763, #42069, #44317, .T. ) ;
#6308 = LINE ( 'NONE', #24538, #22934 ) ;
#6309 = CARTESIAN_POINT ( 'NONE',  ( -1.033464566929133799, -1.928577636452524610E-17, 2.007874015640504162 ) ) ;
#6310 = VERTEX_POINT ( 'NONE', #44438 ) ;
#6311 = CARTESIAN_POINT ( 'NONE',  ( -0.9500414927467377701, -0.1787899950787401604, 1.668307086560410157 ) ) ;
#6312 = CARTESIAN_POINT ( 'NONE',  ( 0.1264236179284866091, -1.481791338528913426, 0.1264236179284866091 ) ) ;
#6313 = STYLED_ITEM ( 'NONE', ( #6008 ), #35488 ) ;
#6314 = CARTESIAN_POINT ( 'NONE',  ( -0.8759842519685039353, 0.000000000000000000, 0.000000000000000000 ) ) ;
#6315 = CARTESIAN_POINT ( 'NONE',  ( 0.5962569168439626477, 1.205361022782824954E-17, -0.09842519685039370636 ) ) ;
#6316 = CARTESIAN_POINT ( 'NONE',  ( -0.07405724077823318263, -1.165478298937900448, -0.1787899950787401604 ) ) ;
#6317 = EDGE_LOOP ( 'NONE', ( #36359, #15533, #3449, #13894 ) ) ;
#6318 = CARTESIAN_POINT ( 'NONE',  ( 0.07405724077823318263, -0.05216535427694517224, -0.1787899950787401604 ) ) ;
#6319 = ORIENTED_EDGE ( 'NONE', *, *, #22404, .F. ) ;
#6320 = EDGE_CURVE ( 'NONE', #9932, #2533, #25713, .T. ) ;
#6321 = ORIENTED_EDGE ( 'NONE', *, *, #2315, .F. ) ;
#6322 = CARTESIAN_POINT ( 'NONE',  ( 0.8759842519685039353, -0.1787899950787401882, 1.075295275536787276 ) ) ;
#6323 = ( GEOMETRIC_REPRESENTATION_CONTEXT ( 3 ) GLOBAL_UNCERTAINTY_ASSIGNED_CONTEXT ( ( #40306 ) ) GLOBAL_UNIT_ASSIGNED_CONTEXT ( ( #1681, #5042, #12502 ) ) REPRESENTATION_CONTEXT ( 'NONE', 'WORKASPACE' ) ) ;
#6324 = DIRECTION ( 'NONE',  ( -1.000000000000000000, 0.000000000000000000, 0.000000000000000000 ) ) ;
#6325 = CARTESIAN_POINT ( 'NONE',  ( 0.3980944881889795228, 0.9100161909011693639, 0.01858545845903165558 ) ) ;
#6326 = ADVANCED_FACE ( 'NONE', ( #20474 ), #13302, .T. ) ;
#6327 = CARTESIAN_POINT ( 'NONE',  ( 0.9412147342319837628, 0.1574803149606300301, 1.867618110236221707 ) ) ;
#6328 = AXIS2_PLACEMENT_3D ( 'NONE', #9787, #19060, #26758 ) ;
#6329 = CARTESIAN_POINT ( 'NONE',  ( -0.1787899950787401882, -0.7534448818360000022, 0.000000000000000000 ) ) ;
#6330 = EDGE_CURVE ( 'NONE', #23068, #47303, #2256, .T. ) ;
#6331 = CARTESIAN_POINT ( 'NONE',  ( -1.002407869896990045, -0.1264236179284866091, 0.2977362204186775885 ) ) ;
#6332 = PRODUCT_DEFINITION ( 'UNKNOWN', '', #41536, #43673 ) ;
#6333 = FACE_OUTER_BOUND ( 'NONE', #41239, .T. ) ;
#6334 = CARTESIAN_POINT ( 'NONE',  ( 1.054774247047244540, -0.07405724077823318263, 1.126968503883244654 ) ) ;
#6335 = CARTESIAN_POINT ( 'NONE',  ( 0.9500414927467377701, -0.1787899950787401604, 1.589566929080094226 ) ) ;
#6336 = CARTESIAN_POINT ( 'NONE',  ( 1.002407869896990045, -0.1264236179284866091, 0.2140748030958428971 ) ) ;
#6337 = CARTESIAN_POINT ( 'NONE',  ( 0.000000000000000000, -0.09842519685039370636, 0.1574803149606299191 ) ) ;
#6339 = CARTESIAN_POINT ( 'NONE',  ( 0.7185039370078739607, 1.928577636452523993E-17, 1.515748031388535200 ) ) ;
#6338 = CARTESIAN_POINT ( 'NONE',  ( 0.8759842491179902213, 0.1574803149606299191, 1.978346456692913646 ) ) ;
#6340 = CARTESIAN_POINT ( 'NONE',  ( 0.1620125744594652917, -0.07969860776396833768, -0.1380421452775067170 ) ) ;
#6341 = CARTESIAN_POINT ( 'NONE',  ( 0.9412147342319837628, -0.1574803149606297803, 0.7800196849318437042 ) ) ;
#6342 = CARTESIAN_POINT ( 'NONE',  ( -0.7185039370078746268, -0.06523048226347956391, 1.793799212490897244 ) ) ;
#6343 = CARTESIAN_POINT ( 'NONE',  ( 1.054774247047244540, -0.07405724077823318263, 0.09842519679663024046 ) ) ;
#6344 = VECTOR ( 'NONE', #907, 39.37007874015748854 ) ;
#6345 = DIRECTION ( 'NONE',  ( -3.469446951953613794E-15, -1.000000000000000000, 0.000000000000000000 ) ) ;
#6347 = CARTESIAN_POINT ( 'NONE',  ( 0.3690944881889778317, 2.862949378880179425E-15, 0.7480314960629921295 ) ) ;
#6346 = CARTESIAN_POINT ( 'NONE',  ( 1.054774247047244540, -0.07405724077823318263, 1.122047244040725422 ) ) ;
#6348 = CARTESIAN_POINT ( 'NONE',  ( 0.8019270111902716547, -0.1787899950787401604, 1.943897637741510254 ) ) ;
#6349 = CARTESIAN_POINT ( 'NONE',  ( 0.8759842519685039353, 0.1574803149606299191, 0.4429133857192448787 ) ) ;
#6350 = ORIENTED_EDGE ( 'NONE', *, *, #35400, .T. ) ;
#6351 = ( NAMED_UNIT ( * ) PLANE_ANGLE_UNIT ( ) SI_UNIT ( $, .RADIAN. ) ) ;
#6352 = CARTESIAN_POINT ( 'NONE',  ( -0.7646288533564489232, -0.1113553986120547346, 0.4576771652468039631 ) ) ;
#6353 = ORIENTED_EDGE ( 'NONE', *, *, #7044, .T. ) ;
#6354 = CARTESIAN_POINT ( 'NONE',  ( 1.054774247047244540, 0.07405724077823318263, 1.284448818843874740 ) ) ;
#6356 = LINE ( 'NONE', #46145, #23134 ) ;
#6355 = CARTESIAN_POINT ( 'NONE',  ( -0.3690944881889761109, 0.1864803149606354127, 0.7480314960629921295 ) ) ;
#6357 = CARTESIAN_POINT ( 'NONE',  ( -0.1787899950787401604, -0.04232283459190578495, -0.07405724077823318263 ) ) ;
#6358 = DIRECTION ( 'NONE',  ( 1.822029033848725028E-16, 0.000000000000000000, 1.000000000000000000 ) ) ;
#6359 = AXIS2_PLACEMENT_3D ( 'NONE', #26493, #37250, #8014 ) ;
#6360 = ORIENTED_EDGE ( 'NONE', *, *, #11275, .F. ) ;
#6361 = CARTESIAN_POINT ( 'NONE',  ( 0.1984097999861146600, 0.07306521771078811067, 0.1708811194342987061 ) ) ;
#6362 = FACE_OUTER_BOUND ( 'NONE', #32085, .T. ) ;
#6363 = CARTESIAN_POINT ( 'NONE',  ( 0.8019270111902717657, 0.1787899950787401604, 0.3937007873478115538 ) ) ;
#6364 = ORIENTED_EDGE ( 'NONE', *, *, #16140, .F. ) ;
#6365 = CARTESIAN_POINT ( 'NONE',  ( -0.7495606340400177148, -0.1264236179284866091, 1.385334645615527549 ) ) ;
#6366 = CARTESIAN_POINT ( 'NONE',  ( -0.1264236179284866091, -1.742618110182456714, -0.1264236179284866091 ) ) ;
#6367 = CARTESIAN_POINT ( 'NONE',  ( -0.8759842519685039353, 0.1787899950787401882, 1.021161417269070837 ) ) ;
#6368 = ADVANCED_FACE ( 'NONE', ( #4908 ), #46344, .F. ) ;
#6369 = CARTESIAN_POINT ( 'NONE',  ( -0.8759842519685039353, 0.1787899950787401882, 1.921751968450173376 ) ) ;
#6370 = ORIENTED_EDGE ( 'NONE', *, *, #5250, .F. ) ;
#6371 = EDGE_CURVE ( 'NONE', #14105, #28863, #19529, .T. ) ;
#6372 = CARTESIAN_POINT ( 'NONE',  ( -0.6971942568897648851, 0.07405724077823318263, 1.062992125930488418 ) ) ;
#6373 = CARTESIAN_POINT ( 'NONE',  ( -0.7495606340400177148, -0.1264236179284866091, 0.6028543306548976854 ) ) ;
#6374 = ( BOUNDED_CURVE ( )  B_SPLINE_CURVE ( 2, ( #34416, #30380, #19065, #30149, #19311, #33964, #41322, #46355, #13769 ),
 .UNSPECIFIED., .F., .F. ) 
 B_SPLINE_CURVE_WITH_KNOTS ( ( 3, 2, 2, 2, 3 ),
 ( 0.9599999999999999645, 0.9625000000000000222, 0.9649999999999999689, 0.9675000000000000266, 0.9699999999999999734 ),
 .UNSPECIFIED. ) 
 CURVE ( )  GEOMETRIC_REPRESENTATION_ITEM ( )  RATIONAL_B_SPLINE_CURVE ( ( 1.000000000000000000, 0.9238795325112869605, 1.000000000000000000, 0.9238795325112869605, 1.000000000000000000, 0.9238795325112869605, 1.000000000000000000, 0.9238795325112799661, 1.000000000000000000 ) ) 
 REPRESENTATION_ITEM ( '' )  ) ;
#6375 = CARTESIAN_POINT ( 'NONE',  ( 1.033464566929133799, 0.000000000000000000, 1.820866141732283561 ) ) ;
#6376 = CARTESIAN_POINT ( 'NONE',  ( 1.737901732061166719E-16, 0.1564960629921311464, 0.2933070866141737065 ) ) ;
#6377 = CARTESIAN_POINT ( 'NONE',  ( -0.07405724077823318263, -0.7176436532686085723, 0.1787899950787401604 ) ) ;
#6378 = VERTEX_POINT ( 'NONE', #37753 ) ;
#6379 = CARTESIAN_POINT ( 'NONE',  ( -0.1238056228176431101, -0.08956144685902442393, 0.1042814069884555189 ) ) ;
#6380 = CARTESIAN_POINT ( 'NONE',  ( -0.01196991696110410314, -0.08706565000358124085, 0.1574804073918250613 ) ) ;
#6381 = EDGE_CURVE ( 'NONE', #3953, #17273, #33360, .T. ) ;
#6382 = ORIENTED_EDGE ( 'NONE', *, *, #21253, .T. ) ;
#6383 = CARTESIAN_POINT ( 'NONE',  ( 1.033464566929133799, 0.000000000000000000, 0.7578740157480314821 ) ) ;
#6384 = FACE_OUTER_BOUND ( 'NONE', #19680, .T. ) ;
#6385 = CARTESIAN_POINT ( 'NONE',  ( -0.8759842519685039353, 0.1787899950787401882, 0.6225393700249762796 ) ) ;
#6386 = CARTESIAN_POINT ( 'NONE',  ( 0.1574803149606299191, 0.07086614173228346358, -1.928577636452523993E-17 ) ) ;
#6387 = ORIENTED_EDGE ( 'NONE', *, *, #28433, .T. ) ;
#6388 = CARTESIAN_POINT ( 'NONE',  ( -1.054774247047244096, 0.000000000000000000, 1.641240157426551161 ) ) ;
#6389 = AXIS2_PLACEMENT_3D ( 'NONE', #21796, #15565, #30204 ) ;
#6390 = PRODUCT_DEFINITION ( 'UNKNOWN', '', #25524, #46091 ) ;
#6391 = DIRECTION ( 'NONE',  ( 0.000000000000000000, 0.000000000000000000, -1.000000000000000000 ) ) ;
#6392 = ( BOUNDED_CURVE ( )  B_SPLINE_CURVE ( 2, ( #26629, #45745, #42141, #9350, #5029, #30704, #9109, #41181, #8869 ),
 .UNSPECIFIED., .F., .F. ) 
 B_SPLINE_CURVE_WITH_KNOTS ( ( 3, 2, 2, 2, 3 ),
 ( 0.4699999999999999734, 0.4724999999999999756, 0.4749999999999999778, 0.4774999999999999800, 0.4799999999999999822 ),
 .UNSPECIFIED. ) 
 CURVE ( )  GEOMETRIC_REPRESENTATION_ITEM ( )  RATIONAL_B_SPLINE_CURVE ( ( 1.000000000000000000, 0.9238795325112879597, 1.000000000000000000, 0.9238795325112869605, 1.000000000000000000, 0.9238795325112869605, 1.000000000000000000, 0.9238795325112869605, 1.000000000000000000 ) ) 
 REPRESENTATION_ITEM ( '' )  ) ;
#6393 = CARTESIAN_POINT ( 'NONE',  ( -0.7185039370078746268, 0.06523048226347956391, 0.4995078740157475883 ) ) ;
#6394 = ORIENTED_EDGE ( 'NONE', *, *, #40067, .T. ) ;
#6395 = CARTESIAN_POINT ( 'NONE',  ( -0.1270800023317771588, -0.7933508961972184359, -0.1270800023317771588 ) ) ;
#6396 = FACE_BOUND ( 'NONE', #6977, .T. ) ;
#6397 = CARTESIAN_POINT ( 'NONE',  ( -0.7646288533564489232, 0.1113553986120547346, 1.392716535325543292 ) ) ;
#6398 = CARTESIAN_POINT ( 'NONE',  ( 0.06523048226347956391, -0.6058070866141728184, 0.1574803149606297803 ) ) ;
#6399 = CARTESIAN_POINT ( 'NONE',  ( -0.06564852040591530324, 0.1217688336447599051, -0.1452423310039973325 ) ) ;
#6400 = CARTESIAN_POINT ( 'NONE',  ( 0.1099139000111727937, 0.3740157480314960647, 1.120507485783946100 ) ) ;
#6401 = CARTESIAN_POINT ( 'NONE',  ( 0.8759842519685039353, -0.1574803149606299191, 1.259842519685039353 ) ) ;
#6402 = CARTESIAN_POINT ( 'NONE',  ( 2.892866454678787531E-17, 0.07086614183981043702, 0.1574803149606299191 ) ) ;
#6404 = DIRECTION ( 'NONE',  ( -1.000000000000000000, 0.000000000000000000, 0.000000000000000000 ) ) ;
#6403 = FACE_OUTER_BOUND ( 'NONE', #12498, .T. ) ;
#6405 = DIRECTION ( 'NONE',  ( 1.000000000000000000, 0.000000000000000000, 0.000000000000000000 ) ) ;
#6407 = CARTESIAN_POINT ( 'NONE',  ( 0.5555748031496109407, 0.9100161909011688088, 0.01858545845903165558 ) ) ;
#6406 = CARTESIAN_POINT ( 'NONE',  ( 0.7495606340400177148, -0.1264236179284866091, 0.5979330708123780092 ) ) ;
#6408 = CARTESIAN_POINT ( 'NONE',  ( 0.3849708276051176936, -0.09842519685039370636, 1.205361022782828805E-17 ) ) ;
#6409 = DIRECTION ( 'NONE',  ( 0.000000000000000000, 0.000000000000000000, 1.000000000000000000 ) ) ;
#6410 = ( REPRESENTATION_RELATIONSHIP ('NONE','NONE', #9609, #45408 ) REPRESENTATION_RELATIONSHIP_WITH_TRANSFORMATION ( #35915 )SHAPE_REPRESENTATION_RELATIONSHIP( ) ) ;
#6411 = FACE_OUTER_BOUND ( 'NONE', #14762, .T. ) ;
#6412 = CARTESIAN_POINT ( 'NONE',  ( 0.8759842519685039353, -0.1787899950787401882, 0.8390748030958424808 ) ) ;
#6413 = CARTESIAN_POINT ( 'NONE',  ( 0.7185039370078746268, -0.06523048226347956391, 1.291830708661417360 ) ) ;
#6414 = CARTESIAN_POINT ( 'NONE',  ( 0.1377952755905512139, 0.1574803149606299191, 0.7066929133858274037 ) ) ;
#6415 = CARTESIAN_POINT ( 'NONE',  ( 0.1797182628040039365, 0.09739713529884430621, -2.200913952912460540E-17 ) ) ;
#6416 = CARTESIAN_POINT ( 'NONE',  ( 0.1264236179284866091, -1.014271653489543290, 0.1264236179284866091 ) ) ;
#6417 = CARTESIAN_POINT ( 'NONE',  ( 0.06523048226347956391, -1.575295275590552713, -0.1574803149606300301 ) ) ;
#6418 = CARTESIAN_POINT ( 'NONE',  ( 0.9412147342319837628, -0.1574803149606297803, 1.291830708553889817 ) ) ;
#6419 = DIRECTION ( 'NONE',  ( -1.000000000000000000, 0.000000000000000000, 0.000000000000000000 ) ) ;
#6420 = CARTESIAN_POINT ( 'NONE',  ( -0.6971942568897637749, 2.189545951927499583E-17, 1.936515747977732405 ) ) ;
#6421 = ORIENTED_EDGE ( 'NONE', *, *, #5639, .F. ) ;
#6422 = CARTESIAN_POINT ( 'NONE',  ( 1.054774247047244540, 0.07405724077823318263, 1.919291338528913871 ) ) ;
#6423 = VERTEX_POINT ( 'NONE', #30588 ) ;
#6424 = CARTESIAN_POINT ( 'NONE',  ( 0.1574803149606300301, -1.417814960522395085, 0.06523048226347956391 ) ) ;
#6425 = CARTESIAN_POINT ( 'NONE',  ( -0.8759842519685039353, -0.1787899950787401882, 1.985728346402929168 ) ) ;
#6426 = CARTESIAN_POINT ( 'NONE',  ( -0.6971942568897648851, -0.07405724077823297447, 1.500984251914741607 ) ) ;
#6427 = CARTESIAN_POINT ( 'NONE',  ( 1.054774247047244540, -0.07405724077823318263, 0.8907480314422985268 ) ) ;
#6428 = EDGE_CURVE ( 'NONE', #11697, #44566, #23137, .T. ) ;
#6429 = CARTESIAN_POINT ( 'NONE',  ( -0.8019270111902717657, -0.1787899950787401604, 1.033464566875371027 ) ) ;
#6430 = CARTESIAN_POINT ( 'NONE',  ( -0.9500414927467378812, -0.1787899950787401604, 0.2165354330171024577 ) ) ;
#6431 = ADVANCED_FACE ( 'NONE', ( #19999 ), #23607, .T. ) ;
#6432 = DIRECTION ( 'NONE',  ( 0.000000000000000000, -1.000000000000000000, 0.000000000000000000 ) ) ;
#6433 = CARTESIAN_POINT ( 'NONE',  ( -1.002407869896990045, -0.1264236179284866091, 1.872539370024976391 ) ) ;
#6434 = CARTESIAN_POINT ( 'NONE',  ( 0.7185039370078739607, 1.928577636452523993E-17, 1.122047243986960652 ) ) ;
#6435 = CARTESIAN_POINT ( 'NONE',  ( -1.033464566929134687, 0.06523048226347956391, 1.902066929133858775 ) ) ;
#6436 = VECTOR ( 'NONE', #6206, 39.37007874015748143 ) ;
#6437 = CARTESIAN_POINT ( 'NONE',  ( 0.2559055118110235560, 0.1252082647764977408, -0.08806600079302280559 ) ) ;
#6438 = CARTESIAN_POINT ( 'NONE',  ( 0.07405724077823318263, -0.3190216060245144036, 0.1787899950787401604 ) ) ;
#6439 = CARTESIAN_POINT ( 'NONE',  ( -0.1204983120504163341, -0.09842519685039370636, -0.1370941885240791192 ) ) ;
#6440 = CARTESIAN_POINT ( 'NONE',  ( 0.1567662409572586624, 1.919832752026695389E-17, -0.0004999999999998990712 ) ) ;
#6441 = CARTESIAN_POINT ( 'NONE',  ( -1.033464566929134687, 0.06523048226347956391, 0.04183070855389029591 ) ) ;
#6442 = ADVANCED_FACE ( 'NONE', ( #8507 ), #24088, .T. ) ;
#6443 = EDGE_CURVE ( 'NONE', #17493, #27640, #37620, .T. ) ;
#6444 = CARTESIAN_POINT ( 'NONE',  ( -0.7495606340400177148, -0.1264236179284866091, 0.1254921259304885850 ) ) ;
#6445 = ORIENTED_EDGE ( 'NONE', *, *, #5035, .T. ) ;
#6446 = EDGE_LOOP ( 'NONE', ( #33560, #24619, #11277, #8369 ) ) ;
#6447 = CARTESIAN_POINT ( 'NONE',  ( 0.1787899950787401604, -1.129921259788756682, 0.07405724077823318263 ) ) ;
#6448 = CARTESIAN_POINT ( 'NONE',  ( 0.07405724077823318263, -1.193897637741512696, -0.1787899950787401604 ) ) ;
#6449 = CARTESIAN_POINT ( 'NONE',  ( 0.000000000000000000, 1.205361022782826802E-17, -0.09842519685039370636 ) ) ;
#6450 = CARTESIAN_POINT ( 'NONE',  ( 0.1797182628040039087, -0.5743548332050922856, 0.07444174185955046430 ) ) ;
#6451 = DIRECTION ( 'NONE',  ( 0.000000000000000000, -0.000000000000000000, -1.000000000000000000 ) ) ;
#6452 = CARTESIAN_POINT ( 'NONE',  ( -0.8759842519685039353, 0.1574803149606299191, 0.8070866141732283561 ) ) ;
#6453 = CARTESIAN_POINT ( 'NONE',  ( -9.642888182262618425E-18, -0.1948818897637795422, -0.1574803149606299191 ) ) ;
#6454 = VECTOR ( 'NONE', #29910, 39.37007874015748143 ) ;
#6455 = CARTESIAN_POINT ( 'NONE',  ( 0.7646288533564489232, 0.1113553986120547346, 1.865157480207432883 ) ) ;
#6456 = CARTESIAN_POINT ( 'NONE',  ( -0.7646288533564489232, 0.1113553986120547346, 1.432086614065700925 ) ) ;
#6457 = CARTESIAN_POINT ( 'NONE',  ( 0.7185039370078739607, 1.928577636452523993E-17, 0.8169291338582678197 ) ) ;
#6458 = CARTESIAN_POINT ( 'NONE',  ( 0.08530144295876790350, -0.2462454212079008276, -0.03730110279447364230 ) ) ;
#6459 = DIRECTION ( 'NONE',  ( 0.000000000000000000, 1.000000000000000000, 0.000000000000000000 ) ) ;
#6461 = CARTESIAN_POINT ( 'NONE',  ( 0.1605229034655418219, -0.1502651944782444349, -0.02070802253792816683 ) ) ;
#6460 = DIRECTION ( 'NONE',  ( 3.385139170096243171E-15, 1.000000000000000000, -0.000000000000000000 ) ) ;
#6462 = CARTESIAN_POINT ( 'NONE',  ( 0.9873396505805591694, 0.1113553986120547346, 0.2017716534357799352 ) ) ;
#6463 = ORIENTED_EDGE ( 'NONE', *, *, #45495, .F. ) ;
#6464 = CARTESIAN_POINT ( 'NONE',  ( 0.1627249056762490320, 0.5419983459879528231, -0.7609487005970335671 ) ) ;
#6465 = CARTESIAN_POINT ( 'NONE',  ( 0.8107537697050254399, 0.1574803149606300301, 0.7209645668216064784 ) ) ;
#6466 = CARTESIAN_POINT ( 'NONE',  ( 0.07405724077823318263, -0.6230314960092281362, 0.1787899950787401604 ) ) ;
#6467 = CARTESIAN_POINT ( 'NONE',  ( 0.1113553986120547346, -0.9970472440944881942, 0.1113553986120547346 ) ) ;
#6468 = DIRECTION ( 'NONE',  ( -1.000000000000000000, 0.000000000000000000, 0.000000000000000000 ) ) ;
#6469 = CARTESIAN_POINT ( 'NONE',  ( -1.054774247047244096, 0.000000000000000000, 1.951279527505291433 ) ) ;
#6470 = ORIENTED_EDGE ( 'NONE', *, *, #41431, .F. ) ;
#6471 = CARTESIAN_POINT ( 'NONE',  ( -0.7495606340400177148, -0.1264236179284866091, 1.468996062938362046 ) ) ;
#6472 = CARTESIAN_POINT ( 'NONE',  ( 1.002407869896990045, 0.1264236179284866091, 1.528051181048598384 ) ) ;
#6473 = ORIENTED_EDGE ( 'NONE', *, *, #3528, .F. ) ;
#6474 = CARTESIAN_POINT ( 'NONE',  ( 0.9412147342319837628, -0.1574803149606297803, 0.9374999998924736788 ) ) ;
#6475 = CARTESIAN_POINT ( 'NONE',  ( 0.1574803149606300301, -1.294783464459401845, -0.06523048226347956391 ) ) ;
#6476 = CARTESIAN_POINT ( 'NONE',  ( -0.6971942568897637749, 2.189545951927499583E-17, 0.5979330708123780092 ) ) ;
#6477 = CARTESIAN_POINT ( 'NONE',  ( 0.8019270111902717657, 0.1787899950787401604, 0.1968503936470238913 ) ) ;
#6478 = DIRECTION ( 'NONE',  ( 0.000000000000000000, -1.000000000000000000, 0.000000000000000000 ) ) ;
#6479 = CARTESIAN_POINT ( 'NONE',  ( -0.8759842519685039353, -0.1787899950787401882, 0.4847440944344252323 ) ) ;
#6480 = CARTESIAN_POINT ( 'NONE',  ( 1.033464566929133799, 0.000000000000000000, 0.6397637795275591399 ) ) ;
#6481 = ADVANCED_FACE ( 'NONE', ( #41541 ), #8744, .F. ) ;
#6482 = CARTESIAN_POINT ( 'NONE',  ( 0.7185039370078739607, 1.928577636452523993E-17, 1.082677165246803241 ) ) ;
#6483 = CARTESIAN_POINT ( 'NONE',  ( 0.1113553986120547346, -0.2687007872940476716, -0.1113553986120547346 ) ) ;
#6484 = CARTESIAN_POINT ( 'NONE',  ( -1.054774247047244540, -0.07405724077823318263, 1.363188976324188895 ) ) ;
#6485 = ORIENTED_EDGE ( 'NONE', *, *, #4623, .T. ) ;
#6486 = AXIS2_PLACEMENT_3D ( 'NONE', #16302, #30930, #31162 ) ;
#6487 = CARTESIAN_POINT ( 'NONE',  ( -0.8107537697050253289, -0.1574803149606297803, 1.532972440944882608 ) ) ;
#6488 = CARTESIAN_POINT ( 'NONE',  ( -0.7185039370078746268, 0.06523048226347956391, 0.4207677165354331561 ) ) ;
#6489 = CARTESIAN_POINT ( 'NONE',  ( 1.002407869896990045, 0.1264236179284866091, 1.331200787347811110 ) ) ;
#6490 = CONICAL_SURFACE ( 'NONE', #31018, 0.08090551181102362266, 0.9599310885968742602 ) ;
#6491 = STYLED_ITEM ( 'NONE', ( #43289 ), #5351 ) ;
#6492 = ORIENTED_EDGE ( 'NONE', *, *, #2496, .F. ) ;
#6493 = ADVANCED_FACE ( 'NONE', ( #34883 ), #1945, .F. ) ;
#6494 = DIRECTION ( 'NONE',  ( 0.000000000000000000, 0.000000000000000000, -1.000000000000000000 ) ) ;
#6495 = CARTESIAN_POINT ( 'NONE',  ( -1.094772975963752103E-17, -1.719120031221364142, -0.1787899950787401882 ) ) ;
#6496 = ORIENTED_EDGE ( 'NONE', *, *, #25069, .T. ) ;
#6497 = CARTESIAN_POINT ( 'NONE',  ( 0.8107537697050254399, 0.1574803149606300301, 0.8095472440944886383 ) ) ;
#6498 = DIRECTION ( 'NONE',  ( 0.000000000000000000, 0.000000000000000000, -1.000000000000000000 ) ) ;
#6499 = VERTEX_POINT ( 'NONE', #1543 ) ;
#6500 = CARTESIAN_POINT ( 'NONE',  ( 0.8759842519685039353, 0.000000000000000000, 4.498031496062992574 ) ) ;
#6501 = CARTESIAN_POINT ( 'NONE',  ( 3.284318927891251994E-17, -0.3499015747493862127, 0.1787899950787401882 ) ) ;
#6502 = ( BOUNDED_CURVE ( )  B_SPLINE_CURVE ( 2, ( #2812, #13852, #21270, #35895, #3048, #17677, #32328, #46908, #4703 ),
 .UNSPECIFIED., .F., .T. ) 
 B_SPLINE_CURVE_WITH_KNOTS ( ( 3, 2, 2, 2, 3 ),
 ( 0.7399999999999999911, 0.7425000000000000488, 0.7449999999999999956, 0.7475000000000000533, 0.7500000000000000000 ),
 .UNSPECIFIED. ) 
 CURVE ( )  GEOMETRIC_REPRESENTATION_ITEM ( )  RATIONAL_B_SPLINE_CURVE ( ( 1.000000000000000000, 0.9238795325112869605, 1.000000000000000000, 0.9238795325112869605, 1.000000000000000000, 0.9238795325112869605, 1.000000000000000000, 0.9238795325112869605, 1.000000000000000000 ) ) 
 REPRESENTATION_ITEM ( '' )  ) ;
#6503 = CARTESIAN_POINT ( 'NONE',  ( 0.1264236179284866091, -0.8026574802611967652, -0.1264236179284866091 ) ) ;
#6504 = CARTESIAN_POINT ( 'NONE',  ( -0.2471921300642929697, -0.09379707428445160922, -0.03645430680490755609 ) ) ;
#6505 = DIRECTION ( 'NONE',  ( 0.000000000000000000, 0.000000000000000000, -1.000000000000000000 ) ) ;
#6506 = CARTESIAN_POINT ( 'NONE',  ( 1.002407869896990045, -0.1264236179284866091, 1.670767716481669440 ) ) ;
#6507 = CARTESIAN_POINT ( 'NONE',  ( 0.6971942568897637749, 2.189545951927499583E-17, 0.2780511810485988278 ) ) ;
#6508 = PRODUCT_DEFINITION_SHAPE ( 'NONE', 'NONE',  #47471 ) ;
#6509 = CARTESIAN_POINT ( 'NONE',  ( -0.07405724077823318263, -0.04835231468593165216, 0.1787899950787401604 ) ) ;
#6510 = CARTESIAN_POINT ( 'NONE',  ( 0.2559055118110236671, -0.07952748568939312090, -0.3079936629965072115 ) ) ;
#6511 = CARTESIAN_POINT ( 'NONE',  ( 0.8759842519685039353, 0.1787899950787401882, 0.6225393700249762796 ) ) ;
#6512 = ADVANCED_FACE ( 'NONE', ( #45397 ), #31983, .T. ) ;
#6513 = CARTESIAN_POINT ( 'NONE',  ( -0.6971942568897648851, 0.07405724077823318263, 0.9891732282926936071 ) ) ;
#6515 = CARTESIAN_POINT ( 'NONE',  ( 0.7185039370078739607, 1.928577636452523993E-17, 1.712598425089322918 ) ) ;
#6514 = CARTESIAN_POINT ( 'NONE',  ( 0.1113553986120547346, -0.9478346456692913202, -0.1113553986120547346 ) ) ;
#6516 = CARTESIAN_POINT ( 'NONE',  ( 3.301370929368692659E-17, -1.684098927693281400, 0.1797182628040039365 ) ) ;
#6517 = CARTESIAN_POINT ( 'NONE',  ( 0.1574803149606299191, -0.5098425195775118102, -1.928577636452523993E-17 ) ) ;
#6518 = CIRCLE ( 'NONE', #8063, 0.1013779527559055538 ) ;
#6519 = CARTESIAN_POINT ( 'NONE',  ( 1.002407869896990045, -0.1264236179284866091, 1.636318897584031484 ) ) ;
#6521 = CARTESIAN_POINT ( 'NONE',  ( -1.033464566929133799, 0.000000000000000000, 1.820866141732283561 ) ) ;
#6520 = CARTESIAN_POINT ( 'NONE',  ( 1.002407869896990045, -0.1264236179284866091, 1.985728346402929168 ) ) ;
#6522 = B_SPLINE_CURVE_WITH_KNOTS ( 'NONE', 3,
 ( #41729, #38160, #41962, #15907, #5323, #19711, #23785, #34829, #16601, #38398, #5568, #34577, #1973, #1731 ),
 .UNSPECIFIED., .F., .F.,
 ( 4, 2, 2, 2, 2, 2, 4 ),
 ( 0.000000000000000000, 0.1250000000000001110, 0.2500000000000002220, 0.3750000000000003331, 0.4375000000000003886, 0.5000000000000004441, 1.000000000000000000 ),
 .UNSPECIFIED. ) ;
#6523 = CIRCLE ( 'NONE', #8066, 0.1377952755905509641 ) ;
#6524 = VECTOR ( 'NONE', #43023, 39.37007874015748143 ) ;
#6525 = ORIENTED_EDGE ( 'NONE', *, *, #8153, .T. ) ;
#6526 = DIRECTION ( 'NONE',  ( -9.133235551360036525E-15, 0.2126700594527874688, -0.9771240687918542056 ) ) ;
#6527 = CARTESIAN_POINT ( 'NONE',  ( 0.2016454051087482324, -0.1790725142610753162, -0.3070225280279249569 ) ) ;
#6529 = CARTESIAN_POINT ( 'NONE',  ( 0.1264236179284866091, -0.1382874015210397711, -0.1264236179284866091 ) ) ;
#6528 = CARTESIAN_POINT ( 'NONE',  ( 0.1574803149606299191, -0.9035433069790866911, -1.928577636452523993E-17 ) ) ;
#6530 = CARTESIAN_POINT ( 'NONE',  ( 0.8759842519685039353, -0.1787899950787401882, 0.6422244093950550958 ) ) ;
#6531 = CARTESIAN_POINT ( 'NONE',  ( 0.1787899950787401604, -0.9675196849856075865, 0.07405724077823318263 ) ) ;
#6532 = CARTESIAN_POINT ( 'NONE',  ( 1.002407869896990045, 0.1264236179284866091, 0.1500984251430867999 ) ) ;
#6533 = DIRECTION ( 'NONE',  ( 0.000000000000000000, 1.000000000000000000, 0.000000000000000000 ) ) ;
#6534 = CARTESIAN_POINT ( 'NONE',  ( 0.7495606340400177148, 0.1264236179284866091, 0.5487204723871811352 ) ) ;
#6535 = FACE_OUTER_BOUND ( 'NONE', #33407, .T. ) ;
#6536 = CARTESIAN_POINT ( 'NONE',  ( -1.054774247047244540, -0.07405724077823318263, 1.397637795221827295 ) ) ;
#6537 = VERTEX_POINT ( 'NONE', #8093 ) ;
#6538 = CARTESIAN_POINT ( 'NONE',  ( -0.2713482210566314223, -0.1500601874062439112, -0.9507959855109898717 ) ) ;
#6539 = CARTESIAN_POINT ( 'NONE',  ( 1.002407869896990045, 0.1264236179284866091, 1.134350393647023614 ) ) ;
#6540 = CARTESIAN_POINT ( 'NONE',  ( -0.1574803149606297803, -1.156988188868850465, 0.06523048226347956391 ) ) ;
#6541 = CARTESIAN_POINT ( 'NONE',  ( -0.9412147342319837628, -0.1574803149606297803, 0.7012795274515276622 ) ) ;
#6542 = CARTESIAN_POINT ( 'NONE',  ( -1.033464566929133799, 0.000000000000000000, 0.3543307085538902057 ) ) ;
#6543 = CARTESIAN_POINT ( 'NONE',  ( 1.054774247047244540, -0.07405724077823318263, 1.791338582623401177 ) ) ;
#6544 = CARTESIAN_POINT ( 'NONE',  ( -0.9412147342319837628, 0.1574803149606300301, 1.355807086614173596 ) ) ;
#6545 = CARTESIAN_POINT ( 'NONE',  ( -0.7495606340400177148, 0.1264236179284866091, 0.8243110235682834519 ) ) ;
#6546 = CARTESIAN_POINT ( 'NONE',  ( 0.8107537697050254399, -0.1574803149606297803, 1.798720472333418918 ) ) ;
#6547 = CARTESIAN_POINT ( 'NONE',  ( -0.8621503180216169016, -0.1583841767695347846, 0.03937007874015844427 ) ) ;
#6548 = CARTESIAN_POINT ( 'NONE',  ( 0.6971942568897637749, 2.189545951927499583E-17, 0.3223425196312759144 ) ) ;
#6549 = CARTESIAN_POINT ( 'NONE',  ( -0.8759842519685039353, -0.1787899950787401882, 0.09104330703285078152 ) ) ;
#6550 = CARTESIAN_POINT ( 'NONE',  ( -0.6971942568897637749, 2.189545951927499583E-17, 0.6323818897100157432 ) ) ;
#6551 = CARTESIAN_POINT ( 'NONE',  ( 0.8759842519685039353, 0.1574803149606299191, 1.584645669183810890 ) ) ;
#6552 = ORIENTED_EDGE ( 'NONE', *, *, #11248, .F. ) ;
#6553 = EDGE_CURVE ( 'NONE', #19219, #46651, #28772, .T. ) ;
#6554 = B_SPLINE_CURVE_WITH_KNOTS ( 'NONE', 3,
 ( #33135, #25925, #43644, #32898, #36705, #47004, #16, #263, #32426, #40507, #3400, #14665, #28841, #18011, #29339, #7696, #43400, #39798, #11311, #43883, #25208, #14908, #11083 ),
 .UNSPECIFIED., .F., .F.,
 ( 4, 2, 2, 1, 1, 1, 2, 2, 2, 1, 1, 2, 2, 4 ),
 ( 0.000000000000000000, 0.2499999999999987788, 0.3749999999999982792, 0.4374999999999980571, 0.4687499999999980016, 0.4843749999999980571, 0.4921874999999981126, 0.4999999999999981126, 0.6249999999999982236, 0.6874999999999983347, 0.7187499999999982236, 0.7343749999999983347, 0.7499999999999983347, 1.000000000000000000 ),
 .UNSPECIFIED. ) ;
#6555 = CARTESIAN_POINT ( 'NONE',  ( 0.1787899950787401604, -0.06200787396198446239, -0.07405724077823318263 ) ) ;
#6556 = CARTESIAN_POINT ( 'NONE',  ( 0.6971942568897637749, 2.189545951927499583E-17, 0.7160433070328504623 ) ) ;
#6557 = CARTESIAN_POINT ( 'NONE',  ( -0.7495606340400177148, 0.1264236179284866091, 1.690452755851748146 ) ) ;
#6558 = CIRCLE ( 'NONE', #5022, 0.1003937007874011050 ) ;
#6559 = EDGE_CURVE ( 'NONE', #27914, #36578, #47416, .T. ) ;
#6560 = CARTESIAN_POINT ( 'NONE',  ( 0.1264236179284866091, -1.471948818843874074, -0.1264236179284866091 ) ) ;
#6561 = DIRECTION ( 'NONE',  ( 1.000000000000000000, 0.000000000000000000, -1.822029033848725275E-16 ) ) ;
#6562 = CARTESIAN_POINT ( 'NONE',  ( 0.000000000000000000, 0.000000000000000000, -0.3149606299212598381 ) ) ;
#6563 = CARTESIAN_POINT ( 'NONE',  ( 0.1264236179284866091, -1.300812944607191213, 0.1264236179284866091 ) ) ;
#6564 = ORIENTED_EDGE ( 'NONE', *, *, #7127, .F. ) ;
#6565 = CARTESIAN_POINT ( 'NONE',  ( -0.07405724077823318263, -0.04724409443442544737, -0.1787899950787401604 ) ) ;
#6566 = VECTOR ( 'NONE', #5579, 39.37007874015748143 ) ;
#6567 = AXIS2_PLACEMENT_3D ( 'NONE', #25527, #6324, #31990 ) ;
#6568 = EDGE_LOOP ( 'NONE', ( #32510, #35002, #40047, #34155, #34537 ) ) ;
#6569 = CARTESIAN_POINT ( 'NONE',  ( 0.6195511811023612925, 0.6102362204724401940, 0.9891732283464566011 ) ) ;
#6570 = CARTESIAN_POINT ( 'NONE',  ( 0.8107537697050253289, 0.1574803149606300301, 1.951279527559056870 ) ) ;
#6571 = CARTESIAN_POINT ( 'NONE',  ( 0.1787899950787401604, -1.439960629867495401, -0.07405724077823318263 ) ) ;
#6572 = EDGE_CURVE ( 'NONE', #38514, #8914, #33298, .T. ) ;
#6573 = CARTESIAN_POINT ( 'NONE',  ( -1.054774247047244540, -0.07405724077823318263, 0.3789370078202520253 ) ) ;
#6574 = CARTESIAN_POINT ( 'NONE',  ( -0.7144400811684905594, 0.03384972598730602578, 1.982630989409186251 ) ) ;
#6575 = CYLINDRICAL_SURFACE ( 'NONE', #21800, 0.1574803149606299191 ) ;
#6576 = CARTESIAN_POINT ( 'NONE',  ( 1.054774247047244540, -0.07405724077823318263, 1.476377952702141449 ) ) ;
#6577 = CARTESIAN_POINT ( 'NONE',  ( 1.054774247047244096, 0.000000000000000000, 0.1796259841982051075 ) ) ;
#6578 = CARTESIAN_POINT ( 'NONE',  ( -0.7646288533564489232, 0.1113553986120547346, 1.914370078740157632 ) ) ;
#6579 = CARTESIAN_POINT ( 'NONE',  ( 0.9412147342319837628, 0.1574803149606300301, 1.670767716535433545 ) ) ;
#6581 = CARTESIAN_POINT ( 'NONE',  ( 1.033464566929134687, -0.06523048226347956391, 1.532972440837355066 ) ) ;
#6580 = CARTESIAN_POINT ( 'NONE',  ( 0.1637325492971695717, -0.08225662854574337934, 0.1377952755905512972 ) ) ;
#6582 = CARTESIAN_POINT ( 'NONE',  ( 0.7646288533564489232, -0.1113553986120547346, 0.7726377951680629685 ) ) ;
#6583 = CARTESIAN_POINT ( 'NONE',  ( -0.7185039370078746268, 0.06523048226347956391, 1.710137795168064079 ) ) ;
#6584 = CARTESIAN_POINT ( 'NONE',  ( -0.1264236179284866091, 0.004429133912031228346, 0.1264236179284866091 ) ) ;
#6585 = CARTESIAN_POINT ( 'NONE',  ( 1.054774247047244540, -0.07405724077823318263, 0.1377952755367876370 ) ) ;
#6587 = CARTESIAN_POINT ( 'NONE',  ( -0.9412147342319837628, -0.1574803149606297803, 0.5437992124908980207 ) ) ;
#6586 = CARTESIAN_POINT ( 'NONE',  ( 0.8759842519685039353, -0.1787899950787401882, 1.193405511757259951 ) ) ;
#6588 = DIRECTION ( 'NONE',  ( 0.000000000000000000, 0.000000000000000000, 1.000000000000000000 ) ) ;
#6589 = CARTESIAN_POINT ( 'NONE',  ( 0.7185039370078746268, -0.06523048226347956391, 0.4552165353255435698 ) ) ;
#6590 = ORIENTED_EDGE ( 'NONE', *, *, #40334, .T. ) ;
#6591 = EDGE_CURVE ( 'NONE', #2533, #27462, #26573, .T. ) ;
#6592 = CARTESIAN_POINT ( 'NONE',  ( -1.033464566929133799, 1.928577636452524610E-17, 2.869337061179095023E-17 ) ) ;
#6593 = CARTESIAN_POINT ( 'NONE',  ( 0.9342451777971542137, 0.1605301618127781826, 0.03936975837968165887 ) ) ;
#6594 = CARTESIAN_POINT ( 'NONE',  ( -0.7646288533564489232, -0.1113553986120547346, 0.3395669290263311213 ) ) ;
#6595 = EDGE_LOOP ( 'NONE', ( #9256, #30277, #9094, #9082 ) ) ;
#6596 = CARTESIAN_POINT ( 'NONE',  ( 1.002407869896990045, -0.1264236179284866091, 1.434547244040724534 ) ) ;
#6598 = CARTESIAN_POINT ( 'NONE',  ( -0.8107537697050234415, -0.1574803149606297803, 0.2239173227271187561 ) ) ;
#6597 = CARTESIAN_POINT ( 'NONE',  ( -0.9873396505805591694, 0.1113553986120547346, 0.09350393700787401619 ) ) ;
#6599 = CARTESIAN_POINT ( 'NONE',  ( -0.07405724077823318263, 0.04625984257344856188, 0.1787899950787401604 ) ) ;
#6600 = EDGE_LOOP ( 'NONE', ( #13462, #35039, #19151 ) ) ;
#6601 = CARTESIAN_POINT ( 'NONE',  ( 0.1600813888244884409, -0.05392405859257631134, -0.1404791960284777486 ) ) ;
#6602 = EDGE_CURVE ( 'NONE', #31572, #25178, #8920, .T. ) ;
#6603 = ORIENTED_EDGE ( 'NONE', *, *, #5035, .F. ) ;
#6604 = CARTESIAN_POINT ( 'NONE',  ( 0.2471922904502826812, 0.03219022224904106305, 0.1427165354330708902 ) ) ;
#6605 = ( NAMED_UNIT ( * ) SI_UNIT ( $, .STERADIAN. ) SOLID_ANGLE_UNIT ( ) ) ;
#6606 = CARTESIAN_POINT ( 'NONE',  ( 0.7495606340400177148, 0.1264236179284866091, 0.5142716534895434011 ) ) ;
#6607 = ORIENTED_EDGE ( 'NONE', *, *, #10130, .T. ) ;
#6608 = CARTESIAN_POINT ( 'NONE',  ( -0.6971942568897648851, 0.07405724077823318263, 1.377952755851748368 ) ) ;
#6610 = CARTESIAN_POINT ( 'NONE',  ( 0.1787899950787401604, -1.641732283410802573, 0.07405724077823318263 ) ) ;
#6609 = CARTESIAN_POINT ( 'NONE',  ( -0.1113553986120547346, -0.4163385825696385711, -0.1113553986120547346 ) ) ;
#6611 = CARTESIAN_POINT ( 'NONE',  ( -0.7495606340400177148, -0.1264236179284866091, 1.154035433017102319 ) ) ;
#6612 = CARTESIAN_POINT ( 'NONE',  ( -0.8759842519685039353, -0.1574803149606299191, 0.03937007874015747977 ) ) ;
#6613 = VERTEX_POINT ( 'NONE', #18873 ) ;
#6614 = CARTESIAN_POINT ( 'NONE',  ( -0.6971942568897648851, -0.07405724077823297447, 1.146653543253323582 ) ) ;
#6615 = ADVANCED_FACE ( 'NONE', ( #12181 ), #8565, .F. ) ;
#6616 = CARTESIAN_POINT ( 'NONE',  ( -0.6971942568897626646, 0.07405724077823318263, 0.7529527558517473684 ) ) ;
#6617 = EDGE_CURVE ( 'NONE', #22586, #4710, #24459, .T. ) ;
#6618 = CARTESIAN_POINT ( 'NONE',  ( -0.7646288533564489232, -0.1113553986120547346, 0.3494094488188976277 ) ) ;
#6619 = DIRECTION ( 'NONE',  ( 1.822029033848725028E-16, 0.000000000000000000, 1.000000000000000000 ) ) ;
#6620 = CARTESIAN_POINT ( 'NONE',  ( 0.07405724077823318263, -0.7127223934260893401, 0.1787899950787401604 ) ) ;
#6621 = ORIENTED_EDGE ( 'NONE', *, *, #38033, .F. ) ;
#6622 = CARTESIAN_POINT ( 'NONE',  ( -0.07443497905850630925, -0.08956195077354547895, 0.1394259959420596495 ) ) ;
#6623 = CARTESIAN_POINT ( 'NONE',  ( -0.7646288533564489232, -0.1113553986120547346, 0.6545275589475906264 ) ) ;
#6624 = VERTEX_POINT ( 'NONE', #16949 ) ;
#6625 = CARTESIAN_POINT ( 'NONE',  ( -0.6971942568897637749, 2.189545951927499583E-17, 0.5536417322297008115 ) ) ;
#6626 = CARTESIAN_POINT ( 'NONE',  ( 0.03372458374097409700, 1.170665729134817035, -0.1030065087509350469 ) ) ;
#6627 = CARTESIAN_POINT ( 'NONE',  ( -1.002407869896990045, -0.1264236179284866091, 1.675688976324189117 ) ) ;
#6628 = LINE ( 'NONE', #21244, #26508 ) ;
#6629 = SURFACE_STYLE_USAGE ( .BOTH. , #10003 ) ;
#6630 = CARTESIAN_POINT ( 'NONE',  ( 1.033464566929133799, 0.000000000000000000, 0.6397637795275591399 ) ) ;
#6631 = CARTESIAN_POINT ( 'NONE',  ( -0.07444174185955065859, -0.9139217623389520595, -0.1797182628040039087 ) ) ;
#6632 = CARTESIAN_POINT ( 'NONE',  ( 0.2471922904502826257, 0.05203836715086061077, 0.1197978718291115713 ) ) ;
#6633 = CARTESIAN_POINT ( 'NONE',  ( -0.7185039370078739607, 1.928577636452523993E-17, 1.318897637687747926 ) ) ;
#6634 = CARTESIAN_POINT ( 'NONE',  ( 1.054774247047244540, 0.07405724077823318263, 0.7775590550643479704 ) ) ;
#6635 = CARTESIAN_POINT ( 'NONE',  ( -0.06523048226347956391, -0.5319881889763778959, 0.1574803149606297803 ) ) ;
#6636 = LINE ( 'NONE', #35425, #5472 ) ;
#6637 = EDGE_CURVE ( 'NONE', #36696, #42555, #31118, .T. ) ;
#6638 = CARTESIAN_POINT ( 'NONE',  ( 0.9873396505805591694, 0.1113553986120547346, 0.1624015746956226358 ) ) ;
#6639 = CARTESIAN_POINT ( 'NONE',  ( 1.033464566929134687, -0.06523048226347956391, 1.188484251968505268 ) ) ;
#6641 = FILL_AREA_STYLE_COLOUR ( '', #45353 ) ;
#6640 = CARTESIAN_POINT ( 'NONE',  ( 0.7479160358676916198, -0.1116595215576704353, 1.985525107522427835 ) ) ;
#6642 = CARTESIAN_POINT ( 'NONE',  ( 1.033464566929133799, 0.000000000000000000, 0.3149606298137326843 ) ) ;
#6643 = AXIS2_PLACEMENT_3D ( 'NONE', #1249, #38393, #30994 ) ;
#6645 = CARTESIAN_POINT ( 'NONE',  ( -0.1574803149606299191, 1.928577636452524610E-17, -0.1574803149606298636 ) ) ;
#6644 = CARTESIAN_POINT ( 'NONE',  ( 0.9500414927467377701, -0.1787899950787401604, 0.6446850393163160442 ) ) ;
#6646 = DIRECTION ( 'NONE',  ( 1.000000000000000000, -3.469446951953614583E-15, 0.000000000000000000 ) ) ;
#6647 = ORIENTED_EDGE ( 'NONE', *, *, #1809, .F. ) ;
#6648 = EDGE_CURVE ( 'NONE', #26440, #30928, #5142, .T. ) ;
#6649 = CARTESIAN_POINT ( 'NONE',  ( 0.1633669211800945209, 0.08028805200495257866, 0.1390640086940820308 ) ) ;
#6650 = DIRECTION ( 'NONE',  ( 0.000000000000000000, 0.000000000000000000, 1.000000000000000000 ) ) ;
#6651 = CARTESIAN_POINT ( 'NONE',  ( 0.8019270111902717657, 0.1787899950787401604, 1.058070866087969186 ) ) ;
#6652 = ORIENTED_EDGE ( 'NONE', *, *, #30354, .F. ) ;
#6653 = FACE_OUTER_BOUND ( 'NONE', #5602, .T. ) ;
#6654 = CARTESIAN_POINT ( 'NONE',  ( 0.000000000000000000, -0.09842519685039370636, 0.000000000000000000 ) ) ;
#6655 = CARTESIAN_POINT ( 'NONE',  ( 0.07444174185955046430, 0.1441491038027811755, -0.1797182628040039087 ) ) ;
#6656 = CARTESIAN_POINT ( 'NONE',  ( -0.1264236179284866091, -1.102854330654897685, 0.1264236179284866091 ) ) ;
#6657 = CARTESIAN_POINT ( 'NONE',  ( 0.1574803149606300301, -1.540846456692913868, -0.06523048226347956391 ) ) ;
#6658 = FACE_OUTER_BOUND ( 'NONE', #42482, .T. ) ;
#6659 = VERTEX_POINT ( 'NONE', #42085 ) ;
#6660 = CARTESIAN_POINT ( 'NONE',  ( -0.6971942568897626646, -0.07405724077823297447, 0.04429133852891373180 ) ) ;
#6661 = ORIENTED_EDGE ( 'NONE', *, *, #10572, .T. ) ;
#6662 = CARTESIAN_POINT ( 'NONE',  ( 0.6971942568897637749, 2.189545951927499583E-17, 1.975885826717889815 ) ) ;
#6663 = VERTEX_POINT ( 'NONE', #20062 ) ;
#6664 = CARTESIAN_POINT ( 'NONE',  ( 0.1113553986120547346, -1.449803149498771759, -0.1113553986120547346 ) ) ;
#6665 = CARTESIAN_POINT ( 'NONE',  ( -0.8019270111902716547, -0.1787899950787401604, 1.904527559001354398 ) ) ;
#6666 = CARTESIAN_POINT ( 'NONE',  ( -1.054774247047244540, -0.07405724077823318263, 1.476377952702141449 ) ) ;
#6667 = CARTESIAN_POINT ( 'NONE',  ( -0.6971942568897626646, -0.07405724077823297447, 0.4035433070328508509 ) ) ;
#6668 = CARTESIAN_POINT ( 'NONE',  ( -1.033464566929133799, 0.000000000000000000, 1.811023621939716444 ) ) ;
#6669 = CARTESIAN_POINT ( 'NONE',  ( -0.8759842519685039353, -0.1787899950787401882, 1.828248031442299082 ) ) ;
#6670 = CARTESIAN_POINT ( 'NONE',  ( -0.7185039370078746268, 0.06523048226347956391, 1.956200787401575880 ) ) ;
#6671 = CARTESIAN_POINT ( 'NONE',  ( 0.1574803149606299746, 0.3740157480314960647, 0.9783464566929134243 ) ) ;
#6672 = CARTESIAN_POINT ( 'NONE',  ( 0.1264236179284866091, -0.2378208186229397725, 0.1264236179284866091 ) ) ;
#6673 = LINE ( 'NONE', #18411, #8818 ) ;
#6674 = FACE_OUTER_BOUND ( 'NONE', #2026, .T. ) ;
#6675 = AXIS2_PLACEMENT_3D ( 'NONE', #36792, #26011, #3945 ) ;
#6676 = ( BOUNDED_CURVE ( )  B_SPLINE_CURVE ( 2, ( #35703, #21066, #17712, #24221, #46227, #32365, #43100, #5980, #16781 ),
 .UNSPECIFIED., .F., .T. ) 
 B_SPLINE_CURVE_WITH_KNOTS ( ( 3, 2, 2, 2, 3 ),
 ( 0.6700000000000000400, 0.6724999999999999867, 0.6750000000000000444, 0.6774999999999999911, 0.6800000000000000488 ),
 .UNSPECIFIED. ) 
 CURVE ( )  GEOMETRIC_REPRESENTATION_ITEM ( )  RATIONAL_B_SPLINE_CURVE ( ( 1.000000000000000000, 0.9238795325112899581, 1.000000000000000000, 0.9238795325112869605, 1.000000000000000000, 0.9238795325112869605, 1.000000000000000000, 0.9238795325112869605, 1.000000000000000000 ) ) 
 REPRESENTATION_ITEM ( '' )  ) ;
#6677 = CARTESIAN_POINT ( 'NONE',  ( -0.8759842519685039353, 0.1787899950787401882, 0.2288385826234019815 ) ) ;
#6678 = VERTEX_POINT ( 'NONE', #38516 ) ;
#6679 = CARTESIAN_POINT ( 'NONE',  ( -0.6971942568897648851, 0.07405724077823318263, 1.264763779473795813 ) ) ;
#6680 = EDGE_LOOP ( 'NONE', ( #13863, #40681, #3190, #33598 ) ) ;
#6681 = CARTESIAN_POINT ( 'NONE',  ( 0.1787899950787401604, -1.361220472387181690, 0.07405724077823318263 ) ) ;
#6682 = DIRECTION ( 'NONE',  ( -3.469446951953613794E-15, -1.000000000000000000, -3.652049423109077687E-16 ) ) ;
#6683 = ( CONVERSION_BASED_UNIT ( 'INCH', #46465 ) LENGTH_UNIT ( ) NAMED_UNIT ( #20364 ) ) ;
#6684 = CARTESIAN_POINT ( 'NONE',  ( -0.1270800023317771588, -0.6260280615515491087, 0.1270800023317771588 ) ) ;
#6685 = CARTESIAN_POINT ( 'NONE',  ( 0.5660731898098425585, -0.09842519685039370636, 1.205361022782828805E-17 ) ) ;
#6686 = CARTESIAN_POINT ( 'NONE',  ( -0.9412147342319837628, 0.1574803149606300301, 0.9916338581601894520 ) ) ;
#6687 = CARTESIAN_POINT ( 'NONE',  ( -0.7646288533564489232, -0.1113553986120547346, 0.6643700787401575214 ) ) ;
#6688 = CARTESIAN_POINT ( 'NONE',  ( 0.06523048226347956391, -0.1579724409448819422, -0.1574803149606300301 ) ) ;
#6689 = ORIENTED_EDGE ( 'NONE', *, *, #16001, .T. ) ;
#6690 = CARTESIAN_POINT ( 'NONE',  ( 1.033464566929133799, 0.000000000000000000, 1.850393700679873854 ) ) ;
#6691 = ORIENTED_EDGE ( 'NONE', *, *, #380, .F. ) ;
#6692 = EDGE_CURVE ( 'NONE', #42489, #28106, #22537, .T. ) ;
#6693 = CARTESIAN_POINT ( 'NONE',  ( 0.7185039370078739607, 1.928577636452523993E-17, 0.2165354329633393804 ) ) ;
#6694 = CARTESIAN_POINT ( 'NONE',  ( 0.9412147342319837628, -0.1574803149606297803, 0.7504921259842516346 ) ) ;
#6695 = LINE ( 'NONE', #21311, #32152 ) ;
#6696 = ADVANCED_FACE ( 'NONE', ( #35411 ), #34705, .T. ) ;
#6697 = VECTOR ( 'NONE', #42238, 39.37007874015748143 ) ;
#6699 = DIRECTION ( 'NONE',  ( 0.000000000000000000, -1.000000000000000000, 0.000000000000000000 ) ) ;
#6698 = CARTESIAN_POINT ( 'NONE',  ( 0.4755220087074803481, -0.09842519685039370636, 1.205361022782828805E-17 ) ) ;
#6700 = CARTESIAN_POINT ( 'NONE',  ( 1.033464566929134687, 0.06523048226347956391, 0.1599409447743626866 ) ) ;
#6701 = EDGE_CURVE ( 'NONE', #19636, #19079, #41734, .T. ) ;
#6702 = ORIENTED_EDGE ( 'NONE', *, *, #5516, .F. ) ;
#6703 = ADVANCED_FACE ( 'NONE', ( #16715 ), #31346, .F. ) ;
#6704 = ORIENTED_EDGE ( 'NONE', *, *, #26274, .T. ) ;
#6705 = CARTESIAN_POINT ( 'NONE',  ( 0.7185039370078739607, 1.928577636452523993E-17, 0.8169291338582678197 ) ) ;
#6706 = CARTESIAN_POINT ( 'NONE',  ( 0.1574803149606299746, 0.2876548164643190630, -0.2627373885913885099 ) ) ;
#6707 = CARTESIAN_POINT ( 'NONE',  ( -0.06523048226347956391, -1.545767716427905336, 0.1574803149606297803 ) ) ;
#6708 = CARTESIAN_POINT ( 'NONE',  ( -0.07405724077823318263, -0.5639763778989922427, -0.1787899950787401604 ) ) ;
#6709 = CARTESIAN_POINT ( 'NONE',  ( 0.06523048226347956391, -1.102854330708662456, -0.1574803149606300301 ) ) ;
#6710 = CARTESIAN_POINT ( 'NONE',  ( 0.7185039370078739607, 1.928577636452523993E-17, 1.043307086506645831 ) ) ;
#6711 = CARTESIAN_POINT ( 'NONE',  ( -0.8759842519685039353, 0.1787899950787401882, 0.3469488188438744070 ) ) ;
#6712 = VERTEX_POINT ( 'NONE', #42336 ) ;
#6713 = CARTESIAN_POINT ( 'NONE',  ( -0.6971942568897648851, -0.07405724077823297447, 1.545275590497416696 ) ) ;
#6714 = CARTESIAN_POINT ( 'NONE',  ( 0.6971942568897648851, -0.07405724077823297447, 1.584645669237574994 ) ) ;
#6715 = CARTESIAN_POINT ( 'NONE',  ( 0.8759842519685039353, 0.000000000000000000, 4.498031496062992574 ) ) ;
#6716 = CARTESIAN_POINT ( 'NONE',  ( -0.7495606340400177148, 0.1264236179284866091, 0.6717519684501732646 ) ) ;
#6717 = CARTESIAN_POINT ( 'NONE',  ( 0.8019270111902717657, 0.1787899950787401604, 0.1574803149068664809 ) ) ;
#6718 = FACE_OUTER_BOUND ( 'NONE', #13424, .T. ) ;
#6719 = CARTESIAN_POINT ( 'NONE',  ( 0.8759842519685039353, -0.1787899950787401882, 0.7258858267178898149 ) ) ;
#6720 = CARTESIAN_POINT ( 'NONE',  ( -0.9500414927467377701, -0.1787899950787401604, 0.7234251967966300878 ) ) ;
#6721 = CARTESIAN_POINT ( 'NONE',  ( 0.1607876024857142205, -0.09201407021838738098, 0.1926022046198413995 ) ) ;
#6722 = DIRECTION ( 'NONE',  ( -1.000000000000000000, -0.000000000000000000, 0.000000000000000000 ) ) ;
#6723 = CARTESIAN_POINT ( 'NONE',  ( -0.1574803149606299191, -0.1751968502861738219, 0.000000000000000000 ) ) ;
#6724 = CARTESIAN_POINT ( 'NONE',  ( -0.8759842519685039353, -0.1787899950787401882, 1.355807086560409491 ) ) ;
#6725 = ORIENTED_EDGE ( 'NONE', *, *, #14530, .F. ) ;
#6726 = CARTESIAN_POINT ( 'NONE',  ( -0.9412147342319837628, 0.1574803149606300301, 0.5290354330708663122 ) ) ;
#6727 = CARTESIAN_POINT ( 'NONE',  ( 0.8759842519685039353, -0.1787899950787401882, 1.513287401521039355 ) ) ;
#6728 = CARTESIAN_POINT ( 'NONE',  ( -0.1344904043211537503, -0.09851384275058189255, -0.1217015355611421323 ) ) ;
#6729 = CARTESIAN_POINT ( 'NONE',  ( -0.1574803149606299191, 0.07021257666614952320, -0.1553045758542780375 ) ) ;
#6730 = ORIENTED_EDGE ( 'NONE', *, *, #12641, .F. ) ;
#6731 = ADVANCED_FACE ( 'NONE', ( #24154 ), #29206, .T. ) ;
#6732 = AXIS2_PLACEMENT_3D ( 'NONE', #1386, #16044, #1872 ) ;
#6733 = ORIENTED_EDGE ( 'NONE', *, *, #4460, .T. ) ;
#6734 = LINE ( 'NONE', #2664, #33870 ) ;
#6735 = ORIENTED_EDGE ( 'NONE', *, *, #15124, .T. ) ;
#6736 = CARTESIAN_POINT ( 'NONE',  ( 0.9500414927467378812, 0.1787899950787401604, 1.407480314906865981 ) ) ;
#6737 = CARTESIAN_POINT ( 'NONE',  ( 0.000000000000000000, 0.000000000000000000, 0.09842519685039370636 ) ) ;
#6738 = AXIS2_PLACEMENT_3D ( 'NONE', #20587, #46218, #20821 ) ;
#6739 = CARTESIAN_POINT ( 'NONE',  ( 0.1787899950787401882, -0.8469488188438739629, -2.189545951927503898E-17 ) ) ;
#6740 = CARTESIAN_POINT ( 'NONE',  ( 0.000000000000000000, 0.000000000000000000, -0.06545654452343109553 ) ) ;
#6741 = DIRECTION ( 'NONE',  ( 1.000000000000000000, 0.000000000000000000, 0.000000000000000000 ) ) ;
#6742 = ( NAMED_UNIT ( * ) PLANE_ANGLE_UNIT ( ) SI_UNIT ( $, .RADIAN. ) ) ;
#6743 = CARTESIAN_POINT ( 'NONE',  ( 0.8759842519685039353, 0.1787899950787401882, 0.2682086613635594752 ) ) ;
#6744 = CARTESIAN_POINT ( 'NONE',  ( -0.1787899950787401882, -0.09510428318986871576, 0.000000000000000000 ) ) ;
#6745 = CARTESIAN_POINT ( 'NONE',  ( -0.1264236179284866091, -0.2810039369541106336, -0.1264236179284866091 ) ) ;
#6746 = FACE_OUTER_BOUND ( 'NONE', #18691, .T. ) ;
#6747 = DIRECTION ( 'NONE',  ( -1.000000000000000000, 0.000000000000000000, 0.000000000000000000 ) ) ;
#6748 = CARTESIAN_POINT ( 'NONE',  ( 0.8759842519685039353, -0.1787899950787401882, 0.6422244093950550958 ) ) ;
#6749 = EDGE_CURVE ( 'NONE', #4137, #28233, #13821, .T. ) ;
#6750 = CARTESIAN_POINT ( 'NONE',  ( -0.6971942568897637749, 2.189545951927499583E-17, 0.9916338582139527791 ) ) ;
#6752 = DIRECTION ( 'NONE',  ( 0.000000000000000000, 0.000000000000000000, 1.000000000000000000 ) ) ;
#6751 = CARTESIAN_POINT ( 'NONE',  ( 0.3108999017613326976, 1.482597719745565090, -0.3467144894627433027 ) ) ;
#6754 = CARTESIAN_POINT ( 'NONE',  ( -0.8890799276390084493, -0.1744314460652860166, 1.988413549619085785 ) ) ;
#6753 = CARTESIAN_POINT ( 'NONE',  ( -0.1797182628040039087, -1.809591053677533479, 0.07444174185955065859 ) ) ;
#6755 = LINE ( 'NONE', #14206, #22297 ) ;
#6756 = CARTESIAN_POINT ( 'NONE',  ( 0.6971942568897648851, 0.07405724077823318263, 1.619094488135213838 ) ) ;
#6758 = CARTESIAN_POINT ( 'NONE',  ( 0.1619802298550984954, 0.1595109072953912188, 2.917077808306172296E-06 ) ) ;
#6757 = DIRECTION ( 'NONE',  ( 1.000000000000000000, 0.000000000000000000, 0.000000000000000000 ) ) ;
#6759 = CARTESIAN_POINT ( 'NONE',  ( 1.054774247047244096, 0.000000000000000000, 0.5339566928596221063 ) ) ;
#6760 = EDGE_CURVE ( 'NONE', #26132, #32405, #45568, .T. ) ;
#6761 = VERTEX_POINT ( 'NONE', #14062 ) ;
#6763 = ORIENTED_EDGE ( 'NONE', *, *, #162, .F. ) ;
#6762 = CARTESIAN_POINT ( 'NONE',  ( -0.1910692666444312182, -0.07766248740295460251, -0.1751191768260007275 ) ) ;
#6764 = ADVANCED_FACE ( 'NONE', ( #35643 ), #32046, .T. ) ;
#6765 = DIRECTION ( 'NONE',  ( 0.000000000000000000, -0.9945218953682737340, -0.1045284632676499736 ) ) ;
#6767 = CARTESIAN_POINT ( 'NONE',  ( -0.07405724077823318263, -0.1309055117572600901, -0.1787899950787401604 ) ) ;
#6766 = CARTESIAN_POINT ( 'NONE',  ( -0.06523048226347956391, -0.9158464565853854378, 0.1574803149606297803 ) ) ;
#6768 = CARTESIAN_POINT ( 'NONE',  ( 0.8019270111902717657, 0.1787899950787401604, 0.6249999999462366729 ) ) ;
#6769 = CARTESIAN_POINT ( 'NONE',  ( -1.094772975963752103E-17, -1.152066929080094448, -0.1787899950787401882 ) ) ;
#6770 = CARTESIAN_POINT ( 'NONE',  ( 0.6971942568897626646, 0.07405724077823318263, 0.04429133852891373180 ) ) ;
#6771 = DIRECTION ( 'NONE',  ( 5.724375810226260600E-16, 0.6156614753256579586, 0.7880107536067221252 ) ) ;
#6772 = CARTESIAN_POINT ( 'NONE',  ( 0.8019270111902716547, 0.1787899950787401604, 0.5856299212060785964 ) ) ;
#6773 = CARTESIAN_POINT ( 'NONE',  ( -0.7495606340400177148, -0.1264236179284866091, 1.582185039316315045 ) ) ;
#6774 = ORIENTED_EDGE ( 'NONE', *, *, #30947, .F. ) ;
#6775 = CARTESIAN_POINT ( 'NONE',  ( 1.033464566929134687, -0.06523048226347956391, 0.1648622047244094890 ) ) ;
#6776 = CARTESIAN_POINT ( 'NONE',  ( 0.6971942568897648851, 0.07405724077823318263, 1.107283464513165949 ) ) ;
#6777 = CARTESIAN_POINT ( 'NONE',  ( 0.6971942568897637749, 2.189545951927499583E-17, 1.774114173174582643 ) ) ;
#6778 = CARTESIAN_POINT ( 'NONE',  ( -1.033464566929134687, 0.06523048226347956391, 0.5634842519685042683 ) ) ;
#6779 = CARTESIAN_POINT ( 'NONE',  ( -0.8759842519685039353, -0.1787899950787401882, 0.8390748030958424808 ) ) ;
#6780 = CARTESIAN_POINT ( 'NONE',  ( 1.033464566929133799, 1.928577636452524610E-17, 4.498031496062992574 ) ) ;
#6781 = CARTESIAN_POINT ( 'NONE',  ( 0.8019270111902716547, -0.1787899950787401604, 0.2903543306548980185 ) ) ;
#6782 = CARTESIAN_POINT ( 'NONE',  ( -0.7495606340400177148, -0.1264236179284866091, 0.2829724408911185041 ) ) ;
#6783 = CARTESIAN_POINT ( 'NONE',  ( -1.054774247047244540, 0.07405724077823318263, 0.6545275590013545086 ) ) ;
#6784 = CARTESIAN_POINT ( 'NONE',  ( 0.7646288533564489232, -0.1113553986120547346, 1.520669291231054876 ) ) ;
#6785 = VERTEX_POINT ( 'NONE', #46637 ) ;
#6786 = CARTESIAN_POINT ( 'NONE',  ( 0.07405724077823318263, -0.03248031490686641154, 0.1787899950787401604 ) ) ;
#6787 = ORIENTED_EDGE ( 'NONE', *, *, #18184, .T. ) ;
#6788 = CARTESIAN_POINT ( 'NONE',  ( 0.9500414927467378812, -0.1787899950787401604, 0.8464566928596233275 ) ) ;
#6789 = CARTESIAN_POINT ( 'NONE',  ( -0.7495606340400177148, -0.1264236179284866091, 1.857775590497417362 ) ) ;
#6790 = ( BOUNDED_CURVE ( )  B_SPLINE_CURVE ( 2, ( #31253, #9674, #45830, #13039, #35318, #5833, #20441, #35077, #2225 ),
 .UNSPECIFIED., .F., .F. ) 
 B_SPLINE_CURVE_WITH_KNOTS ( ( 3, 2, 2, 2, 3 ),
 ( 0.4099999999999999756, 0.4124999999999999778, 0.4149999999999999800, 0.4174999999999999822, 0.4199999999999999845 ),
 .UNSPECIFIED. ) 
 CURVE ( )  GEOMETRIC_REPRESENTATION_ITEM ( )  RATIONAL_B_SPLINE_CURVE ( ( 1.000000000000000000, 0.9238795325112879597, 1.000000000000000000, 0.9238795325112869605, 1.000000000000000000, 0.9238795325112869605, 1.000000000000000000, 0.9238795325112869605, 1.000000000000000000 ) ) 
 REPRESENTATION_ITEM ( '' )  ) ;
#6791 = DIRECTION ( 'NONE',  ( 0.000000000000000000, 0.000000000000000000, -1.000000000000000000 ) ) ;
#6792 = LINE ( 'NONE', #305, #41989 ) ;
#6793 = CARTESIAN_POINT ( 'NONE',  ( -0.07405724077823318263, -1.308194834370970616, 0.1787899950787401604 ) ) ;
#6794 = ORIENTED_EDGE ( 'NONE', *, *, #27034, .F. ) ;
#6795 = CARTESIAN_POINT ( 'NONE',  ( 3.284318927891251994E-17, -0.2268700786863941110, 0.1787899950787401882 ) ) ;
#6796 = VERTEX_POINT ( 'NONE', #129 ) ;
#6797 = ORIENTED_EDGE ( 'NONE', *, *, #2837, .T. ) ;
#6798 = CARTESIAN_POINT ( 'NONE',  ( 1.002407869896990045, 0.1264236179284866091, 1.090059055064346527 ) ) ;
#6799 = CARTESIAN_POINT ( 'NONE',  ( 7.107660667885412143E-05, -0.1226968624036212790, -0.06307306040149587845 ) ) ;
#6800 = CARTESIAN_POINT ( 'NONE',  ( -0.2471911387362889789, -0.08795568039072379496, 0.05508755932689571311 ) ) ;
#6801 = CARTESIAN_POINT ( 'NONE',  ( 0.8107537697050253289, -0.1574803149606297803, 1.926673228346456490 ) ) ;
#6802 = CARTESIAN_POINT ( 'NONE',  ( 0.07405724077823318263, -1.607283464513165949, 0.1787899950787401604 ) ) ;
#6803 = AXIS2_PLACEMENT_3D ( 'NONE', #4134, #63, #3906 ) ;
#6804 = EDGE_CURVE ( 'NONE', #4911, #18221, #47369, .T. ) ;
#6805 = CARTESIAN_POINT ( 'NONE',  ( -0.6971942568897648851, 0.07405724077823318263, 0.5167322834108035723 ) ) ;
#6806 = CARTESIAN_POINT ( 'NONE',  ( -0.7104269446534671184, 0.008049294727412099545, 1.983122017755077904 ) ) ;
#6807 = CARTESIAN_POINT ( 'NONE',  ( 0.4453382816733590377, 1.205361022782824954E-17, -0.09842519685039370636 ) ) ;
#6808 = CIRCLE ( 'NONE', #674, 0.1377952755905511861 ) ;
#6809 = CARTESIAN_POINT ( 'NONE',  ( 1.054774247047244540, 0.07405724077823318263, 1.560039370024976835 ) ) ;
#6810 = CARTESIAN_POINT ( 'NONE',  ( -0.7646288533564489232, 0.1113553986120547346, 0.6053149605223937524 ) ) ;
#6811 = EDGE_CURVE ( 'NONE', #23847, #19846, #45860, .T. ) ;
#6812 = CARTESIAN_POINT ( 'NONE',  ( 0.03906282586613502722, 0.1299212598425196485, 0.1731955441111237004 ) ) ;
#6813 = DIRECTION ( 'NONE',  ( 1.822029033848725028E-16, 0.000000000000000000, 1.000000000000000000 ) ) ;
#6814 = LINE ( 'NONE', #35139, #47359 ) ;
#6815 = CARTESIAN_POINT ( 'NONE',  ( -0.9873396505805591694, -0.1113553986120547346, 1.806102362097196767 ) ) ;
#6816 = CARTESIAN_POINT ( 'NONE',  ( 0.9500414927467378812, -0.1787899950787401604, 0.2116141731745827814 ) ) ;
#6817 = CARTESIAN_POINT ( 'NONE',  ( 0.7023594456989278312, -0.01011419101508406575, 0.03936580841072691989 ) ) ;
#6819 = CARTESIAN_POINT ( 'NONE',  ( -1.033464566929134687, 0.06523048226347956391, 1.941437007874014187 ) ) ;
#6818 = CARTESIAN_POINT ( 'NONE',  ( 0.9500414927467377701, -0.1787899950787401604, 1.077755905458048113 ) ) ;
#6820 = CARTESIAN_POINT ( 'NONE',  ( -1.033464566929133799, 0.000000000000000000, 1.929133858160188897 ) ) ;
#6821 = CARTESIAN_POINT ( 'NONE',  ( -0.6971942568897648851, -0.07405724077823297447, 1.146653543253323582 ) ) ;
#6822 = CARTESIAN_POINT ( 'NONE',  ( 0.7185039370078746268, 0.06523048226347956391, 0.4896653542231815259 ) ) ;
#6823 = ORIENTED_EDGE ( 'NONE', *, *, #40550, .T. ) ;
#6824 = DIRECTION ( 'NONE',  ( 0.000000000000000000, 0.6156614753256605121, 0.7880107536067204599 ) ) ;
#6825 = CARTESIAN_POINT ( 'NONE',  ( -1.033464566929134687, -0.06523048226347956391, 0.4699803148531029318 ) ) ;
#6826 = CARTESIAN_POINT ( 'NONE',  ( -0.9873396505805591694, -0.1113553986120547346, 1.540354330708661568 ) ) ;
#6827 = CARTESIAN_POINT ( 'NONE',  ( 0.7495606340400177148, -0.1264236179284866091, 1.464074803095842370 ) ) ;
#6829 = CARTESIAN_POINT ( 'NONE',  ( -0.9873396505805591694, -0.1113553986120547346, 0.2312992124908980207 ) ) ;
#6828 = CARTESIAN_POINT ( 'NONE',  ( 0.6195511811023624027, 0.9842519685039370358, -0.7135826771653542844 ) ) ;
#6830 = CARTESIAN_POINT ( 'NONE',  ( 0.07405724077823318263, 0.02657480320336980464, -0.1787899950787401604 ) ) ;
#6831 = VERTEX_POINT ( 'NONE', #17409 ) ;
#6832 = DIRECTION ( 'NONE',  ( -3.364312195833787750E-15, -1.000000000000000000, 0.000000000000000000 ) ) ;
#6833 = VECTOR ( 'NONE', #41165, 39.37007874015748854 ) ;
#6834 = CARTESIAN_POINT ( 'NONE',  ( 0.1924606493446845146, 0.07681961335490640475, 0.1743158631585779439 ) ) ;
#6835 = CARTESIAN_POINT ( 'NONE',  ( 0.1184675242425066999, -0.09842519685039370636, 1.870565676741756000 ) ) ;
#6836 = ORIENTED_EDGE ( 'NONE', *, *, #34771, .T. ) ;
#6837 = CARTESIAN_POINT ( 'NONE',  ( 0.8759842519685039353, -0.1787899950787401882, 0.5684055117572598403 ) ) ;
#6838 = ORIENTED_EDGE ( 'NONE', *, *, #38581, .T. ) ;
#6839 = CARTESIAN_POINT ( 'NONE',  ( -0.06523048226347956391, 0.09301181113114917465, -0.1574803149606300301 ) ) ;
#6840 = CARTESIAN_POINT ( 'NONE',  ( -1.002407869896990045, -0.1264236179284866091, 1.124507873961984261 ) ) ;
#6841 = CARTESIAN_POINT ( 'NONE',  ( -0.8759842519685039353, -0.1574803149606299191, 0.1968503937007874127 ) ) ;
#6842 = CARTESIAN_POINT ( 'NONE',  ( -1.002407869896990045, -0.1264236179284866091, 1.158956692859621995 ) ) ;
#6843 = AXIS2_PLACEMENT_3D ( 'NONE', #20930, #35572, #46096 ) ;
#6844 = CARTESIAN_POINT ( 'NONE',  ( -1.054774247047244540, -0.07405724077823318263, 0.8120078739619844832 ) ) ;
#6845 = ADVANCED_FACE ( 'NONE', ( #6384 ), #36110, .T. ) ;
#6846 = CARTESIAN_POINT ( 'NONE',  ( -0.6971942568897637749, 2.189545951927499583E-17, 0.2436023621509610382 ) ) ;
#6847 = DIRECTION ( 'NONE',  ( -0.000000000000000000, -0.6156614753256605121, -0.7880107536067204599 ) ) ;
#6848 = DIRECTION ( 'NONE',  ( 0.000000000000000000, -1.000000000000000000, 0.000000000000000000 ) ) ;
#6849 = CARTESIAN_POINT ( 'NONE',  ( 0.1787899950787401604, -0.8652814485442000825, 0.07405724077823318263 ) ) ;
#6850 = ORIENTED_EDGE ( 'NONE', *, *, #11781, .T. ) ;
#6851 = CARTESIAN_POINT ( 'NONE',  ( 0.07971570266418918915, -0.08956247127877224601, 0.1225084993081602541 ) ) ;
#6852 = AXIS2_PLACEMENT_3D ( 'NONE', #10460, #31568, #14289 ) ;
#6853 = CARTESIAN_POINT ( 'NONE',  ( -0.07405724077823318263, 0.1250000000537635492, 0.1787899950787401604 ) ) ;
#6854 = VERTEX_POINT ( 'NONE', #17889 ) ;
#6855 = CARTESIAN_POINT ( 'NONE',  ( -0.9412147342319837628, -0.1574803149606297803, 0.3469488187901108023 ) ) ;
#6856 = CARTESIAN_POINT ( 'NONE',  ( -0.6971942568897626646, -0.07405724077823297447, 0.5954724408911187261 ) ) ;
#6857 = LINE ( 'NONE', #14782, #2387 ) ;
#6858 = ORIENTED_EDGE ( 'NONE', *, *, #12795, .F. ) ;
#6859 = CARTESIAN_POINT ( 'NONE',  ( -1.002407869896990045, -0.1264236179284866091, 1.754429133804503715 ) ) ;
#6860 = VERTEX_POINT ( 'NONE', #32534 ) ;
#6861 = CARTESIAN_POINT ( 'NONE',  ( -0.07874015748031495954, -0.5708661417322833387, 0.9783464566929284123 ) ) ;
#6862 = EDGE_CURVE ( 'NONE', #5618, #47458, #45474, .T. ) ;
#6863 = AXIS2_PLACEMENT_3D ( 'NONE', #39705, #10031, #36397 ) ;
#6864 = CARTESIAN_POINT ( 'NONE',  ( -0.6971942568897626646, 0.07405724077823318263, 0.1230314960092287191 ) ) ;
#6865 = CARTESIAN_POINT ( 'NONE',  ( 0.9412147342319837628, -0.1574803149606297803, 0.6323818897637792924 ) ) ;
#6866 = CARTESIAN_POINT ( 'NONE',  ( 0.1797182628040039087, -0.8105753056460376360, 0.07444174185955046430 ) ) ;
#6867 = CARTESIAN_POINT ( 'NONE',  ( 0.9412147342319837628, 0.1574803149606300301, 0.6373031494987716483 ) ) ;
#6868 = CARTESIAN_POINT ( 'NONE',  ( -1.033464566929134687, 0.06523048226347956391, 1.341043306979086136 ) ) ;
#6869 = CARTESIAN_POINT ( 'NONE',  ( 0.8759842519685039353, 0.1787899950787401882, 0.7849409448281259305 ) ) ;
#6870 = CARTESIAN_POINT ( 'NONE',  ( 2.892866454678787531E-17, -0.6476377952755905110, 0.1574803149606299191 ) ) ;
#6871 = CARTESIAN_POINT ( 'NONE',  ( -0.1272003972225189405, 0.1291484615524529089, 0.1088019360944664504 ) ) ;
#6872 = CARTESIAN_POINT ( 'NONE',  ( 0.5236220472440944462, -0.08090551181102362266, 1.098083891755157578E-17 ) ) ;
#6873 = EDGE_CURVE ( 'NONE', #38091, #29608, #21238, .T. ) ;
#6874 = CARTESIAN_POINT ( 'NONE',  ( 0.7646288533564489232, -0.1113553986120547346, 1.333661417322834719 ) ) ;
#6876 = DIRECTION ( 'NONE',  ( 0.000000000000000000, -0.7880107536067239016, 0.6156614753256557382 ) ) ;
#6875 = CARTESIAN_POINT ( 'NONE',  ( 0.7862461320375258023, -0.1462158868424255076, 1.986452941589757826 ) ) ;
#6877 = LINE ( 'NONE', #2339, #41152 ) ;
#6879 = CARTESIAN_POINT ( 'NONE',  ( 0.1574803149606299191, 1.086379535891623949, -0.03715491745706125948 ) ) ;
#6878 = CARTESIAN_POINT ( 'NONE',  ( 1.054774247047244540, 0.07405724077823318263, 0.6938976377415124741 ) ) ;
#6880 = CARTESIAN_POINT ( 'NONE',  ( -0.9873396505805591694, 0.1113553986120547346, 0.6840551181102363376 ) ) ;
#6881 = DIRECTION ( 'NONE',  ( 0.000000000000000000, 0.000000000000000000, -1.000000000000000000 ) ) ;
#6882 = EDGE_LOOP ( 'NONE', ( #7362, #23755 ) ) ;
#6883 = DIRECTION ( 'NONE',  ( 0.000000000000000000, 1.000000000000000000, 0.000000000000000000 ) ) ;
#6884 = CARTESIAN_POINT ( 'NONE',  ( 0.9873396505805591694, -0.1113553986120547346, 1.737204724409448842 ) ) ;
#6885 = CARTESIAN_POINT ( 'NONE',  ( 0.8759842519685039353, -0.1574803149606299191, 0.7086614173228346081 ) ) ;
#6886 = CARTESIAN_POINT ( 'NONE',  ( 0.8019270111902717657, -0.1787899950787401604, 0.9153543306548987957 ) ) ;
#6887 = EDGE_LOOP ( 'NONE', ( #17059, #29288, #13911, #36469 ) ) ;
#6888 = CARTESIAN_POINT ( 'NONE',  ( -0.7185039370078739607, 0.000000000000000000, -2.869337061179095023E-17 ) ) ;
#6889 = CARTESIAN_POINT ( 'NONE',  ( -0.1270800023317771588, 0.08263335577128524956, 0.1270800023317771588 ) ) ;
#6890 = CARTESIAN_POINT ( 'NONE',  ( 0.1264236179284866091, -1.280019684985606254, -0.1264236179284866091 ) ) ;
#6891 = CARTESIAN_POINT ( 'NONE',  ( -0.06523048226347956391, -1.570374015748031704, -0.1574803149606300301 ) ) ;
#6892 = DIRECTION ( 'NONE',  ( -0.000000000000000000, 1.000000000000000000, -0.000000000000000000 ) ) ;
#6893 = CARTESIAN_POINT ( 'NONE',  ( -0.8019270111902717657, 0.1787899950787401604, 0.1525590550643468046 ) ) ;
#6894 = ORIENTED_EDGE ( 'NONE', *, *, #35349, .F. ) ;
#6895 = DIRECTION ( 'NONE',  ( -1.000000000000000000, 0.000000000000000000, 0.000000000000000000 ) ) ;
#6896 = VERTEX_POINT ( 'NONE', #3743 ) ;
#6897 = CARTESIAN_POINT ( 'NONE',  ( -0.06523048226347956391, -1.403051180994835390, -0.1574803149606300301 ) ) ;
#6898 = CARTESIAN_POINT ( 'NONE',  ( -0.7185039370078739607, 1.928577636452523993E-17, 1.476377952648377789 ) ) ;
#6899 = CARTESIAN_POINT ( 'NONE',  ( -0.6971942568897648851, -0.07405724077823297447, 1.658464566875369472 ) ) ;
#6900 = CARTESIAN_POINT ( 'NONE',  ( -0.8019270111902717657, 0.1787899950787401604, 1.097440944828127041 ) ) ;
#6901 = VECTOR ( 'NONE', #36881, 39.37007874015748143 ) ;
#6902 = CARTESIAN_POINT ( 'NONE',  ( -0.1607584476970242982, 0.09202339627320738069, -0.1926191378137585286 ) ) ;
#6903 = CARTESIAN_POINT ( 'NONE',  ( -0.7495606340400177148, -0.1264236179284866091, 1.902066929080094448 ) ) ;
#6904 = CARTESIAN_POINT ( 'NONE',  ( -0.9412147342319837628, 0.1574803149606300301, 1.473917322834645605 ) ) ;
#6905 = CARTESIAN_POINT ( 'NONE',  ( -0.8107537697050253289, 0.1574803149606300301, 1.951279527559056870 ) ) ;
#6906 = CARTESIAN_POINT ( 'NONE',  ( -0.9873396505805591694, -0.1113553986120547346, 1.894685039370078927 ) ) ;
#6907 = CARTESIAN_POINT ( 'NONE',  ( 0.1787899950787401604, -0.4666594013001046926, -0.07405724077823318263 ) ) ;
#6908 = CARTESIAN_POINT ( 'NONE',  ( -0.1537350773408287519, -0.09842519685039370636, 0.06905093064059350527 ) ) ;
#6909 = DIRECTION ( 'NONE',  ( 0.000000000000000000, -0.6156614753256639538, -0.7880107536067174623 ) ) ;
#6910 = DIRECTION ( 'NONE',  ( 1.000000000000000000, -3.469446951953625233E-15, -0.000000000000000000 ) ) ;
#6911 = AXIS2_PLACEMENT_3D ( 'NONE', #23945, #1878, #2575 ) ;
#6912 = VECTOR ( 'NONE', #30881, 39.37007874015748143 ) ;
#6913 = CARTESIAN_POINT ( 'NONE',  ( -0.8019270111902717657, -0.1787899950787401604, 0.08858267711159097113 ) ) ;
#6914 = ORIENTED_EDGE ( 'NONE', *, *, #37069, .T. ) ;
#6915 = ADVANCED_FACE ( 'NONE', ( #18365 ), #2724, .T. ) ;
#6916 = CARTESIAN_POINT ( 'NONE',  ( -1.054774247047244540, -0.07405724077823318263, 1.441929133804504604 ) ) ;
#6917 = ORIENTED_EDGE ( 'NONE', *, *, #32102, .T. ) ;
#6918 = CARTESIAN_POINT ( 'NONE',  ( 0.07405724077823318263, -1.174212598371433769, 0.1787899950787401604 ) ) ;
#6919 = CARTESIAN_POINT ( 'NONE',  ( -0.1787899950787401604, -1.341535433017102541, -0.07405724077823318263 ) ) ;
#6920 = ADVANCED_FACE ( 'NONE', ( #40151 ), #10724, .F. ) ;
#6921 = CARTESIAN_POINT ( 'NONE',  ( 0.000000000000000000, 0.1102362204724409434, 0.2007874015748031815 ) ) ;
#6922 = CARTESIAN_POINT ( 'NONE',  ( 0.7646288533564489232, 0.1113553986120547346, 0.3789370078740157410 ) ) ;
#6923 = CARTESIAN_POINT ( 'NONE',  ( -0.1797182628040039087, -0.5891186127326517585, 0.07444174185955065859 ) ) ;
#6924 = CARTESIAN_POINT ( 'NONE',  ( 1.530041696156790562E-15, 0.4667239666988196034, -0.7023826619074857724 ) ) ;
#6925 = CARTESIAN_POINT ( 'NONE',  ( -0.7185039370078746268, 0.06523048226347956391, 0.9227362203649142058 ) ) ;
#6926 = CARTESIAN_POINT ( 'NONE',  ( -0.9412147342319837628, -0.1574803149606297803, 0.9473425196850395746 ) ) ;
#6927 = CARTESIAN_POINT ( 'NONE',  ( 0.7495606340400177148, 0.1264236179284866091, 0.4749015747493858242 ) ) ;
#6928 = CARTESIAN_POINT ( 'NONE',  ( 0.1113553986120547346, -0.1998031496062991907, -0.1113553986120547346 ) ) ;
#6929 = CARTESIAN_POINT ( 'NONE',  ( 1.033464566929134687, -0.06523048226347956391, 1.769192913278299306 ) ) ;
#6930 = CARTESIAN_POINT ( 'NONE',  ( 0.1574803149606299191, 0.3883517482604913473, -0.6419475548153091848 ) ) ;
#6931 = EDGE_CURVE ( 'NONE', #2, #41717, #4246, .T. ) ;
#6932 = CARTESIAN_POINT ( 'NONE',  ( 0.9873396505805591694, -0.1113553986120547346, 0.8710629921259842590 ) ) ;
#6933 = CARTESIAN_POINT ( 'NONE',  ( 0.1702179831425535972, -0.1972188338741404368, -0.03726912461316504721 ) ) ;
#6934 = CARTESIAN_POINT ( 'NONE',  ( 0.7185039370078739607, 1.928577636452523993E-17, 1.476377952648377789 ) ) ;
#6935 = CIRCLE ( 'NONE', #40614, 0.4724409448818900348 ) ;
#6936 = EDGE_CURVE ( 'NONE', #13381, #27058, #4198, .T. ) ;
#6938 = CARTESIAN_POINT ( 'NONE',  ( 0.1583858528204715732, -0.1020630898162695754, -0.1041062675987072944 ) ) ;
#6937 = DIRECTION ( 'NONE',  ( -1.000000000000000000, 0.000000000000000000, 0.000000000000000000 ) ) ;
#6939 = CARTESIAN_POINT ( 'NONE',  ( 0.8107537697050253289, 0.1574803149606300301, 0.1697834644594022058 ) ) ;
#6940 = VERTEX_POINT ( 'NONE', #12132 ) ;
#6941 = CARTESIAN_POINT ( 'NONE',  ( -0.1787899950787401604, -0.07677165348954355373, 0.07405724077823318263 ) ) ;
#6942 = CARTESIAN_POINT ( 'NONE',  ( 0.2395294000716133853, 0.000000000000000000, 0.8759842519685039353 ) ) ;
#6943 = CARTESIAN_POINT ( 'NONE',  ( 0.1574803149606299191, -1.533464566821606034, -1.928577636452523993E-17 ) ) ;
#6944 = CARTESIAN_POINT ( 'NONE',  ( -0.1264236179284866091, -0.7583661416785196785, -0.1264236179284866091 ) ) ;
#6945 = CARTESIAN_POINT ( 'NONE',  ( -0.8107537697050234415, -0.1574803149606297803, 0.06643700776648873985 ) ) ;
#6946 = VECTOR ( 'NONE', #24006, 39.37007874015748143 ) ;
#6947 = CARTESIAN_POINT ( 'NONE',  ( 0.1574803149606300301, -0.9896653543307096790, -0.06523048226347956391 ) ) ;
#6948 = CARTESIAN_POINT ( 'NONE',  ( 0.9412147342319837628, -0.1574803149606297803, 0.8981299211523156023 ) ) ;
#6949 = FACE_OUTER_BOUND ( 'NONE', #21995, .T. ) ;
#6950 = CARTESIAN_POINT ( 'NONE',  ( -0.8019270111902717657, -0.1787899950787401604, 0.4035433070328508509 ) ) ;
#6951 = EDGE_LOOP ( 'NONE', ( #38270, #33709, #28283, #32704 ) ) ;
#6952 = ORIENTED_EDGE ( 'NONE', *, *, #27421, .F. ) ;
#6953 = CARTESIAN_POINT ( 'NONE',  ( -0.6971942568897637749, 2.189545951927499583E-17, 1.660925196796630088 ) ) ;
#6954 = AXIS2_PLACEMENT_3D ( 'NONE', #43531, #25355, #3759 ) ;
#6955 = CARTESIAN_POINT ( 'NONE',  ( 0.6971942568897648851, 0.07405724077823318263, 1.619094488135213838 ) ) ;
#6956 = ORIENTED_EDGE ( 'NONE', *, *, #4243, .F. ) ;
#6957 = CARTESIAN_POINT ( 'NONE',  ( -1.054774247047244540, -0.07405724077823318263, 0.7726377952218265177 ) ) ;
#6958 = CARTESIAN_POINT ( 'NONE',  ( 0.9500414927467378812, -0.1787899950787401604, 0.1771653542769452139 ) ) ;
#6959 = DIRECTION ( 'NONE',  ( -5.411399086424348811E-15, -1.000000000000000000, 0.000000000000000000 ) ) ;
#6960 = CARTESIAN_POINT ( 'NONE',  ( 0.7495606340400177148, 0.1264236179284866091, 0.7898622046706456068 ) ) ;
#6961 = CARTESIAN_POINT ( 'NONE',  ( -0.9500414927467377701, 0.1787899950787401604, 0.6594488188438737408 ) ) ;
#6962 = CARTESIAN_POINT ( 'NONE',  ( 1.033464566929133799, 1.928577636452524610E-17, 4.498031496062992574 ) ) ;
#6963 = ( BOUNDED_CURVE ( )  B_SPLINE_CURVE ( 2, ( #6339, #9956, #10195, #28417, #46831, #16909, #24801, #6581, #35827 ),
 .UNSPECIFIED., .F., .F. ) 
 B_SPLINE_CURVE_WITH_KNOTS ( ( 3, 2, 2, 2, 3 ),
 ( 0.7500000000000000000, 0.7524999999999999467, 0.7550000000000000044, 0.7574999999999999512, 0.7600000000000000089 ),
 .UNSPECIFIED. ) 
 CURVE ( )  GEOMETRIC_REPRESENTATION_ITEM ( )  RATIONAL_B_SPLINE_CURVE ( ( 1.000000000000000000, 0.9238795325112899581, 1.000000000000000000, 0.9238795325112869605, 1.000000000000000000, 0.9238795325112869605, 1.000000000000000000, 0.9238795325112869605, 1.000000000000000000 ) ) 
 REPRESENTATION_ITEM ( '' )  ) ;
#6964 = CARTESIAN_POINT ( 'NONE',  ( -0.8759842519685039353, -0.1574803149606299191, 0.8661417322834645827 ) ) ;
#6965 = CARTESIAN_POINT ( 'NONE',  ( 0.06523048226347956391, -0.1481299211523154913, -0.1574803149606300301 ) ) ;
#6966 = CARTESIAN_POINT ( 'NONE',  ( -0.8107537697050253289, 0.1574803149606300301, 1.941437007766490863 ) ) ;
#6967 = ORIENTED_EDGE ( 'NONE', *, *, #26978, .F. ) ;
#6968 = CARTESIAN_POINT ( 'NONE',  ( -0.9873396505805591694, 0.1113553986120547346, 1.510826771653543288 ) ) ;
#6969 = CARTESIAN_POINT ( 'NONE',  ( -0.7185039370078746268, 0.06523048226347956391, 0.4601377952755902889 ) ) ;
#6970 = CARTESIAN_POINT ( 'NONE',  ( 1.054774247047244540, 0.07405724077823318263, 1.446850393647023836 ) ) ;
#6971 = CARTESIAN_POINT ( 'NONE',  ( -0.1717461275140602373, -0.09851383607918347274, -0.03673640942690917233 ) ) ;
#6972 = DIRECTION ( 'NONE',  ( -1.000000000000000000, 0.000000000000000000, 0.000000000000000000 ) ) ;
#6973 = ORIENTED_EDGE ( 'NONE', *, *, #24367, .F. ) ;
#6974 = EDGE_CURVE ( 'NONE', #3940, #32303, #40946, .T. ) ;
#6975 = AXIS2_PLACEMENT_3D ( 'NONE', #32062, #13835, #28478 ) ;
#6976 = CARTESIAN_POINT ( 'NONE',  ( -0.1787899950787401604, -1.751108220197743259, -0.07405724077823318263 ) ) ;
#6977 = EDGE_LOOP ( 'NONE', ( #12832, #18302 ) ) ;
#6978 = EDGE_CURVE ( 'NONE', #37979, #8121, #26584, .T. ) ;
#6979 = EDGE_LOOP ( 'NONE', ( #9941, #42278 ) ) ;
#6980 = CIRCLE ( 'NONE', #45240, 0.1377952755905509641 ) ;
#6981 = COLOUR_RGB ( '', 0.66274510, 0.83137255, 0.94901961) ;
#6982 = CARTESIAN_POINT ( 'NONE',  ( 0.4330708661417322913, 0.1574803149606299191, -0.9891732283464566011 ) ) ;
#6983 = CARTESIAN_POINT ( 'NONE',  ( -1.094772975963752103E-17, -0.8764763778989921317, -0.1787899950787401882 ) ) ;
#6984 = CARTESIAN_POINT ( 'NONE',  ( -0.2471921406146342093, -0.06698952652845348299, -0.09859233283838723938 ) ) ;
#6985 = CARTESIAN_POINT ( 'NONE',  ( -0.9873396505805591694, -0.1113553986120547346, 0.9793307085538898171 ) ) ;
#6986 = CARTESIAN_POINT ( 'NONE',  ( 0.6971942568897626646, -0.07405724077823297447, 0.3592519684501735977 ) ) ;
#6987 = CARTESIAN_POINT ( 'NONE',  ( 0.1797182628040039087, -0.2151028647011559158, -0.07444174185955065859 ) ) ;
#6988 = CARTESIAN_POINT ( 'NONE',  ( 0.1264236179284866091, -0.1886082201977429262, -0.1264236179284866091 ) ) ;
#6989 = CARTESIAN_POINT ( 'NONE',  ( 0.07405724077823318263, -0.07185039364702387743, 0.1787899950787401604 ) ) ;
#6990 = DIRECTION ( 'NONE',  ( 0.000000000000000000, -0.2126700594527834443, 0.9771240687918547607 ) ) ;
#6991 = CARTESIAN_POINT ( 'NONE',  ( 0.8759842519685039353, -0.1787899950787401882, 0.6815944881352126172 ) ) ;
#6992 = CARTESIAN_POINT ( 'NONE',  ( -0.6971942568897648851, -0.07405724077823297447, 0.9547244093950545407 ) ) ;
#6993 = CARTESIAN_POINT ( 'NONE',  ( 0.1574803149606299191, -0.5708661417322835607, -6.991093932140394160E-17 ) ) ;
#6994 = CARTESIAN_POINT ( 'NONE',  ( 0.1270800023317771588, -1.708705226905880004, -0.1270800023317771588 ) ) ;
#6995 = DIRECTION ( 'NONE',  ( -1.000000000000000000, 0.000000000000000000, 0.000000000000000000 ) ) ;
#6996 = CARTESIAN_POINT ( 'NONE',  ( 1.054774247047244096, 0.000000000000000000, 1.680610236166708793 ) ) ;
#6998 = CARTESIAN_POINT ( 'NONE',  ( 0.1637019648151215312, 0.1609904454352970582, 5.735411161861398686E-09 ) ) ;
#6997 = CARTESIAN_POINT ( 'NONE',  ( 1.229559056033039366E-16, -0.0009842519685041700977, 0.4921259842519680183 ) ) ;
#6999 = ORIENTED_EDGE ( 'NONE', *, *, #3018, .T. ) ;
#7000 = ORIENTED_EDGE ( 'NONE', *, *, #16935, .T. ) ;
#7001 = DIRECTION ( 'NONE',  ( 1.000000000000000000, -0.000000000000000000, -0.000000000000000000 ) ) ;
#7003 = CARTESIAN_POINT ( 'NONE',  ( -0.07405724077823318263, -0.1702755904974175283, -0.1787899950787401604 ) ) ;
#7002 = CARTESIAN_POINT ( 'NONE',  ( -9.642888182262618425E-18, -0.8937007872940473385, -0.1574803149606299191 ) ) ;
#7004 = CARTESIAN_POINT ( 'NONE',  ( -0.6971942568897637749, 2.189545951927499583E-17, 0.4404527558517480901 ) ) ;
#7005 = CARTESIAN_POINT ( 'NONE',  ( 1.054774247047244540, -0.07405724077823318263, 0.6102362204186774219 ) ) ;
#7006 = CARTESIAN_POINT ( 'NONE',  ( 0.07405724077823318263, -1.075787401521038689, -0.1787899950787401604 ) ) ;
#7007 = CARTESIAN_POINT ( 'NONE',  ( 0.6971942568897637749, 2.189545951927499583E-17, 0.04675196845017354913 ) ) ;
#7008 = CARTESIAN_POINT ( 'NONE',  ( -1.033464566929133799, 0.000000000000000000, 1.535433070758614127 ) ) ;
#7009 = AXIS2_PLACEMENT_3D ( 'NONE', #23522, #11797, #19432 ) ;
#7010 = CARTESIAN_POINT ( 'NONE',  ( -0.8019270111902717657, 0.1787899950787401604, 1.648622047190331230 ) ) ;
#7011 = VERTEX_POINT ( 'NONE', #22667 ) ;
#7012 = CARTESIAN_POINT ( 'NONE',  ( -0.8019270111902717657, -0.1787899950787401604, 1.156496062938362046 ) ) ;
#7013 = CARTESIAN_POINT ( 'NONE',  ( -0.2896304277639956681, -0.1109299681405381544, -1.001705941724043258 ) ) ;
#7014 = CARTESIAN_POINT ( 'NONE',  ( 1.054774247047244096, 0.000000000000000000, 1.129429133804503937 ) ) ;
#7015 = CARTESIAN_POINT ( 'NONE',  ( -0.1574803149606297803, -1.117618110128692832, 0.06523048226347956391 ) ) ;
#7016 = CARTESIAN_POINT ( 'NONE',  ( -0.7185039370078746268, -0.06523048226347956391, 0.6520669290263312323 ) ) ;
#7017 = CIRCLE ( 'NONE', #10875, 0.09842519685039320676 ) ;
#7018 = AXIS2_PLACEMENT_3D ( 'NONE', #10683, #46370, #3477 ) ;
#7019 = DIRECTION ( 'NONE',  ( 0.000000000000000000, 1.000000000000000000, 0.000000000000000000 ) ) ;
#7020 = CARTESIAN_POINT ( 'NONE',  ( 0.6971942568897637749, 2.189545951927499583E-17, 1.892224409395055096 ) ) ;
#7021 = CARTESIAN_POINT ( 'NONE',  ( -0.7185039370078746268, 0.06523048226347956391, 0.5388779527559054427 ) ) ;
#7022 = CARTESIAN_POINT ( 'NONE',  ( -0.8019270111902717657, 0.1787899950787401604, 0.8612204723871809131 ) ) ;
#7023 = CARTESIAN_POINT ( 'NONE',  ( -0.1476377952755905387, -0.4812165006432426728, -0.8611016091043821596 ) ) ;
#7024 = CARTESIAN_POINT ( 'NONE',  ( 0.8019270111902716547, -0.1787899950787401604, 0.3297244093950555954 ) ) ;
#7025 = CARTESIAN_POINT ( 'NONE',  ( -0.9500414927467377701, -0.1787899950787401604, 0.2903543306548980185 ) ) ;
#7026 = CARTESIAN_POINT ( 'NONE',  ( -0.6971942568897626646, 0.07405724077823318263, 0.7480314960092282472 ) ) ;
#7027 = CARTESIAN_POINT ( 'NONE',  ( 0.7185039370078746268, -0.06523048226347956391, 1.596948818790111080 ) ) ;
#7028 = VERTEX_POINT ( 'NONE', #44447 ) ;
#7029 = CARTESIAN_POINT ( 'NONE',  ( -0.07405724077823318263, 0.04133858273092887170, 0.1787899950787401604 ) ) ;
#7030 = CARTESIAN_POINT ( 'NONE',  ( 1.002407869896990045, 0.1264236179284866091, 0.7406496062454487328 ) ) ;
#7031 = CARTESIAN_POINT ( 'NONE',  ( 0.9500414927467377701, 0.1787899950787401604, 1.018700787347811110 ) ) ;
#7032 = CARTESIAN_POINT ( 'NONE',  ( -1.054774247047244540, -0.07405724077823318263, 1.830708661363559253 ) ) ;
#7033 = ADVANCED_FACE ( 'NONE', ( #4915 ), #4426, .T. ) ;
#7034 = CARTESIAN_POINT ( 'NONE',  ( 0.6971942568897648851, -0.07405724077823297447, 1.973425196796630088 ) ) ;
#7035 = ORIENTED_EDGE ( 'NONE', *, *, #37774, .F. ) ;
#7036 = EDGE_CURVE ( 'NONE', #28784, #17791, #7994, .T. ) ;
#7037 = CARTESIAN_POINT ( 'NONE',  ( 0.8759842519685039353, 0.1574803149606299191, 1.318897637795275690 ) ) ;
#7038 = CARTESIAN_POINT ( 'NONE',  ( -1.094772975963752103E-17, -1.325419243819789594, -0.1787899950787401882 ) ) ;
#7039 = EDGE_LOOP ( 'NONE', ( #45728, #41884, #45115, #35610 ) ) ;
#7040 = CARTESIAN_POINT ( 'NONE',  ( -0.07405724077823318263, -0.3228346456155278266, -0.1787899950787401604 ) ) ;
#7041 = EDGE_CURVE ( 'NONE', #16843, #27712, #43697, .T. ) ;
#7042 = EDGE_LOOP ( 'NONE', ( #11508, #2865, #27213, #27416 ) ) ;
#7043 = CARTESIAN_POINT ( 'NONE',  ( 0.8759842519685039353, 0.1787899950787401882, 1.213090551127338435 ) ) ;
#7044 = EDGE_CURVE ( 'NONE', #6663, #21819, #18698, .T. ) ;
#7045 = DIRECTION ( 'NONE',  ( 0.000000000000000000, -1.000000000000000000, 0.000000000000000000 ) ) ;
#7046 = CARTESIAN_POINT ( 'NONE',  ( -1.181162989532618060E-16, 0.000000000000000000, -0.3937007874015748254 ) ) ;
#7047 = CARTESIAN_POINT ( 'NONE',  ( 1.002407869896990045, -0.1264236179284866091, 0.09596456687537027741 ) ) ;
#7048 = AXIS2_PLACEMENT_3D ( 'NONE', #29618, #25521, #44159 ) ;
#7049 = AXIS2_PLACEMENT_3D ( 'NONE', #2171, #44829, #41452 ) ;
#7050 = CARTESIAN_POINT ( 'NONE',  ( -0.1264236179284866091, -1.614665354276944909, 0.1264236179284866091 ) ) ;
#7051 = CARTESIAN_POINT ( 'NONE',  ( 0.1787899950787401882, -0.7731299212060788184, -2.189545951927503898E-17 ) ) ;
#7052 = CARTESIAN_POINT ( 'NONE',  ( -0.8759842519685039353, 0.1787899950787401882, 0.5093503936470236138 ) ) ;
#7053 = CARTESIAN_POINT ( 'NONE',  ( 0.07444174185955046430, -1.312543809583045284, -0.1797182628040039087 ) ) ;
#7054 = CARTESIAN_POINT ( 'NONE',  ( -0.2559055118110236116, -0.1477471161312043368, -0.3149606299212598381 ) ) ;
#7055 = CARTESIAN_POINT ( 'NONE',  ( 0.8759842519685039353, -0.1787899950787401882, 1.277066929080094448 ) ) ;
#7056 = CARTESIAN_POINT ( 'NONE',  ( 0.8759842519685039353, -0.1787899950787401882, 1.665846456639149764 ) ) ;
#7057 = CARTESIAN_POINT ( 'NONE',  ( -0.8759842519685039353, 0.1574803149606299191, 0.6003937006798740761 ) ) ;
#7058 = FACE_OUTER_BOUND ( 'NONE', #33594, .T. ) ;
#7059 = CARTESIAN_POINT ( 'NONE',  ( 0.1602931993194442739, 0.07955613945526338049, -0.1377952755905511861 ) ) ;
#7060 = CARTESIAN_POINT ( 'NONE',  ( -9.642888182262618425E-18, -0.7755905510735748853, -0.1574803149606299191 ) ) ;
#7061 = CARTESIAN_POINT ( 'NONE',  ( -1.033464566929134687, -0.06523048226347956391, 1.769192913278299306 ) ) ;
#7062 = CARTESIAN_POINT ( 'NONE',  ( 1.054774247047244096, 0.000000000000000000, 0.2189960629383626012 ) ) ;
#7064 = LINE ( 'NONE', #32735, #876 ) ;
#7063 = CARTESIAN_POINT ( 'NONE',  ( 0.6971942568897637749, 2.189545951927499583E-17, 1.183562992072220599 ) ) ;
#7065 = CARTESIAN_POINT ( 'NONE',  ( -1.054774247047244540, 0.07405724077823318263, 1.205708661363558365 ) ) ;
#7066 = CARTESIAN_POINT ( 'NONE',  ( 1.033464566929133799, 0.000000000000000000, 0.4724409447743622148 ) ) ;
#7067 = ORIENTED_EDGE ( 'NONE', *, *, #19315, .F. ) ;
#7068 = LINE ( 'NONE', #6592, #24563 ) ;
#7069 = CARTESIAN_POINT ( 'NONE',  ( 0.9674136657275992368, 0.1412476989763037649, 0.03936995337663032335 ) ) ;
#7070 = CARTESIAN_POINT ( 'NONE',  ( 0.8759842519685039353, -0.1574803149606299191, 0.2755905511811023723 ) ) ;
#7071 = CARTESIAN_POINT ( 'NONE',  ( -0.7185039370078746268, -0.06523048226347956391, 0.3764763778452286935 ) ) ;
#7072 = ORIENTED_EDGE ( 'NONE', *, *, #45431, .F. ) ;
#7073 = CARTESIAN_POINT ( 'NONE',  ( 1.054774247047244540, -0.07405724077823318263, 1.437007873961985371 ) ) ;
#7074 = CARTESIAN_POINT ( 'NONE',  ( -1.033464566929134687, 0.06523048226347956391, 1.154035433070866423 ) ) ;
#7076 = FACE_OUTER_BOUND ( 'NONE', #18821, .T. ) ;
#7075 = CARTESIAN_POINT ( 'NONE',  ( -1.033464566929134687, -0.06523048226347956391, 1.779035433070867311 ) ) ;
#7077 = DIRECTION ( 'NONE',  ( 0.000000000000000000, 0.000000000000000000, 1.000000000000000000 ) ) ;
#7078 = CARTESIAN_POINT ( 'NONE',  ( -0.1264236179284866091, -0.04478346451316559534, -0.1264236179284866091 ) ) ;
#7079 = VERTEX_POINT ( 'NONE', #43995 ) ;
#7080 = LINE ( 'NONE', #32026, #16132 ) ;
#7081 = ( BOUNDED_CURVE ( )  B_SPLINE_CURVE ( 2, ( #31833, #3033, #35659, #36124, #6161, #17425, #46650, #39685, #39226 ),
 .UNSPECIFIED., .F., .T. ) 
 B_SPLINE_CURVE_WITH_KNOTS ( ( 3, 2, 2, 2, 3 ),
 ( 0.8000000000000000444, 0.8024999999999999911, 0.8050000000000000488, 0.8074999999999999956, 0.8100000000000000533 ),
 .UNSPECIFIED. ) 
 CURVE ( )  GEOMETRIC_REPRESENTATION_ITEM ( )  RATIONAL_B_SPLINE_CURVE ( ( 1.000000000000000000, 0.9238795325112869605, 1.000000000000000000, 0.9238795325112869605, 1.000000000000000000, 0.9238795325112869605, 1.000000000000000000, 0.9238795325112829637, 1.000000000000000000 ) ) 
 REPRESENTATION_ITEM ( '' )  ) ;
#7082 = CIRCLE ( 'NONE', #4778, 0.09842519685039370636 ) ;
#7083 = EDGE_LOOP ( 'NONE', ( #26120, #43385, #40436, #24323 ) ) ;
#7084 = CARTESIAN_POINT ( 'NONE',  ( 0.4632545931758527691, -0.08090551181102362266, 1.098083891755157578E-17 ) ) ;
#7085 = DIRECTION ( 'NONE',  ( 0.000000000000000000, 0.000000000000000000, -1.000000000000000000 ) ) ;
#7086 = CARTESIAN_POINT ( 'NONE',  ( 1.054774247047244540, 0.07405724077823318263, 0.5413385826234012876 ) ) ;
#7087 = ORIENTED_EDGE ( 'NONE', *, *, #2710, .T. ) ;
#7088 = CARTESIAN_POINT ( 'NONE',  ( -1.002407869896990045, -0.1264236179284866091, 1.473917322780881722 ) ) ;
#7089 = CARTESIAN_POINT ( 'NONE',  ( -0.1787899950787401604, -1.779527559001355952, -0.07405724077823318263 ) ) ;
#7090 = CARTESIAN_POINT ( 'NONE',  ( -0.8019270111902717657, -0.1787899950787401604, 1.156496062938362046 ) ) ;
#7091 = VECTOR ( 'NONE', #34541, 39.37007874015748143 ) ;
#7092 = CARTESIAN_POINT ( 'NONE',  ( -0.7185039370078739607, 1.928577636452523993E-17, 0.1870078740157480324 ) ) ;
#7093 = EDGE_LOOP ( 'NONE', ( #26363, #18372, #16064, #13224 ) ) ;
#7094 = EDGE_CURVE ( 'NONE', #12359, #10722, #7569, .T. ) ;
#7095 = CARTESIAN_POINT ( 'NONE',  ( -1.002407869896990045, 0.1264236179284866091, 0.2288385826234019815 ) ) ;
#7096 = CARTESIAN_POINT ( 'NONE',  ( 1.033464566929133799, 0.000000000000000000, 1.653543306979086580 ) ) ;
#7097 = CARTESIAN_POINT ( 'NONE',  ( -0.07405724077823318263, -0.8505176690166401654, -0.1787899950787401604 ) ) ;
#7098 = ORIENTED_EDGE ( 'NONE', *, *, #30598, .F. ) ;
#7099 = CARTESIAN_POINT ( 'NONE',  ( 0.0001126629808640675258, -0.08956164707051811336, 0.1524538216589708950 ) ) ;
#7100 = CARTESIAN_POINT ( 'NONE',  ( -0.07405724077823318263, 0.1496062992663619862, -0.1787899950787401604 ) ) ;
#7101 = EDGE_LOOP ( 'NONE', ( #18028, #41010, #12496, #19859, #3742 ) ) ;
#7102 = CARTESIAN_POINT ( 'NONE',  ( 0.5236220472440944462, 4.616380251121755931E-17, 0.000000000000000000 ) ) ;
#7103 = EDGE_CURVE ( 'NONE', #46991, #32643, #1799, .T. ) ;
#7104 = DIRECTION ( 'NONE',  ( 0.5735764363510447161, 0.8191520442889925757, 0.000000000000000000 ) ) ;
#7105 = ( BOUNDED_CURVE ( )  B_SPLINE_CURVE ( 2, ( #33215, #19019, #26244, #794, #33919, #22384, #11625, #22147, #30109 ),
 .UNSPECIFIED., .F., .T. ) 
 B_SPLINE_CURVE_WITH_KNOTS ( ( 3, 2, 2, 2, 3 ),
 ( 0.8499999999999999778, 0.8525000000000000355, 0.8549999999999999822, 0.8575000000000000400, 0.8599999999999999867 ),
 .UNSPECIFIED. ) 
 CURVE ( )  GEOMETRIC_REPRESENTATION_ITEM ( )  RATIONAL_B_SPLINE_CURVE ( ( 1.000000000000000000, 0.9238795325112939549, 1.000000000000000000, 0.9238795325112869605, 1.000000000000000000, 0.9238795325112869605, 1.000000000000000000, 0.9238795325112869605, 1.000000000000000000 ) ) 
 REPRESENTATION_ITEM ( '' )  ) ;
#7106 = CARTESIAN_POINT ( 'NONE',  ( -1.054774247047244540, 0.07405724077823318263, 0.8120078739619844832 ) ) ;
#7107 = LINE ( 'NONE', #21964, #6213 ) ;
#7108 = ORIENTED_EDGE ( 'NONE', *, *, #1961, .T. ) ;
#7109 = CARTESIAN_POINT ( 'NONE',  ( -1.054774247047244540, 0.07405724077823318263, 1.840551181048599938 ) ) ;
#7110 = CARTESIAN_POINT ( 'NONE',  ( 0.7185039370078739607, 1.928577636452523993E-17, 1.328740157480315043 ) ) ;
#7111 = CARTESIAN_POINT ( 'NONE',  ( -0.7495606340400177148, 0.1264236179284866091, 0.04183070860765386589 ) ) ;
#7112 = VERTEX_POINT ( 'NONE', #20482 ) ;
#7113 = CARTESIAN_POINT ( 'NONE',  ( 0.8759842519685039353, -0.1574803149606299191, 0.6692913385826771977 ) ) ;
#7114 = CARTESIAN_POINT ( 'NONE',  ( -0.1797182628040039087, -0.8302603450161165632, -0.07444174185955065859 ) ) ;
#7115 = CARTESIAN_POINT ( 'NONE',  ( -0.8759842519685039353, 0.1574803149606299191, 0.4035433069790866356 ) ) ;
#7116 = CARTESIAN_POINT ( 'NONE',  ( -0.8107537697050253289, -0.1574803149606297803, 1.326279527451528661 ) ) ;
#7117 = CARTESIAN_POINT ( 'NONE',  ( 0.9500414927467378812, 0.1787899950787401604, 0.7431102361667091261 ) ) ;
#7118 = CARTESIAN_POINT ( 'NONE',  ( 2.892866454678787531E-17, -0.5688976377952755792, 0.1574803149606299191 ) ) ;
#7119 = AXIS2_PLACEMENT_3D ( 'NONE', #33307, #40671, #15085 ) ;
#7120 = AXIS2_PLACEMENT_3D ( 'NONE', #43599, #8541, #44947 ) ;
#7121 = CARTESIAN_POINT ( 'NONE',  ( -0.1613734868294114388, 0.1271050926819339011, 0.03304375603688991525 ) ) ;
#7122 = CARTESIAN_POINT ( 'NONE',  ( 0.7185039370078739607, 0.000000000000000000, 4.498031496062992574 ) ) ;
#7123 = CARTESIAN_POINT ( 'NONE',  ( 0.7646288533564489232, 0.1113553986120547346, 1.323818897637795367 ) ) ;
#7125 = DIRECTION ( 'NONE',  ( 1.000000000000000000, 0.000000000000000000, 0.000000000000000000 ) ) ;
#7124 = CARTESIAN_POINT ( 'NONE',  ( 0.7775410103530361328, -0.1400450413635906666, 1.986256998439228871 ) ) ;
#7126 = CARTESIAN_POINT ( 'NONE',  ( 1.033464566929134687, 0.06523048226347956391, 0.3174212597349925224 ) ) ;
#7127 = EDGE_CURVE ( 'NONE', #20507, #36580, #13147, .T. ) ;
#7128 = AXIS2_PLACEMENT_3D ( 'NONE', #11761, #16470, #19812 ) ;
#7130 = CARTESIAN_POINT ( 'NONE',  ( 0.4028871391076110364, -0.08090551181102362266, 0.000000000000000000 ) ) ;
#7129 = CARTESIAN_POINT ( 'NONE',  ( 0.9500414927467377701, -0.1787899950787401604, 0.7234251967966300878 ) ) ;
#7131 = DIRECTION ( 'NONE',  ( 0.000000000000000000, 3.556183125752454544E-15, 1.000000000000000000 ) ) ;
#7132 = ORIENTED_EDGE ( 'NONE', *, *, #5522, .T. ) ;
#7133 = LINE ( 'NONE', #2808, #37528 ) ;
#7134 = B_SPLINE_CURVE_WITH_KNOTS ( 'NONE', 3,
 ( #14481, #43694, #6799, #36301, #46815, #21176, #24785, #21906, #36528, #17122, #35811, #32236, #28653, #13530 ),
 .UNSPECIFIED., .F., .F.,
 ( 4, 2, 2, 2, 2, 2, 4 ),
 ( 0.000000000000000000, 0.1249999999999997502, 0.2499999999999995004, 0.3749999999999992228, 0.4374999999999993894, 0.4999999999999995559, 1.000000000000000000 ),
 .UNSPECIFIED. ) ;
#7135 = CARTESIAN_POINT ( 'NONE',  ( 0.4208034506101054895, -3.032960542342102697E-32, 0.09842519685039370636 ) ) ;
#7136 = CARTESIAN_POINT ( 'NONE',  ( 0.8759842519685039353, -0.1787899950787401882, 1.035925196796629866 ) ) ;
#7137 = DIRECTION ( 'NONE',  ( 1.000000000000000000, 0.000000000000000000, 0.000000000000000000 ) ) ;
#7138 = CARTESIAN_POINT ( 'NONE',  ( -0.07405724077823318263, -1.218503936954111300, 0.1787899950787401604 ) ) ;
#7139 = CARTESIAN_POINT ( 'NONE',  ( -0.1113553986120547346, -1.449803149606299080, -0.1113553986120547346 ) ) ;
#7140 = CARTESIAN_POINT ( 'NONE',  ( 0.4330708661417322913, 0.000000000000000000, 0.9891732283464566011 ) ) ;
#7141 = UNCERTAINTY_MEASURE_WITH_UNIT (LENGTH_MEASURE( 1.000000000000000082E-05 ), #26155, 'distance_accuracy_value', 'NONE') ;
#7142 = CARTESIAN_POINT ( 'NONE',  ( -0.8019270111902717657, -0.1787899950787401604, 0.1673228345919057225 ) ) ;
#7143 = ORIENTED_EDGE ( 'NONE', *, *, #10415, .F. ) ;
#7144 = CARTESIAN_POINT ( 'NONE',  ( 0.000000000000000000, 0.000000000000000000, -0.1436967020037460685 ) ) ;
#7145 = CARTESIAN_POINT ( 'NONE',  ( -1.002407869896990045, -0.1264236179284866091, 1.911909448765133801 ) ) ;
#7146 = CARTESIAN_POINT ( 'NONE',  ( -0.7495606340400177148, 0.1264236179284866091, 1.729822834591905556 ) ) ;
#7147 = CARTESIAN_POINT ( 'NONE',  ( -0.6971942568897648851, 0.07405724077823318263, 1.102362204670646495 ) ) ;
#7148 = CARTESIAN_POINT ( 'NONE',  ( -1.002407869896990045, 0.1264236179284866091, 0.4256889763241890057 ) ) ;
#7149 = EDGE_CURVE ( 'NONE', #4172, #9090, #16772, .T. ) ;
#7150 = CARTESIAN_POINT ( 'NONE',  ( -0.1924606493446819333, 0.07681961335490891662, -0.1743158631585794982 ) ) ;
#7151 = CARTESIAN_POINT ( 'NONE',  ( -0.7495606340400177148, -0.1264236179284866091, 1.980807086560409491 ) ) ;
#7152 = CARTESIAN_POINT ( 'NONE',  ( 0.08837038158042308245, -0.09266989036297280935, -0.2344124146308698975 ) ) ;
#7153 = CARTESIAN_POINT ( 'NONE',  ( -0.7185039370078746268, 0.06523048226347956391, 1.916830708661418248 ) ) ;
#7154 = DIRECTION ( 'NONE',  ( 0.8660254037844389297, 0.000000000000000000, -0.4999999999999994449 ) ) ;
#7155 = CARTESIAN_POINT ( 'NONE',  ( 0.1264236179284866091, -0.3559310548434121979, 0.1264236179284866091 ) ) ;
#7156 = CARTESIAN_POINT ( 'NONE',  ( 0.04596748140029709162, -0.09842519685039370636, 0.1460059822399198959 ) ) ;
#7157 = CARTESIAN_POINT ( 'NONE',  ( -1.033464566929133799, 0.000000000000000000, 0.9842519683964094934 ) ) ;
#7158 = CARTESIAN_POINT ( 'NONE',  ( 0.5555748031496118289, 1.194414586609139128, -0.06082000038405787484 ) ) ;
#7159 = VECTOR ( 'NONE', #14374, 39.37007874015748143 ) ;
#7160 = EDGE_CURVE ( 'NONE', #28305, #6831, #4154, .T. ) ;
#7161 = CARTESIAN_POINT ( 'NONE',  ( -0.6971942568897626646, -0.07405724077823297447, 0.2805118109698587214 ) ) ;
#7162 = VERTEX_POINT ( 'NONE', #2497 ) ;
#7163 = CIRCLE ( 'NONE', #20939, 0.1968503937007874405 ) ;
#7164 = CARTESIAN_POINT ( 'NONE',  ( -0.6971942568897648851, 0.07405724077823318263, 1.343503936954111966 ) ) ;
#7165 = ORIENTED_EDGE ( 'NONE', *, *, #45760, .T. ) ;
#7166 = CARTESIAN_POINT ( 'NONE',  ( -0.07405724077823318263, -1.154527559001354842, -0.1787899950787401604 ) ) ;
#7167 = CARTESIAN_POINT ( 'NONE',  ( 0.1787899950787401882, -1.398129921206078707, -2.189545951927503898E-17 ) ) ;
#7168 = LENGTH_MEASURE_WITH_UNIT ( LENGTH_MEASURE( 0.02539999999999999897 ), #44051 ) ;
#7169 = CARTESIAN_POINT ( 'NONE',  ( 0.3761369780785432937, 0.9186225489812598344, -0.8759842519689370333 ) ) ;
#7170 = CARTESIAN_POINT ( 'NONE',  ( 1.033464566929133799, 0.000000000000000000, 0.4035433070866141780 ) ) ;
#7171 = CARTESIAN_POINT ( 'NONE',  ( -0.1797182628040039087, -0.6284886914728088358, 0.07444174185955065859 ) ) ;
#7172 = LINE ( 'NONE', #47431, #44649 ) ;
#7173 = CARTESIAN_POINT ( 'NONE',  ( -1.033464566929134687, -0.06523048226347956391, 0.9030511809948348345 ) ) ;
#7174 = CARTESIAN_POINT ( 'NONE',  ( 0.1574803149606299191, -0.2047244094488188948, -1.928577636452523993E-17 ) ) ;
#7175 = CARTESIAN_POINT ( 'NONE',  ( 1.033464566929133799, 0.000000000000000000, 1.771653543199558811 ) ) ;
#7176 = ORIENTED_EDGE ( 'NONE', *, *, #38109, .F. ) ;
#7177 = AXIS2_PLACEMENT_3D ( 'NONE', #19378, #41513, #38191 ) ;
#7178 = CARTESIAN_POINT ( 'NONE',  ( -1.033464566929133799, 0.000000000000000000, 1.417322834538141674 ) ) ;
#7179 = CARTESIAN_POINT ( 'NONE',  ( 0.8759842519685039353, 0.1574803149606299191, 0.8070866141732283561 ) ) ;
#7180 = CARTESIAN_POINT ( 'NONE',  ( -1.033464566929134687, 0.06523048226347956391, 1.075295275590550048 ) ) ;
#7182 = CARTESIAN_POINT ( 'NONE',  ( 0.3604359965418638123, 4.466152701071653354E-17, 0.000000000000000000 ) ) ;
#7181 = LINE ( 'NONE', #14612, #14096 ) ;
#7183 = CARTESIAN_POINT ( 'NONE',  ( 0.7185039370078746268, 0.06523048226347956391, 0.2534448817822366751 ) ) ;
#7184 = ORIENTED_EDGE ( 'NONE', *, *, #17160, .T. ) ;
#7185 = ORIENTED_EDGE ( 'NONE', *, *, #41907, .T. ) ;
#7186 = CARTESIAN_POINT ( 'NONE',  ( 0.7185039370078692977, 0.06523048226347515077, 1.906988188868851797 ) ) ;
#7187 = CARTESIAN_POINT ( 'NONE',  ( -0.8107537697050254399, -0.1574803149606297803, 0.7750984250893222516 ) ) ;
#7188 = CARTESIAN_POINT ( 'NONE',  ( -0.1574803149606299191, -1.474409448711370141, 0.000000000000000000 ) ) ;
#7189 = CARTESIAN_POINT ( 'NONE',  ( -0.07405724077823318263, -0.6820866141194646959, -0.1787899950787401604 ) ) ;
#7190 = CARTESIAN_POINT ( 'NONE',  ( -0.8107537697050234415, -0.1574803149606297803, 0.1451771652468037688 ) ) ;
#7191 = CARTESIAN_POINT ( 'NONE',  ( -0.06523048226347956391, -1.043799212598425452, 0.1574803149606297803 ) ) ;
#7192 = CARTESIAN_POINT ( 'NONE',  ( 0.8759842519685039353, 0.1574803149606299191, 0.9547244093412913246 ) ) ;
#7193 = CYLINDRICAL_SURFACE ( 'NONE', #46643, 0.4724409448818896462 ) ;
#7194 = CARTESIAN_POINT ( 'NONE',  ( -0.9500414927467378812, -0.1787899950787401604, 0.4084645668753704717 ) ) ;
#7195 = VERTEX_POINT ( 'NONE', #2034 ) ;
#7196 = ORIENTED_EDGE ( 'NONE', *, *, #9960, .T. ) ;
#7197 = VECTOR ( 'NONE', #26346, 39.37007874015748143 ) ;
#7198 = CARTESIAN_POINT ( 'NONE',  ( -0.9500414927467378812, -0.1787899950787401604, 1.633858267662771313 ) ) ;
#7199 = ORIENTED_EDGE ( 'NONE', *, *, #31190, .T. ) ;
#7200 = EDGE_CURVE ( 'NONE', #26963, #40024, #24874, .T. ) ;
#7201 = CARTESIAN_POINT ( 'NONE',  ( 0.6971942568897648851, -0.07405724077823297447, 1.505905511757261284 ) ) ;
#7202 = CARTESIAN_POINT ( 'NONE',  ( -0.9500414927467378812, -0.1787899950787401604, 0.7677165353793073965 ) ) ;
#7203 = CARTESIAN_POINT ( 'NONE',  ( 0.9500414927467378812, -0.1787899950787401604, 0.1377952755367876370 ) ) ;
#7204 = LINE ( 'NONE', #36453, #18217 ) ;
#7205 = CARTESIAN_POINT ( 'NONE',  ( 1.054774247047244540, 0.07405724077823318263, 0.7381889763241898939 ) ) ;
#7206 = CARTESIAN_POINT ( 'NONE',  ( -0.6971942568897637749, 2.189545951927499583E-17, 0.6323818897100157432 ) ) ;
#7207 = CARTESIAN_POINT ( 'NONE',  ( 0.003062405574123280416, -0.1000190445539560907, 0.1023525292014032806 ) ) ;
#7208 = ADVANCED_FACE ( 'NONE', ( #19775 ), #5633, .T. ) ;
#7209 = CARTESIAN_POINT ( 'NONE',  ( 0.7646288533564489232, 0.1113553986120547346, 1.077755905404283565 ) ) ;
#7210 = CARTESIAN_POINT ( 'NONE',  ( 0.1574803149606300301, -0.1579724408373548161, 0.06523048226347956391 ) ) ;
#7211 = CARTESIAN_POINT ( 'NONE',  ( -0.8107537697050253289, -0.1574803149606297803, 1.838090551073574774 ) ) ;
#7212 = ORIENTED_EDGE ( 'NONE', *, *, #34931, .T. ) ;
#7213 = CARTESIAN_POINT ( 'NONE',  ( -0.8107537697050253289, 0.1574803149606300301, 1.518208661417322469 ) ) ;
#7214 = CARTESIAN_POINT ( 'NONE',  ( 0.9500414927467377701, 0.1787899950787401604, 1.451771653489543290 ) ) ;
#7215 = CARTESIAN_POINT ( 'NONE',  ( -0.1561580984082978352, -0.09851383248064074505, 0.06438758770809645260 ) ) ;
#7216 = DIRECTION ( 'NONE',  ( -1.000000000000000000, 0.000000000000000000, 0.000000000000000000 ) ) ;
#7217 = ORIENTED_EDGE ( 'NONE', *, *, #25255, .T. ) ;
#7218 = EDGE_CURVE ( 'NONE', #12474, #9619, #20245, .T. ) ;
#7219 = EDGE_CURVE ( 'NONE', #38209, #42434, #505, .T. ) ;
#7220 = CARTESIAN_POINT ( 'NONE',  ( -0.1787899950787401604, -1.706816881615065951, 0.07405724077823318263 ) ) ;
#7221 = ORIENTED_EDGE ( 'NONE', *, *, #39267, .T. ) ;
#7222 = ORIENTED_EDGE ( 'NONE', *, *, #19756, .T. ) ;
#7223 = AXIS2_PLACEMENT_3D ( 'NONE', #38987, #28723, #42791 ) ;
#7224 = DIRECTION ( 'NONE',  ( -1.000000000000000000, 0.000000000000000000, 0.000000000000000000 ) ) ;
#7225 = CARTESIAN_POINT ( 'NONE',  ( 0.1787899950787401604, -0.9625984251430860228, -0.07405724077823318263 ) ) ;
#7226 = CARTESIAN_POINT ( 'NONE',  ( -0.2471922904502822094, -0.05170400041268939650, -0.1201839652816935194 ) ) ;
#7227 = ( CONVERSION_BASED_UNIT ( 'INCH', #36473 ) LENGTH_UNIT ( ) NAMED_UNIT ( #30168 ) ) ;
#7228 = LENGTH_MEASURE_WITH_UNIT ( LENGTH_MEASURE( 0.02539999999999999897 ), #7455 ) ;
#7229 = CARTESIAN_POINT ( 'NONE',  ( 0.8019270111902717657, -0.1787899950787401604, 1.742125984198204858 ) ) ;
#7230 = CARTESIAN_POINT ( 'NONE',  ( 0.9500414927467378812, 0.1787899950787401604, 0.2657480314422993595 ) ) ;
#7231 = CLOSED_SHELL ( 'NONE', ( #20807, #19087, #21475, #23283, #22901, #15739, #30708, #7033, #1627, #36746, #32999, #46243, #15559, #2052, #198, #22344, #23924, #4144, #17053, #26424, #38257, #42954, #18980, #28361, #15440, #18872, #46569, #5580, #21357, #19196, #30770, #43829, #17319, #44235, #8496, #12851, #31021, #38151, #27849, #35304, #21713, #39209, #42611, #41139, #38705, #2536, #25690, #15325, #17523, #29043, #13340, #46897, #28104, #14678, #45689, #43870, #516, #28098, #37572, #29327, #31727, #14838, #47446, #32153, #41682, #6845, #6731, #8390, #22074, #14298, #4570, #27484, #46237, #18610, #46397, #27755, #22673, #15026, #27156, #30880, #40309, #19314, #31529, #6092, #38207, #10321, #9269, #45035, #22839, #43647, #35670, #14010, #12123, #40828, #11652, #39000, #16728, #25163, #1796, #33848, #21829, #41582, #12578, #18766, #3147, #6431, #8051, #10286, #20021, #25874, #43931, #28985, #12696, #26086, #31571, #42593, #25223, #9374, #29861, #33387, #46731, #37273, #27845, #20995, #16034, #1506, #39856, #25453, #19427, #26971, #13311, #17427, #590, #7789, #30988, #32363, #8828, #44584, #42622, #29269, #5904, #43817, #36905, #10639, #24477, #25059, #37803, #41732, #27244, #11375, #7836, #6764, #28307, #41420, #30493, #27946, #18129, #32811, #37765, #11933, #9260, #9158, #21200, #25567, #28655, #44503, #40770, #16787, #39213, #36633, #17106, #26530, #42828, #29335, #42718, #10839, #16621, #9789, #43654, #34528, #8991, #13741, #10203, #33192, #11767, #39525, #4917, #5996, #26482, #12306, #47305, #23884, #15615, #1392, #21810, #44134, #34583, #40387, #37299, #46095, #36234, #34328, #32709, #13798, #38846, #31091, #12628, #36, #9103, #15279, #41518, #32387, #14606, #4351, #24220, #14566, #21510, #36955, #12251, #38856, #4914, #34805, #32342, #25727, #527, #2045, #7411, #25319 ) ) ;
#7232 = CARTESIAN_POINT ( 'NONE',  ( -0.1270800023317771588, -0.1634296363546990094, -0.1270800023317771588 ) ) ;
#7233 = CARTESIAN_POINT ( 'NONE',  ( 0.1787899950787401604, -0.1123286926386875273, -0.07405724077823318263 ) ) ;
#7234 = CARTESIAN_POINT ( 'NONE',  ( 0.1264236179284866091, -0.06938976372576398377, 0.1264236179284866091 ) ) ;
#7235 = FACE_OUTER_BOUND ( 'NONE', #2150, .T. ) ;
#7236 = CARTESIAN_POINT ( 'NONE',  ( 0.8759842519685039353, 0.1787899950787401882, 0.6619094487651338010 ) ) ;
#7238 = CARTESIAN_POINT ( 'NONE',  ( 1.033464566929133799, 0.000000000000000000, 1.112204724409448842 ) ) ;
#7237 = CARTESIAN_POINT ( 'NONE',  ( -0.8512729243857075634, 0.1743046752856882431, 0.03937007874015844427 ) ) ;
#7239 = DIRECTION ( 'NONE',  ( 0.000000000000000000, 0.000000000000000000, -1.000000000000000000 ) ) ;
#7240 = CARTESIAN_POINT ( 'NONE',  ( -0.1787899950787401604, -0.4360236219934807145, -0.07405724077823318263 ) ) ;
#7241 = CARTESIAN_POINT ( 'NONE',  ( 0.8759842519685039353, 0.1574803149606299191, 0.9547244093412913246 ) ) ;
#7242 = CARTESIAN_POINT ( 'NONE',  ( 0.9500414927467378812, 0.1787899950787401604, 1.648622047190331230 ) ) ;
#7244 = FACE_OUTER_BOUND ( 'NONE', #5134, .T. ) ;
#7243 = CARTESIAN_POINT ( 'NONE',  ( -0.8759842519685039353, 0.000000000000000000, 0.000000000000000000 ) ) ;
#7245 = CARTESIAN_POINT ( 'NONE',  ( 0.8019270111902716547, 0.1787899950787401604, 0.5068897637257642197 ) ) ;
#7246 = ORIENTED_EDGE ( 'NONE', *, *, #37890, .F. ) ;
#7248 = ORIENTED_EDGE ( 'NONE', *, *, #29609, .T. ) ;
#7247 = EDGE_CURVE ( 'NONE', #9117, #3818, #12732, .T. ) ;
#7249 = FACE_OUTER_BOUND ( 'NONE', #42234, .T. ) ;
#7250 = CARTESIAN_POINT ( 'NONE',  ( 0.1264236179284866091, -0.3351377952218271283, -0.1264236179284866091 ) ) ;
#7252 = CARTESIAN_POINT ( 'NONE',  ( 0.1571168540705091266, 0.1349219317376052774, 0.04713923310955830254 ) ) ;
#7251 = CARTESIAN_POINT ( 'NONE',  ( -1.054774247047244096, 0.000000000000000000, 0.4601377952218267953 ) ) ;
#7253 = CARTESIAN_POINT ( 'NONE',  ( 0.1264236179284866091, -1.117618110182456714, -0.1264236179284866091 ) ) ;
#7254 = CARTESIAN_POINT ( 'NONE',  ( 1.054774247047244096, 0.000000000000000000, 0.02706692908009476414 ) ) ;
#7255 = CARTESIAN_POINT ( 'NONE',  ( 0.2362204724409448509, 0.1574803149606299191, 1.186023622047243986 ) ) ;
#7256 = CARTESIAN_POINT ( 'NONE',  ( -0.8019270111902717657, 0.1787899950787401604, 1.530511810969859443 ) ) ;
#7257 = VERTEX_POINT ( 'NONE', #29139 ) ;
#7258 = CIRCLE ( 'NONE', #27942, 0.09940944881889700324 ) ;
#7259 = CARTESIAN_POINT ( 'NONE',  ( -0.6971942568897637749, 2.189545951927499583E-17, 1.188484251914740275 ) ) ;
#7260 = CARTESIAN_POINT ( 'NONE',  ( -0.2610081115717082234, -0.1673295453843248459, -0.8705991056603238354 ) ) ;
#7261 = EDGE_CURVE ( 'NONE', #27285, #2328, #3453, .T. ) ;
#7262 = CARTESIAN_POINT ( 'NONE',  ( 0.9500414927467378812, -0.1787899950787401604, 1.122047244040725644 ) ) ;
#7263 = AXIS2_PLACEMENT_3D ( 'NONE', #1136, #44972, #1369 ) ;
#7264 = AXIS2_PLACEMENT_3D ( 'NONE', #44630, #4376, #12327 ) ;
#7265 = CARTESIAN_POINT ( 'NONE',  ( 0.7495606340400177148, -0.1264236179284866091, 1.818405511757259729 ) ) ;
#7266 = CARTESIAN_POINT ( 'NONE',  ( -0.9873396505805591694, -0.1113553986120547346, 0.6348425196850393526 ) ) ;
#7267 = CARTESIAN_POINT ( 'NONE',  ( -0.6971942568897648851, -0.07405724077823297447, 1.107283464513165949 ) ) ;
#7268 = CARTESIAN_POINT ( 'NONE',  ( 0.2397010884053811242, 4.466152701071653354E-17, 0.000000000000000000 ) ) ;
#7269 = CARTESIAN_POINT ( 'NONE',  ( -0.08568752866851420125, -0.2460225145194475105, -0.03726912461313686836 ) ) ;
#7270 = CARTESIAN_POINT ( 'NONE',  ( 0.8759842519685039353, -0.1787899950787401882, 0.2534448818360003908 ) ) ;
#7271 = CARTESIAN_POINT ( 'NONE',  ( -0.9500414927467377701, 0.1787899950787401604, 0.2657480314422993595 ) ) ;
#7272 = CARTESIAN_POINT ( 'NONE',  ( -1.054774247047244540, 0.07405724077823318263, 0.6938976377415123631 ) ) ;
#7273 = CARTESIAN_POINT ( 'NONE',  ( 0.9412147342319837628, 0.1574803149606300301, 1.582185039262551607 ) ) ;
#7274 = EDGE_LOOP ( 'NONE', ( #20749, #31049, #18927, #29137 ) ) ;
#7275 = CARTESIAN_POINT ( 'NONE',  ( 0.1264236179284866091, -0.05954724404072461036, -0.1264236179284866091 ) ) ;
#7276 = CARTESIAN_POINT ( 'NONE',  ( 0.7495606340400177148, -0.1264236179284866091, 0.7209645668753701386 ) ) ;
#7277 = CARTESIAN_POINT ( 'NONE',  ( 1.054774247047244540, -0.07405724077823318263, 1.087598425143086578 ) ) ;
#7278 = CARTESIAN_POINT ( 'NONE',  ( -0.6971942568897648851, -0.07405724077823297447, 1.894685039316315489 ) ) ;
#7279 = CARTESIAN_POINT ( 'NONE',  ( 1.054774247047244540, -0.07405724077823318263, 1.870078740103715331 ) ) ;
#7280 = EDGE_CURVE ( 'NONE', #34218, #7655, #7134, .T. ) ;
#7281 = DIRECTION ( 'NONE',  ( 0.000000000000000000, 0.000000000000000000, 1.000000000000000000 ) ) ;
#7282 = CARTESIAN_POINT ( 'NONE',  ( 0.1787899950787401604, -1.332801133583568776, -0.07405724077823318263 ) ) ;
#7283 = ORIENTED_EDGE ( 'NONE', *, *, #41575, .F. ) ;
#7284 = CARTESIAN_POINT ( 'NONE',  ( -0.1264236179284866091, -0.3499015747493862127, 0.1264236179284866091 ) ) ;
#7285 = CARTESIAN_POINT ( 'NONE',  ( 0.7495606340400177148, 0.1264236179284866091, 1.257381889710015743 ) ) ;
#7286 = DIRECTION ( 'NONE',  ( -0.000000000000000000, -0.000000000000000000, 1.000000000000000000 ) ) ;
#7287 = CARTESIAN_POINT ( 'NONE',  ( 0.7646288533564489232, 0.1113553986120547346, 1.392716535325543292 ) ) ;
#7288 = CARTESIAN_POINT ( 'NONE',  ( 0.7185039370078746268, -0.06523048226347956391, 1.921751968503937480 ) ) ;
#7289 = AXIS2_PLACEMENT_3D ( 'NONE', #7614, #32821, #25133 ) ;
#7290 = CIRCLE ( 'NONE', #14933, 0.09842519685039370636 ) ;
#7291 = CARTESIAN_POINT ( 'NONE',  ( -1.094772975963752103E-17, -1.668799212544661348, -0.1787899950787401882 ) ) ;
#7292 = CARTESIAN_POINT ( 'NONE',  ( -1.094772975963752103E-17, -1.742618110182456714, -0.1787899950787401882 ) ) ;
#7293 = CARTESIAN_POINT ( 'NONE',  ( -0.8759842519685039353, 0.1787899950787401882, 0.4699803149068661479 ) ) ;
#7294 = FACE_OUTER_BOUND ( 'NONE', #24349, .T. ) ;
#7296 = CARTESIAN_POINT ( 'NONE',  ( -0.7136811659038074795, -0.04132492306600986376, 1.984037415143555583 ) ) ;
#7295 = CARTESIAN_POINT ( 'NONE',  ( 0.1797182628040039087, -1.322386329268085525, 0.07444174185955046430 ) ) ;
#7297 = CARTESIAN_POINT ( 'NONE',  ( -1.033464566929133799, 0.000000000000000000, 1.190944881889763884 ) ) ;
#7298 = CARTESIAN_POINT ( 'NONE',  ( 0.7495606340400177148, -0.1264236179284866091, 1.232775590497417362 ) ) ;
#7299 = CARTESIAN_POINT ( 'NONE',  ( 1.054774247047244096, 0.000000000000000000, 1.715059055064346527 ) ) ;
#7301 = EDGE_CURVE ( 'NONE', #28693, #580, #2955, .T. ) ;
#7300 = CARTESIAN_POINT ( 'NONE',  ( 0.2362204724409449064, -0.5708661417322835607, 0.9783464566929134243 ) ) ;
#7302 = CARTESIAN_POINT ( 'NONE',  ( -0.1377952755905511584, 0.1564960629921283985, 0.7066929133858274037 ) ) ;
#7303 = CARTESIAN_POINT ( 'NONE',  ( 1.033464566929134687, -0.06523048226347956391, 0.8243110235145210130 ) ) ;
#7304 = LINE ( 'NONE', #21924, #46139 ) ;
#7305 = CARTESIAN_POINT ( 'NONE',  ( -1.033464566929133799, 0.000000000000000000, 1.811023621939716444 ) ) ;
#7306 = CARTESIAN_POINT ( 'NONE',  ( 0.9500414927467378812, -0.1787899950787401604, 0.1328740156942679607 ) ) ;
#7307 = EDGE_CURVE ( 'NONE', #6310, #19153, #31093, .T. ) ;
#7308 = CARTESIAN_POINT ( 'NONE',  ( 0.7025502174926940846, -0.01165807630412045957, 0.03936777229701638597 ) ) ;
#7309 = DIRECTION ( 'NONE',  ( -3.494233027178502331E-15, -1.000000000000000000, -0.000000000000000000 ) ) ;
#7310 = CARTESIAN_POINT ( 'NONE',  ( -0.9873396505805591694, -0.1113553986120547346, 1.924212598317669221 ) ) ;
#7311 = CARTESIAN_POINT ( 'NONE',  ( -0.8019270111902717657, -0.1787899950787401604, 1.230314960576156746 ) ) ;
#7312 = CARTESIAN_POINT ( 'NONE',  ( 0.9412147342319837628, -0.1574803149606297803, 0.6619094487113696967 ) ) ;
#7313 = VERTEX_POINT ( 'NONE', #10424 ) ;
#7314 = ( NAMED_UNIT ( * ) SI_UNIT ( $, .STERADIAN. ) SOLID_ANGLE_UNIT ( ) ) ;
#7315 = EDGE_CURVE ( 'NONE', #47128, #14871, #15017, .T. ) ;
#7316 = CARTESIAN_POINT ( 'NONE',  ( 0.9653975661131874997, 0.1427198071953197922, 0.03937007654474576623 ) ) ;
#7317 = PRODUCT_DEFINITION_SHAPE ( 'NONE', 'NONE',  #36823 ) ;
#7318 = CARTESIAN_POINT ( 'NONE',  ( -0.9412147342319837628, -0.1574803149606297803, 0.3469488187901108023 ) ) ;
#7319 = DIRECTION ( 'NONE',  ( -1.000000000000000000, 0.000000000000000000, 0.000000000000000000 ) ) ;
#7320 = CARTESIAN_POINT ( 'NONE',  ( 0.9500414927467378812, -0.1787899950787401604, 1.392716535379308285 ) ) ;
#7321 = ADVANCED_FACE ( 'NONE', ( #39153 ), #25023, .F. ) ;
#7322 = CARTESIAN_POINT ( 'NONE',  ( 0.7185039370078739607, 1.928577636452523993E-17, 0.2657480314960630197 ) ) ;
#7324 = DIRECTION ( 'NONE',  ( -3.469446951953614978E-15, -1.000000000000000000, 3.995705278811693553E-31 ) ) ;
#7323 = CARTESIAN_POINT ( 'NONE',  ( -0.8107537697050254399, 0.1574803149606300301, 0.1008858267716536417 ) ) ;
#7325 = CARTESIAN_POINT ( 'NONE',  ( -1.094772975963752103E-17, -0.1284448818360001965, -0.1787899950787401882 ) ) ;
#7326 = ORIENTED_EDGE ( 'NONE', *, *, #32760, .T. ) ;
#7327 = DIRECTION ( 'NONE',  ( 1.000000000000000000, 0.000000000000000000, -1.822029033848725275E-16 ) ) ;
#7328 = CARTESIAN_POINT ( 'NONE',  ( -0.3690944881889767215, 5.970426471673286898E-15, -0.7480314960629921295 ) ) ;
#7329 = DIRECTION ( 'NONE',  ( 0.000000000000000000, -1.000000000000000000, 0.000000000000000000 ) ) ;
#7330 = ORIENTED_EDGE ( 'NONE', *, *, #11662, .F. ) ;
#7331 = CARTESIAN_POINT ( 'NONE',  ( 0.9500414927467378812, -0.1787899950787401604, 0.6496062991588353874 ) ) ;
#7332 = ORIENTED_EDGE ( 'NONE', *, *, #16551, .F. ) ;
#7333 = CARTESIAN_POINT ( 'NONE',  ( -0.1574803149606300301, 0.05856299223351124628, -0.06523048226347956391 ) ) ;
#7334 = CARTESIAN_POINT ( 'NONE',  ( -1.054774247047244096, 0.000000000000000000, 1.168799212544661348 ) ) ;
#7335 = AXIS2_PLACEMENT_3D ( 'NONE', #19833, #27300, #34463 ) ;
#7336 = CIRCLE ( 'NONE', #16503, 0.1968503937007874405 ) ;
#7337 = ORIENTED_EDGE ( 'NONE', *, *, #32450, .T. ) ;
#7338 = CARTESIAN_POINT ( 'NONE',  ( -1.002407869896990045, 0.1264236179284866091, 1.050688976324189117 ) ) ;
#7339 = CARTESIAN_POINT ( 'NONE',  ( -0.9500414927467378812, 0.1787899950787401604, 0.7824803149068669805 ) ) ;
#7340 = CARTESIAN_POINT ( 'NONE',  ( -0.1631814734428333746, 0.2012842543237216564, -0.3131151337379057265 ) ) ;
#7341 = CARTESIAN_POINT ( 'NONE',  ( -0.8759842519685039353, 0.1787899950787401882, 0.1550196849856066983 ) ) ;
#7342 = CARTESIAN_POINT ( 'NONE',  ( 0.9412147342319837628, -0.1574803149606297803, 1.813484251968503935 ) ) ;
#7343 = CARTESIAN_POINT ( 'NONE',  ( 0.7185039370078739607, 1.928577636452523993E-17, 1.633858267609007875 ) ) ;
#7344 = CARTESIAN_POINT ( 'NONE',  ( 3.284318927891251994E-17, -0.7939231808276635549, 0.1787899950787401882 ) ) ;
#7345 = ORIENTED_EDGE ( 'NONE', *, *, #21362, .T. ) ;
#7346 = CARTESIAN_POINT ( 'NONE',  ( 0.7185039370078739607, 1.928577636452523993E-17, 0.3838582677165354173 ) ) ;
#7347 = CARTESIAN_POINT ( 'NONE',  ( 0.7185039370078739607, 1.928577636452523993E-17, 1.053149606299212504 ) ) ;
#7348 = APPLICATION_CONTEXT ( 'automotive_design' ) ;
#7349 = VERTEX_POINT ( 'NONE', #6569 ) ;
#7350 = CARTESIAN_POINT ( 'NONE',  ( 1.054774247047244096, 0.000000000000000000, 1.045767716481669440 ) ) ;
#7351 = CARTESIAN_POINT ( 'NONE',  ( -0.7495606340400177148, 0.1264236179284866091, 0.7455708660879684091 ) ) ;
#7352 = CARTESIAN_POINT ( 'NONE',  ( -0.7646288533564489232, -0.1113553986120547346, 0.5757874014672763607 ) ) ;
#7353 = CARTESIAN_POINT ( 'NONE',  ( -0.8019270111902716547, 0.1787899950787401604, 1.771653543253322249 ) ) ;
#7354 = AXIS2_PLACEMENT_3D ( 'NONE', #45958, #13173, #16520 ) ;
#7355 = CARTESIAN_POINT ( 'NONE',  ( -1.054774247047244540, 0.07405724077823318263, 0.06889763774151215492 ) ) ;
#7356 = CARTESIAN_POINT ( 'NONE',  ( 0.7646288533564489232, 0.1113553986120547346, 0.6151574803149606474 ) ) ;
#7357 = CARTESIAN_POINT ( 'NONE',  ( -0.1270800023317771588, -0.8720910536775334787, -0.1270800023317771588 ) ) ;
#7358 = FACE_OUTER_BOUND ( 'NONE', #30567, .T. ) ;
#7359 = CARTESIAN_POINT ( 'NONE',  ( -0.7646288533564489232, 0.1113553986120547346, 1.471456692805858113 ) ) ;
#7360 = CARTESIAN_POINT ( 'NONE',  ( 0.8019270111902717657, -0.1787899950787401604, 0.8021653542769460188 ) ) ;
#7361 = VECTOR ( 'NONE', #33663, 39.37007874015748143 ) ;
#7362 = ORIENTED_EDGE ( 'NONE', *, *, #29891, .T. ) ;
#7363 = DIRECTION ( 'NONE',  ( 1.000000000000000000, 0.000000000000000000, -1.822029033848725275E-16 ) ) ;
#7364 = CARTESIAN_POINT ( 'NONE',  ( 0.7646288533564489232, 0.1113553986120547346, 1.481299212598425230 ) ) ;
#7366 = LINE ( 'NONE', #25822, #14728 ) ;
#7365 = CARTESIAN_POINT ( 'NONE',  ( 0.9186159177457573488, -0.1711103661972301349, 1.988942757455733679 ) ) ;
#7367 = CARTESIAN_POINT ( 'NONE',  ( 0.7646288533564489232, -0.1113553986120547346, 1.481299212490897466 ) ) ;
#7368 = ORIENTED_EDGE ( 'NONE', *, *, #24534, .T. ) ;
#7369 = ( BOUNDED_CURVE ( )  B_SPLINE_CURVE ( 2, ( #42374, #38316, #16526, #42121, #5726, #9336, #23954, #20342, #31394 ),
 .UNSPECIFIED., .F., .T. ) 
 B_SPLINE_CURVE_WITH_KNOTS ( ( 3, 2, 2, 2, 3 ),
 ( 0.5699999999999999512, 0.5725000000000000089, 0.5749999999999999556, 0.5775000000000000133, 0.5799999999999999600 ),
 .UNSPECIFIED. ) 
 CURVE ( )  GEOMETRIC_REPRESENTATION_ITEM ( )  RATIONAL_B_SPLINE_CURVE ( ( 1.000000000000000000, 0.9238795325112899581, 1.000000000000000000, 0.9238795325112869605, 1.000000000000000000, 0.9238795325112869605, 1.000000000000000000, 0.9238795325112869605, 1.000000000000000000 ) ) 
 REPRESENTATION_ITEM ( '' )  ) ;
#7370 = EDGE_CURVE ( 'NONE', #9016, #19819, #39356, .T. ) ;
#7372 = CARTESIAN_POINT ( 'NONE',  ( 0.1574803149606300023, 0.08669520607260541856, -0.1182208702464773997 ) ) ;
#7371 = CARTESIAN_POINT ( 'NONE',  ( 0.9500414927467377701, -0.1787899950787401604, 0.7627952755367883864 ) ) ;
#7373 = CARTESIAN_POINT ( 'NONE',  ( 3.284318927891251994E-17, -0.8174212597887557941, 0.1787899950787401882 ) ) ;
#7374 = CYLINDRICAL_SURFACE ( 'NONE', #3963, 0.1574803149606299191 ) ;
#7375 = EDGE_LOOP ( 'NONE', ( #12548, #10542, #25317 ) ) ;
#7376 = CARTESIAN_POINT ( 'NONE',  ( -0.9873396505805591694, 0.1113553986120547346, 1.156496062992125928 ) ) ;
#7377 = DIRECTION ( 'NONE',  ( 0.000000000000000000, 0.000000000000000000, 1.000000000000000000 ) ) ;
#7378 = CARTESIAN_POINT ( 'NONE',  ( 1.054774247047244540, -0.07405724077823318263, 1.003937007820251193 ) ) ;
#7379 = EDGE_CURVE ( 'NONE', #13286, #21785, #40091, .T. ) ;
#7380 = DIRECTION ( 'NONE',  ( 0.000000000000000000, 0.000000000000000000, -1.000000000000000000 ) ) ;
#7381 = CARTESIAN_POINT ( 'NONE',  ( 2.892866454678787531E-17, -1.553149606299212504, 0.1574803149606299191 ) ) ;
#7382 = CARTESIAN_POINT ( 'NONE',  ( 0.7185039370078739607, 1.928577636452523993E-17, 1.250000000000000000 ) ) ;
#7383 = ORIENTED_EDGE ( 'NONE', *, *, #26695, .T. ) ;
#7384 = CARTESIAN_POINT ( 'NONE',  ( -1.054774247047244096, 0.000000000000000000, 0.1008858267178899676 ) ) ;
#7385 = CARTESIAN_POINT ( 'NONE',  ( -0.7185039370078739607, 1.928577636452523993E-17, 0.6988188976377952555 ) ) ;
#7386 = VERTEX_POINT ( 'NONE', #39621 ) ;
#7387 = CARTESIAN_POINT ( 'NONE',  ( -0.1113553986120547346, -0.2982283463491657294, -0.1113553986120547346 ) ) ;
#7388 = CARTESIAN_POINT ( 'NONE',  ( -0.8019270111902717657, -0.1787899950787401604, 0.3297244093950552069 ) ) ;
#7389 = ( BOUNDED_CURVE ( )  B_SPLINE_CURVE ( 2, ( #4436, #44692, #41326, #33494, #8054, #11436, #11910, #849, #26532 ),
 .UNSPECIFIED., .F., .F. ) 
 B_SPLINE_CURVE_WITH_KNOTS ( ( 3, 2, 2, 2, 3 ),
 ( 0.2399999999999999911, 0.2424999999999999933, 0.2449999999999999956, 0.2474999999999999978, 0.2500000000000000000 ),
 .UNSPECIFIED. ) 
 CURVE ( )  GEOMETRIC_REPRESENTATION_ITEM ( )  RATIONAL_B_SPLINE_CURVE ( ( 1.000000000000000000, 0.9238795325112869605, 1.000000000000000000, 0.9238795325112869605, 1.000000000000000000, 0.9238795325112869605, 1.000000000000000000, 0.9238795325112879597, 1.000000000000000000 ) ) 
 REPRESENTATION_ITEM ( '' )  ) ;
#7390 = DIRECTION ( 'NONE',  ( -1.000000000000000000, 0.000000000000000000, 0.000000000000000000 ) ) ;
#7391 = CARTESIAN_POINT ( 'NONE',  ( 0.9873396505805591694, -0.1113553986120547346, 0.9891732283464568232 ) ) ;
#7392 = FACE_OUTER_BOUND ( 'NONE', #20550, .T. ) ;
#7393 = FACE_OUTER_BOUND ( 'NONE', #39319, .T. ) ;
#7394 = CARTESIAN_POINT ( 'NONE',  ( -0.07405724077823318263, -0.3633129446071917679, 0.1787899950787401604 ) ) ;
#7395 = CARTESIAN_POINT ( 'NONE',  ( -0.004819917375885433841, -0.09842519685039370636, 0.1563213176426297146 ) ) ;
#7396 = CARTESIAN_POINT ( 'NONE',  ( 0.8070866141732283561, 0.000000000000000000, -0.7574803149606299524 ) ) ;
#7397 = CARTESIAN_POINT ( 'NONE',  ( -0.8759842519685039353, 0.000000000000000000, 4.498031496062992574 ) ) ;
#7398 = CARTESIAN_POINT ( 'NONE',  ( -0.8759842519685039353, 0.1787899950787401882, 0.3469488188438744070 ) ) ;
#7399 = CARTESIAN_POINT ( 'NONE',  ( -0.7495606340400177148, -0.1264236179284866091, 1.390255905458047447 ) ) ;
#7400 = VERTEX_POINT ( 'NONE', #42970 ) ;
#7401 = CARTESIAN_POINT ( 'NONE',  ( 0.07405724077823318263, -1.159448818843874074, -0.1787899950787401604 ) ) ;
#7402 = CARTESIAN_POINT ( 'NONE',  ( -0.1264236179284866091, -1.334153543253322916, 0.1264236179284866091 ) ) ;
#7403 = DIRECTION ( 'NONE',  ( 0.000000000000000000, 1.000000000000000000, 0.000000000000000000 ) ) ;
#7404 = DIRECTION ( 'NONE',  ( -0.9955207525527457468, 0.09454327705773096779, 6.999999999999998572E-15 ) ) ;
#7405 = CYLINDRICAL_SURFACE ( 'NONE', #40036, 0.1574803149606299191 ) ;
#7406 = CARTESIAN_POINT ( 'NONE',  ( -0.06523048226347956391, -0.1924212598425195098, -0.1574803149606300301 ) ) ;
#7407 = CARTESIAN_POINT ( 'NONE',  ( 0.9412147342319837628, -0.1574803149606297803, 1.843011810916095561 ) ) ;
#7408 = ORIENTED_EDGE ( 'NONE', *, *, #36911, .T. ) ;
#7409 = FACE_OUTER_BOUND ( 'NONE', #19472, .T. ) ;
#7410 = DIRECTION ( 'NONE',  ( -1.000000000000000000, 0.000000000000000000, 0.000000000000000000 ) ) ;
#7411 = ADVANCED_FACE ( 'NONE', ( #39383 ), #27267, .T. ) ;
#7413 = CARTESIAN_POINT ( 'NONE',  ( -0.8759842519685039353, -0.1574803149606299191, 0.8267716535433071723 ) ) ;
#7412 = PLANE ( 'NONE',  #17888 ) ;
#7414 = CARTESIAN_POINT ( 'NONE',  ( 0.4620708661417356478, 0.9842519685039370358, -0.7135826771653542844 ) ) ;
#7415 = VERTEX_POINT ( 'NONE', #18067 ) ;
#7416 = ADVANCED_FACE ( 'NONE', ( #3205 ), #43453, .T. ) ;
#7417 = ORIENTED_EDGE ( 'NONE', *, *, #34073, .T. ) ;
#7418 = DIRECTION ( 'NONE',  ( -1.000000000000000000, -5.377642775528100415E-15, 4.197754538034199640E-15 ) ) ;
#7419 = CARTESIAN_POINT ( 'NONE',  ( 0.1787899950787401604, -1.513779527505292322, -0.07405724077823318263 ) ) ;
#7420 = CARTESIAN_POINT ( 'NONE',  ( 0.06523048226347956391, -1.580216535325544402, 0.1574803149606297803 ) ) ;
#7421 = CARTESIAN_POINT ( 'NONE',  ( 0.1787899950787401882, -0.7337598424659212970, -2.189545951927503898E-17 ) ) ;
#7422 = CARTESIAN_POINT ( 'NONE',  ( -0.9412147342319837628, -0.1574803149606297803, 0.07135826760900840227 ) ) ;
#7423 = CARTESIAN_POINT ( 'NONE',  ( 0.1574803149606300301, -1.068405511811023612, -0.06523048226347956391 ) ) ;
#7424 = CARTESIAN_POINT ( 'NONE',  ( 0.8107537697050253289, 0.1574803149606300301, 0.9571850392625528281 ) ) ;
#7425 = CARTESIAN_POINT ( 'NONE',  ( 0.9412147342319837628, 0.1574803149606300301, 0.5290354330708663122 ) ) ;
#7426 = CARTESIAN_POINT ( 'NONE',  ( -0.7495606340400177148, 0.1264236179284866091, 0.3518700786863940833 ) ) ;
#7427 = ORIENTED_EDGE ( 'NONE', *, *, #7625, .T. ) ;
#7428 = ORIENTED_EDGE ( 'NONE', *, *, #45869, .F. ) ;
#7429 = CARTESIAN_POINT ( 'NONE',  ( -0.7495606340400177148, 0.1264236179284866091, 1.656003936954110412 ) ) ;
#7430 = ORIENTED_EDGE ( 'NONE', *, *, #40777, .F. ) ;
#7431 = CARTESIAN_POINT ( 'NONE',  ( 0.8019270111902717657, -0.1787899950787401604, 1.628937007820252303 ) ) ;
#7432 = CARTESIAN_POINT ( 'NONE',  ( -0.9500414927467378812, 0.1787899950787401604, 0.8612204723871809131 ) ) ;
#7433 = CARTESIAN_POINT ( 'NONE',  ( 0.6971942568897626646, 0.07405724077823318263, 0.2805118109698587214 ) ) ;
#7434 = CARTESIAN_POINT ( 'NONE',  ( 1.033464566929133799, 1.928577636452524610E-17, 4.498031496062992574 ) ) ;
#7435 = CARTESIAN_POINT ( 'NONE',  ( 0.6971942568897648851, 0.07405724077823318263, 0.7923228345919055560 ) ) ;
#7436 = CARTESIAN_POINT ( 'NONE',  ( -0.8759842519685039353, -0.1787899950787401882, 0.6422244093950550958 ) ) ;
#7437 = AXIS2_PLACEMENT_3D ( 'NONE', #1886, #16521, #31150 ) ;
#7438 = CARTESIAN_POINT ( 'NONE',  ( -0.8759842519685039353, 0.000000000000000000, 0.000000000000000000 ) ) ;
#7439 = FACE_OUTER_BOUND ( 'NONE', #1425, .T. ) ;
#7440 = CARTESIAN_POINT ( 'NONE',  ( -0.8019270111902717657, -0.1787899950787401604, 1.589566929080094448 ) ) ;
#7441 = CARTESIAN_POINT ( 'NONE',  ( -1.033464566929134687, 0.06523048226347956391, 1.892224409341292546 ) ) ;
#7442 = ORIENTED_EDGE ( 'NONE', *, *, #3583, .T. ) ;
#7443 = CARTESIAN_POINT ( 'NONE',  ( 1.002407869896990045, 0.1264236179284866091, 1.528051181048598384 ) ) ;
#7444 = CARTESIAN_POINT ( 'NONE',  ( -0.7185039370078739607, 1.928577636452523993E-17, 1.564960629921259949 ) ) ;
#7445 = ORIENTED_EDGE ( 'NONE', *, *, #20397, .F. ) ;
#7446 = ADVANCED_FACE ( 'NONE', ( #39854 ), #22128, .T. ) ;
#7447 = ORIENTED_EDGE ( 'NONE', *, *, #11487, .T. ) ;
#7448 = VERTEX_POINT ( 'NONE', #22603 ) ;
#7449 = CARTESIAN_POINT ( 'NONE',  ( -0.8759842519685039353, -0.1574803149606299191, 1.141732283464567121 ) ) ;
#7450 = CARTESIAN_POINT ( 'NONE',  ( 0.1787899950787401882, -0.4187992125446614589, -2.189545951927503898E-17 ) ) ;
#7451 = CARTESIAN_POINT ( 'NONE',  ( 0.1264236179284866091, -0.8518700786863936392, 0.1264236179284866091 ) ) ;
#7452 = ORIENTED_EDGE ( 'NONE', *, *, #38778, .T. ) ;
#7453 = CARTESIAN_POINT ( 'NONE',  ( -0.2471920549080087737, -0.08080427097412125337, -0.07167403547431477895 ) ) ;
#7454 = LINE ( 'NONE', #256, #3395 ) ;
#7455 = ( LENGTH_UNIT ( ) NAMED_UNIT ( * ) SI_UNIT ( $, .METRE. ) ) ;
#7456 = CARTESIAN_POINT ( 'NONE',  ( 0.8019270111902717657, -0.1787899950787401604, 1.781496062938362934 ) ) ;
#7457 = CARTESIAN_POINT ( 'NONE',  ( -0.1797182628040039365, -0.2372485339924944592, 0.000000000000000000 ) ) ;
#7458 = CARTESIAN_POINT ( 'NONE',  ( 0.07405724077823318263, -0.1221712123237270187, 0.1787899950787401604 ) ) ;
#7459 = CARTESIAN_POINT ( 'NONE',  ( 0.7185039370078739607, 1.928577636452523993E-17, 0.1377952754830242266 ) ) ;
#7460 = CARTESIAN_POINT ( 'NONE',  ( 0.8019270111902717657, 0.1787899950787401604, 0.6249999999462366729 ) ) ;
#7461 = CIRCLE ( 'NONE', #34288, 0.2431102362204724532 ) ;
#7462 = EDGE_CURVE ( 'NONE', #370, #28768, #69, .T. ) ;
#7464 = FILL_AREA_STYLE ('',( #33376 ) ) ;
#7463 = CARTESIAN_POINT ( 'NONE',  ( -0.9027521039302758288, 0.1709455099970345893, 0.03937007874015843734 ) ) ;
#7465 = CARTESIAN_POINT ( 'NONE',  ( -1.181162989532618060E-16, -0.0009842519685041700977, -0.3937007874015748254 ) ) ;
#7466 = CARTESIAN_POINT ( 'NONE',  ( 0.9873396505805591694, 0.1113553986120547346, 0.9498031494987716483 ) ) ;
#7467 = CARTESIAN_POINT ( 'NONE',  ( 0.8759842519685039353, 0.1787899950787401882, 1.887303149552535420 ) ) ;
#7468 = CARTESIAN_POINT ( 'NONE',  ( -0.2088134963331629290, -0.06712557525897992761, 0.1648743713630835273 ) ) ;
#7469 = EDGE_CURVE ( 'NONE', #36271, #4939, #44619, .T. ) ;
#7470 = CARTESIAN_POINT ( 'NONE',  ( 0.1558458267876807191, -0.09164332750980157261, 0.1168596517594511774 ) ) ;
#7471 = CARTESIAN_POINT ( 'NONE',  ( 3.284318927891251994E-17, -0.3499015747493862127, 0.1787899950787401882 ) ) ;
#7473 = CARTESIAN_POINT ( 'NONE',  ( 0.5057057357416000487, 1.205361022782824954E-17, -0.09842519685039370636 ) ) ;
#7472 = CARTESIAN_POINT ( 'NONE',  ( -0.6971942568897637749, 2.189545951927499583E-17, 0.4798228345919055560 ) ) ;
#7474 = CARTESIAN_POINT ( 'NONE',  ( -0.1787899950787401604, -1.065944881836000224, -0.07405724077823318263 ) ) ;
#7475 = CARTESIAN_POINT ( 'NONE',  ( 0.6971942568897626646, -0.07405724077823297447, 0.04921259837143338034 ) ) ;
#7476 = DIRECTION ( 'NONE',  ( 0.000000000000000000, -1.000000000000000000, 0.000000000000000000 ) ) ;
#7477 = CARTESIAN_POINT ( 'NONE',  ( -1.002407869896990045, -0.1264236179284866091, 1.670767716481669440 ) ) ;
#7478 = ORIENTED_EDGE ( 'NONE', *, *, #26809, .F. ) ;
#7479 = CARTESIAN_POINT ( 'NONE',  ( -0.8019270111902717657, 0.1787899950787401604, 1.220472440891118504 ) ) ;
#7480 = PLANE ( 'NONE',  #36037 ) ;
#7481 = CARTESIAN_POINT ( 'NONE',  ( -0.1574803149606297803, -1.196358267609008763, 0.06523048226347956391 ) ) ;
#7482 = CARTESIAN_POINT ( 'NONE',  ( 1.054774247047244540, 0.07405724077823318263, 0.02952755900135457801 ) ) ;
#7483 = CARTESIAN_POINT ( 'NONE',  ( -0.9412147342319837628, 0.1574803149606300301, 0.6471456692913395425 ) ) ;
#7484 = CARTESIAN_POINT ( 'NONE',  ( -0.6971942568897637749, 2.189545951927499583E-17, 0.9867125983714331028 ) ) ;
#7485 = CARTESIAN_POINT ( 'NONE',  ( -0.7185039370078746268, -0.06523048226347956391, 1.606791338582677309 ) ) ;
#7486 = CARTESIAN_POINT ( 'NONE',  ( 0.3906197235759846786, 4.466152701071653354E-17, 0.000000000000000000 ) ) ;
#7487 = CARTESIAN_POINT ( 'NONE',  ( 0.7495606340400177148, 0.1264236179284866091, 0.3174212597887562382 ) ) ;
#7488 = CARTESIAN_POINT ( 'NONE',  ( -0.7495606340400177148, 0.1264236179284866091, 0.2337598424659216578 ) ) ;
#7489 = CARTESIAN_POINT ( 'NONE',  ( -0.8019270111902717657, -0.1787899950787401604, 0.7972440944344250102 ) ) ;
#7490 = ORIENTED_EDGE ( 'NONE', *, *, #21276, .T. ) ;
#7491 = ( BOUNDED_CURVE ( )  B_SPLINE_CURVE ( 2, ( #7347, #33005, #29204, #3740, #11193, #29441, #44215, #3512, #40608 ),
 .UNSPECIFIED., .F., .T. ) 
 B_SPLINE_CURVE_WITH_KNOTS ( ( 3, 2, 2, 2, 3 ),
 ( 0.5300000000000000266, 0.5324999999999999734, 0.5350000000000000311, 0.5374999999999999778, 0.5400000000000000355 ),
 .UNSPECIFIED. ) 
 CURVE ( )  GEOMETRIC_REPRESENTATION_ITEM ( )  RATIONAL_B_SPLINE_CURVE ( ( 1.000000000000000000, 0.9238795325112869605, 1.000000000000000000, 0.9238795325112869605, 1.000000000000000000, 0.9238795325112869605, 1.000000000000000000, 0.9238795325112869605, 1.000000000000000000 ) ) 
 REPRESENTATION_ITEM ( '' )  ) ;
#7492 = CIRCLE ( 'NONE', #34303, 0.1574803149606300579 ) ;
#7493 = CARTESIAN_POINT ( 'NONE',  ( -0.1787899950787401882, -0.04478346451316559534, 0.000000000000000000 ) ) ;
#7494 = ORIENTED_EDGE ( 'NONE', *, *, #46842, .T. ) ;
#7495 = CARTESIAN_POINT ( 'NONE',  ( 0.6971942568897626646, 0.07405724077823318263, 0.7529527558517473684 ) ) ;
#7496 = CARTESIAN_POINT ( 'NONE',  ( 0.8019270111902716547, -0.1787899950787401604, 1.117125984198206412 ) ) ;
#7497 = CARTESIAN_POINT ( 'NONE',  ( -0.9500414927467377701, 0.1787899950787401604, 1.840551181048599938 ) ) ;
#7498 = ORIENTED_EDGE ( 'NONE', *, *, #34709, .T. ) ;
#7499 = CARTESIAN_POINT ( 'NONE',  ( 0.8019270111902717657, -0.1787899950787401604, 1.938976377898990799 ) ) ;
#7500 = AXIS2_PLACEMENT_3D ( 'NONE', #31272, #31973, #42485 ) ;
#7501 = CARTESIAN_POINT ( 'NONE',  ( -0.7185039370078739607, 1.928577636452523993E-17, 0.1870078740157480324 ) ) ;
#7502 = CARTESIAN_POINT ( 'NONE',  ( -0.1264236179284866091, -1.350025543032387976, 0.1264236179284866091 ) ) ;
#7503 = ORIENTED_EDGE ( 'NONE', *, *, #9522, .T. ) ;
#7504 = CARTESIAN_POINT ( 'NONE',  ( -0.07405724077823318263, -0.2293307086076536994, 0.1787899950787401604 ) ) ;
#7505 = CARTESIAN_POINT ( 'NONE',  ( -0.1574803149606300301, 0.01919291349335381161, -0.06523048226347956391 ) ) ;
#7506 = ORIENTED_EDGE ( 'NONE', *, *, #10016, .T. ) ;
#7507 = CARTESIAN_POINT ( 'NONE',  ( 0.7495606340400177148, 0.1264236179284866091, 1.218011810969858111 ) ) ;
#7508 = CARTESIAN_POINT ( 'NONE',  ( 0.000000000000000000, 1.205361022782826802E-17, -0.09842519685039370636 ) ) ;
#7509 = CARTESIAN_POINT ( 'NONE',  ( -0.7185039370078746268, 0.06523048226347956391, 1.001476377845229804 ) ) ;
#7510 = CARTESIAN_POINT ( 'NONE',  ( 1.002407869896990045, -0.1264236179284866091, 0.05659448813521283234 ) ) ;
#7511 = EDGE_CURVE ( 'NONE', #9744, #20867, #41631, .T. ) ;
#7512 = CARTESIAN_POINT ( 'NONE',  ( -0.1787899950787401882, -1.619586614119464585, 0.000000000000000000 ) ) ;
#7513 = CARTESIAN_POINT ( 'NONE',  ( -0.1787899950787401604, -1.735236220418678643, -0.07405724077823318263 ) ) ;
#7514 = CARTESIAN_POINT ( 'NONE',  ( -0.6971942568897637749, 2.189545951927499583E-17, 0.4798228345919055560 ) ) ;
#7515 = AXIS2_PLACEMENT_3D ( 'NONE', #24865, #36130, #25356 ) ;
#7516 = CARTESIAN_POINT ( 'NONE',  ( -0.1377952755905511306, 1.687505431895958571E-17, -0.3149606299212598381 ) ) ;
#7518 = CARTESIAN_POINT ( 'NONE',  ( -0.7105523864618353835, 0.009560899065524132434, 1.983094267893590334 ) ) ;
#7517 = CARTESIAN_POINT ( 'NONE',  ( -0.1270800023317771588, -1.492169793835013802, 0.1270800023317771588 ) ) ;
#7519 = CARTESIAN_POINT ( 'NONE',  ( 0.1602931993194442739, -0.07955613945526318620, 0.1377952755905511861 ) ) ;
#7520 = CARTESIAN_POINT ( 'NONE',  ( 1.054774247047244540, 0.07405724077823318263, 1.171259842465921741 ) ) ;
#7521 = CARTESIAN_POINT ( 'NONE',  ( 0.8019270111902716547, 0.1787899950787401604, 1.648622047190331230 ) ) ;
#7522 = CARTESIAN_POINT ( 'NONE',  ( 0.1627249056762490320, 0.5419983459879528231, -0.7609487005970335671 ) ) ;
#7523 = EDGE_CURVE ( 'NONE', #7079, #27600, #43936, .T. ) ;
#7524 = CARTESIAN_POINT ( 'NONE',  ( 0.05391291923841142614, 0.1299212598425196763, 0.1701573640430796008 ) ) ;
#7525 = DIRECTION ( 'NONE',  ( -1.000000000000000000, 0.000000000000000000, -7.047314121155770932E-15 ) ) ;
#7526 = LINE ( 'NONE', #40804, #6013 ) ;
#7528 = CARTESIAN_POINT ( 'NONE',  ( -0.7185039370078739607, 1.928577636452523993E-17, 1.919291338582677309 ) ) ;
#7527 = CARTESIAN_POINT ( 'NONE',  ( -0.1113553986120547346, -0.8100393699712126194, -0.1113553986120547346 ) ) ;
#7529 = CARTESIAN_POINT ( 'NONE',  ( 0.8759842519685039353, -0.1574803149606299191, 0.5413385825696385156 ) ) ;
#7530 = CIRCLE ( 'NONE', #20536, 0.09842519685039310962 ) ;
#7531 = CARTESIAN_POINT ( 'NONE',  ( 1.054774247047244540, -0.07405724077823318263, 0.3346456692375748831 ) ) ;
#7532 = CARTESIAN_POINT ( 'NONE',  ( 0.7099242514868753240, -0.04392859927252232982, 0.03937034313776070077 ) ) ;
#7534 = CARTESIAN_POINT ( 'NONE',  ( -0.8759842519685039353, 0.000000000000000000, 0.000000000000000000 ) ) ;
#7533 = CARTESIAN_POINT ( 'NONE',  ( 1.054774247047244540, -0.07405724077823318263, 1.279527559001355730 ) ) ;
#7535 = EDGE_CURVE ( 'NONE', #5864, #18566, #12069, .T. ) ;
#7536 = CARTESIAN_POINT ( 'NONE',  ( 0.1574803149606299191, 1.928577636452524918E-17, -0.07924015748031493223 ) ) ;
#7537 = CARTESIAN_POINT ( 'NONE',  ( -0.6971942568897637749, 2.189545951927499583E-17, 1.222933070812378009 ) ) ;
#7538 = CARTESIAN_POINT ( 'NONE',  ( 0.7185039370078746268, 0.06523048226347956391, 0.7258858266641259327 ) ) ;
#7539 = ORIENTED_EDGE ( 'NONE', *, *, #32770, .T. ) ;
#7540 = CARTESIAN_POINT ( 'NONE',  ( 0.5717220857807087109, 0.09842519685039370636, 1.205361022782828805E-17 ) ) ;
#7541 = CARTESIAN_POINT ( 'NONE',  ( 0.8895385448872797918, 0.1731831457854506318, 0.03937007870486500943 ) ) ;
#7542 = CARTESIAN_POINT ( 'NONE',  ( -0.8070866141732283561, -0.3937007874015746034, -0.8559055118110230342 ) ) ;
#7543 = CARTESIAN_POINT ( 'NONE',  ( 0.5555748031496099415, 0.6449983665207553729, -0.7480314960629920185 ) ) ;
#7544 = CARTESIAN_POINT ( 'NONE',  ( 0.6971942568897637749, 2.189545951927499583E-17, 1.459153543253322693 ) ) ;
#7545 = CARTESIAN_POINT ( 'NONE',  ( -0.7185039370078746268, 0.06523048226347956391, 1.168799212598425896 ) ) ;
#7546 = CARTESIAN_POINT ( 'NONE',  ( 0.1618536817988697474, -0.1553100982366859006, 0.01202753685200385302 ) ) ;
#7547 = CARTESIAN_POINT ( 'NONE',  ( -0.8759842519685039353, 0.1787899950787401882, 0.07135826766277185429 ) ) ;
#7548 = CARTESIAN_POINT ( 'NONE',  ( -0.07405724077823318263, -0.1259842519147404416, -0.1787899950787401604 ) ) ;
#7549 = CARTESIAN_POINT ( 'NONE',  ( 0.7185039370078746268, -0.06523048226347956391, 1.321358267609009429 ) ) ;
#7550 = VERTEX_POINT ( 'NONE', #36986 ) ;
#7551 = CARTESIAN_POINT ( 'NONE',  ( -0.8107537697050254399, 0.1574803149606300301, 0.3764763779527559029 ) ) ;
#7552 = CARTESIAN_POINT ( 'NONE',  ( -0.1235961452251413406, -0.09842519685039370636, 0.2140748031496062798 ) ) ;
#7553 = CARTESIAN_POINT ( 'NONE',  ( 0.6971942568897626646, 0.07405724077823318263, 0.5561023621509617598 ) ) ;
#7554 = ORIENTED_EDGE ( 'NONE', *, *, #41843, .T. ) ;
#7555 = CARTESIAN_POINT ( 'NONE',  ( -0.1787899950787401882, -1.816437007820251859, 0.000000000000000000 ) ) ;
#7556 = CARTESIAN_POINT ( 'NONE',  ( -0.8019270111902717657, -0.1787899950787401604, 1.195866141678520345 ) ) ;
#7557 = DIRECTION ( 'NONE',  ( 0.000000000000000000, 1.000000000000000000, 0.000000000000000000 ) ) ;
#7558 = CARTESIAN_POINT ( 'NONE',  ( -1.002407869896990045, -0.1264236179284866091, 0.8489173227808819444 ) ) ;
#7559 = CARTESIAN_POINT ( 'NONE',  ( 0.8759842519685039353, 0.000000000000000000, 2.007874015640504162 ) ) ;
#7560 = CARTESIAN_POINT ( 'NONE',  ( -0.8019270111902717657, 0.1787899950787401604, 0.1968503936470238913 ) ) ;
#7561 = CARTESIAN_POINT ( 'NONE',  ( 0.003583035186818364637, 0.1402401972141572029, -0.03270545601320399426 ) ) ;
#7562 = DIRECTION ( 'NONE',  ( -1.000000000000000000, 0.000000000000000000, 0.000000000000000000 ) ) ;
#7563 = CARTESIAN_POINT ( 'NONE',  ( 3.284318927891251994E-17, -0.8332932595678209653, 0.1787899950787401882 ) ) ;
#7564 = ORIENTED_EDGE ( 'NONE', *, *, #19593, .T. ) ;
#7565 = CARTESIAN_POINT ( 'NONE',  ( -0.9873396505805591694, -0.1113553986120547346, 0.8612204723334173639 ) ) ;
#7566 = ORIENTED_EDGE ( 'NONE', *, *, #9639, .F. ) ;
#7567 = ORIENTED_EDGE ( 'NONE', *, *, #14071, .F. ) ;
#7568 = ADVANCED_FACE ( 'NONE', ( #11132 ), #22840, .T. ) ;
#7569 = LINE ( 'NONE', #26037, #24837 ) ;
#7570 = TOROIDAL_SURFACE ( 'NONE', #6021, 0.7775590551181102983, 0.009842519685039369942 ) ;
#7571 = CARTESIAN_POINT ( 'NONE',  ( -0.8759842519685039353, 0.1787899950787401882, 0.8193897637257637756 ) ) ;
#7572 = FACE_OUTER_BOUND ( 'NONE', #9048, .T. ) ;
#7573 = EDGE_CURVE ( 'NONE', #3237, #43250, #236, .T. ) ;
#7574 = CONICAL_SURFACE ( 'NONE', #13695, 0.1574803149606299191, 0.9599310885968713736 ) ;
#7575 = ADVANCED_FACE ( 'NONE', ( #15673 ), #33191, .F. ) ;
#7576 = CARTESIAN_POINT ( 'NONE',  ( -0.7495606340400177148, 0.1264236179284866091, 1.813484251914740053 ) ) ;
#7577 = ORIENTED_EDGE ( 'NONE', *, *, #4400, .F. ) ;
#7578 = CARTESIAN_POINT ( 'NONE',  ( 0.9873396505805591694, 0.1113553986120547346, 0.6840551181102363376 ) ) ;
#7579 = CARTESIAN_POINT ( 'NONE',  ( -0.1797182628040039087, -0.9483705812365885723, -0.07444174185955065859 ) ) ;
#7580 = LINE ( 'NONE', #384, #14108 ) ;
#7581 = CARTESIAN_POINT ( 'NONE',  ( -0.8107537697050253289, 0.1574803149606300301, 1.468996062884598830 ) ) ;
#7582 = CARTESIAN_POINT ( 'NONE',  ( 0.6971942568897626646, -0.07405724077823297447, 0.7578740156942689321 ) ) ;
#7583 = DIRECTION ( 'NONE',  ( 0.000000000000000000, 0.000000000000000000, -1.000000000000000000 ) ) ;
#7584 = CARTESIAN_POINT ( 'NONE',  ( 0.7646288533564489232, -0.1113553986120547346, 1.412401574803149540 ) ) ;
#7586 = DIRECTION ( 'NONE',  ( 0.000000000000000000, 0.000000000000000000, -1.000000000000000000 ) ) ;
#7585 = CARTESIAN_POINT ( 'NONE',  ( 0.8111863842034094940, -0.1598013345783634853, 1.986982674346258415 ) ) ;
#7587 = CARTESIAN_POINT ( 'NONE',  ( 0.8759842519685039353, -0.1574803149606299191, 1.722440944774362270 ) ) ;
#7588 = CARTESIAN_POINT ( 'NONE',  ( -0.06523048226347956391, -0.6550196849318432601, -0.1574803149606300301 ) ) ;
#7590 = CARTESIAN_POINT ( 'NONE',  ( -0.9412147342319837628, -0.1574803149606297803, 1.419783464566930054 ) ) ;
#7589 = CARTESIAN_POINT ( 'NONE',  ( 0.8019270111902716547, 0.1787899950787401604, 0.9005905511273391006 ) ) ;
#7591 = VECTOR ( 'NONE', #41985, 39.37007874015748143 ) ;
#7592 = CARTESIAN_POINT ( 'NONE',  ( 0.1264236179284866091, -0.7731299212060788184, 0.1264236179284866091 ) ) ;
#7593 = LINE ( 'NONE', #37786, #8548 ) ;
#7594 = CARTESIAN_POINT ( 'NONE',  ( 0.7646288533564489232, 0.1113553986120547346, 0.9301181102362204856 ) ) ;
#7595 = LINE ( 'NONE', #29236, #46591 ) ;
#7596 = CARTESIAN_POINT ( 'NONE',  ( 0.9500414927467378812, 0.1787899950787401604, 0.9744094487651340231 ) ) ;
#7597 = CARTESIAN_POINT ( 'NONE',  ( -0.1574803149606300301, -1.722933070866142335, -0.06523048226347956391 ) ) ;
#7598 = CARTESIAN_POINT ( 'NONE',  ( 0.000000000000000000, 0.000000000000000000, -0.0009999999999999347518 ) ) ;
#7599 = ORIENTED_EDGE ( 'NONE', *, *, #37764, .T. ) ;
#7600 = DIRECTION ( 'NONE',  ( -1.000000000000000000, 0.000000000000000000, 0.000000000000000000 ) ) ;
#7601 = ORIENTED_EDGE ( 'NONE', *, *, #7616, .F. ) ;
#7602 = AXIS2_PLACEMENT_3D ( 'NONE', #4226, #18855, #33512 ) ;
#7603 = CARTESIAN_POINT ( 'NONE',  ( 0.7185039370078739607, 1.928577636452523993E-17, 1.761811023622047223 ) ) ;
#7604 = CARTESIAN_POINT ( 'NONE',  ( 0.07405724077823318263, -1.449803149552535642, 0.1787899950787401604 ) ) ;
#7605 = CARTESIAN_POINT ( 'NONE',  ( 0.9873396505805591694, -0.1113553986120547346, 0.3494094487113705294 ) ) ;
#7606 = CARTESIAN_POINT ( 'NONE',  ( -1.002407869896990045, -0.1264236179284866091, 1.749507873961984483 ) ) ;
#7607 = CARTESIAN_POINT ( 'NONE',  ( -1.002407869896990045, 0.1264236179284866091, 0.8538385826234016207 ) ) ;
#7608 = CARTESIAN_POINT ( 'NONE',  ( -0.9412147342319837628, -0.1574803149606297803, 0.1107283463491657988 ) ) ;
#7609 = CARTESIAN_POINT ( 'NONE',  ( 0.7185039370078746268, -0.06523048226347956391, 0.9768700787401572994 ) ) ;
#7610 = FACE_OUTER_BOUND ( 'NONE', #40216, .T. ) ;
#7611 = CARTESIAN_POINT ( 'NONE',  ( 0.07034821948466062069, 0.08559642391438646025, -0.2448175074096619885 ) ) ;
#7612 = CARTESIAN_POINT ( 'NONE',  ( -0.2644617891023671730, 0.1618364700813167412, -0.9199053124863334485 ) ) ;
#7613 = CARTESIAN_POINT ( 'NONE',  ( -0.2329120156667235930, -0.08955973368226792519, -0.06010530154842106537 ) ) ;
#7614 = CARTESIAN_POINT ( 'NONE',  ( -0.8070866141732283561, 0.000000000000000000, 0.7574803149606299524 ) ) ;
#7615 = DIRECTION ( 'NONE',  ( 0.000000000000000000, 0.000000000000000000, 1.000000000000000000 ) ) ;
#7616 = EDGE_CURVE ( 'NONE', #12883, #35279, #40554, .T. ) ;
#7617 = CARTESIAN_POINT ( 'NONE',  ( -1.002407869896990045, -0.1264236179284866091, 0.3715551180564728440 ) ) ;
#7618 = EDGE_CURVE ( 'NONE', #31956, #27577, #33425, .T. ) ;
#7620 = EDGE_LOOP ( 'NONE', ( #17052, #7176, #27750, #25201 ) ) ;
#7619 = AXIS2_PLACEMENT_3D ( 'NONE', #26889, #41446, #8648 ) ;
#7621 = ORIENTED_EDGE ( 'NONE', *, *, #13429, .T. ) ;
#7622 = EDGE_CURVE ( 'NONE', #42395, #24436, #30308, .T. ) ;
#7623 = CARTESIAN_POINT ( 'NONE',  ( -1.002407869896990045, 0.1264236179284866091, 1.331200787347811110 ) ) ;
#7624 = ORIENTED_EDGE ( 'NONE', *, *, #40079, .F. ) ;
#7625 = EDGE_CURVE ( 'NONE', #28962, #38421, #18013, .T. ) ;
#7626 = CARTESIAN_POINT ( 'NONE',  ( 0.1787899950787401882, -1.324311023568283341, -2.189545951927503898E-17 ) ) ;
#7627 = AXIS2_PLACEMENT_3D ( 'NONE', #46738, #32640, #14410 ) ;
#7628 = CARTESIAN_POINT ( 'NONE',  ( 0.1264236179284866091, -1.432578740103716664, -0.1264236179284866091 ) ) ;
#7629 = ( BOUNDED_CURVE ( )  B_SPLINE_CURVE ( 2, ( #10437, #25037, #17368, #46832, #42741, #31782, #20728, #3217, #20499 ),
 .UNSPECIFIED., .F., .T. ) 
 B_SPLINE_CURVE_WITH_KNOTS ( ( 3, 2, 2, 2, 3 ),
 ( 0.3200000000000000067, 0.3225000000000000089, 0.3250000000000000111, 0.3275000000000000133, 0.3300000000000000155 ),
 .UNSPECIFIED. ) 
 CURVE ( )  GEOMETRIC_REPRESENTATION_ITEM ( )  RATIONAL_B_SPLINE_CURVE ( ( 1.000000000000000000, 0.9238795325112869605, 1.000000000000000000, 0.9238795325112869605, 1.000000000000000000, 0.9238795325112869605, 1.000000000000000000, 0.9238795325112869605, 1.000000000000000000 ) ) 
 REPRESENTATION_ITEM ( '' )  ) ;
#7630 = DIRECTION ( 'NONE',  ( 1.000000000000000000, 0.000000000000000000, 0.000000000000000000 ) ) ;
#7631 = DIRECTION ( 'NONE',  ( 1.000000000000000000, 0.000000000000000000, 0.000000000000000000 ) ) ;
#7632 = CARTESIAN_POINT ( 'NONE',  ( -0.8759842519685039353, 0.1574803149606299191, 1.072834645561763889 ) ) ;
#7633 = VECTOR ( 'NONE', #20931, 39.37007874015748143 ) ;
#7634 = FACE_OUTER_BOUND ( 'NONE', #45486, .T. ) ;
#7635 = CARTESIAN_POINT ( 'NONE',  ( -0.1574803149606299191, -0.2244094488188976555, 0.000000000000000000 ) ) ;
#7636 = ORIENTED_EDGE ( 'NONE', *, *, #39035, .F. ) ;
#7637 = CARTESIAN_POINT ( 'NONE',  ( 0.8107537697050253289, 0.1574803149606300301, 1.902066929026330788 ) ) ;
#7638 = EDGE_LOOP ( 'NONE', ( #36980, #44240, #20004, #27759 ) ) ;
#7639 = CARTESIAN_POINT ( 'NONE',  ( -0.1355716054994425268, -0.09355356640806745949, -0.1165615083013312042 ) ) ;
#7640 = CARTESIAN_POINT ( 'NONE',  ( 0.8107537697050253289, 0.1574803149606300301, 1.006397637795276800 ) ) ;
#7641 = DIRECTION ( 'NONE',  ( 0.000000000000000000, 0.000000000000000000, 1.000000000000000000 ) ) ;
#7642 = CARTESIAN_POINT ( 'NONE',  ( 0.1113553986120547346, -0.5049212597349921339, -0.1113553986120547346 ) ) ;
#7643 = DIRECTION ( 'NONE',  ( -0.000000000000000000, 0.6156614753256597350, 0.7880107536067206819 ) ) ;
#7644 = CARTESIAN_POINT ( 'NONE',  ( -0.1850388559550336376, -0.08126078924477943277, -0.1786007880584631891 ) ) ;
#7645 = CARTESIAN_POINT ( 'NONE',  ( -0.2617290863461586570, 0.1662196327273371133, 0.8538226567781561638 ) ) ;
#7646 = CARTESIAN_POINT ( 'NONE',  ( -0.8107537697050254399, -0.1574803149606297803, 0.9817913385826764205 ) ) ;
#7647 = CARTESIAN_POINT ( 'NONE',  ( 0.1787899950787401604, -1.553149606245448178, -0.07405724077823318263 ) ) ;
#7648 = CARTESIAN_POINT ( 'NONE',  ( 0.1113553986120547346, -1.538385826664125711, 0.1113553986120547346 ) ) ;
#7649 = CARTESIAN_POINT ( 'NONE',  ( 0.1787899950787401604, -0.8100393700249772788, -0.07405724077823318263 ) ) ;
#7650 = CARTESIAN_POINT ( 'NONE',  ( 0.1113553986120547346, -1.233267716535433101, 0.1113553986120547346 ) ) ;
#7652 = ( BOUNDED_CURVE ( )  B_SPLINE_CURVE ( 2, ( #925, #38311, #41400, #26840, #15823, #37353, #15583, #1396, #19142 ),
 .UNSPECIFIED., .F., .T. ) 
 B_SPLINE_CURVE_WITH_KNOTS ( ( 3, 2, 2, 2, 3 ),
 ( 0.09500000000000000111, 0.09750000000000000333, 0.1000000000000000056, 0.1024999999999999939, 0.1049999999999999961 ),
 .UNSPECIFIED. ) 
 CURVE ( )  GEOMETRIC_REPRESENTATION_ITEM ( )  RATIONAL_B_SPLINE_CURVE ( ( 1.000000000000000000, 0.9238795325112869605, 1.000000000000000000, 0.9238795325112869605, 1.000000000000000000, 0.9238795325112869605, 1.000000000000000000, 0.9238795325112869605, 1.000000000000000000 ) ) 
 REPRESENTATION_ITEM ( '' )  ) ;
#7651 = CARTESIAN_POINT ( 'NONE',  ( 0.9873396505805591694, 0.1113553986120547346, 1.028543306979086802 ) ) ;
#7653 = DIRECTION ( 'NONE',  ( 0.000000000000000000, -1.000000000000000000, 0.000000000000000000 ) ) ;
#7654 = CARTESIAN_POINT ( 'NONE',  ( -1.054774247047244096, 0.000000000000000000, 0.3764763778989925203 ) ) ;
#7655 = VERTEX_POINT ( 'NONE', #3684 ) ;
#7656 = ORIENTED_EDGE ( 'NONE', *, *, #19032, .F. ) ;
#7657 = ORIENTED_EDGE ( 'NONE', *, *, #7160, .T. ) ;
#7658 = CARTESIAN_POINT ( 'NONE',  ( -1.002407869896990045, -0.1264236179284866091, 1.636318897584031484 ) ) ;
#7659 = CARTESIAN_POINT ( 'NONE',  ( 0.7495606340400177148, 0.1264236179284866091, 1.774114173174582643 ) ) ;
#7660 = CARTESIAN_POINT ( 'NONE',  ( -0.7495606340400177148, -0.1264236179284866091, 0.7209645668753701386 ) ) ;
#7661 = DIRECTION ( 'NONE',  ( 0.000000000000000000, 0.000000000000000000, -1.000000000000000000 ) ) ;
#7662 = CARTESIAN_POINT ( 'NONE',  ( 0.9500414927467378812, 0.1787899950787401604, 0.3100393700249766682 ) ) ;
#7663 = AXIS2_PLACEMENT_3D ( 'NONE', #26053, #29917, #8526 ) ;
#7664 = CARTESIAN_POINT ( 'NONE',  ( -0.8759842519685039353, -0.1574803149606299191, 0.4625984250893235838 ) ) ;
#7665 = CARTESIAN_POINT ( 'NONE',  ( -1.002407869896990045, -0.1264236179284866091, 1.198326771599779628 ) ) ;
#7666 = CARTESIAN_POINT ( 'NONE',  ( -1.054774247047244540, 0.07405724077823318263, 0.6545275590013546196 ) ) ;
#7667 = CIRCLE ( 'NONE', #20659, 0.5019685039370077595 ) ;
#7668 = CARTESIAN_POINT ( 'NONE',  ( 0.0005737749932833635311, -0.1108949133173220275, 0.08352002191787535890 ) ) ;
#7669 = CARTESIAN_POINT ( 'NONE',  ( -0.8759842519685039353, 0.1574803149606299191, 1.663385826664125933 ) ) ;
#7670 = CARTESIAN_POINT ( 'NONE',  ( -0.6971942568897648851, 0.07405724077823318263, 1.540354330654897685 ) ) ;
#7671 = CARTESIAN_POINT ( 'NONE',  ( -1.033464566929134687, 0.06523048226347956391, 1.852854330601134691 ) ) ;
#7672 = ORIENTED_EDGE ( 'NONE', *, *, #7301, .F. ) ;
#7673 = CARTESIAN_POINT ( 'NONE',  ( 0.2871444924769515628, 0.9382165298418956301, -1.070508272602716637 ) ) ;
#7674 = CARTESIAN_POINT ( 'NONE',  ( 0.9412147342319837628, 0.1574803149606300301, 1.631397637795275468 ) ) ;
#7675 = CIRCLE ( 'NONE', #13804, 0.08090551181102362266 ) ;
#7676 = CARTESIAN_POINT ( 'NONE',  ( 0.05548443445031432664, -0.09851382384500374789, 0.1418811546954053260 ) ) ;
#7677 = CARTESIAN_POINT ( 'NONE',  ( 0.3425196850393700809, 4.616380251121755931E-17, 0.000000000000000000 ) ) ;
#7678 = EDGE_LOOP ( 'NONE', ( #19026, #15942, #11771, #16125 ) ) ;
#7679 = EDGE_CURVE ( 'NONE', #3517, #33652, #31228, .T. ) ;
#7680 = EDGE_LOOP ( 'NONE', ( #32414, #12904, #31395, #10232, #28916, #42307 ) ) ;
#7681 = B_SPLINE_CURVE_WITH_KNOTS ( 'NONE', 3,
 ( #12424, #8797, #20054, #23430, #1841, #16480, #38038, #19820, #38510, #3506, #3964, #18581, #29671, #25568, #4418, #7340, #21953, #4188, #43982 ),
 .UNSPECIFIED., .F., .F.,
 ( 4, 2, 2, 1, 2, 2, 2, 2, 2, 4 ),
 ( 0.000000000000000000, 0.2499999999999990563, 0.3749999999999982236, 0.4374999999999977796, 0.4687499999999974465, 0.4999999999999971134, 0.6249999999999972244, 0.6874999999999972244, 0.7499999999999971134, 1.000000000000000000 ),
 .UNSPECIFIED. ) ;
#7682 = EDGE_CURVE ( 'NONE', #23548, #1642, #5424, .T. ) ;
#7683 = CARTESIAN_POINT ( 'NONE',  ( 0.07405724077823318263, -0.9625984251430860228, -0.1787899950787401604 ) ) ;
#7684 = CARTESIAN_POINT ( 'NONE',  ( 0.1264236179284866091, -0.4532480314422991929, -0.1264236179284866091 ) ) ;
#7685 = CARTESIAN_POINT ( 'NONE',  ( 0.1787899950787401604, -0.9675196849856075865, 0.07405724077823318263 ) ) ;
#7686 = ORIENTED_EDGE ( 'NONE', *, *, #39158, .F. ) ;
#7687 = AXIS2_PLACEMENT_3D ( 'NONE', #32427, #6747, #39571 ) ;
#7688 = LINE ( 'NONE', #22076, #15629 ) ;
#7689 = SHAPE_REPRESENTATION_RELATIONSHIP ( 'NONE' , 'NONE' ,  #11151, #38737 ) ;
#7690 = CARTESIAN_POINT ( 'NONE',  ( 0.9500414927467378812, -0.1787899950787401604, 1.786417322780882388 ) ) ;
#7691 = CARTESIAN_POINT ( 'NONE',  ( 0.07444174185955065859, -0.1855753056460376360, 0.1797182628040039087 ) ) ;
#7692 = CARTESIAN_POINT ( 'NONE',  ( 0.1899652659299175261, 0.1858176586719255396, -0.3092881115733999708 ) ) ;
#7693 = PRODUCT_DEFINITION_SHAPE ( 'NONE', 'NONE',  #47464 ) ;
#7694 = AXIS2_PLACEMENT_3D ( 'NONE', #31721, #9673, #17552 ) ;
#7695 = CARTESIAN_POINT ( 'NONE',  ( -0.1787899950787401604, -0.1259842519147404416, -0.07405724077823318263 ) ) ;
#7696 = CARTESIAN_POINT ( 'NONE',  ( 0.2471914725378836220, -0.08966515697934822338, -0.05042473337714371839 ) ) ;
#7697 = CARTESIAN_POINT ( 'NONE',  ( 1.054774247047244540, 0.07405724077823318263, 0.7726377952218265177 ) ) ;
#7699 = CARTESIAN_POINT ( 'NONE',  ( 0.7185039370078746268, -0.06523048226347956391, 1.124507873908221267 ) ) ;
#7698 = CARTESIAN_POINT ( 'NONE',  ( -1.028254228867618192, 0.05473827914784732546, 0.03937007874015843040 ) ) ;
#7701 = CARTESIAN_POINT ( 'NONE',  ( 0.3000685424736224127, -0.09842519685039370636, 0.000000000000000000 ) ) ;
#7700 = CARTESIAN_POINT ( 'NONE',  ( 0.1377952755905511861, -1.365923996832131609E-16, 0.8070866141732283561 ) ) ;
#7702 = CARTESIAN_POINT ( 'NONE',  ( 0.7185039370078746268, -0.06523048226347956391, 1.685531496062991019 ) ) ;
#7703 = CARTESIAN_POINT ( 'NONE',  ( 0.7495606340400177148, -0.1264236179284866091, 1.823326771599779406 ) ) ;
#7704 = VERTEX_POINT ( 'NONE', #19473 ) ;
#7705 = CARTESIAN_POINT ( 'NONE',  ( 1.033464566929134687, -0.06523048226347956391, 0.1254921259842518844 ) ) ;
#7706 = CARTESIAN_POINT ( 'NONE',  ( 0.1574803149606299746, 0.000000000000000000, 0.000000000000000000 ) ) ;
#7707 = CARTESIAN_POINT ( 'NONE',  ( -0.1787899950787401882, -0.2416338582139531399, 0.000000000000000000 ) ) ;
#7708 = DIRECTION ( 'NONE',  ( 1.822029033848725028E-16, 0.000000000000000000, 1.000000000000000000 ) ) ;
#7709 = EDGE_CURVE ( 'NONE', #32411, #22975, #6522, .T. ) ;
#7710 = CARTESIAN_POINT ( 'NONE',  ( 3.284318927891251994E-17, -1.132381889710015743, 0.1787899950787401882 ) ) ;
#7711 = CARTESIAN_POINT ( 'NONE',  ( 1.054774247047244540, 0.07405724077823318263, 0.3051181101824569919 ) ) ;
#7712 = CARTESIAN_POINT ( 'NONE',  ( 0.1476377952755906220, 1.571700394971587755, -2.465016072061059660 ) ) ;
#7713 = CARTESIAN_POINT ( 'NONE',  ( -1.002407869896990045, -0.1264236179284866091, 1.631397637741511808 ) ) ;
#7714 = ORIENTED_EDGE ( 'NONE', *, *, #4187, .T. ) ;
#7715 = CARTESIAN_POINT ( 'NONE',  ( -0.8759842519685039353, -0.1787899950787401882, 1.119586614119464585 ) ) ;
#7716 = CARTESIAN_POINT ( 'NONE',  ( 0.8759842519685039353, -0.1574803149606299191, 1.023622047244094446 ) ) ;
#7717 = CARTESIAN_POINT ( 'NONE',  ( 1.054774247047244096, 0.000000000000000000, 1.286909448765133801 ) ) ;
#7718 = CARTESIAN_POINT ( 'NONE',  ( 0.6971942568897648851, 0.07405724077823318263, 1.929133858213952335 ) ) ;
#7719 = CARTESIAN_POINT ( 'NONE',  ( -0.8759842519685039353, 0.1787899950787401882, 1.055610236166708793 ) ) ;
#7720 = CARTESIAN_POINT ( 'NONE',  ( 0.1571385178022536022, 0.1334669528786600612, -0.04962495032650500459 ) ) ;
#7721 = CARTESIAN_POINT ( 'NONE',  ( -0.05572156214699382215, -0.2633233733571747059, -0.05578523004296883497 ) ) ;
#7722 = CARTESIAN_POINT ( 'NONE',  ( 1.002407869896990045, 0.1264236179284866091, 0.3863188975840318173 ) ) ;
#7723 = CARTESIAN_POINT ( 'NONE',  ( -0.7495606340400177148, -0.1264236179284866091, 0.2042322834108035723 ) ) ;
#7724 = UNCERTAINTY_MEASURE_WITH_UNIT (LENGTH_MEASURE( 1.000000000000000082E-05 ), #39041, 'distance_accuracy_value', 'NONE') ;
#7725 = CARTESIAN_POINT ( 'NONE',  ( -0.8759842519685039353, 0.1787899950787401882, 0.7406496062454487328 ) ) ;
#7726 = EDGE_LOOP ( 'NONE', ( #8432, #10992, #38886, #15283 ) ) ;
#7727 = AXIS2_PLACEMENT_3D ( 'NONE', #42526, #38723, #20732 ) ;
#7728 = CARTESIAN_POINT ( 'NONE',  ( -0.7185039370078746268, 0.06523048226347956391, 0.8833661416247559073 ) ) ;
#7729 = ORIENTED_EDGE ( 'NONE', *, *, #27158, .T. ) ;
#7730 = CARTESIAN_POINT ( 'NONE',  ( 0.8019270111902717657, -0.1787899950787401604, 0.9202755904974182499 ) ) ;
#7731 = CARTESIAN_POINT ( 'NONE',  ( -0.8019270111902716547, -0.1787899950787401604, 1.899606299158834943 ) ) ;
#7732 = ORIENTED_EDGE ( 'NONE', *, *, #36038, .T. ) ;
#7733 = STYLED_ITEM ( 'NONE', ( #47336 ), #20411 ) ;
#7734 = EDGE_CURVE ( 'NONE', #18573, #28525, #11734, .T. ) ;
#7735 = AXIS2_PLACEMENT_3D ( 'NONE', #5049, #12259, #15147 ) ;
#7736 = EDGE_CURVE ( 'NONE', #31278, #26592, #22919, .T. ) ;
#7737 = FACE_OUTER_BOUND ( 'NONE', #25691, .T. ) ;
#7738 = CARTESIAN_POINT ( 'NONE',  ( 0.1264236179284866091, -1.448450739882781502, -0.1264236179284866091 ) ) ;
#7739 = ORIENTED_EDGE ( 'NONE', *, *, #38350, .T. ) ;
#7740 = CONICAL_SURFACE ( 'NONE', #9257, 0.1574803149606299191, 0.9599310885968735940 ) ;
#7741 = DIRECTION ( 'NONE',  ( 1.000000000000000000, 0.000000000000000000, -1.822029033848725275E-16 ) ) ;
#7742 = CARTESIAN_POINT ( 'NONE',  ( 0.07405724077823318263, -0.3425196849856064762, 0.1787899950787401604 ) ) ;
#7743 = DIRECTION ( 'NONE',  ( 1.000000000000000000, 0.000000000000000000, 0.000000000000000000 ) ) ;
#7744 = VERTEX_POINT ( 'NONE', #37865 ) ;
#7745 = CARTESIAN_POINT ( 'NONE',  ( 1.054774247047244540, -0.07405724077823318263, 1.161417322780881278 ) ) ;
#7746 = EDGE_CURVE ( 'NONE', #19657, #4309, #1943, .T. ) ;
#7747 = DIRECTION ( 'NONE',  ( 0.000000000000000000, 0.000000000000000000, 1.000000000000000000 ) ) ;
#7748 = LINE ( 'NONE', #25528, #44482 ) ;
#7749 = CARTESIAN_POINT ( 'NONE',  ( 0.8019270111902717657, -0.1787899950787401604, 0.1673228345919057225 ) ) ;
#7750 = CARTESIAN_POINT ( 'NONE',  ( 0.1787899950787401604, -1.676181102308441639, -0.07405724077823318263 ) ) ;
#7751 = CARTESIAN_POINT ( 'NONE',  ( -1.094772975963752103E-17, -1.703248031442299304, -0.1787899950787401882 ) ) ;
#7752 = SHAPE_DEFINITION_REPRESENTATION ( #12849, #45408 ) ;
#7753 = CARTESIAN_POINT ( 'NONE',  ( -1.054774247047244096, 0.000000000000000000, 0.5388779527021417826 ) ) ;
#7754 = CARTESIAN_POINT ( 'NONE',  ( 0.9873396505805591694, 0.1113553986120547346, 0.3690944881889763884 ) ) ;
#7756 = CARTESIAN_POINT ( 'NONE',  ( -0.7106060021345387279, -0.02103896280498998572, 1.983649324475407427 ) ) ;
#7755 = CARTESIAN_POINT ( 'NONE',  ( -0.1270800023317771588, -1.383902077299580702, -0.1270800023317771588 ) ) ;
#7757 = CARTESIAN_POINT ( 'NONE',  ( 0.5358894627757212481, 4.766607801171850497E-17, 0.000000000000000000 ) ) ;
#7758 = CARTESIAN_POINT ( 'NONE',  ( 1.002407869896990045, -0.1264236179284866091, 1.321358267662771757 ) ) ;
#7759 = CARTESIAN_POINT ( 'NONE',  ( 1.002407869896990045, -0.1264236179284866091, 1.631397637741511808 ) ) ;
#7760 = AXIS2_PLACEMENT_3D ( 'NONE', #42762, #35155, #1587 ) ;
#7761 = CARTESIAN_POINT ( 'NONE',  ( -0.7185039370078739607, 1.928577636452523993E-17, 1.013779527559055094 ) ) ;
#7762 = CARTESIAN_POINT ( 'NONE',  ( -0.9873396505805591694, 0.1113553986120547346, 1.510826771653543288 ) ) ;
#7763 = AXIS2_PLACEMENT_3D ( 'NONE', #37474, #25987, #553 ) ;
#7764 = CYLINDRICAL_SURFACE ( 'NONE', #24401, 0.1574803149606299191 ) ;
#7765 = CARTESIAN_POINT ( 'NONE',  ( -0.8759842519685039353, -0.1574803149606299191, 1.929133858267716661 ) ) ;
#7766 = DIRECTION ( 'NONE',  ( 0.000000000000000000, 1.000000000000000000, 0.000000000000000000 ) ) ;
#7767 = CARTESIAN_POINT ( 'NONE',  ( 1.002407869896990045, 0.1264236179284866091, 0.3420275590013546751 ) ) ;
#7768 = ADVANCED_FACE ( 'NONE', ( #41413, #230 ), #7904, .T. ) ;
#7769 = SHAPE_REPRESENTATION ( 'U-Bolt', ( #20860 ), #15520 ) ;
#7770 = CARTESIAN_POINT ( 'NONE',  ( 0.4620708661417344820, 0.6102362204724408601, 0.5854071585544579071 ) ) ;
#7771 = DIRECTION ( 'NONE',  ( -1.000000000000000000, -0.000000000000000000, -0.000000000000000000 ) ) ;
#7772 = CARTESIAN_POINT ( 'NONE',  ( 0.9873396505805591694, -0.1113553986120547346, 0.6643700786326299790 ) ) ;
#7773 = ORIENTED_EDGE ( 'NONE', *, *, #43106, .T. ) ;
#7774 = LINE ( 'NONE', #22152, #32248 ) ;
#7775 = CARTESIAN_POINT ( 'NONE',  ( -0.1720110121816429416, -0.4314947915448568705, -0.9748904863234528761 ) ) ;
#7776 = VERTEX_POINT ( 'NONE', #44312 ) ;
#7777 = CARTESIAN_POINT ( 'NONE',  ( -0.1797182628040039365, -0.04039814029170692850, 0.000000000000000000 ) ) ;
#7778 = CARTESIAN_POINT ( 'NONE',  ( -0.1574803149606300301, -1.043799212490898132, -0.06523048226347956391 ) ) ;
#7779 = VERTEX_POINT ( 'NONE', #11996 ) ;
#7780 = CARTESIAN_POINT ( 'NONE',  ( -0.7646288533564489232, 0.1113553986120547346, 1.599409448818897683 ) ) ;
#7781 = CARTESIAN_POINT ( 'NONE',  ( 1.054774247047244540, -0.07405724077823318263, 1.633858267662771313 ) ) ;
#7783 = CARTESIAN_POINT ( 'NONE',  ( 0.9873396505805591694, 0.1113553986120547346, 1.668307086614173373 ) ) ;
#7782 = CARTESIAN_POINT ( 'NONE',  ( -0.7185039370078741827, 0.06523048226347841205, 0.9325787401574796576 ) ) ;
#7784 = DIRECTION ( 'NONE',  ( 0.000000000000000000, 0.000000000000000000, -1.000000000000000000 ) ) ;
#7785 = CARTESIAN_POINT ( 'NONE',  ( -0.1787899950787401604, -0.1948818897100161873, 0.07405724077823318263 ) ) ;
#7786 = ORIENTED_EDGE ( 'NONE', *, *, #23827, .F. ) ;
#7787 = CARTESIAN_POINT ( 'NONE',  ( 0.5962569168439626477, -0.09842519685039370636, 1.205361022782828805E-17 ) ) ;
#7788 = CARTESIAN_POINT ( 'NONE',  ( -0.01929052294527481767, -0.05062618494071657177, 0.2742915362215331831 ) ) ;
#7789 = ADVANCED_FACE ( 'NONE', ( #25895 ), #4772, .T. ) ;
#7790 = CARTESIAN_POINT ( 'NONE',  ( 0.8759842519685039353, -0.1787899950787401882, 0.8046259841982047467 ) ) ;
#7791 = CARTESIAN_POINT ( 'NONE',  ( -0.8759842519685039353, 0.1787899950787401882, 1.488681102308440751 ) ) ;
#7792 = CARTESIAN_POINT ( 'NONE',  ( -1.094772975963752103E-17, -1.786909448765134023, -0.1787899950787401882 ) ) ;
#7793 = CARTESIAN_POINT ( 'NONE',  ( -0.6971942568897648851, 0.07405724077823318263, 1.304133858213953667 ) ) ;
#7794 = ORIENTED_EDGE ( 'NONE', *, *, #41040, .T. ) ;
#7795 = VECTOR ( 'NONE', #5098, 39.37007874015748143 ) ;
#7796 = TOROIDAL_SURFACE ( 'NONE', #18505, 0.7874015748031495399, 0.04921259842519685318 ) ;
#7797 = EDGE_CURVE ( 'NONE', #28803, #31115, #8610, .T. ) ;
#7798 = LINE ( 'NONE', #18816, #17656 ) ;
#7799 = CARTESIAN_POINT ( 'NONE',  ( -0.6971942568897626646, 0.07405724077823318263, 0.3198818897100162983 ) ) ;
#7800 = CARTESIAN_POINT ( 'NONE',  ( 0.2362204724409448509, 0.1574803149606299191, 0.9891732283464566011 ) ) ;
#7801 = CARTESIAN_POINT ( 'NONE',  ( 0.000000000000000000, 0.0004086818895575684884, 0.000000000000000000 ) ) ;
#7802 = CARTESIAN_POINT ( 'NONE',  ( 0.1264236179284866091, -1.054749952481206732, -0.1264236179284866091 ) ) ;
#7803 = ORIENTED_EDGE ( 'NONE', *, *, #36431, .F. ) ;
#7804 = CARTESIAN_POINT ( 'NONE',  ( 0.1787899950787401604, 0.1397637795813224670, -0.07405724077823318263 ) ) ;
#7805 = ORIENTED_EDGE ( 'NONE', *, *, #35245, .T. ) ;
#7806 = ORIENTED_EDGE ( 'NONE', *, *, #13961, .F. ) ;
#7807 = CIRCLE ( 'NONE', #8553, 0.09842519685039370636 ) ;
#7808 = EDGE_CURVE ( 'NONE', #3412, #38506, #1176, .T. ) ;
#7809 = PRODUCT_DEFINITION ( 'UNKNOWN', '', #30151, #29373 ) ;
#7810 = CARTESIAN_POINT ( 'NONE',  ( -0.8759842519685039353, 0.1787899950787401882, 1.847933070812378009 ) ) ;
#7811 = CARTESIAN_POINT ( 'NONE',  ( -1.094772975963752103E-17, -0.5270669290800944484, -0.1787899950787401882 ) ) ;
#7812 = CARTESIAN_POINT ( 'NONE',  ( -0.8070866141732283561, 0.000000000000000000, 0.6580708661417323802 ) ) ;
#7813 = CARTESIAN_POINT ( 'NONE',  ( -0.9412147342319837628, 0.1574803149606300301, 0.9227362204724416372 ) ) ;
#7814 = DIRECTION ( 'NONE',  ( 0.000000000000000000, 0.000000000000000000, 1.000000000000000000 ) ) ;
#7815 = CARTESIAN_POINT ( 'NONE',  ( -0.07444174185955065859, -1.056638297772022339, 0.1797182628040039087 ) ) ;
#7816 = CARTESIAN_POINT ( 'NONE',  ( 0.02178664995600260515, -0.2829157040455655414, -0.2993662881637836892 ) ) ;
#7817 = CARTESIAN_POINT ( 'NONE',  ( -0.9412147342319837628, -0.1574803149606297803, 1.528051180994836056 ) ) ;
#7818 = CARTESIAN_POINT ( 'NONE',  ( 0.9500414927467378812, 0.1787899950787401604, 0.9793307086076531442 ) ) ;
#7819 = CARTESIAN_POINT ( 'NONE',  ( 0.08946752424252854552, 0.3740157480314960647, 1.224299699984021661 ) ) ;
#7820 = VECTOR ( 'NONE', #39574, 39.37007874015748143 ) ;
#7821 = CARTESIAN_POINT ( 'NONE',  ( 0.9873396505805591694, -0.1113553986120547346, 1.422244094488188892 ) ) ;
#7823 = CARTESIAN_POINT ( 'NONE',  ( 0.7185039370078739607, 1.928577636452523993E-17, 1.594488188868850242 ) ) ;
#7822 = CARTESIAN_POINT ( 'NONE',  ( 0.7356779250440615980, 0.08313417247115993669, 1.981581519332723751 ) ) ;
#7824 = CARTESIAN_POINT ( 'NONE',  ( 0.1574803149606299191, 0.000000000000000000, 0.000000000000000000 ) ) ;
#7825 = AXIS2_PLACEMENT_3D ( 'NONE', #9558, #35200, #46900 ) ;
#7827 = CARTESIAN_POINT ( 'NONE',  ( 0.1554371429169571495, 0.1330479920330144283, 0.04514466913490206706 ) ) ;
#7826 = CARTESIAN_POINT ( 'NONE',  ( 1.054774247047244540, 0.07405724077823318263, 0.7726377952218266287 ) ) ;
#7828 = ADVANCED_BREP_SHAPE_REPRESENTATION ( 'Handle Arm Left', ( #36032, #20860 ), #187 ) ;
#7829 = CARTESIAN_POINT ( 'NONE',  ( 0.07405724077823318263, -0.8001968503399367050, -0.1787899950787401604 ) ) ;
#7830 = ORIENTED_EDGE ( 'NONE', *, *, #45870, .F. ) ;
#7831 = CARTESIAN_POINT ( 'NONE',  ( 0.9873396505805591694, 0.1113553986120547346, 0.9202755905511811330 ) ) ;
#7832 = VECTOR ( 'NONE', #37334, 39.37007874015748143 ) ;
#7834 = FACE_OUTER_BOUND ( 'NONE', #4531, .T. ) ;
#7833 = AXIS2_PLACEMENT_3D ( 'NONE', #45772, #34091, #34320 ) ;
#7835 = CARTESIAN_POINT ( 'NONE',  ( 0.6971942568897648851, -0.07405724077823297447, 1.107283464513165949 ) ) ;
#7836 = ADVANCED_FACE ( 'NONE', ( #11760 ), #19156, .T. ) ;
#7837 = CARTESIAN_POINT ( 'NONE',  ( 1.928577636452524610E-17, -0.09842519685039370636, -0.1574803149606299191 ) ) ;
#7838 = CARTESIAN_POINT ( 'NONE',  ( 0.1574803149606299191, -1.740157480314960869, -1.928577636452523993E-17 ) ) ;
#7839 = CARTESIAN_POINT ( 'NONE',  ( 1.033464566929133799, 0.000000000000000000, 1.299212598317669221 ) ) ;
#7840 = CARTESIAN_POINT ( 'NONE',  ( -0.1377952755905512694, 1.687505431895960112E-17, -0.3149606299212598381 ) ) ;
#7841 = CARTESIAN_POINT ( 'NONE',  ( 0.1574803149606299746, -5.122214988120488358E-16, -8.878505979408856939E-16 ) ) ;
#7842 = CARTESIAN_POINT ( 'NONE',  ( -0.8019270111902717657, -0.1787899950787401604, 0.2066929133320631329 ) ) ;
#7843 = VECTOR ( 'NONE', #34202, 39.37007874015748143 ) ;
#7844 = EDGE_CURVE ( 'NONE', #34120, #46098, #45511, .T. ) ;
#7845 = CARTESIAN_POINT ( 'NONE',  ( 0.7646288533564489232, 0.1113553986120547346, 0.3395669291338583307 ) ) ;
#7846 = CARTESIAN_POINT ( 'NONE',  ( -0.8759842519685039353, -0.1787899950787401882, 1.626476377898992132 ) ) ;
#7847 = CARTESIAN_POINT ( 'NONE',  ( -0.7495606340400177148, 0.1264236179284866091, 0.8636811023084409733 ) ) ;
#7848 = CARTESIAN_POINT ( 'NONE',  ( -0.8759842519685039353, -0.1787899950787401882, 0.4502952755367874427 ) ) ;
#7849 = DIRECTION ( 'NONE',  ( -1.000000000000000000, 0.000000000000000000, 0.000000000000000000 ) ) ;
#7850 = CARTESIAN_POINT ( 'NONE',  ( 0.9412147342319837628, -0.1574803149606297803, 0.9867125984251977622 ) ) ;
#7851 = CARTESIAN_POINT ( 'NONE',  ( 0.6971942568897637749, 2.189545951927499583E-17, 0.08120078734781142893 ) ) ;
#7852 = DIRECTION ( 'NONE',  ( 0.000000000000000000, -0.7880107536067200158, 0.6156614753256607342 ) ) ;
#7853 = CARTESIAN_POINT ( 'NONE',  ( -0.07405724077823318263, -0.4174468028749078186, -0.1787899950787401604 ) ) ;
#7854 = CARTESIAN_POINT ( 'NONE',  ( -0.08928429026229449395, -0.08955962610386575262, -0.2342853990049039437 ) ) ;
#7855 = CARTESIAN_POINT ( 'NONE',  ( -1.181162989532618060E-16, 0.000000000000000000, -0.3937007874015748254 ) ) ;
#7856 = CARTESIAN_POINT ( 'NONE',  ( 0.000000000000000000, -0.09842519685039370636, 0.000000000000000000 ) ) ;
#7857 = VECTOR ( 'NONE', #37893, 39.37007874015748143 ) ;
#7858 = CARTESIAN_POINT ( 'NONE',  ( 0.2559039420239669349, -0.09551646024251110589, -0.06431648083822334716 ) ) ;
#7859 = CARTESIAN_POINT ( 'NONE',  ( -1.054774247047244540, 0.07405724077823318263, 0.3001968503399373711 ) ) ;
#7860 = ORIENTED_EDGE ( 'NONE', *, *, #33079, .T. ) ;
#7861 = ORIENTED_EDGE ( 'NONE', *, *, #34177, .F. ) ;
#7862 = CARTESIAN_POINT ( 'NONE',  ( -0.6971942568897648851, 0.07405724077823318263, 1.422244094434425898 ) ) ;
#7863 = VERTEX_POINT ( 'NONE', #26381 ) ;
#7864 = AXIS2_PLACEMENT_3D ( 'NONE', #31844, #38071, #42363 ) ;
#7865 = CARTESIAN_POINT ( 'NONE',  ( 0.07405724077823318263, -1.356299212544662014, -0.1787899950787401604 ) ) ;
#7866 = CARTESIAN_POINT ( 'NONE',  ( -0.1264236179284866091, -1.501476377898992354, -0.1264236179284866091 ) ) ;
#7867 = SURFACE_STYLE_FILL_AREA ( #22017 ) ;
#7868 = CARTESIAN_POINT ( 'NONE',  ( 0.000000000000000000, 0.000000000000000000, 0.000000000000000000 ) ) ;
#7869 = CARTESIAN_POINT ( 'NONE',  ( 1.033464566929134687, -0.06523048226347956391, 0.3223425196850393526 ) ) ;
#7870 = DIRECTION ( 'NONE',  ( -0.000000000000000000, 1.000000000000000000, -0.000000000000000000 ) ) ;
#7871 = CARTESIAN_POINT ( 'NONE',  ( -0.8759842519685039353, 0.1574803149606299191, 1.112204724301921299 ) ) ;
#7872 = PRESENTATION_LAYER_ASSIGNMENT (  '', '', ( #23184 ) ) ;
#7873 = CARTESIAN_POINT ( 'NONE',  ( 0.8759842519685039353, 0.1787899950787401882, 0.4699803149068661479 ) ) ;
#7874 = DIRECTION ( 'NONE',  ( 1.000000000000000000, -0.000000000000000000, -0.000000000000000000 ) ) ;
#7875 = CARTESIAN_POINT ( 'NONE',  ( 2.892866454678787531E-17, -0.2933070866141732624, 0.1574803149606299191 ) ) ;
#7876 = CARTESIAN_POINT ( 'NONE',  ( 0.000000000000000000, 0.000000000000000000, -0.02633646578327370619 ) ) ;
#7877 = ORIENTED_EDGE ( 'NONE', *, *, #11017, .F. ) ;
#7878 = CARTESIAN_POINT ( 'NONE',  ( -0.6971942568897648851, 0.07405724077823318263, 0.9498031495525356416 ) ) ;
#7879 = CARTESIAN_POINT ( 'NONE',  ( 0.7185039370078746268, -0.06523048226347956391, 0.9768700787401572994 ) ) ;
#7880 = DIRECTION ( 'NONE',  ( -0.000000000000000000, 1.000000000000000000, 0.000000000000000000 ) ) ;
#7881 = CARTESIAN_POINT ( 'NONE',  ( -0.7185039370078739607, 1.928577636452523993E-17, 0.8169291338582678197 ) ) ;
#7882 = CARTESIAN_POINT ( 'NONE',  ( 0.7185039370078739607, 1.928577636452523993E-17, 1.712598425089322918 ) ) ;
#7883 = CARTESIAN_POINT ( 'NONE',  ( 0.1555210144364655711, 0.02856957593376195301, -0.1377952755905573479 ) ) ;
#7884 = CARTESIAN_POINT ( 'NONE',  ( -0.2645270498714851759, 0.1617305326345081506, 0.9203172363904412734 ) ) ;
#7885 = CARTESIAN_POINT ( 'NONE',  ( 1.002407869896990045, 0.1264236179284866091, 0.7357283464029290565 ) ) ;
#7886 = EDGE_CURVE ( 'NONE', #40994, #426, #33577, .T. ) ;
#7887 = ORIENTED_EDGE ( 'NONE', *, *, #30299, .F. ) ;
#7888 = LINE ( 'NONE', #19386, #14960 ) ;
#7889 = CARTESIAN_POINT ( 'NONE',  ( 1.033464566929134687, 0.06523048226347956391, 1.144192913278300194 ) ) ;
#7890 = CARTESIAN_POINT ( 'NONE',  ( -0.1787899950787401604, -1.494094488135213394, 0.07405724077823318263 ) ) ;
#7891 = CARTESIAN_POINT ( 'NONE',  ( 0.1264236179284866091, -0.6894685038832439883, -0.1264236179284866091 ) ) ;
#7892 = CARTESIAN_POINT ( 'NONE',  ( 0.1574803149606300301, -1.270177165354331006, 0.06523048226347956391 ) ) ;
#7893 = CARTESIAN_POINT ( 'NONE',  ( 0.8107537697050253289, -0.1574803149606297803, 1.168799212490898354 ) ) ;
#7894 = EDGE_CURVE ( 'NONE', #39, #44444, #7258, .T. ) ;
#7895 = FACE_BOUND ( 'NONE', #14239, .T. ) ;
#7896 = CIRCLE ( 'NONE', #30780, 0.1574803149606300579 ) ;
#7897 = CARTESIAN_POINT ( 'NONE',  ( -0.7495606340400177148, -0.1264236179284866091, 0.4798228345919055560 ) ) ;
#7898 = VERTEX_POINT ( 'NONE', #15118 ) ;
#7899 = VERTEX_POINT ( 'NONE', #11514 ) ;
#7900 = EDGE_LOOP ( 'NONE', ( #23747, #42863, #46854, #25233 ) ) ;
#7901 = EDGE_CURVE ( 'NONE', #15275, #1242, #11102, .T. ) ;
#7902 = CARTESIAN_POINT ( 'NONE',  ( 0.8019270111902717657, 0.1787899950787401604, 1.732283464513166615 ) ) ;
#7903 = CARTESIAN_POINT ( 'NONE',  ( -0.8019270111902717657, -0.1787899950787401604, 0.8415354330171019859 ) ) ;
#7904 = PLANE ( 'NONE',  #40908 ) ;
#7905 = CARTESIAN_POINT ( 'NONE',  ( 0.6971942568897637749, 2.189545951927499583E-17, 0.2829724408911185041 ) ) ;
#7906 = EDGE_CURVE ( 'NONE', #19295, #24379, #37365, .T. ) ;
#7907 = CARTESIAN_POINT ( 'NONE',  ( -0.6971942568897648851, -0.07405724077823297447, 1.304133858213953667 ) ) ;
#7908 = CARTESIAN_POINT ( 'NONE',  ( -0.9500414927467377701, 0.1787899950787401604, 0.7775590550643457499 ) ) ;
#7909 = CARTESIAN_POINT ( 'NONE',  ( -1.002407869896990045, 0.1264236179284866091, 0.9325787401037164415 ) ) ;
#7910 = CARTESIAN_POINT ( 'NONE',  ( 0.8759842519685039353, 0.1574803149606299191, 0.9153543306011338032 ) ) ;
#7911 = CARTESIAN_POINT ( 'NONE',  ( -0.7185039370078692977, 0.06523048226347515077, 1.670767716427905780 ) ) ;
#7912 = CARTESIAN_POINT ( 'NONE',  ( -0.8759842519685039353, 0.1787899950787401882, 1.651082677111590513 ) ) ;
#7913 = CARTESIAN_POINT ( 'NONE',  ( -0.7185039370078746268, 0.06523048226347956391, 1.906988188868851797 ) ) ;
#7914 = ORIENTED_EDGE ( 'NONE', *, *, #38750, .F. ) ;
#7915 = DIRECTION ( 'NONE',  ( 1.000000000000000000, -5.859809909139239229E-15, 3.662381193212024616E-15 ) ) ;
#7916 = CARTESIAN_POINT ( 'NONE',  ( -0.9873396505805591694, -0.1113553986120547346, 1.619094488188976388 ) ) ;
#7917 = CARTESIAN_POINT ( 'NONE',  ( 0.1700368126712054895, -0.4340694319687135039, -0.9728789567668699734 ) ) ;
#7918 = CARTESIAN_POINT ( 'NONE',  ( -0.2395411720923122101, -0.09842519685039370636, 0.02158160309225409801 ) ) ;
#7919 = CARTESIAN_POINT ( 'NONE',  ( 0.8759842519685039353, -0.1574803149606299191, 1.013779527451527551 ) ) ;
#7920 = VERTEX_POINT ( 'NONE', #34756 ) ;
#7921 = ( BOUNDED_CURVE ( )  B_SPLINE_CURVE ( 2, ( #41386, #34734, #27076, #8588, #23225, #41624, #37839, #38302, #31139 ),
 .UNSPECIFIED., .F., .T. ) 
 B_SPLINE_CURVE_WITH_KNOTS ( ( 3, 2, 2, 2, 3 ),
 ( 0.3400000000000000244, 0.3425000000000000266, 0.3449999999999999734, 0.3474999999999999756, 0.3499999999999999778 ),
 .UNSPECIFIED. ) 
 CURVE ( )  GEOMETRIC_REPRESENTATION_ITEM ( )  RATIONAL_B_SPLINE_CURVE ( ( 1.000000000000000000, 0.9238795325112869605, 1.000000000000000000, 0.9238795325112869605, 1.000000000000000000, 0.9238795325112869605, 1.000000000000000000, 0.9238795325112849621, 1.000000000000000000 ) ) 
 REPRESENTATION_ITEM ( '' )  ) ;
#7922 = ORIENTED_EDGE ( 'NONE', *, *, #14949, .F. ) ;
#7923 = ORIENTED_EDGE ( 'NONE', *, *, #23275, .T. ) ;
#7924 = CARTESIAN_POINT ( 'NONE',  ( -0.1264236179284866091, -0.8764763778989921317, -0.1264236179284866091 ) ) ;
#7925 = CARTESIAN_POINT ( 'NONE',  ( 0.1787899950787401882, -0.4581692912848189247, -2.189545951927503898E-17 ) ) ;
#7926 = CARTESIAN_POINT ( 'NONE',  ( -0.1264236179284866091, -1.029035433017102319, -0.1264236179284866091 ) ) ;
#7927 = DIRECTION ( 'NONE',  ( 1.000000000000000000, 0.000000000000000000, 0.000000000000000000 ) ) ;
#7928 = CARTESIAN_POINT ( 'NONE',  ( 1.054774247047244540, 0.07405724077823318263, 1.756889763725764553 ) ) ;
#7929 = CARTESIAN_POINT ( 'NONE',  ( 0.1270800023317771588, -0.3405949906854078280, 0.1270800023317771588 ) ) ;
#7930 = B_SPLINE_CURVE_WITH_KNOTS ( 'NONE', 3,
 ( #30639, #26566, #30185, #41123, #40339, #44639 ),
 .UNSPECIFIED., .F., .F.,
 ( 4, 2, 4 ),
 ( 0.000000000000000000, 0.0001956124598869668702, 0.0003912249197739337404 ),
 .UNSPECIFIED. ) ;
#7931 = CARTESIAN_POINT ( 'NONE',  ( -0.06523048226347956391, 0.1373031496062993018, 0.1574803149606297803 ) ) ;
#7932 = CARTESIAN_POINT ( 'NONE',  ( 0.1787899950787401882, -0.06446850388324429360, -2.189545951927503898E-17 ) ) ;
#7933 = CARTESIAN_POINT ( 'NONE',  ( 0.8070866141732283561, -0.0009842519685049383633, 0.8559055118110230342 ) ) ;
#7934 = B_SPLINE_CURVE_WITH_KNOTS ( 'NONE', 3,
 ( #26979, #30579, #13068, #42267 ),
 .UNSPECIFIED., .F., .F.,
 ( 4, 4 ),
 ( 0.000000000000000000, 0.0002204554312150490089 ),
 .UNSPECIFIED. ) ;
#7935 = CARTESIAN_POINT ( 'NONE',  ( 0.6971942568897626646, 0.07405724077823318263, 0.8267716534895444003 ) ) ;
#7936 = ( BOUNDED_SURFACE ( )  B_SPLINE_SURFACE ( 1, 2, ( 
 ( #41474, #30765, #4596, #23074, #44609, #34345, #19465, #1476, #27169, #16134, #33417, #15664, #11825, #33887, #531, #37445, #30302, #41721, #8925, #44852, #26213, #34118, #40780, #22596, #10539, #5560, #17705, #6913, #46935, #28279, #32354, #25134, #27411, #24669, #19933, #10296, #21056, #3080, #43338, #39266, #12774, #35697, #6444, #23776, #2833, #3329, #47179, #38390, #17467, #21535, #32590, #14125, #39725, #36172, #14366, #35918, #13639, #29011, #25389, #42842, #17937, #32101, #39501, #24909, #43567, #30991, #20170, #10781, #28766, #45554, #34569, #10054, #1965, #41955, #16367, #9161, #39967, #34823, #1722, #16596, #31878, #28522, #46457, #46691, #6677, #13879, #43093, #21293, #43807, #8094, #44497, #18640, #21782, #19112, #11007, #26089, #4472, #33779, #44267, #26338, #36867, #11241, #14830, #44736, #26574, #7161, #25853, #22236, #33299, #3568, #11716, #36411, #40899, #7859, #11955, #181, #22715, #423, #37323, #646, #22477, #888, #25627, #30194, #47417, #40435, #18183, #32825, #15548, #14592, #40203, #11467, #7398, #15076, #29264, #29953, #15300, #22009, #36632, #4020, #3796, #18414, #7617, #33061, #29495, #29723, #44043, #40664, #37093, #4241, #18874, #33532, #4969, #19596, #41844, #41366, #8566, #45681, #8804, #44969, #4727, #45929, #13141, #9293, #12182, #34455, #12668, #31119, #41129, #12432, #12901, #23199, #37815, #23671, #34237, #1368, #38045, #26807, #8328, #22958, #27535, #27051, #38517, #42086, #16024, #37568, #45448, #30647, #45210, #41601, #5203, #34941, #19350, #23439, #34005, #9050, #38278, #31347, #19827, #1603, #5448, #1134, #16254, #30889, #20063, #23913, #27295, #34706, #1850, #15792, #16487, #5688, #20300, #2088, #16717, #30420, #6625, #35644, #3017, #13580, #13823, #6141, #16950, #9997, #31587, #28712, #17652, #39207, #42337, #39673, #46170, #46638, #25081, #6856, #17410, #46877, #24611, #31818, #35412, #17890, #47120, #27778, #46404, #42782, #6385, #24155, #32300, #9532, #14063, #28466, #32535, #20768, #43284, #20997, #10484, #21239, #43033, #21474, #13367, #3265, #20538, #28219, #38760, #5921, #36111, #35173, #27994, #32048, #42558, #2784, #2316, #9768, #35867, #24378, #38977, #10239, #2551, #17183, #24847, #39446, #29680, #21963, #33249, #25331, #29208, #3974, #40152, #377, #47371, #14542, #29445, #3516, #18128, #36818, #7351, #21730, #10726, #26038, #40612, #15028, #36365, #3746, #14781, #22184, #14313, #36584, #18591, #32774, #43757, #25808, #10959, #25579, #18366, #33008, #28953, #43517, #44219, #131, #39919, #11419, #43996, #7106, #11197, #40381, #7571, #9923, #6545, #3431, #38905, #28146, #2473, #10401, #6779, #47280, #2932, #31741, #43429, #3182, #24303, #28871, #39830, #7022, #2709, #28382, #21397, #6066, #24767, #47037, #29116, #25243, #46329, #6301, #20691, #13740, #42950, #35332, #20924, #13981, #21646, #17099, #17811, #10158, #36279, #13512, #42704, #24530, #31972, #14229, #39130, #36022, #35566, #39600, #32459, #17337, #10638, #46797, #18045, #32689, #39364, #17569, #46556, #14457, #32208, #9690, #21156, #35790, #28631, #43189, #25003, #29597, #33872, #14694, #7484, #40763, #26197, #46, #30053, #14936, #990, #29818, #33631, #29368, #7958, #44595, #22578, #3890, #37192, #745, #3661, #290, #43668, #33399, #44140, #4336, #18968, #11339, #36506, #25951, #40530, #43908, #7719, #26434, #22809, #11109, #22336, #11811, #8185, #15406, #40998, #37422, #4577, #11570, #36731, #19212, #15647, #18515, #10879, #36964, #15174, #515, #25499, #7267, #25730, #40066, #21885, #18284, #32926, #33168, #40301, #22103, #4118, #18741, #44363, #26669, #31209, #34326, #19683, #8659, #35030, #8422, #12530, #44836, #1458, #23295, #2179, #23051, #27150, #12047, #23536, #4823, #16580, #23761, #41219, #1950, #12990, #27631, #37912, #16117, #27393, #37671, #45311, #20156, #30285, #45782, #19446, #26900, #34101, #30740, #41705, #1228, #41461, #34551, #42183, #15881, #38371, #8905, #9390, #30506, #45067, #12282, #5067, #34804, #38138, #41937, #5301, #12762, #9144, #19919, #5545, #1703, #24008, #38609, #16349, #30973, #45540, #5786, #20391, #25182, #46260, #32140, #42132, #5021, #34053, #23251, #27580, #8374, #1178, #34505, #19876, #41173, #23719, #8612, #9343, #23493, #27347, #23003, #1658, #38326, #16304, #45019, #30932, #41890, #44784, #41415, #37366, #27106, #37867, #45493, #12720, #19640, #30234, #34284, #1410, #37615, #16071, #20110, #16535, #4774, #30696, #5498, #1898, #9098, #34758, #31164, #45734, #5255, #30461, #12947, #4521, #12232, #19159, #45260, #8859, #41655, #33821, #938, #19402, #15598, #11998, #26618, #15839, #26856, #12481, #38093, #20349, #31400, #13866, #34988, #39489, #28041, #28754, #6666, #42381, #17229, #42826, #43078, #43321, #42601, #10283, #38800, #5959, #6426, #20579, #24197, #20813, #9579, #23962, #38569, #21282, #9812, #35907, #3062, #35223, #5734, #10040, #2359, #46210, #16992, #35451, #17691, #2132, #31634, #16761, #24658, #21045, #14110, #24421, #39022, #35686, #45972, #31864, #13411, #2823, #32340, #46921, #13185, #27820, #46444, #6189, #2595, #39252, #13625, #47166, #40189, #14349, #11457, #411, #21997, #25122, #22459, #28998, #29483, #7846, #37082, #173, #29709, #36621, #14577, #18171, #630, #29939, #10524, #29251, #25615, #3781, #6899, #15062, #39714, #44255, #11229, #15288, #3557, #26073, #18401, #40645, #4006, #25840, #4230, #43556, #33517, #3311, #43798, #21520, #36157, #18859, #17927, #10768, #14818, #25378, #33048, #32580, #33288, #18627, #39955, #7146, #44025, #21770, #36400, #10997, #32810, #47406, #40422, #7606, #22220, #36853, #16245, #30408, #41832, #8314, #22944, #45198, #11940, #26562, #1591, #12169, #15537, #8080, #16475, #5191, #15779, #23657, #11699, #19098, #41120, #19341, #30876, #33765, #8794, #30180, #23428, #38032, #37552, #19815, #34226, #34443, #9035, #44957, #4954, #4715, #12659, #19581, #27284, #38267, #5432, #44484, #26793, #33992, #41350, #34692, #1119, #8554, #20051, #26327, #23188, #40886, #37801, #22702, #30636, #37308, #1354, #4457, #16011, #9985, #38747, #28206, #35632, #38505, #35161, #31106, #20753, #31576, #13570, #6369, #2305, #23899, #46157, #16933, #34929, #13352, #13809, #10225, #2077, #27982, #17396, #43019, #42769, #20983, #32035, #24831, #46393, #24144, #39435, #35851, #5911, #28450, #42549, #2541, #35398, #2772, #42074, #31332 ),
 ( #9752, #24366, #20526, #21226, #45669, #12887, #38964, #6129, #17168, #27520, #46625, #9277, #6612, #31808, #5676, #24595, #20285, #39195, #16703, #45914, #13129, #42325, #9519, #8434, #4345, #8198, #3251, #15415, #4587, #44603, #25316, #30066, #22821, #25066, #21716, #17638, #7968, #18751, #756, #41007, #36348, #10469, #33409, #3502, #21462, #526, #1002, #44847, #36093, #15183, #19223, #30296, #11819, #37436, #33880, #12056, #33642, #10711, #26680, #23063, #39903, #15656, #29829, #37202, #22589, #41229, #28697, #17876, #37681, #26442, #43267, #32283, #7092, #47108, #39658, #14049, #6841, #46864, #32520, #14296, #44372, #11580, #43501, #28940, #26207, #40772, #18979, #45549, #26912, #38618, #45791, #19456, #24016, #35041, #2187, #45322, #23545, #1957, #34110, #19927, #42195, #24252, #20401, #8671, #1468, #1239, #8916, #38147, #15893, #16126, #9153, #16809, #45078, #12997, #5310, #31448, #30517, #23304, #5075, #27161, #9401, #37921, #16590, #19695, #34814, #31215, #30752, #27641, #41947, #5794, #46032, #34562, #12769, #34336, #13242, #27405, #27869, #42428, #9635, #4834, #1714, #12539, #16361, #12290, #41714, #30982, #23771, #38380, #5553, #20162, #42656, #21343, #3130, #35514, #35972, #28575, #17759, #36230, #10101, #46741, #24482, #32408, #13930, #46983, #3383, #25191, #43622, #6488, #2655, #24713, #29064, #9870, #17286, #14177, #28820, #39075, #39777, #39313, #10829, #24955, #43382, #6247, #10593, #6969, #21592, #46505, #17991, #32645, #46271, #42891, #38850, #43140, #21106, #47230, #14415, #35745, #31691, #2880, #17516, #20872, #32151, #6015, #20636, #31921, #10346, #35282, #2419, #17049, #13465, #28094, #13684, #6726, #28322, #39553, #44778, #7021, #3889, #29115, #36505, #40065, #25729, #39599, #14228, #11108, #45, #6778, #43188, #36278, #43428, #3181, #21396, #36021, #40300, #17810, #36730, #18044, #3430, #39829, #11994, #32458, #43667, #10400, #43907, #21645, #28870, #10637, #25242, #32688, #47279, #10878, #22102, #33167, #25498, #3660, #7266, #18283, #14693, #29367, #30230, #7483, #289, #18514, #15592, #2158, #35250, #42853, #6687, #31424, #46701, #24445, #17717, #5765, #27843, #38822, #13435, #43102, #42404, #35707, #16785, #2385, #10062, #21304, #46001, #13890, #39045, #32367, #20370, #9604, #5985, #28065, #10308, #24226, #2844, #20605, #21070, #17480, #17021, #32114, #28290, #28535, #35932, #6211, #46469, #31658, #24921, #13653, #39513, #3092, #46946, #43347, #20840, #46231, #35479, #28781, #42628, #2619, #14137, #10550, #17252, #38589, #31889, #35010, #24681, #39278, #6452, #22909, #12138, #4679, #33487, #37522, #30378, #33258, #29907, #25148, #15500, #26294, #8283, #1083, #44456, #18596, #40851, #11670, #29683, #8045, #8522, #4923, #44224, #22675, #26762, #37766, #19308, #15744, #41319, #19546, #41085, #18832, #34193, #30599, #603, #23150, #37275, #44684, #30146, #44924, #36826, #26046, #1321, #33962, #3978, #39738, #15260, #7813, #382, #21549, #15034, #15978, #11428, #45163, #4430, #19062, #4203, #6926, #40619, #33730, #22429, #841, #37050, #11902, #26524, #27005, #31538, #42515, #9718, #5392, #31072, #24105, #8758, #27488, #2272, #31771, #27948, #1556, #9000, #23395, #16443, #45636, #20488, #38712, #34898, #35126, #12854, #13092, #38234, #30843, #42039, #45410, #13317, #16896, #23859, #38000, #24331, #12623, #31300, #38930, #20716, #2039, #46119, #9241, #38471, #20015, #2505, #12384, #5159, #5641, #16671, #27725, #19780, #35360, #34413, #17129, #42287, #27246, #34654, #41800, #5882, #23624, #1804, #19384, #23235, #16053, #30680, #45243, #27084, #23477, #34487, #26258, #47089, #39889, #40352, #29178, #11165, #14283, #28923, #43487, #10932, #7074, #32982, #25553, #40124, #105, #25782, #7545, #22156, #36791, #15471, #30349, #41768, #8488, #19984, #33933, #1055, #23365, #22880, #37492, #27217, #37736, #26495, #33698, #27457, #42002, #38202, #41057, #15947, #41523, #12594, #22647, #41288, #8971, #4650, #19276, #5125, #15714, #44897, #19514, #8255, #37251, #4403, #23590, #23123, #34623, #5364, #12110, #19031, #26970, #4892, #34162, #1292, #30573, #16412, #44653, #45134, #11870, #19751, #34386, #12825, #12351, #8729, #1525, #16179, #30810, #45379, #1773, #31039, #45606, #27695, #24302, #42949, #21155, #39129, #31971, #10157, #2931, #24529, #2241, #17568, #28630, #16861, #6544, #2472, #28145, #46328, #13739, #20217, #9457, #46555, #6300, #34865, #9206, #31504, #38684, #31271, #5609, #16641, #17336, #2013, #24766, #13290, #46087, #35094, #23826, #45850, #38904, #38441, #17098, #13057, #32207, #2708, #42257, #28381, #46796, #24075, #6065, #31740, #20923, #5851, #13511, #20460, #42703, #9922, #35565, #21105, #20870, #28573, #21342, #2654, #35744, #10592, #40018, #17285, #43621, #32406, #14033, #46504, #13682, #24711, #13929, #10828, #42890, #21591, #10100, #6968, #36229, #46982, #7213, #39776, #21836, #29315, #43862, #39312, #6487, #22768, #18928, #40953, #23012, #44794, #15847, #26146, #22290, #44323, #1188, #29547, #36925, #37376, #4532, #14886, #26628, #29774, #30470, #44555, #946, #44099, #19169, #41180, #33827, #18693, #15605, #30243, #18467, #15129, #11063, #701, #11526, #37625, #4783, #7916, #3846, #22530, #37148, #11293, #4296, #19409, #34060, #25682, #25905, #22061, #33588, #36686, #33354, #15359, #242, #33118, #30009, #474, #11773, #26391, #16766, #30941, #42386, #8868, #23499, #45744, #45268, #12489, #2140, #12726, #1419, #8622, #2365, #17002, #13191, #16078, #38332, #16544, #34995, #45026, #16313, #31407, #27114, #41662, #27591, #38102, #5265, #41899, #30703, #12241, #26864, #45982, #45502, #9586, #27827, #19884, #41425, #1908, #34513, #1666, #27356, #9108, #38808, #23260, #23728, #37875, #12953, #42140, #35233, #5505, #20118, #9349, #5028, #34765, #31171, #23970, #24205, #5967, #5742, #38573, #20357, #20586, #19650, #34294, #24664, #20820, #13872, #35459, #47173, #21527, #43087, #46216, #43562, #2602, #3070, #29004, #10773, #21288, #3319, #28515, #2828, #39259, #21776, #3563, #31641, #17461, #46684, #10291, #28049, #36165, #13417, #17932, #32348, #36405, #6435, #14356, #24901, #39960, #25129, #46928, #7153, #17235, #9823, #24428, #32095, #39028, #6197, #31871, #46450, #13633, #17700, #28272, #39496, #42836, #6905, #14118, #6670, #28760, #21051, #43330, #10532, #39719, #40428, #40195, #25846, #26332 ) ),
 .UNSPECIFIED., .F., .F., .F. ) 
 B_SPLINE_SURFACE_WITH_KNOTS ( ( 2, 2 ),
 ( 3, 2, 2, 2, 2, 2, 2, 2, 2, 2, 2, 2, 2, 2, 2, 2, 2, 2, 2, 2, 2, 2, 2, 2, 2, 2, 2, 2, 2, 2, 2, 2, 2, 2, 2, 2, 2, 2, 2, 2, 2, 2, 2, 2, 2, 2, 2, 2, 2, 2, 2, 2, 2, 2, 2, 2, 2, 2, 2, 2, 2, 2, 2, 2, 2, 2, 2, 2, 2, 2, 2, 2, 2, 2, 2, 2, 2, 2, 2, 2, 2, 2, 2, 2, 2, 2, 2, 2, 2, 2, 2, 2, 2, 2, 2, 2, 2, 2, 2, 2, 2, 2, 2, 2, 2, 2, 2, 2, 2, 2, 2, 2, 2, 2, 2, 2, 2, 2, 2, 2, 2, 2, 2, 2, 2, 2, 2, 2, 2, 2, 2, 2, 2, 2, 2, 2, 2, 2, 2, 2, 2, 2, 2, 2, 2, 2, 2, 2, 2, 2, 2, 2, 2, 2, 2, 2, 2, 2, 2, 2, 2, 2, 2, 2, 2, 2, 2, 2, 2, 2, 2, 2, 2, 2, 2, 2, 2, 2, 2, 2, 2, 2, 2, 2, 2, 2, 2, 2, 2, 2, 2, 2, 2, 2, 2, 2, 2, 2, 2, 2, 2, 2, 2, 2, 2, 2, 2, 2, 2, 2, 2, 2, 2, 2, 2, 2, 2, 2, 2, 2, 2, 2, 2, 2, 2, 2, 2, 2, 2, 2, 2, 2, 2, 2, 2, 2, 2, 2, 2, 2, 2, 2, 2, 2, 2, 2, 2, 2, 2, 2, 2, 2, 2, 2, 2, 2, 2, 2, 2, 2, 2, 2, 2, 2, 2, 2, 2, 2, 2, 2, 2, 2, 2, 2, 2, 2, 2, 2, 2, 2, 2, 2, 2, 2, 2, 2, 2, 2, 2, 2, 2, 2, 2, 2, 2, 2, 2, 2, 2, 2, 2, 2, 2, 2, 2, 2, 2, 2, 2, 2, 2, 2, 2, 2, 2, 2, 2, 2, 2, 2, 2, 2, 2, 2, 2, 2, 2, 2, 2, 2, 2, 2, 2, 2, 2, 2, 2, 2, 2, 2, 2, 2, 2, 2, 2, 2, 2, 2, 2, 2, 2, 2, 2, 2, 2, 2, 2, 2, 2, 2, 2, 2, 2, 2, 2, 2, 2, 2, 2, 2, 2, 2, 2, 2, 2, 2, 2, 2, 2, 2, 2, 2, 2, 2, 2, 2, 2, 2, 2, 2, 2, 2, 2, 2, 2, 2, 2, 2, 2, 2, 3 ),
 ( 0.000000000000000000, 1.000000000000000000 ),
 ( 0.000000000000000000, 0.002500000000000000052, 0.005000000000000000104, 0.007499999999999999722, 0.01000000000000000021, 0.01250000000000000069, 0.01499999999999999944, 0.01750000000000000167, 0.02000000000000000042, 0.02249999999999999917, 0.02500000000000000139, 0.02750000000000000014, 0.02999999999999999889, 0.03250000000000000111, 0.03500000000000000333, 0.03749999999999999861, 0.04000000000000000083, 0.04250000000000000305, 0.04499999999999999833, 0.04750000000000000056, 0.05000000000000000278, 0.05249999999999999806, 0.05500000000000000028, 0.05750000000000000250, 0.05999999999999999778, 0.06250000000000000000, 0.06500000000000000222, 0.06750000000000000444, 0.07000000000000000666, 0.07249999999999999500, 0.07499999999999999722, 0.07749999999999999944, 0.08000000000000000167, 0.08250000000000000389, 0.08500000000000000611, 0.08749999999999999445, 0.08999999999999999667, 0.09249999999999999889, 0.09500000000000000111, 0.09750000000000000333, 0.1000000000000000056, 0.1024999999999999939, 0.1049999999999999961, 0.1074999999999999983, 0.1100000000000000006, 0.1125000000000000028, 0.1150000000000000050, 0.1174999999999999933, 0.1199999999999999956, 0.1224999999999999978, 0.1250000000000000000, 0.1275000000000000022, 0.1300000000000000044, 0.1325000000000000067, 0.1350000000000000089, 0.1375000000000000111, 0.1400000000000000133, 0.1424999999999999878, 0.1449999999999999900, 0.1474999999999999922, 0.1499999999999999944, 0.1524999999999999967, 0.1549999999999999989, 0.1575000000000000011, 0.1600000000000000033, 0.1625000000000000056, 0.1650000000000000078, 0.1675000000000000100, 0.1700000000000000122, 0.1724999999999999867, 0.1749999999999999889, 0.1774999999999999911, 0.1799999999999999933, 0.1824999999999999956, 0.1849999999999999978, 0.1875000000000000000, 0.1900000000000000022, 0.1925000000000000044, 0.1950000000000000067, 0.1975000000000000089, 0.2000000000000000111, 0.2025000000000000133, 0.2049999999999999878, 0.2074999999999999900, 0.2099999999999999922, 0.2124999999999999944, 0.2149999999999999967, 0.2174999999999999989, 0.2200000000000000011, 0.2225000000000000033, 0.2250000000000000056, 0.2275000000000000078, 0.2300000000000000100, 0.2325000000000000122, 0.2349999999999999867, 0.2374999999999999889, 0.2399999999999999911, 0.2424999999999999933, 0.2449999999999999956, 0.2474999999999999978, 0.2500000000000000000, 0.2525000000000000022, 0.2550000000000000044, 0.2575000000000000067, 0.2600000000000000089, 0.2625000000000000111, 0.2650000000000000133, 0.2675000000000000155, 0.2700000000000000178, 0.2725000000000000200, 0.2750000000000000222, 0.2775000000000000244, 0.2800000000000000266, 0.2824999999999999734, 0.2849999999999999756, 0.2874999999999999778, 0.2899999999999999800, 0.2924999999999999822, 0.2949999999999999845, 0.2974999999999999867, 0.2999999999999999889, 0.3024999999999999911, 0.3049999999999999933, 0.3074999999999999956, 0.3099999999999999978, 0.3125000000000000000, 0.3150000000000000022, 0.3175000000000000044, 0.3200000000000000067, 0.3225000000000000089, 0.3250000000000000111, 0.3275000000000000133, 0.3300000000000000155, 0.3325000000000000178, 0.3350000000000000200, 0.3375000000000000222, 0.3400000000000000244, 0.3425000000000000266, 0.3449999999999999734, 0.3474999999999999756, 0.3499999999999999778, 0.3524999999999999800, 0.3549999999999999822, 0.3574999999999999845, 0.3599999999999999867, 0.3624999999999999889, 0.3649999999999999911, 0.3674999999999999933, 0.3699999999999999956, 0.3724999999999999978, 0.3750000000000000000, 0.3775000000000000022, 0.3800000000000000044, 0.3825000000000000067, 0.3850000000000000089, 0.3875000000000000111, 0.3900000000000000133, 0.3925000000000000155, 0.3950000000000000178, 0.3975000000000000200, 0.4000000000000000222, 0.4025000000000000244, 0.4050000000000000266, 0.4074999999999999734, 0.4099999999999999756, 0.4124999999999999778, 0.4149999999999999800, 0.4174999999999999822, 0.4199999999999999845, 0.4224999999999999867, 0.4249999999999999889, 0.4274999999999999911, 0.4299999999999999933, 0.4324999999999999956, 0.4349999999999999978, 0.4375000000000000000, 0.4400000000000000022, 0.4425000000000000044, 0.4450000000000000067, 0.4475000000000000089, 0.4500000000000000111, 0.4525000000000000133, 0.4550000000000000155, 0.4575000000000000178, 0.4600000000000000200, 0.4625000000000000222, 0.4650000000000000244, 0.4675000000000000266, 0.4699999999999999734, 0.4724999999999999756, 0.4749999999999999778, 0.4774999999999999800, 0.4799999999999999822, 0.4824999999999999845, 0.4849999999999999867, 0.4874999999999999889, 0.4899999999999999911, 0.4924999999999999933, 0.4949999999999999956, 0.4974999999999999978, 0.5000000000000000000, 0.5024999999999999467, 0.5050000000000000044, 0.5074999999999999512, 0.5100000000000000089, 0.5124999999999999556, 0.5150000000000000133, 0.5174999999999999600, 0.5200000000000000178, 0.5224999999999999645, 0.5250000000000000222, 0.5274999999999999689, 0.5300000000000000266, 0.5324999999999999734, 0.5350000000000000311, 0.5374999999999999778, 0.5400000000000000355, 0.5424999999999999822, 0.5450000000000000400, 0.5474999999999999867, 0.5500000000000000444, 0.5524999999999999911, 0.5550000000000000488, 0.5574999999999999956, 0.5600000000000000533, 0.5625000000000000000, 0.5649999999999999467, 0.5675000000000000044, 0.5699999999999999512, 0.5725000000000000089, 0.5749999999999999556, 0.5775000000000000133, 0.5799999999999999600, 0.5825000000000000178, 0.5849999999999999645, 0.5875000000000000222, 0.5899999999999999689, 0.5925000000000000266, 0.5949999999999999734, 0.5975000000000000311, 0.5999999999999999778, 0.6025000000000000355, 0.6049999999999999822, 0.6075000000000000400, 0.6099999999999999867, 0.6125000000000000444, 0.6149999999999999911, 0.6175000000000000488, 0.6199999999999999956, 0.6225000000000000533, 0.6250000000000000000, 0.6274999999999999467, 0.6300000000000000044, 0.6324999999999999512, 0.6350000000000000089, 0.6374999999999999556, 0.6400000000000000133, 0.6424999999999999600, 0.6450000000000000178, 0.6474999999999999645, 0.6500000000000000222, 0.6524999999999999689, 0.6550000000000000266, 0.6574999999999999734, 0.6600000000000000311, 0.6624999999999999778, 0.6650000000000000355, 0.6674999999999999822, 0.6700000000000000400, 0.6724999999999999867, 0.6750000000000000444, 0.6774999999999999911, 0.6800000000000000488, 0.6824999999999999956, 0.6850000000000000533, 0.6875000000000000000, 0.6899999999999999467, 0.6925000000000000044, 0.6949999999999999512, 0.6975000000000000089, 0.6999999999999999556, 0.7025000000000000133, 0.7049999999999999600, 0.7075000000000000178, 0.7099999999999999645, 0.7125000000000000222, 0.7149999999999999689, 0.7175000000000000266, 0.7199999999999999734, 0.7225000000000000311, 0.7249999999999999778, 0.7275000000000000355, 0.7299999999999999822, 0.7325000000000000400, 0.7349999999999999867, 0.7375000000000000444, 0.7399999999999999911, 0.7425000000000000488, 0.7449999999999999956, 0.7475000000000000533, 0.7500000000000000000, 0.7524999999999999467, 0.7550000000000000044, 0.7574999999999999512, 0.7600000000000000089, 0.7624999999999999556, 0.7650000000000000133, 0.7674999999999999600, 0.7700000000000000178, 0.7724999999999999645, 0.7750000000000000222, 0.7774999999999999689, 0.7800000000000000266, 0.7824999999999999734, 0.7850000000000000311, 0.7874999999999999778, 0.7900000000000000355, 0.7924999999999999822, 0.7950000000000000400, 0.7974999999999999867, 0.8000000000000000444, 0.8024999999999999911, 0.8050000000000000488, 0.8074999999999999956, 0.8100000000000000533, 0.8125000000000000000, 0.8149999999999999467, 0.8175000000000000044, 0.8199999999999999512, 0.8225000000000000089, 0.8249999999999999556, 0.8275000000000000133, 0.8299999999999999600, 0.8325000000000000178, 0.8349999999999999645, 0.8375000000000000222, 0.8399999999999999689, 0.8425000000000000266, 0.8449999999999999734, 0.8475000000000000311, 0.8499999999999999778, 0.8525000000000000355, 0.8549999999999999822, 0.8575000000000000400, 0.8599999999999999867, 0.8625000000000000444, 0.8649999999999999911, 0.8675000000000000488, 0.8699999999999999956, 0.8725000000000000533, 0.8750000000000000000, 0.8774999999999999467, 0.8800000000000000044, 0.8824999999999999512, 0.8850000000000000089, 0.8874999999999999556, 0.8900000000000000133, 0.8924999999999999600, 0.8950000000000000178, 0.8974999999999999645, 0.9000000000000000222, 0.9024999999999999689, 0.9050000000000000266, 0.9074999999999999734, 0.9100000000000000311, 0.9124999999999999778, 0.9150000000000000355, 0.9174999999999999822, 0.9200000000000000400, 0.9224999999999999867, 0.9250000000000000444, 0.9274999999999999911, 0.9300000000000000488, 0.9324999999999999956, 0.9350000000000000533, 0.9375000000000000000, 0.9399999999999999467, 0.9425000000000000044, 0.9449999999999999512, 0.9475000000000000089, 0.9499999999999999556, 0.9525000000000000133, 0.9549999999999999600, 0.9575000000000000178, 0.9599999999999999645, 0.9625000000000000222, 0.9649999999999999689, 0.9675000000000000266, 0.9699999999999999734, 0.9725000000000000311, 0.9749999999999999778, 0.9775000000000000355, 0.9799999999999999822, 0.9825000000000000400, 0.9849999999999999867, 0.9875000000000000444, 0.9899999999999999911, 0.9925000000000000488, 0.9949999999999999956, 0.9975000000000000533, 1.000000000000000000 ),
 .UNSPECIFIED. ) 
 GEOMETRIC_REPRESENTATION_ITEM ( )  RATIONAL_B_SPLINE_SURFACE ( (
 ( 1.000000000000000000, 0.9238795325112869605, 1.000000000000000000, 0.9238795325112869605, 1.000000000000000000, 0.9238795325112869605, 1.000000000000000000, 0.9238795325112869605, 1.000000000000000000, 0.9238795325112869605, 1.000000000000000000, 0.9238795325112869605, 1.000000000000000000, 0.9238795325112869605, 1.000000000000000000, 0.9238795325112869605, 1.000000000000000000, 0.9238795325112869605, 1.000000000000000000, 0.9238795325112869605, 1.000000000000000000, 0.9238795325112869605, 1.000000000000000000, 0.9238795325112869605, 1.000000000000000000, 0.9238795325112869605, 1.000000000000000000, 0.9238795325112869605, 1.000000000000000000, 0.9238795325112869605, 1.000000000000000000, 0.9238795325112869605, 1.000000000000000000, 0.9238795325112869605, 1.000000000000000000, 0.9238795325112869605, 1.000000000000000000, 0.9238795325112869605, 1.000000000000000000, 0.9238795325112869605, 1.000000000000000000, 0.9238795325112869605, 1.000000000000000000, 0.9238795325112869605, 1.000000000000000000, 0.9238795325112869605, 1.000000000000000000, 0.9238795325112869605, 1.000000000000000000, 0.9238795325112869605, 1.000000000000000000, 0.9238795325112869605, 1.000000000000000000, 0.9238795325112869605, 1.000000000000000000, 0.9238795325112869605, 1.000000000000000000, 0.9238795325112869605, 1.000000000000000000, 0.9238795325112869605, 1.000000000000000000, 0.9238795325112869605, 1.000000000000000000, 0.9238795325112869605, 1.000000000000000000, 0.9238795325112869605, 1.000000000000000000, 0.9238795325112869605, 1.000000000000000000, 0.9238795325112869605, 1.000000000000000000, 0.9238795325112869605, 1.000000000000000000, 0.9238795325112869605, 1.000000000000000000, 0.9238795325112869605, 1.000000000000000000, 0.9238795325112869605, 1.000000000000000000, 0.9238795325112869605, 1.000000000000000000, 0.9238795325112869605, 1.000000000000000000, 0.9238795325112869605, 1.000000000000000000, 0.9238795325112869605, 1.000000000000000000, 0.9238795325112869605, 1.000000000000000000, 0.9238795325112869605, 1.000000000000000000, 0.9238795325112869605, 1.000000000000000000, 0.9238795325112869605, 1.000000000000000000, 0.9238795325112869605, 1.000000000000000000, 0.9238795325112869605, 1.000000000000000000, 0.9238795325112869605, 1.000000000000000000, 0.9238795325112869605, 1.000000000000000000, 0.9238795325112869605, 1.000000000000000000, 0.9238795325112869605, 1.000000000000000000, 0.9238795325112869605, 1.000000000000000000, 0.9238795325112869605, 1.000000000000000000, 0.9238795325112869605, 1.000000000000000000, 0.9238795325112869605, 1.000000000000000000, 0.9238795325112869605, 1.000000000000000000, 0.9238795325112869605, 1.000000000000000000, 0.9238795325112869605, 1.000000000000000000, 0.9238795325112869605, 1.000000000000000000, 0.9238795325112869605, 1.000000000000000000, 0.9238795325112869605, 1.000000000000000000, 0.9238795325112869605, 1.000000000000000000, 0.9238795325112869605, 1.000000000000000000, 0.9238795325112869605, 1.000000000000000000, 0.9238795325112869605, 1.000000000000000000, 0.9238795325112869605, 1.000000000000000000, 0.9238795325112869605, 1.000000000000000000, 0.9238795325112869605, 1.000000000000000000, 0.9238795325112869605, 1.000000000000000000, 0.9238795325112869605, 1.000000000000000000, 0.9238795325112869605, 1.000000000000000000, 0.9238795325112869605, 1.000000000000000000, 0.9238795325112869605, 1.000000000000000000, 0.9238795325112869605, 1.000000000000000000, 0.9238795325112869605, 1.000000000000000000, 0.9238795325112869605, 1.000000000000000000, 0.9238795325112869605, 1.000000000000000000, 0.9238795325112869605, 1.000000000000000000, 0.9238795325112869605, 1.000000000000000000, 0.9238795325112869605, 1.000000000000000000, 0.9238795325112869605, 1.000000000000000000, 0.9238795325112869605, 1.000000000000000000, 0.9238795325112869605, 1.000000000000000000, 0.9238795325112869605, 1.000000000000000000, 0.9238795325112869605, 1.000000000000000000, 0.9238795325112869605, 1.000000000000000000, 0.9238795325112869605, 1.000000000000000000, 0.9238795325112869605, 1.000000000000000000, 0.9238795325112869605, 1.000000000000000000, 0.9238795325112869605, 1.000000000000000000, 0.9238795325112869605, 1.000000000000000000, 0.9238795325112869605, 1.000000000000000000, 0.9238795325112869605, 1.000000000000000000, 0.9238795325112869605, 1.000000000000000000, 0.9238795325112869605, 1.000000000000000000, 0.9238795325112869605, 1.000000000000000000, 0.9238795325112869605, 1.000000000000000000, 0.9238795325112869605, 1.000000000000000000, 0.9238795325112869605, 1.000000000000000000, 0.9238795325112869605, 1.000000000000000000, 0.9238795325112869605, 1.000000000000000000, 0.9238795325112869605, 1.000000000000000000, 0.9238795325112869605, 1.000000000000000000, 0.9238795325112869605, 1.000000000000000000, 0.9238795325112869605, 1.000000000000000000, 0.9238795325112869605, 1.000000000000000000, 0.9238795325112869605, 1.000000000000000000, 0.9238795325112869605, 1.000000000000000000, 0.9238795325112869605, 1.000000000000000000, 0.9238795325112869605, 1.000000000000000000, 0.9238795325112869605, 1.000000000000000000, 0.9238795325112869605, 1.000000000000000000, 0.9238795325112869605, 1.000000000000000000, 0.9238795325112869605, 1.000000000000000000, 0.9238795325112869605, 1.000000000000000000, 0.9238795325112869605, 1.000000000000000000, 0.9238795325112869605, 1.000000000000000000, 0.9238795325112869605, 1.000000000000000000, 0.9238795325112869605, 1.000000000000000000, 0.9238795325112869605, 1.000000000000000000, 0.9238795325112869605, 1.000000000000000000, 0.9238795325112869605, 1.000000000000000000, 0.9238795325112869605, 1.000000000000000000, 0.9238795325112869605, 1.000000000000000000, 0.9238795325112869605, 1.000000000000000000, 0.9238795325112869605, 1.000000000000000000, 0.9238795325112869605, 1.000000000000000000, 0.9238795325112869605, 1.000000000000000000, 0.9238795325112869605, 1.000000000000000000, 0.9238795325112869605, 1.000000000000000000, 0.9238795325112869605, 1.000000000000000000, 0.9238795325112869605, 1.000000000000000000, 0.9238795325112869605, 1.000000000000000000, 0.9238795325112869605, 1.000000000000000000, 0.9238795325112869605, 1.000000000000000000, 0.9238795325112869605, 1.000000000000000000, 0.9238795325112869605, 1.000000000000000000, 0.9238795325112869605, 1.000000000000000000, 0.9238795325112869605, 1.000000000000000000, 0.9238795325112869605, 1.000000000000000000, 0.9238795325112869605, 1.000000000000000000, 0.9238795325112869605, 1.000000000000000000, 0.9238795325112869605, 1.000000000000000000, 0.9238795325112869605, 1.000000000000000000, 0.9238795325112869605, 1.000000000000000000, 0.9238795325112869605, 1.000000000000000000, 0.9238795325112869605, 1.000000000000000000, 0.9238795325112869605, 1.000000000000000000, 0.9238795325112869605, 1.000000000000000000, 0.9238795325112869605, 1.000000000000000000, 0.9238795325112869605, 1.000000000000000000, 0.9238795325112869605, 1.000000000000000000, 0.9238795325112869605, 1.000000000000000000, 0.9238795325112869605, 1.000000000000000000, 0.9238795325112869605, 1.000000000000000000, 0.9238795325112869605, 1.000000000000000000, 0.9238795325112869605, 1.000000000000000000, 0.9238795325112869605, 1.000000000000000000, 0.9238795325112869605, 1.000000000000000000, 0.9238795325112869605, 1.000000000000000000, 0.9238795325112869605, 1.000000000000000000, 0.9238795325112869605, 1.000000000000000000, 0.9238795325112869605, 1.000000000000000000, 0.9238795325112869605, 1.000000000000000000, 0.9238795325112869605, 1.000000000000000000, 0.9238795325112869605, 1.000000000000000000, 0.9238795325112869605, 1.000000000000000000, 0.9238795325112869605, 1.000000000000000000, 0.9238795325112869605, 1.000000000000000000, 0.9238795325112869605, 1.000000000000000000, 0.9238795325112869605, 1.000000000000000000, 0.9238795325112869605, 1.000000000000000000, 0.9238795325112869605, 1.000000000000000000, 0.9238795325112869605, 1.000000000000000000, 0.9238795325112869605, 1.000000000000000000, 0.9238795325112869605, 1.000000000000000000, 0.9238795325112869605, 1.000000000000000000, 0.9238795325112869605, 1.000000000000000000, 0.9238795325112869605, 1.000000000000000000, 0.9238795325112869605, 1.000000000000000000, 0.9238795325112869605, 1.000000000000000000, 0.9238795325112869605, 1.000000000000000000, 0.9238795325112869605, 1.000000000000000000, 0.9238795325112869605, 1.000000000000000000, 0.9238795325112869605, 1.000000000000000000, 0.9238795325112869605, 1.000000000000000000, 0.9238795325112869605, 1.000000000000000000, 0.9238795325112869605, 1.000000000000000000, 0.9238795325112869605, 1.000000000000000000, 0.9238795325112869605, 1.000000000000000000, 0.9238795325112869605, 1.000000000000000000, 0.9238795325112869605, 1.000000000000000000, 0.9238795325112869605, 1.000000000000000000, 0.9238795325112869605, 1.000000000000000000, 0.9238795325112869605, 1.000000000000000000, 0.9238795325112869605, 1.000000000000000000, 0.9238795325112869605, 1.000000000000000000, 0.9238795325112869605, 1.000000000000000000, 0.9238795325112869605, 1.000000000000000000, 0.9238795325112869605, 1.000000000000000000, 0.9238795325112869605, 1.000000000000000000, 0.9238795325112869605, 1.000000000000000000, 0.9238795325112869605, 1.000000000000000000, 0.9238795325112869605, 1.000000000000000000, 0.9238795325112869605, 1.000000000000000000, 0.9238795325112869605, 1.000000000000000000, 0.9238795325112869605, 1.000000000000000000, 0.9238795325112869605, 1.000000000000000000, 0.9238795325112869605, 1.000000000000000000, 0.9238795325112869605, 1.000000000000000000, 0.9238795325112869605, 1.000000000000000000, 0.9238795325112869605, 1.000000000000000000, 0.9238795325112869605, 1.000000000000000000, 0.9238795325112869605, 1.000000000000000000, 0.9238795325112869605, 1.000000000000000000, 0.9238795325112869605, 1.000000000000000000, 0.9238795325112869605, 1.000000000000000000, 0.9238795325112869605, 1.000000000000000000, 0.9238795325112869605, 1.000000000000000000, 0.9238795325112869605, 1.000000000000000000, 0.9238795325112869605, 1.000000000000000000, 0.9238795325112869605, 1.000000000000000000, 0.9238795325112869605, 1.000000000000000000, 0.9238795325112869605, 1.000000000000000000, 0.9238795325112869605, 1.000000000000000000, 0.9238795325112869605, 1.000000000000000000, 0.9238795325112869605, 1.000000000000000000, 0.9238795325112869605, 1.000000000000000000, 0.9238795325112869605, 1.000000000000000000, 0.9238795325112869605, 1.000000000000000000, 0.9238795325112869605, 1.000000000000000000, 0.9238795325112869605, 1.000000000000000000, 0.9238795325112869605, 1.000000000000000000, 0.9238795325112869605, 1.000000000000000000, 0.9238795325112869605, 1.000000000000000000, 0.9238795325112869605, 1.000000000000000000, 0.9238795325112869605, 1.000000000000000000, 0.9238795325112869605, 1.000000000000000000, 0.9238795325112869605, 1.000000000000000000, 0.9238795325112869605, 1.000000000000000000, 0.9238795325112869605, 1.000000000000000000, 0.9238795325112869605, 1.000000000000000000, 0.9238795325112869605, 1.000000000000000000, 0.9238795325112869605, 1.000000000000000000, 0.9238795325112869605, 1.000000000000000000, 0.9238795325112869605, 1.000000000000000000, 0.9238795325112869605, 1.000000000000000000, 0.9238795325112869605, 1.000000000000000000, 0.9238795325112869605, 1.000000000000000000, 0.9238795325112869605, 1.000000000000000000, 0.9238795325112869605, 1.000000000000000000, 0.9238795325112869605, 1.000000000000000000, 0.9238795325112869605, 1.000000000000000000, 0.9238795325112869605, 1.000000000000000000, 0.9238795325112869605, 1.000000000000000000, 0.9238795325112869605, 1.000000000000000000, 0.9238795325112869605, 1.000000000000000000, 0.9238795325112869605, 1.000000000000000000, 0.9238795325112869605, 1.000000000000000000, 0.9238795325112869605, 1.000000000000000000, 0.9238795325112869605, 1.000000000000000000, 0.9238795325112869605, 1.000000000000000000, 0.9238795325112869605, 1.000000000000000000, 0.9238795325112869605, 1.000000000000000000, 0.9238795325112869605, 1.000000000000000000, 0.9238795325112869605, 1.000000000000000000, 0.9238795325112869605, 1.000000000000000000, 0.9238795325112869605, 1.000000000000000000, 0.9238795325112869605, 1.000000000000000000, 0.9238795325112869605, 1.000000000000000000, 0.9238795325112869605, 1.000000000000000000, 0.9238795325112869605, 1.000000000000000000, 0.9238795325112869605, 1.000000000000000000, 0.9238795325112869605, 1.000000000000000000, 0.9238795325112869605, 1.000000000000000000, 0.9238795325112869605, 1.000000000000000000, 0.9238795325112869605, 1.000000000000000000, 0.9238795325112869605, 1.000000000000000000, 0.9238795325112869605, 1.000000000000000000, 0.9238795325112869605, 1.000000000000000000, 0.9238795325112869605, 1.000000000000000000, 0.9238795325112869605, 1.000000000000000000, 0.9238795325112869605, 1.000000000000000000, 0.9238795325112869605, 1.000000000000000000, 0.9238795325112869605, 1.000000000000000000, 0.9238795325112869605, 1.000000000000000000, 0.9238795325112869605, 1.000000000000000000, 0.9238795325112869605, 1.000000000000000000, 0.9238795325112869605, 1.000000000000000000, 0.9238795325112869605, 1.000000000000000000, 0.9238795325112869605, 1.000000000000000000, 0.9238795325112869605, 1.000000000000000000, 0.9238795325112869605, 1.000000000000000000, 0.9238795325112869605, 1.000000000000000000, 0.9238795325112869605, 1.000000000000000000, 0.9238795325112869605, 1.000000000000000000, 0.9238795325112869605, 1.000000000000000000, 0.9238795325112869605, 1.000000000000000000, 0.9238795325112869605, 1.000000000000000000, 0.9238795325112869605, 1.000000000000000000, 0.9238795325112869605, 1.000000000000000000, 0.9238795325112869605, 1.000000000000000000, 0.9238795325112869605, 1.000000000000000000, 0.9238795325112869605, 1.000000000000000000, 0.9238795325112869605, 1.000000000000000000, 0.9238795325112869605, 1.000000000000000000, 0.9238795325112869605, 1.000000000000000000, 0.9238795325112869605, 1.000000000000000000, 0.9238795325112869605, 1.000000000000000000, 0.9238795325112869605, 1.000000000000000000, 0.9238795325112869605, 1.000000000000000000, 0.9238795325112869605, 1.000000000000000000, 0.9238795325112869605, 1.000000000000000000, 0.9238795325112869605, 1.000000000000000000, 0.9238795325112869605, 1.000000000000000000, 0.9238795325112869605, 1.000000000000000000, 0.9238795325112869605, 1.000000000000000000, 0.9238795325112869605, 1.000000000000000000, 0.9238795325112869605, 1.000000000000000000, 0.9238795325112869605, 1.000000000000000000, 0.9238795325112869605, 1.000000000000000000, 0.9238795325112869605, 1.000000000000000000, 0.9238795325112869605, 1.000000000000000000, 0.9238795325112869605, 1.000000000000000000, 0.9238795325112869605, 1.000000000000000000, 0.9238795325112869605, 1.000000000000000000, 0.9238795325112869605, 1.000000000000000000, 0.9238795325112869605, 1.000000000000000000, 0.9238795325112869605, 1.000000000000000000, 0.9238795325112869605, 1.000000000000000000, 0.9238795325112869605, 1.000000000000000000, 0.9238795325112869605, 1.000000000000000000, 0.9238795325112869605, 1.000000000000000000, 0.9238795325112869605, 1.000000000000000000, 0.9238795325112869605, 1.000000000000000000, 0.9238795325112869605, 1.000000000000000000, 0.9238795325112869605, 1.000000000000000000, 0.9238795325112869605, 1.000000000000000000, 0.9238795325112869605, 1.000000000000000000, 0.9238795325112869605, 1.000000000000000000, 0.9238795325112869605, 1.000000000000000000, 0.9238795325112869605, 1.000000000000000000, 0.9238795325112869605, 1.000000000000000000, 0.9238795325112869605, 1.000000000000000000, 0.9238795325112869605, 1.000000000000000000, 0.9238795325112869605, 1.000000000000000000, 0.9238795325112869605, 1.000000000000000000, 0.9238795325112869605, 1.000000000000000000, 0.9238795325112869605, 1.000000000000000000, 0.9238795325112869605, 1.000000000000000000, 0.9238795325112869605, 1.000000000000000000, 0.9238795325112869605, 1.000000000000000000, 0.9238795325112869605, 1.000000000000000000, 0.9238795325112869605, 1.000000000000000000, 0.9238795325112869605, 1.000000000000000000, 0.9238795325112869605, 1.000000000000000000, 0.9238795325112869605, 1.000000000000000000, 0.9238795325112869605, 1.000000000000000000, 0.9238795325112869605, 1.000000000000000000, 0.9238795325112869605, 1.000000000000000000, 0.9238795325112869605, 1.000000000000000000, 0.9238795325112869605, 1.000000000000000000, 0.9238795325112869605, 1.000000000000000000, 0.9238795325112869605, 1.000000000000000000, 0.9238795325112869605, 1.000000000000000000, 0.9238795325112869605, 1.000000000000000000, 0.9238795325112869605, 1.000000000000000000, 0.9238795325112869605, 1.000000000000000000, 0.9238795325112869605, 1.000000000000000000, 0.9238795325112869605, 1.000000000000000000, 0.9238795325112869605, 1.000000000000000000, 0.9238795325112869605, 1.000000000000000000, 0.9238795325112869605, 1.000000000000000000, 0.9238795325112869605, 1.000000000000000000, 0.9238795325112869605, 1.000000000000000000, 0.9238795325112869605, 1.000000000000000000, 0.9238795325112869605, 1.000000000000000000, 0.9238795325112869605, 1.000000000000000000, 0.9238795325112869605, 1.000000000000000000, 0.9238795325112869605, 1.000000000000000000, 0.9238795325112869605, 1.000000000000000000, 0.9238795325112869605, 1.000000000000000000, 0.9238795325112869605, 1.000000000000000000, 0.9238795325112869605, 1.000000000000000000, 0.9238795325112869605, 1.000000000000000000, 0.9238795325112869605, 1.000000000000000000, 0.9238795325112869605, 1.000000000000000000, 0.9238795325112869605, 1.000000000000000000, 0.9238795325112869605, 1.000000000000000000, 0.9238795325112869605, 1.000000000000000000, 0.9238795325112869605, 1.000000000000000000, 0.9238795325112869605, 1.000000000000000000, 0.9238795325112869605, 1.000000000000000000, 0.9238795325112869605, 1.000000000000000000, 0.9238795325112869605, 1.000000000000000000, 0.9238795325112869605, 1.000000000000000000, 0.9238795325112869605, 1.000000000000000000, 0.9238795325112869605, 1.000000000000000000),
 ( 1.000000000000000000, 0.9238795325112869605, 1.000000000000000000, 0.9238795325112869605, 1.000000000000000000, 0.9238795325112869605, 1.000000000000000000, 0.9238795325112869605, 1.000000000000000000, 0.9238795325112869605, 1.000000000000000000, 0.9238795325112869605, 1.000000000000000000, 0.9238795325112869605, 1.000000000000000000, 0.9238795325112869605, 1.000000000000000000, 0.9238795325112869605, 1.000000000000000000, 0.9238795325112869605, 1.000000000000000000, 0.9238795325112869605, 1.000000000000000000, 0.9238795325112869605, 1.000000000000000000, 0.9238795325112869605, 1.000000000000000000, 0.9238795325112869605, 1.000000000000000000, 0.9238795325112869605, 1.000000000000000000, 0.9238795325112869605, 1.000000000000000000, 0.9238795325112869605, 1.000000000000000000, 0.9238795325112869605, 1.000000000000000000, 0.9238795325112869605, 1.000000000000000000, 0.9238795325112869605, 1.000000000000000000, 0.9238795325112869605, 1.000000000000000000, 0.9238795325112869605, 1.000000000000000000, 0.9238795325112869605, 1.000000000000000000, 0.9238795325112869605, 1.000000000000000000, 0.9238795325112869605, 1.000000000000000000, 0.9238795325112869605, 1.000000000000000000, 0.9238795325112869605, 1.000000000000000000, 0.9238795325112869605, 1.000000000000000000, 0.9238795325112869605, 1.000000000000000000, 0.9238795325112869605, 1.000000000000000000, 0.9238795325112869605, 1.000000000000000000, 0.9238795325112869605, 1.000000000000000000, 0.9238795325112869605, 1.000000000000000000, 0.9238795325112869605, 1.000000000000000000, 0.9238795325112869605, 1.000000000000000000, 0.9238795325112869605, 1.000000000000000000, 0.9238795325112869605, 1.000000000000000000, 0.9238795325112869605, 1.000000000000000000, 0.9238795325112869605, 1.000000000000000000, 0.9238795325112869605, 1.000000000000000000, 0.9238795325112869605, 1.000000000000000000, 0.9238795325112869605, 1.000000000000000000, 0.9238795325112869605, 1.000000000000000000, 0.9238795325112869605, 1.000000000000000000, 0.9238795325112869605, 1.000000000000000000, 0.9238795325112869605, 1.000000000000000000, 0.9238795325112869605, 1.000000000000000000, 0.9238795325112869605, 1.000000000000000000, 0.9238795325112869605, 1.000000000000000000, 0.9238795325112869605, 1.000000000000000000, 0.9238795325112869605, 1.000000000000000000, 0.9238795325112869605, 1.000000000000000000, 0.9238795325112869605, 1.000000000000000000, 0.9238795325112869605, 1.000000000000000000, 0.9238795325112869605, 1.000000000000000000, 0.9238795325112869605, 1.000000000000000000, 0.9238795325112869605, 1.000000000000000000, 0.9238795325112869605, 1.000000000000000000, 0.9238795325112869605, 1.000000000000000000, 0.9238795325112869605, 1.000000000000000000, 0.9238795325112869605, 1.000000000000000000, 0.9238795325112869605, 1.000000000000000000, 0.9238795325112869605, 1.000000000000000000, 0.9238795325112869605, 1.000000000000000000, 0.9238795325112869605, 1.000000000000000000, 0.9238795325112869605, 1.000000000000000000, 0.9238795325112869605, 1.000000000000000000, 0.9238795325112869605, 1.000000000000000000, 0.9238795325112869605, 1.000000000000000000, 0.9238795325112869605, 1.000000000000000000, 0.9238795325112869605, 1.000000000000000000, 0.9238795325112869605, 1.000000000000000000, 0.9238795325112869605, 1.000000000000000000, 0.9238795325112869605, 1.000000000000000000, 0.9238795325112869605, 1.000000000000000000, 0.9238795325112869605, 1.000000000000000000, 0.9238795325112869605, 1.000000000000000000, 0.9238795325112869605, 1.000000000000000000, 0.9238795325112869605, 1.000000000000000000, 0.9238795325112869605, 1.000000000000000000, 0.9238795325112869605, 1.000000000000000000, 0.9238795325112869605, 1.000000000000000000, 0.9238795325112869605, 1.000000000000000000, 0.9238795325112869605, 1.000000000000000000, 0.9238795325112869605, 1.000000000000000000, 0.9238795325112869605, 1.000000000000000000, 0.9238795325112869605, 1.000000000000000000, 0.9238795325112869605, 1.000000000000000000, 0.9238795325112869605, 1.000000000000000000, 0.9238795325112869605, 1.000000000000000000, 0.9238795325112869605, 1.000000000000000000, 0.9238795325112869605, 1.000000000000000000, 0.9238795325112869605, 1.000000000000000000, 0.9238795325112869605, 1.000000000000000000, 0.9238795325112869605, 1.000000000000000000, 0.9238795325112869605, 1.000000000000000000, 0.9238795325112869605, 1.000000000000000000, 0.9238795325112869605, 1.000000000000000000, 0.9238795325112869605, 1.000000000000000000, 0.9238795325112869605, 1.000000000000000000, 0.9238795325112869605, 1.000000000000000000, 0.9238795325112869605, 1.000000000000000000, 0.9238795325112869605, 1.000000000000000000, 0.9238795325112869605, 1.000000000000000000, 0.9238795325112869605, 1.000000000000000000, 0.9238795325112869605, 1.000000000000000000, 0.9238795325112869605, 1.000000000000000000, 0.9238795325112869605, 1.000000000000000000, 0.9238795325112869605, 1.000000000000000000, 0.9238795325112869605, 1.000000000000000000, 0.9238795325112869605, 1.000000000000000000, 0.9238795325112869605, 1.000000000000000000, 0.9238795325112869605, 1.000000000000000000, 0.9238795325112869605, 1.000000000000000000, 0.9238795325112869605, 1.000000000000000000, 0.9238795325112869605, 1.000000000000000000, 0.9238795325112869605, 1.000000000000000000, 0.9238795325112869605, 1.000000000000000000, 0.9238795325112869605, 1.000000000000000000, 0.9238795325112869605, 1.000000000000000000, 0.9238795325112869605, 1.000000000000000000, 0.9238795325112869605, 1.000000000000000000, 0.9238795325112869605, 1.000000000000000000, 0.9238795325112869605, 1.000000000000000000, 0.9238795325112869605, 1.000000000000000000, 0.9238795325112869605, 1.000000000000000000, 0.9238795325112869605, 1.000000000000000000, 0.9238795325112869605, 1.000000000000000000, 0.9238795325112869605, 1.000000000000000000, 0.9238795325112869605, 1.000000000000000000, 0.9238795325112869605, 1.000000000000000000, 0.9238795325112869605, 1.000000000000000000, 0.9238795325112869605, 1.000000000000000000, 0.9238795325112869605, 1.000000000000000000, 0.9238795325112869605, 1.000000000000000000, 0.9238795325112869605, 1.000000000000000000, 0.9238795325112869605, 1.000000000000000000, 0.9238795325112869605, 1.000000000000000000, 0.9238795325112869605, 1.000000000000000000, 0.9238795325112869605, 1.000000000000000000, 0.9238795325112869605, 1.000000000000000000, 0.9238795325112869605, 1.000000000000000000, 0.9238795325112869605, 1.000000000000000000, 0.9238795325112869605, 1.000000000000000000, 0.9238795325112869605, 1.000000000000000000, 0.9238795325112869605, 1.000000000000000000, 0.9238795325112869605, 1.000000000000000000, 0.9238795325112869605, 1.000000000000000000, 0.9238795325112869605, 1.000000000000000000, 0.9238795325112869605, 1.000000000000000000, 0.9238795325112869605, 1.000000000000000000, 0.9238795325112869605, 1.000000000000000000, 0.9238795325112869605, 1.000000000000000000, 0.9238795325112869605, 1.000000000000000000, 0.9238795325112869605, 1.000000000000000000, 0.9238795325112869605, 1.000000000000000000, 0.9238795325112869605, 1.000000000000000000, 0.9238795325112869605, 1.000000000000000000, 0.9238795325112869605, 1.000000000000000000, 0.9238795325112869605, 1.000000000000000000, 0.9238795325112869605, 1.000000000000000000, 0.9238795325112869605, 1.000000000000000000, 0.9238795325112869605, 1.000000000000000000, 0.9238795325112869605, 1.000000000000000000, 0.9238795325112869605, 1.000000000000000000, 0.9238795325112869605, 1.000000000000000000, 0.9238795325112869605, 1.000000000000000000, 0.9238795325112869605, 1.000000000000000000, 0.9238795325112869605, 1.000000000000000000, 0.9238795325112869605, 1.000000000000000000, 0.9238795325112869605, 1.000000000000000000, 0.9238795325112869605, 1.000000000000000000, 0.9238795325112869605, 1.000000000000000000, 0.9238795325112869605, 1.000000000000000000, 0.9238795325112869605, 1.000000000000000000, 0.9238795325112869605, 1.000000000000000000, 0.9238795325112869605, 1.000000000000000000, 0.9238795325112869605, 1.000000000000000000, 0.9238795325112869605, 1.000000000000000000, 0.9238795325112869605, 1.000000000000000000, 0.9238795325112869605, 1.000000000000000000, 0.9238795325112869605, 1.000000000000000000, 0.9238795325112869605, 1.000000000000000000, 0.9238795325112869605, 1.000000000000000000, 0.9238795325112869605, 1.000000000000000000, 0.9238795325112869605, 1.000000000000000000, 0.9238795325112869605, 1.000000000000000000, 0.9238795325112869605, 1.000000000000000000, 0.9238795325112869605, 1.000000000000000000, 0.9238795325112869605, 1.000000000000000000, 0.9238795325112869605, 1.000000000000000000, 0.9238795325112869605, 1.000000000000000000, 0.9238795325112869605, 1.000000000000000000, 0.9238795325112869605, 1.000000000000000000, 0.9238795325112869605, 1.000000000000000000, 0.9238795325112869605, 1.000000000000000000, 0.9238795325112869605, 1.000000000000000000, 0.9238795325112869605, 1.000000000000000000, 0.9238795325112869605, 1.000000000000000000, 0.9238795325112869605, 1.000000000000000000, 0.9238795325112869605, 1.000000000000000000, 0.9238795325112869605, 1.000000000000000000, 0.9238795325112869605, 1.000000000000000000, 0.9238795325112869605, 1.000000000000000000, 0.9238795325112869605, 1.000000000000000000, 0.9238795325112869605, 1.000000000000000000, 0.9238795325112869605, 1.000000000000000000, 0.9238795325112869605, 1.000000000000000000, 0.9238795325112869605, 1.000000000000000000, 0.9238795325112869605, 1.000000000000000000, 0.9238795325112869605, 1.000000000000000000, 0.9238795325112869605, 1.000000000000000000, 0.9238795325112869605, 1.000000000000000000, 0.9238795325112869605, 1.000000000000000000, 0.9238795325112869605, 1.000000000000000000, 0.9238795325112869605, 1.000000000000000000, 0.9238795325112869605, 1.000000000000000000, 0.9238795325112869605, 1.000000000000000000, 0.9238795325112869605, 1.000000000000000000, 0.9238795325112869605, 1.000000000000000000, 0.9238795325112869605, 1.000000000000000000, 0.9238795325112869605, 1.000000000000000000, 0.9238795325112869605, 1.000000000000000000, 0.9238795325112869605, 1.000000000000000000, 0.9238795325112869605, 1.000000000000000000, 0.9238795325112869605, 1.000000000000000000, 0.9238795325112869605, 1.000000000000000000, 0.9238795325112869605, 1.000000000000000000, 0.9238795325112869605, 1.000000000000000000, 0.9238795325112869605, 1.000000000000000000, 0.9238795325112869605, 1.000000000000000000, 0.9238795325112869605, 1.000000000000000000, 0.9238795325112869605, 1.000000000000000000, 0.9238795325112869605, 1.000000000000000000, 0.9238795325112869605, 1.000000000000000000, 0.9238795325112869605, 1.000000000000000000, 0.9238795325112869605, 1.000000000000000000, 0.9238795325112869605, 1.000000000000000000, 0.9238795325112869605, 1.000000000000000000, 0.9238795325112869605, 1.000000000000000000, 0.9238795325112869605, 1.000000000000000000, 0.9238795325112869605, 1.000000000000000000, 0.9238795325112869605, 1.000000000000000000, 0.9238795325112869605, 1.000000000000000000, 0.9238795325112869605, 1.000000000000000000, 0.9238795325112869605, 1.000000000000000000, 0.9238795325112869605, 1.000000000000000000, 0.9238795325112869605, 1.000000000000000000, 0.9238795325112869605, 1.000000000000000000, 0.9238795325112869605, 1.000000000000000000, 0.9238795325112869605, 1.000000000000000000, 0.9238795325112869605, 1.000000000000000000, 0.9238795325112869605, 1.000000000000000000, 0.9238795325112869605, 1.000000000000000000, 0.9238795325112869605, 1.000000000000000000, 0.9238795325112869605, 1.000000000000000000, 0.9238795325112869605, 1.000000000000000000, 0.9238795325112869605, 1.000000000000000000, 0.9238795325112869605, 1.000000000000000000, 0.9238795325112869605, 1.000000000000000000, 0.9238795325112869605, 1.000000000000000000, 0.9238795325112869605, 1.000000000000000000, 0.9238795325112869605, 1.000000000000000000, 0.9238795325112869605, 1.000000000000000000, 0.9238795325112869605, 1.000000000000000000, 0.9238795325112869605, 1.000000000000000000, 0.9238795325112869605, 1.000000000000000000, 0.9238795325112869605, 1.000000000000000000, 0.9238795325112869605, 1.000000000000000000, 0.9238795325112869605, 1.000000000000000000, 0.9238795325112869605, 1.000000000000000000, 0.9238795325112869605, 1.000000000000000000, 0.9238795325112869605, 1.000000000000000000, 0.9238795325112869605, 1.000000000000000000, 0.9238795325112869605, 1.000000000000000000, 0.9238795325112869605, 1.000000000000000000, 0.9238795325112869605, 1.000000000000000000, 0.9238795325112869605, 1.000000000000000000, 0.9238795325112869605, 1.000000000000000000, 0.9238795325112869605, 1.000000000000000000, 0.9238795325112869605, 1.000000000000000000, 0.9238795325112869605, 1.000000000000000000, 0.9238795325112869605, 1.000000000000000000, 0.9238795325112869605, 1.000000000000000000, 0.9238795325112869605, 1.000000000000000000, 0.9238795325112869605, 1.000000000000000000, 0.9238795325112869605, 1.000000000000000000, 0.9238795325112869605, 1.000000000000000000, 0.9238795325112869605, 1.000000000000000000, 0.9238795325112869605, 1.000000000000000000, 0.9238795325112869605, 1.000000000000000000, 0.9238795325112869605, 1.000000000000000000, 0.9238795325112869605, 1.000000000000000000, 0.9238795325112869605, 1.000000000000000000, 0.9238795325112869605, 1.000000000000000000, 0.9238795325112869605, 1.000000000000000000, 0.9238795325112869605, 1.000000000000000000, 0.9238795325112869605, 1.000000000000000000, 0.9238795325112869605, 1.000000000000000000, 0.9238795325112869605, 1.000000000000000000, 0.9238795325112869605, 1.000000000000000000, 0.9238795325112869605, 1.000000000000000000, 0.9238795325112869605, 1.000000000000000000, 0.9238795325112869605, 1.000000000000000000, 0.9238795325112869605, 1.000000000000000000, 0.9238795325112869605, 1.000000000000000000, 0.9238795325112869605, 1.000000000000000000, 0.9238795325112869605, 1.000000000000000000, 0.9238795325112869605, 1.000000000000000000, 0.9238795325112869605, 1.000000000000000000, 0.9238795325112869605, 1.000000000000000000, 0.9238795325112869605, 1.000000000000000000, 0.9238795325112869605, 1.000000000000000000, 0.9238795325112869605, 1.000000000000000000, 0.9238795325112869605, 1.000000000000000000, 0.9238795325112869605, 1.000000000000000000, 0.9238795325112869605, 1.000000000000000000, 0.9238795325112869605, 1.000000000000000000, 0.9238795325112869605, 1.000000000000000000, 0.9238795325112869605, 1.000000000000000000, 0.9238795325112869605, 1.000000000000000000, 0.9238795325112869605, 1.000000000000000000, 0.9238795325112869605, 1.000000000000000000, 0.9238795325112869605, 1.000000000000000000, 0.9238795325112869605, 1.000000000000000000, 0.9238795325112869605, 1.000000000000000000, 0.9238795325112869605, 1.000000000000000000, 0.9238795325112869605, 1.000000000000000000, 0.9238795325112869605, 1.000000000000000000, 0.9238795325112869605, 1.000000000000000000, 0.9238795325112869605, 1.000000000000000000, 0.9238795325112869605, 1.000000000000000000, 0.9238795325112869605, 1.000000000000000000, 0.9238795325112869605, 1.000000000000000000, 0.9238795325112869605, 1.000000000000000000, 0.9238795325112869605, 1.000000000000000000, 0.9238795325112869605, 1.000000000000000000, 0.9238795325112869605, 1.000000000000000000, 0.9238795325112869605, 1.000000000000000000, 0.9238795325112869605, 1.000000000000000000, 0.9238795325112869605, 1.000000000000000000, 0.9238795325112869605, 1.000000000000000000, 0.9238795325112869605, 1.000000000000000000, 0.9238795325112869605, 1.000000000000000000, 0.9238795325112869605, 1.000000000000000000, 0.9238795325112869605, 1.000000000000000000, 0.9238795325112869605, 1.000000000000000000, 0.9238795325112869605, 1.000000000000000000, 0.9238795325112869605, 1.000000000000000000, 0.9238795325112869605, 1.000000000000000000, 0.9238795325112869605, 1.000000000000000000, 0.9238795325112869605, 1.000000000000000000, 0.9238795325112869605, 1.000000000000000000, 0.9238795325112869605, 1.000000000000000000, 0.9238795325112869605, 1.000000000000000000, 0.9238795325112869605, 1.000000000000000000, 0.9238795325112869605, 1.000000000000000000, 0.9238795325112869605, 1.000000000000000000, 0.9238795325112869605, 1.000000000000000000, 0.9238795325112869605, 1.000000000000000000, 0.9238795325112869605, 1.000000000000000000, 0.9238795325112869605, 1.000000000000000000, 0.9238795325112869605, 1.000000000000000000, 0.9238795325112869605, 1.000000000000000000, 0.9238795325112869605, 1.000000000000000000, 0.9238795325112869605, 1.000000000000000000, 0.9238795325112869605, 1.000000000000000000, 0.9238795325112869605, 1.000000000000000000, 0.9238795325112869605, 1.000000000000000000, 0.9238795325112869605, 1.000000000000000000, 0.9238795325112869605, 1.000000000000000000, 0.9238795325112869605, 1.000000000000000000, 0.9238795325112869605, 1.000000000000000000, 0.9238795325112869605, 1.000000000000000000, 0.9238795325112869605, 1.000000000000000000, 0.9238795325112869605, 1.000000000000000000, 0.9238795325112869605, 1.000000000000000000, 0.9238795325112869605, 1.000000000000000000, 0.9238795325112869605, 1.000000000000000000, 0.9238795325112869605, 1.000000000000000000, 0.9238795325112869605, 1.000000000000000000, 0.9238795325112869605, 1.000000000000000000, 0.9238795325112869605, 1.000000000000000000, 0.9238795325112869605, 1.000000000000000000, 0.9238795325112869605, 1.000000000000000000, 0.9238795325112869605, 1.000000000000000000, 0.9238795325112869605, 1.000000000000000000, 0.9238795325112869605, 1.000000000000000000, 0.9238795325112869605, 1.000000000000000000, 0.9238795325112869605, 1.000000000000000000, 0.9238795325112869605, 1.000000000000000000, 0.9238795325112869605, 1.000000000000000000, 0.9238795325112869605, 1.000000000000000000, 0.9238795325112869605, 1.000000000000000000, 0.9238795325112869605, 1.000000000000000000, 0.9238795325112869605, 1.000000000000000000, 0.9238795325112869605, 1.000000000000000000, 0.9238795325112869605, 1.000000000000000000, 0.9238795325112869605, 1.000000000000000000, 0.9238795325112869605, 1.000000000000000000) ) ) 
 REPRESENTATION_ITEM ( '' )  SURFACE ( )  ) ;
#7937 = CARTESIAN_POINT ( 'NONE',  ( -0.7185039370078739607, 1.928577636452523993E-17, 1.555118110128692832 ) ) ;
#7939 = CARTESIAN_POINT ( 'NONE',  ( -0.9893807788331910880, -0.1382476043231838647, 1.990360454373647947 ) ) ;
#7938 = LINE ( 'NONE', #2798, #32839 ) ;
#7940 = VECTOR ( 'NONE', #716, 39.37007874015748143 ) ;
#7941 = CARTESIAN_POINT ( 'NONE',  ( 0.7185039370078746268, -0.06523048226347956391, 1.252460629921259061 ) ) ;
#7942 = CARTESIAN_POINT ( 'NONE',  ( 1.002407869896990045, -0.1264236179284866091, 1.793799212544661348 ) ) ;
#7943 = DIRECTION ( 'NONE',  ( 1.000000000000000000, 0.000000000000000000, 0.000000000000000000 ) ) ;
#7944 = ORIENTED_EDGE ( 'NONE', *, *, #18516, .F. ) ;
#7945 = CARTESIAN_POINT ( 'NONE',  ( 0.7185039370078746268, 0.06523048226347956391, 0.1058070866141733041 ) ) ;
#7946 = CARTESIAN_POINT ( 'NONE',  ( -0.1377952755905511029, 1.687505431895958263E-17, -0.3149606299212598381 ) ) ;
#7947 = CARTESIAN_POINT ( 'NONE',  ( -0.1787899950787401604, -0.2440944881352131168, -0.07405724077823318263 ) ) ;
#7948 = CARTESIAN_POINT ( 'NONE',  ( 0.1594510458733777170, 0.1460701887063883264, 0.02793386226028452338 ) ) ;
#7949 = CARTESIAN_POINT ( 'NONE',  ( -0.1787899950787401604, -1.184055118056472455, -0.07405724077823318263 ) ) ;
#7950 = CARTESIAN_POINT ( 'NONE',  ( 0.8759842519685039353, -0.1787899950787401882, 0.2534448818360003908 ) ) ;
#7951 = EDGE_CURVE ( 'NONE', #36924, #39408, #38568, .T. ) ;
#7952 = CARTESIAN_POINT ( 'NONE',  ( 1.033464566929134687, 0.06523048226347956391, 0.05167322834645669133 ) ) ;
#7953 = CARTESIAN_POINT ( 'NONE',  ( -0.6971942568897637749, 2.189545951927499583E-17, 1.813484251914740053 ) ) ;
#7954 = ORIENTED_EDGE ( 'NONE', *, *, #25911, .F. ) ;
#7955 = DIRECTION ( 'NONE',  ( 0.000000000000000000, -1.000000000000000000, 0.000000000000000000 ) ) ;
#7956 = CARTESIAN_POINT ( 'NONE',  ( 1.054774247047244540, -0.07405724077823318263, 1.323818897584032817 ) ) ;
#7957 = CARTESIAN_POINT ( 'NONE',  ( 1.002407869896990045, -0.1264236179284866091, 1.985728346402929168 ) ) ;
#7958 = CARTESIAN_POINT ( 'NONE',  ( -1.002407869896990045, 0.1264236179284866091, 1.011318897584031484 ) ) ;
#7959 = EDGE_CURVE ( 'NONE', #22067, #45034, #10053, .T. ) ;
#7960 = CARTESIAN_POINT ( 'NONE',  ( -0.07382755323629552890, -0.09842514923570476471, -0.1628384097759718319 ) ) ;
#7961 = LINE ( 'NONE', #40069, #39215 ) ;
#7962 = CARTESIAN_POINT ( 'NONE',  ( 0.9500414927467377701, 0.1787899950787401604, 0.5068897637257642197 ) ) ;
#7963 = CARTESIAN_POINT ( 'NONE',  ( -1.002407869896990045, -0.1264236179284866091, 0.3715551180564728440 ) ) ;
#7964 = CARTESIAN_POINT ( 'NONE',  ( -0.6971942568897637749, 2.189545951927499583E-17, 0.6717519684501732646 ) ) ;
#7965 = CARTESIAN_POINT ( 'NONE',  ( 0.7185039370078746268, -0.06523048226347956391, 1.675688976270425679 ) ) ;
#7966 = EDGE_LOOP ( 'NONE', ( #7143, #11533, #18934, #47438 ) ) ;
#7967 = CARTESIAN_POINT ( 'NONE',  ( 0.000000000000000000, 0.000000000000000000, -0.1828167807439035619 ) ) ;
#7968 = CARTESIAN_POINT ( 'NONE',  ( -0.8759842519685039353, 0.1574803149606299191, 0.09842519685039370636 ) ) ;
#7969 = CARTESIAN_POINT ( 'NONE',  ( 0.8019270111902716547, -0.1787899950787401604, 1.077755905458048113 ) ) ;
#7970 = CARTESIAN_POINT ( 'NONE',  ( -0.8759842519685039353, -0.1787899950787401882, 1.980807086560409491 ) ) ;
#7971 = AXIS2_PLACEMENT_3D ( 'NONE', #21970, #25586, #32547 ) ;
#7972 = ORIENTED_EDGE ( 'NONE', *, *, #14716, .T. ) ;
#7973 = CARTESIAN_POINT ( 'NONE',  ( -0.8019270111902717657, -0.1787899950787401604, 0.8809055117572599514 ) ) ;
#7974 = CARTESIAN_POINT ( 'NONE',  ( 0.1264236179284866091, -1.487820818622939134, -0.1264236179284866091 ) ) ;
#7975 = AXIS2_PLACEMENT_3D ( 'NONE', #31654, #6682, #13888 ) ;
#7976 = ORIENTED_EDGE ( 'NONE', *, *, #46184, .T. ) ;
#7977 = CARTESIAN_POINT ( 'NONE',  ( -0.1264236179284866091, -0.5073818897100158543, 0.1264236179284866091 ) ) ;
#7978 = CARTESIAN_POINT ( 'NONE',  ( -0.06523048226347956391, 0.02903543317839319890, 0.1574803149606297803 ) ) ;
#7979 = EDGE_LOOP ( 'NONE', ( #27343, #3272, #28805, #7445, #43825 ) ) ;
#7980 = CARTESIAN_POINT ( 'NONE',  ( 0.6971942568897648851, -0.07405724077823297447, 1.225393700733637514 ) ) ;
#7981 = DIRECTION ( 'NONE',  ( 0.5000000000000007772, 0.8660254037844382635, 0.000000000000000000 ) ) ;
#7982 = DIRECTION ( 'NONE',  ( -0.8191520442889861364, 1.003171929053517844E-16, 0.5735764363510541530 ) ) ;
#7983 = CARTESIAN_POINT ( 'NONE',  ( 1.002407869896990045, -0.1264236179284866091, 1.513287401521039355 ) ) ;
#7984 = CARTESIAN_POINT ( 'NONE',  ( 0.6971942568897626646, 0.07405724077823318263, 0.1181102361667090567 ) ) ;
#7985 = CARTESIAN_POINT ( 'NONE',  ( 0.1264236179284866091, -1.752460629867496067, -0.1264236179284866091 ) ) ;
#7986 = CARTESIAN_POINT ( 'NONE',  ( -0.1787899950787401604, -1.695866141678520567, -0.07405724077823318263 ) ) ;
#7987 = APPLICATION_PROTOCOL_DEFINITION ( 'draft international standard', 'automotive_design', 1998, #15052 ) ;
#7988 = CARTESIAN_POINT ( 'NONE',  ( -1.033464566929134687, -0.06523048226347956391, 1.139271653435781184 ) ) ;
#7989 = ORIENTED_EDGE ( 'NONE', *, *, #24157, .F. ) ;
#7990 = CARTESIAN_POINT ( 'NONE',  ( -0.9500414927467377701, -0.1787899950787401604, 0.6102362204186774219 ) ) ;
#7991 = CARTESIAN_POINT ( 'NONE',  ( 0.06523048226347956391, -0.7878937007874025067, -0.1574803149606300301 ) ) ;
#7992 = CARTESIAN_POINT ( 'NONE',  ( 0.1797182628040039365, -1.438035935567297141, -2.200913952912460540E-17 ) ) ;
#7993 = CARTESIAN_POINT ( 'NONE',  ( 0.8759842519685039353, 0.000000000000000000, 4.498031496062992574 ) ) ;
#7994 = CIRCLE ( 'NONE', #14134, 0.07874015748031495954 ) ;
#7995 = CARTESIAN_POINT ( 'NONE',  ( 0.2471922904502826257, 0.09660984127287175482, -0.02629157619858345576 ) ) ;
#7996 = CARTESIAN_POINT ( 'NONE',  ( 0.8019270111902717657, 0.1787899950787401604, 1.338582677111590069 ) ) ;
#7997 = CARTESIAN_POINT ( 'NONE',  ( 0.7495606340400177148, 0.1264236179284866091, 1.651082677111590513 ) ) ;
#7998 = AXIS2_PLACEMENT_3D ( 'NONE', #4350, #41011, #30521 ) ;
#7999 = VECTOR ( 'NONE', #10189, 39.37007874015748143 ) ;
#8000 = CARTESIAN_POINT ( 'NONE',  ( -0.8070866141732283561, 0.000000000000000000, -0.7574803149606299524 ) ) ;
#8001 = CARTESIAN_POINT ( 'NONE',  ( 0.1377952755905511861, 0.1564960629921262614, -0.8070866141732283561 ) ) ;
#8002 = CARTESIAN_POINT ( 'NONE',  ( 0.7646288533564489232, -0.1113553986120547346, 0.8120078739082204899 ) ) ;
#8003 = CARTESIAN_POINT ( 'NONE',  ( 0.1476377952755906220, 0.4814845645395590679, -0.4766254685646189593 ) ) ;
#8004 = EDGE_CURVE ( 'NONE', #10926, #31032, #27855, .T. ) ;
#8005 = DIRECTION ( 'NONE',  ( 1.000000000000000000, 0.000000000000000000, -1.822029033848725275E-16 ) ) ;
#8006 = LINE ( 'NONE', #11627, #22275 ) ;
#8007 = CARTESIAN_POINT ( 'NONE',  ( 0.8107537697050253289, 0.1574803149606300301, 0.6815944880814486240 ) ) ;
#8008 = ORIENTED_EDGE ( 'NONE', *, *, #26812, .F. ) ;
#8009 = CARTESIAN_POINT ( 'NONE',  ( -0.8019270111902717657, 0.1787899950787401604, 1.062992125930488418 ) ) ;
#8010 = CARTESIAN_POINT ( 'NONE',  ( -0.1574803149606299191, -0.4410959923581754816, -0.9673892061308019263 ) ) ;
#8011 = ORIENTED_EDGE ( 'NONE', *, *, #47, .T. ) ;
#8012 = CARTESIAN_POINT ( 'NONE',  ( 0.1797182628040039087, -0.06254380958304553428, 0.07444174185955046430 ) ) ;
#8013 = CARTESIAN_POINT ( 'NONE',  ( -0.07405724077823318263, -1.233267716481668774, -0.1787899950787401604 ) ) ;
#8014 = DIRECTION ( 'NONE',  ( -3.469446951953612217E-15, -1.000000000000000000, 0.000000000000000000 ) ) ;
#8015 = CARTESIAN_POINT ( 'NONE',  ( 1.002407869896990045, -0.1264236179284866091, 1.552657480261196765 ) ) ;
#8016 = ADVANCED_FACE ( 'NONE', ( #8857 ), #16069, .T. ) ;
#8018 = LINE ( 'NONE', #43489, #13951 ) ;
#8017 = CARTESIAN_POINT ( 'NONE',  ( -0.7185039370078739607, 1.928577636452523993E-17, 0.9350393700787401619 ) ) ;
#8019 = CARTESIAN_POINT ( 'NONE',  ( 0.8759842519685039353, 0.1574803149606299191, 0.3641732282389295583 ) ) ;
#8020 = CARTESIAN_POINT ( 'NONE',  ( 0.1264236179284866091, -0.1333661416785200671, -0.1264236179284866091 ) ) ;
#8021 = CARTESIAN_POINT ( 'NONE',  ( 0.9412147342319837628, 0.1574803149606300301, 1.306594488081449290 ) ) ;
#8022 = EDGE_LOOP ( 'NONE', ( #19176, #42426, #17165, #14056 ) ) ;
#8023 = CARTESIAN_POINT ( 'NONE',  ( 0.2395294000716133853, 0.1968503937007874127, 1.181102362204724310 ) ) ;
#8024 = DIRECTION ( 'NONE',  ( 0.000000000000000000, 0.000000000000000000, 1.000000000000000000 ) ) ;
#8025 = CARTESIAN_POINT ( 'NONE',  ( 0.8019270111902717657, -0.1787899950787401604, 0.6840551180564720113 ) ) ;
#8026 = CARTESIAN_POINT ( 'NONE',  ( 0.7495606340400177148, 0.1264236179284866091, 0.8686023621509606496 ) ) ;
#8027 = CARTESIAN_POINT ( 'NONE',  ( -0.1574803149606299191, -0.05708661406570126468, 0.000000000000000000 ) ) ;
#8028 = CARTESIAN_POINT ( 'NONE',  ( -1.054774247047244540, 0.07405724077823318263, 1.289370078686393750 ) ) ;
#8029 = CARTESIAN_POINT ( 'NONE',  ( -0.7495606340400177148, -0.1264236179284866091, 0.2878937007336381804 ) ) ;
#8030 = DIRECTION ( 'NONE',  ( 1.000000000000000000, -0.000000000000000000, -0.000000000000000000 ) ) ;
#8031 = AXIS2_PLACEMENT_3D ( 'NONE', #44265, #15073, #47415 ) ;
#8032 = AXIS2_PLACEMENT_3D ( 'NONE', #19929, #16364, #7557 ) ;
#8033 = DIRECTION ( 'NONE',  ( -1.000000000000000000, 0.000000000000000000, 0.000000000000000000 ) ) ;
#8034 = CARTESIAN_POINT ( 'NONE',  ( -0.1264236179284866091, -1.005537354056009969, -0.1264236179284866091 ) ) ;
#8035 = EDGE_LOOP ( 'NONE', ( #1710, #3014, #36563, #34820, #10818, #44347 ) ) ;
#8036 = CARTESIAN_POINT ( 'NONE',  ( 0.07405724077823318263, 0.05118110241596821736, 0.1787899950787401604 ) ) ;
#8037 = VECTOR ( 'NONE', #34710, 39.37007874015748854 ) ;
#8038 = ORIENTED_EDGE ( 'NONE', *, *, #14363, .T. ) ;
#8039 = ADVANCED_FACE ( 'NONE', ( #23961 ), #2131, .T. ) ;
#8040 = CYLINDRICAL_SURFACE ( 'NONE', #25376, 0.2559055118110236116 ) ;
#8041 = DIRECTION ( 'NONE',  ( -1.000000000000000000, 0.000000000000000000, 0.000000000000000000 ) ) ;
#8042 = CARTESIAN_POINT ( 'NONE',  ( 0.1787899950787401604, -0.5344488188438744070, -0.07405724077823318263 ) ) ;
#8043 = ( BOUNDED_CURVE ( )  B_SPLINE_CURVE ( 2, ( #3470, #35826, #21192, #17846, #39396, #25767, #40337, #10916, #39630 ),
 .UNSPECIFIED., .F., .T. ) 
 B_SPLINE_CURVE_WITH_KNOTS ( ( 3, 2, 2, 2, 3 ),
 ( 0.5000000000000000000, 0.5024999999999999467, 0.5050000000000000044, 0.5074999999999999512, 0.5100000000000000089 ),
 .UNSPECIFIED. ) 
 CURVE ( )  GEOMETRIC_REPRESENTATION_ITEM ( )  RATIONAL_B_SPLINE_CURVE ( ( 1.000000000000000000, 0.9238795325112869605, 1.000000000000000000, 0.9238795325112869605, 1.000000000000000000, 0.9238795325112869605, 1.000000000000000000, 0.9238795325112869605, 1.000000000000000000 ) ) 
 REPRESENTATION_ITEM ( '' )  ) ;
#8044 = CARTESIAN_POINT ( 'NONE',  ( -0.8759842519685039353, 0.1787899950787401882, 0.1550196849856066983 ) ) ;
#8045 = CARTESIAN_POINT ( 'NONE',  ( -0.7185039370078746268, 0.06523048226347956391, 0.8538385826771660581 ) ) ;
#8046 = LINE ( 'NONE', #23151, #41459 ) ;
#8047 = DIRECTION ( 'NONE',  ( -0.5735764363510518216, 0.8191520442889876907, 1.003171929053519693E-16 ) ) ;
#8048 = CARTESIAN_POINT ( 'NONE',  ( -0.1270800023317771588, -0.9508312111578485215, -0.1270800023317771588 ) ) ;
#8049 = PLANE ( 'NONE',  #33253 ) ;
#8050 = CARTESIAN_POINT ( 'NONE',  ( -1.033464566929133799, 0.000000000000000000, 1.496062992018456494 ) ) ;
#8051 = ADVANCED_FACE ( 'NONE', ( #12718 ), #20578, .T. ) ;
#8052 = CARTESIAN_POINT ( 'NONE',  ( 1.054774247047244540, -0.07405724077823318263, 0.9301181101824563813 ) ) ;
#8053 = CARTESIAN_POINT ( 'NONE',  ( 0.8019270111902716547, -0.1787899950787401604, 0.1279527558517483676 ) ) ;
#8054 = CARTESIAN_POINT ( 'NONE',  ( 0.8759842519685039353, 0.1574803149606299191, 0.5216535431995598104 ) ) ;
#8055 = CARTESIAN_POINT ( 'NONE',  ( 0.8759842519685039353, -0.1574803149606299191, 1.338582677165354395 ) ) ;
#8057 = CYLINDRICAL_SURFACE ( 'NONE', #27660, 0.1574803149606299191 ) ;
#8056 = CARTESIAN_POINT ( 'NONE',  ( 0.7249778915871685214, -0.07478501380931205922, 1.984713715274026846 ) ) ;
#8058 = CARTESIAN_POINT ( 'NONE',  ( 1.284448818897637956, 0.000000000000000000, -1.181102362204724310 ) ) ;
#8059 = EDGE_CURVE ( 'NONE', #39837, #14452, #41653, .T. ) ;
#8061 = CARTESIAN_POINT ( 'NONE',  ( 0.1586955767088203406, 0.1469626601063697413, 0.02104375706135626356 ) ) ;
#8060 = CARTESIAN_POINT ( 'NONE',  ( 0.9500414927467377701, -0.1787899950787401604, 0.8809055117572600624 ) ) ;
#8063 = AXIS2_PLACEMENT_3D ( 'NONE', #8148, #705, #15363 ) ;
#8062 = CARTESIAN_POINT ( 'NONE',  ( 0.1264236179284866091, -0.6943897637257637756, 0.1264236179284866091 ) ) ;
#8064 = ORIENTED_EDGE ( 'NONE', *, *, #14890, .F. ) ;
#8065 = CARTESIAN_POINT ( 'NONE',  ( -0.7185039370078739607, 0.000000000000000000, -2.869337061179095023E-17 ) ) ;
#8066 = AXIS2_PLACEMENT_3D ( 'NONE', #6740, #21359, #26633 ) ;
#8067 = AXIS2_PLACEMENT_3D ( 'NONE', #1133, #44266, #44735 ) ;
#8068 = CARTESIAN_POINT ( 'NONE',  ( 0.003857550520839538987, -0.1410454915399121656, 0.03130963158119893369 ) ) ;
#8069 = CARTESIAN_POINT ( 'NONE',  ( 0.6971942568897648851, -0.07405724077823297447, 1.146653543253323582 ) ) ;
#8070 = EDGE_CURVE ( 'NONE', #6712, #7899, #21370, .T. ) ;
#8071 = CARTESIAN_POINT ( 'NONE',  ( 0.04485236092672649499, -0.5708661417322835607, 1.206847064312615903 ) ) ;
#8072 = CARTESIAN_POINT ( 'NONE',  ( 0.06523048226347956391, -1.629429133858268930, 0.1574803149606297803 ) ) ;
#8073 = CARTESIAN_POINT ( 'NONE',  ( -0.7185039370078746268, -0.06523048226347956391, 0.5044291338582675976 ) ) ;
#8074 = VERTEX_POINT ( 'NONE', #27345 ) ;
#8075 = LINE ( 'NONE', #3776, #29859 ) ;
#8076 = CARTESIAN_POINT ( 'NONE',  ( -0.6971942568897626646, 0.07405724077823318263, 0.2755905511273391006 ) ) ;
#8077 = ORIENTED_EDGE ( 'NONE', *, *, #13535, .T. ) ;
#8078 = CARTESIAN_POINT ( 'NONE',  ( -0.7646288533564489232, -0.1113553986120547346, 0.7037401574803149318 ) ) ;
#8079 = CARTESIAN_POINT ( 'NONE',  ( 0.07405724077823318263, -1.592519684985606254, -0.1787899950787401604 ) ) ;
#8080 = CARTESIAN_POINT ( 'NONE',  ( -0.8759842519685039353, -0.1787899950787401882, 1.783956692859621995 ) ) ;
#8081 = CARTESIAN_POINT ( 'NONE',  ( -0.7495606340400177148, 0.1264236179284866091, 0.9030511810485984947 ) ) ;
#8082 = CARTESIAN_POINT ( 'NONE',  ( -1.054774247047244540, -0.07405724077823318263, 0.5364173227808821665 ) ) ;
#8083 = CARTESIAN_POINT ( 'NONE',  ( -1.033464566929134687, -0.06523048226347956391, 0.1156496061916856694 ) ) ;
#8084 = CYLINDRICAL_SURFACE ( 'NONE', #24731, 0.1864803149606299171 ) ;
#8085 = CARTESIAN_POINT ( 'NONE',  ( 0.1345513924870780087, 0.1295369909362752148, -0.09891213622343476841 ) ) ;
#8086 = CARTESIAN_POINT ( 'NONE',  ( 0.02442443439252881682, 0.05525422739384140691, -0.2713316170948109063 ) ) ;
#8087 = CARTESIAN_POINT ( 'NONE',  ( 0.1968503937007874682, -0.5192708129487058066, -0.8938220056861535534 ) ) ;
#8088 = CARTESIAN_POINT ( 'NONE',  ( -0.07405724077823318263, -0.6142971965756950370, -0.1787899950787401604 ) ) ;
#8089 = CARTESIAN_POINT ( 'NONE',  ( -0.01779600182615102485, -0.08955987627499310821, 0.2207522308509031472 ) ) ;
#8090 = DIRECTION ( 'NONE',  ( -0.000000000000000000, 1.000000000000000000, -0.000000000000000000 ) ) ;
#8091 = CARTESIAN_POINT ( 'NONE',  ( 1.033464566929134687, 0.06523048226347956391, 1.783956692913386544 ) ) ;
#8092 = AXIS2_PLACEMENT_3D ( 'NONE', #865, #15769, #33278 ) ;
#8093 = CARTESIAN_POINT ( 'NONE',  ( 0.7185039370078739607, 1.928577636452523993E-17, 1.555118110128692832 ) ) ;
#8094 = CARTESIAN_POINT ( 'NONE',  ( -0.6971942568897626646, -0.07405724077823297447, 0.2411417322297011168 ) ) ;
#8095 = CARTESIAN_POINT ( 'NONE',  ( 0.1787899950787401882, -1.728962550906403495, -2.189545951927503898E-17 ) ) ;
#8096 = EDGE_LOOP ( 'NONE', ( #32413, #41131 ) ) ;
#8097 = FACE_OUTER_BOUND ( 'NONE', #21451, .T. ) ;
#8098 = VERTEX_POINT ( 'NONE', #9096 ) ;
#8099 = CARTESIAN_POINT ( 'NONE',  ( -1.002407869896990045, -0.1264236179284866091, 1.557578740103716441 ) ) ;
#8100 = ORIENTED_EDGE ( 'NONE', *, *, #20127, .F. ) ;
#8101 = EDGE_CURVE ( 'NONE', #30394, #22319, #13184, .T. ) ;
#8102 = CARTESIAN_POINT ( 'NONE',  ( 0.1787899950787401882, -1.363681102308440973, -2.189545951927503898E-17 ) ) ;
#8103 = CARTESIAN_POINT ( 'NONE',  ( 3.284318927891251994E-17, -1.565452755851747924, 0.1787899950787401882 ) ) ;
#8104 = LINE ( 'NONE', #22726, #25588 ) ;
#8105 = CARTESIAN_POINT ( 'NONE',  ( 0.1644020957507537628, -0.08115590401245532937, 0.1405661490837558925 ) ) ;
#8106 = CARTESIAN_POINT ( 'NONE',  ( 1.033464566929134687, 0.06523048226347956391, 0.4847440944881890590 ) ) ;
#8107 = CARTESIAN_POINT ( 'NONE',  ( 0.5555748031496077211, 2.215965818540671970E-15, 0.7480314960629921295 ) ) ;
#8108 = CARTESIAN_POINT ( 'NONE',  ( -1.033464566929134687, -0.06523048226347956391, 1.139271653435780962 ) ) ;
#8109 = EDGE_CURVE ( 'NONE', #20455, #1535, #42495, .T. ) ;
#8110 = LINE ( 'NONE', #24976, #39050 ) ;
#8111 = CARTESIAN_POINT ( 'NONE',  ( 1.033464566929133799, 0.000000000000000000, 1.929133858160188897 ) ) ;
#8112 = ORIENTED_EDGE ( 'NONE', *, *, #47127, .F. ) ;
#8113 = CARTESIAN_POINT ( 'NONE',  ( 0.9873396505805591694, -0.1113553986120547346, 0.04429133858267716300 ) ) ;
#8114 = CARTESIAN_POINT ( 'NONE',  ( -1.054774247047244540, -0.07405724077823318263, 0.9694881889226145688 ) ) ;
#8115 = PLANE ( 'NONE',  #11348 ) ;
#8116 = CARTESIAN_POINT ( 'NONE',  ( 0.7185039370078739607, 1.928577636452523993E-17, 1.525590551181102317 ) ) ;
#8117 = CARTESIAN_POINT ( 'NONE',  ( -0.1649531470039379555, -0.08956211461529646478, 0.02954168907489855556 ) ) ;
#8118 = ORIENTED_EDGE ( 'NONE', *, *, #13747, .F. ) ;
#8119 = CARTESIAN_POINT ( 'NONE',  ( 0.1586952649960582662, -0.05525522230752598352, -0.1377952755905511306 ) ) ;
#8120 = AXIS2_PLACEMENT_3D ( 'NONE', #14672, #3640, #20 ) ;
#8121 = VERTEX_POINT ( 'NONE', #41950 ) ;
#8122 = ADVANCED_FACE ( 'NONE', ( #4837 ), #14929, .T. ) ;
#8123 = DIRECTION ( 'NONE',  ( 7.888609052210116302E-31, 0.6156614753256598460, 0.7880107536067206819 ) ) ;
#8124 = CARTESIAN_POINT ( 'NONE',  ( 0.9412147342319837628, -0.1574803149606297803, 1.380413385826771533 ) ) ;
#8125 = CARTESIAN_POINT ( 'NONE',  ( 0.07405724077823318263, -1.523622047190330564, 0.1787899950787401604 ) ) ;
#8126 = CARTESIAN_POINT ( 'NONE',  ( 3.284318927891251994E-17, -0.9404527558517480346, 0.1787899950787401882 ) ) ;
#8127 = CARTESIAN_POINT ( 'NONE',  ( -0.1113553986120547346, -1.174212598425196985, -0.1113553986120547346 ) ) ;
#8128 = CARTESIAN_POINT ( 'NONE',  ( 0.9873396505805591694, -0.1113553986120547346, 1.058070866034204860 ) ) ;
#8129 = CARTESIAN_POINT ( 'NONE',  ( 0.9412147342319837628, 0.1574803149606300301, 1.828248031496063630 ) ) ;
#8130 = UNCERTAINTY_MEASURE_WITH_UNIT (LENGTH_MEASURE( 1.000000000000000082E-05 ), #44890, 'distance_accuracy_value', 'NONE') ;
#8131 = CARTESIAN_POINT ( 'NONE',  ( -0.8019270111902717657, 0.1787899950787401604, 0.4675196849856070869 ) ) ;
#8132 = ORIENTED_EDGE ( 'NONE', *, *, #31532, .F. ) ;
#8133 = CARTESIAN_POINT ( 'NONE',  ( -0.6971942568897648851, -0.07405724077823297447, 1.742125984198204858 ) ) ;
#8134 = CARTESIAN_POINT ( 'NONE',  ( 0.6971942568897648851, -0.07405724077823297447, 1.663385826717890925 ) ) ;
#8135 = CARTESIAN_POINT ( 'NONE',  ( 2.892866454678787531E-17, -1.346456692805858113, 0.1574803149606299191 ) ) ;
#8136 = DIRECTION ( 'NONE',  ( 0.000000000000000000, 0.000000000000000000, 1.000000000000000000 ) ) ;
#8137 = CARTESIAN_POINT ( 'NONE',  ( 0.7495606340400177148, 0.1264236179284866091, 0.2386811023084413619 ) ) ;
#8138 = DIRECTION ( 'NONE',  ( -1.000000000000000000, -0.000000000000000000, 0.000000000000000000 ) ) ;
#8139 = CARTESIAN_POINT ( 'NONE',  ( -1.002407869896990045, 0.1264236179284866091, 1.168799212544661348 ) ) ;
#8140 = CARTESIAN_POINT ( 'NONE',  ( -0.9500414927467378812, 0.1787899950787401604, 0.1131889763241892138 ) ) ;
#8141 = DIRECTION ( 'NONE',  ( 1.822029033848725028E-16, 0.000000000000000000, 1.000000000000000000 ) ) ;
#8142 = CARTESIAN_POINT ( 'NONE',  ( -0.9500414927467378812, 0.1787899950787401604, 1.530511810969859443 ) ) ;
#8143 = CARTESIAN_POINT ( 'NONE',  ( -0.8759842519685039353, -0.1574803149606299191, 1.998031495955464587 ) ) ;
#8144 = VERTEX_POINT ( 'NONE', #19459 ) ;
#8145 = CARTESIAN_POINT ( 'NONE',  ( 0.8107537697050254399, -0.1574803149606297803, 0.9719488187901104137 ) ) ;
#8146 = CARTESIAN_POINT ( 'NONE',  ( 0.7495606340400177148, 0.1264236179284866091, 1.577263779473795369 ) ) ;
#8147 = CARTESIAN_POINT ( 'NONE',  ( -0.1299735959408482300, -0.09851383385443740481, 0.1030069632188811007 ) ) ;
#8148 = CARTESIAN_POINT ( 'NONE',  ( 0.1377952755905511861, 0.1574803149606299191, -0.8070866141732283561 ) ) ;
#8149 = EDGE_LOOP ( 'NONE', ( #30196, #26286, #17746, #7185, #35437 ) ) ;
#8150 = VERTEX_POINT ( 'NONE', #8674 ) ;
#8151 = CARTESIAN_POINT ( 'NONE',  ( -0.8019270111902716547, -0.1787899950787401604, 1.156496062938362046 ) ) ;
#8152 = ORIENTED_EDGE ( 'NONE', *, *, #18556, .F. ) ;
#8153 = EDGE_CURVE ( 'NONE', #8512, #8746, #32996, .T. ) ;
#8154 = CARTESIAN_POINT ( 'NONE',  ( -0.1787899950787401604, -0.8740157479777336258, -0.07405724077823318263 ) ) ;
#8155 = EDGE_CURVE ( 'NONE', #31760, #30794, #4850, .T. ) ;
#8156 = CARTESIAN_POINT ( 'NONE',  ( -1.094772975963752103E-17, -1.073326771599779628, -0.1787899950787401882 ) ) ;
#8157 = ORIENTED_EDGE ( 'NONE', *, *, #42018, .T. ) ;
#8158 = CARTESIAN_POINT ( 'NONE',  ( 0.1797182628040039365, -0.2963036521027306858, -2.200913952912460540E-17 ) ) ;
#8159 = EDGE_CURVE ( 'NONE', #30980, #23202, #13030, .T. ) ;
#8160 = CARTESIAN_POINT ( 'NONE',  ( -0.1574803149606299191, 0.09055118110236221041, 0.000000000000000000 ) ) ;
#8161 = CARTESIAN_POINT ( 'NONE',  ( 3.284318927891251994E-17, -0.1924212597887563214, 0.1787899950787401882 ) ) ;
#8162 = EDGE_CURVE ( 'NONE', #41227, #11128, #25026, .T. ) ;
#8163 = CARTESIAN_POINT ( 'NONE',  ( 0.5057057357416000487, 4.766607801171850497E-17, 0.000000000000000000 ) ) ;
#8164 = CARTESIAN_POINT ( 'NONE',  ( 0.9500414927467378812, 0.1787899950787401604, 0.8169291338045038264 ) ) ;
#8166 = SURFACE_SIDE_STYLE ('',( #29795 ) ) ;
#8165 = CARTESIAN_POINT ( 'NONE',  ( -0.7646288533564489232, -0.1113553986120547346, 1.560039369971212508 ) ) ;
#8167 = DIRECTION ( 'NONE',  ( 0.000000000000000000, 0.000000000000000000, 1.000000000000000000 ) ) ;
#8168 = CARTESIAN_POINT ( 'NONE',  ( 0.8759842519685039353, 0.000000000000000000, 4.498031496062992574 ) ) ;
#8169 = CARTESIAN_POINT ( 'NONE',  ( 0.9500414927467378812, 0.1787899950787401604, 1.884842519631275026 ) ) ;
#8170 = CARTESIAN_POINT ( 'NONE',  ( 0.7646288533564489232, 0.1113553986120547346, 0.1427165354330708902 ) ) ;
#8171 = CYLINDRICAL_SURFACE ( 'NONE', #16794, 0.1574803149606299191 ) ;
#8173 = CARTESIAN_POINT ( 'NONE',  ( 0.07405724077823318263, -0.3326771653005671237, -0.1787899950787401604 ) ) ;
#8172 = CARTESIAN_POINT ( 'NONE',  ( -0.06523048226347956391, -0.9552165353255434033, 0.1574803149606297803 ) ) ;
#8174 = CARTESIAN_POINT ( 'NONE',  ( 1.033464566929133799, 0.000000000000000000, 0.4724409447743622148 ) ) ;
#8176 = CIRCLE ( 'NONE', #35001, 0.09842519685039370636 ) ;
#8175 = CARTESIAN_POINT ( 'NONE',  ( 3.284318927891251994E-17, -1.250492125930488196, 0.1787899950787401882 ) ) ;
#8177 = CARTESIAN_POINT ( 'NONE',  ( 0.8759842519685039353, -0.1787899950787401882, 0.2928149605761578567 ) ) ;
#8178 = DIRECTION ( 'NONE',  ( 1.822029033848725028E-16, 0.000000000000000000, 1.000000000000000000 ) ) ;
#8179 = CARTESIAN_POINT ( 'NONE',  ( -0.8019270111902717657, 0.1787899950787401604, 1.727362204670645385 ) ) ;
#8180 = ORIENTED_EDGE ( 'NONE', *, *, #43386, .T. ) ;
#8181 = CARTESIAN_POINT ( 'NONE',  ( -0.8019270111902717657, 0.1787899950787401604, 1.259842519631276359 ) ) ;
#8182 = CARTESIAN_POINT ( 'NONE',  ( -1.033464566929134687, 0.06523048226347956391, 0.3272637795275590289 ) ) ;
#8183 = CARTESIAN_POINT ( 'NONE',  ( -0.6971942568897626646, -0.07405724077823297447, 0.5216535432533228045 ) ) ;
#8184 = CARTESIAN_POINT ( 'NONE',  ( 1.002407869896990045, 0.1264236179284866091, 1.916830708607653477 ) ) ;
#8185 = CARTESIAN_POINT ( 'NONE',  ( -0.7495606340400177148, -0.1264236179284866091, 1.070374015694267600 ) ) ;
#8186 = FACE_OUTER_BOUND ( 'NONE', #42368, .T. ) ;
#8187 = CARTESIAN_POINT ( 'NONE',  ( -0.07818037259012035334, -0.09842482883889538958, -0.1607972800070663622 ) ) ;
#8188 = CARTESIAN_POINT ( 'NONE',  ( 0.3123359580052492146, 4.616380251121755931E-17, 0.000000000000000000 ) ) ;
#8189 = CARTESIAN_POINT ( 'NONE',  ( 0.8019270111902716547, 0.1787899950787401604, 0.4724409448281262636 ) ) ;
#8190 = CARTESIAN_POINT ( 'NONE',  ( -1.002407869896990045, 0.1264236179284866091, 0.4601377952218267953 ) ) ;
#8191 = CARTESIAN_POINT ( 'NONE',  ( -0.9500414927467378812, 0.1787899950787401604, 0.8562992125446617919 ) ) ;
#8192 = CARTESIAN_POINT ( 'NONE',  ( 0.8107537697050253289, 0.1574803149606300301, 1.705216535325545069 ) ) ;
#8193 = ORIENTED_EDGE ( 'NONE', *, *, #31586, .T. ) ;
#8194 = ORIENTED_EDGE ( 'NONE', *, *, #23654, .F. ) ;
#8195 = ( BOUNDED_CURVE ( )  B_SPLINE_CURVE ( 2, ( #29358, #7952, #22803, #18504, #4569, #29808, #19203, #15640, #44355 ),
 .UNSPECIFIED., .F., .T. ) 
 B_SPLINE_CURVE_WITH_KNOTS ( ( 3, 2, 2, 2, 3 ),
 ( 0.02000000000000000042, 0.02249999999999999917, 0.02500000000000000139, 0.02750000000000000014, 0.02999999999999999889 ),
 .UNSPECIFIED. ) 
 CURVE ( )  GEOMETRIC_REPRESENTATION_ITEM ( )  RATIONAL_B_SPLINE_CURVE ( ( 1.000000000000000000, 0.9238795325112869605, 1.000000000000000000, 0.9238795325112869605, 1.000000000000000000, 0.9238795325112869605, 1.000000000000000000, 0.9238795325112869605, 1.000000000000000000 ) ) 
 REPRESENTATION_ITEM ( '' )  ) ;
#8196 = CARTESIAN_POINT ( 'NONE',  ( 0.000000000000000000, 0.3740157480314960647, 0.9783464566929134243 ) ) ;
#8197 = CARTESIAN_POINT ( 'NONE',  ( 0.9500414927467378812, 0.1787899950787401604, 0.9005905511273389896 ) ) ;
#8198 = CARTESIAN_POINT ( 'NONE',  ( -0.7185039370078746268, -0.06523048226347956391, 0.07135826771653554224 ) ) ;
#8199 = CARTESIAN_POINT ( 'NONE',  ( 0.8019270111902716547, 0.1787899950787401604, 1.220472440891118504 ) ) ;
#8200 = CARTESIAN_POINT ( 'NONE',  ( -0.2160974785307145929, -0.09851385176812245403, -0.1192534063745566836 ) ) ;
#8201 = ORIENTED_EDGE ( 'NONE', *, *, #16256, .T. ) ;
#8202 = LINE ( 'NONE', #22826, #28707 ) ;
#8203 = CARTESIAN_POINT ( 'NONE',  ( 0.1558458267876820791, -0.1470250908559870007, -0.02093562383110287445 ) ) ;
#8204 = CARTESIAN_POINT ( 'NONE',  ( -0.4338976377952755703, 5.489612613713267203E-34, 0.000000000000000000 ) ) ;
#8205 = CARTESIAN_POINT ( 'NONE',  ( -0.1264236179284866091, -1.468135779252860207, 0.1264236179284866091 ) ) ;
#8206 = ORIENTED_EDGE ( 'NONE', *, *, #32698, .F. ) ;
#8207 = CARTESIAN_POINT ( 'NONE',  ( 0.1264236179284866091, -0.4975393700249764461, 0.1264236179284866091 ) ) ;
#8208 = CARTESIAN_POINT ( 'NONE',  ( -0.2984316586355670875, -0.08457185433607530833, 0.7311987702743616424 ) ) ;
#8209 = VERTEX_POINT ( 'NONE', #16128 ) ;
#8210 = CARTESIAN_POINT ( 'NONE',  ( 1.002407869896990045, 0.1264236179284866091, 1.326279527505291433 ) ) ;
#8211 = DIRECTION ( 'NONE',  ( 0.000000000000000000, 1.000000000000000000, 0.000000000000000000 ) ) ;
#8212 = FACE_OUTER_BOUND ( 'NONE', #869, .T. ) ;
#8213 = AXIS2_PLACEMENT_3D ( 'NONE', #40116, #95, #18332 ) ;
#8214 = ( BOUNDED_CURVE ( )  B_SPLINE_CURVE ( 2, ( #5438, #34698, #2080, #1842, #28211, #7342, #35403, #18119, #6375 ),
 .UNSPECIFIED., .F., .F. ) 
 B_SPLINE_CURVE_WITH_KNOTS ( ( 3, 2, 2, 2, 3 ),
 ( 0.9100000000000000311, 0.9124999999999999778, 0.9150000000000000355, 0.9174999999999999822, 0.9200000000000000400 ),
 .UNSPECIFIED. ) 
 CURVE ( )  GEOMETRIC_REPRESENTATION_ITEM ( )  RATIONAL_B_SPLINE_CURVE ( ( 1.000000000000000000, 0.9238795325112869605, 1.000000000000000000, 0.9238795325112869605, 1.000000000000000000, 0.9238795325112869605, 1.000000000000000000, 0.9238795325112869605, 1.000000000000000000 ) ) 
 REPRESENTATION_ITEM ( '' )  ) ;
#8215 = EDGE_CURVE ( 'NONE', #15970, #41905, #30755, .T. ) ;
#8216 = CARTESIAN_POINT ( 'NONE',  ( 0.6971942568897637749, 2.189545951927499583E-17, 1.537893700733637736 ) ) ;
#8217 = CARTESIAN_POINT ( 'NONE',  ( 0.7495606340400177148, 0.1264236179284866091, 0.1550196849856066983 ) ) ;
#8218 = ( BOUNDED_CURVE ( )  B_SPLINE_CURVE ( 2, ( #41875, #8840, #19622, #9080, #23699, #38308, #5480, #20095, #34741 ),
 .UNSPECIFIED., .F., .F. ) 
 B_SPLINE_CURVE_WITH_KNOTS ( ( 3, 2, 2, 2, 3 ),
 ( 0.1300000000000000044, 0.1325000000000000067, 0.1350000000000000089, 0.1375000000000000111, 0.1400000000000000133 ),
 .UNSPECIFIED. ) 
 CURVE ( )  GEOMETRIC_REPRESENTATION_ITEM ( )  RATIONAL_B_SPLINE_CURVE ( ( 1.000000000000000000, 0.9238795325112869605, 1.000000000000000000, 0.9238795325112869605, 1.000000000000000000, 0.9238795325112869605, 1.000000000000000000, 0.9238795325112869605, 1.000000000000000000 ) ) 
 REPRESENTATION_ITEM ( '' )  ) ;
#8219 = EDGE_CURVE ( 'NONE', #5728, #26896, #34838, .T. ) ;
#8220 = CARTESIAN_POINT ( 'NONE',  ( 0.07405724077823318263, 0.1140492601172180265, 0.1787899950787401604 ) ) ;
#8221 = CARTESIAN_POINT ( 'NONE',  ( -0.1787899950787401882, -1.732775590497417362, 0.000000000000000000 ) ) ;
#8222 = DIRECTION ( 'NONE',  ( 1.000000000000000000, 0.000000000000000000, 0.000000000000000000 ) ) ;
#8223 = EDGE_CURVE ( 'NONE', #43350, #36523, #47061, .T. ) ;
#8224 = CARTESIAN_POINT ( 'NONE',  ( -1.054774247047244540, 0.07405724077823318263, 0.6594488188438737408 ) ) ;
#8226 = CARTESIAN_POINT ( 'NONE',  ( 0.9412147342319837628, 0.1574803149606300301, 0.3715551181102362266 ) ) ;
#8225 = CARTESIAN_POINT ( 'NONE',  ( 0.1574803149606300301, -0.6796259842519688510, 0.06523048226347956391 ) ) ;
#8227 = CARTESIAN_POINT ( 'NONE',  ( 0.1270800023317771588, -1.472484754464935097, -0.1270800023317771588 ) ) ;
#8228 = CYLINDRICAL_SURFACE ( 'NONE', #38623, 0.1574803149606299191 ) ;
#8229 = FACE_OUTER_BOUND ( 'NONE', #4023, .T. ) ;
#8230 = CARTESIAN_POINT ( 'NONE',  ( 0.7495606340400177148, -0.1264236179284866091, 1.390255905458047447 ) ) ;
#8231 = CARTESIAN_POINT ( 'NONE',  ( 0.7495606340400177148, -0.1264236179284866091, 1.779035433017102319 ) ) ;
#8232 = CARTESIAN_POINT ( 'NONE',  ( 1.054774247047244540, 0.07405724077823318263, 0.2608267715997797387 ) ) ;
#8234 = ORIENTED_EDGE ( 'NONE', *, *, #34815, .F. ) ;
#8233 = CARTESIAN_POINT ( 'NONE',  ( -0.7646288533564489232, -0.1113553986120547346, 1.638779527451527551 ) ) ;
#8235 = DIRECTION ( 'NONE',  ( 0.000000000000000000, -0.7880107536067215701, 0.6156614753256588468 ) ) ;
#8236 = DIRECTION ( 'NONE',  ( 0.000000000000000000, 0.7880107536067200158, -0.6156614753256607342 ) ) ;
#8237 = LINE ( 'NONE', #22628, #25525 ) ;
#8238 = CARTESIAN_POINT ( 'NONE',  ( 0.3849708276051176936, 4.766607801171850497E-17, 0.000000000000000000 ) ) ;
#8239 = CARTESIAN_POINT ( 'NONE',  ( 0.6971942568897626646, 0.07405724077823318263, 0.2755905511273391006 ) ) ;
#8240 = CARTESIAN_POINT ( 'NONE',  ( 0.7480772688632181255, -0.1073106677863766983, 0.03937439283920037697 ) ) ;
#8242 = CARTESIAN_POINT ( 'NONE',  ( -1.002407869896990045, -0.1264236179284866091, 1.990649606245448844 ) ) ;
#8241 = CARTESIAN_POINT ( 'NONE',  ( 1.054774247047244540, 0.07405724077823318263, 1.245078740103716886 ) ) ;
#8243 = CARTESIAN_POINT ( 'NONE',  ( -1.033464566929133799, 0.000000000000000000, 1.338582677057826853 ) ) ;
#8244 = VECTOR ( 'NONE', #3216, 39.37007874015748143 ) ;
#8245 = CARTESIAN_POINT ( 'NONE',  ( -0.8107537697050254399, 0.1574803149606300301, 0.9571850392625507187 ) ) ;
#8246 = CARTESIAN_POINT ( 'NONE',  ( 0.9412147342319837628, -0.1574803149606297803, 0.6225393699712132856 ) ) ;
#8247 = ORIENTED_EDGE ( 'NONE', *, *, #15074, .T. ) ;
#8248 = CARTESIAN_POINT ( 'NONE',  ( 0.9412147342319837628, 0.1574803149606300301, 1.395177165354331672 ) ) ;
#8249 = CARTESIAN_POINT ( 'NONE',  ( 0.2559055118110236116, 0.1477471161312045311, -0.1122047244094488277 ) ) ;
#8250 = ORIENTED_EDGE ( 'NONE', *, *, #19908, .T. ) ;
#8251 = CARTESIAN_POINT ( 'NONE',  ( -0.1797182628040039087, -0.08222884895312435050, -0.07444174185955065859 ) ) ;
#8252 = CARTESIAN_POINT ( 'NONE',  ( -0.1787899950787401882, -1.225885826717889815, 0.000000000000000000 ) ) ;
#8253 = DIRECTION ( 'NONE',  ( -0.000000000000000000, 0.7829934116339072325, 0.6220299971367095893 ) ) ;
#8254 = CARTESIAN_POINT ( 'NONE',  ( 0.6971942568897637749, 2.189545951927499583E-17, 1.616633858213952779 ) ) ;
#8255 = CARTESIAN_POINT ( 'NONE',  ( -0.7185039370078739607, 1.928577636452523993E-17, 1.250000000000000000 ) ) ;
#8256 = CARTESIAN_POINT ( 'NONE',  ( -0.4620708661417322616, 0.9842519685039375910, -0.7135826771653542844 ) ) ;
#8258 = CARTESIAN_POINT ( 'NONE',  ( 0.1602931993194442739, 0.07955613945526338049, -0.1377952755905511861 ) ) ;
#8257 = CARTESIAN_POINT ( 'NONE',  ( -0.1113553986120547346, 0.04625984251968504046, -0.1113553986120547346 ) ) ;
#8259 = CARTESIAN_POINT ( 'NONE',  ( 0.8759842519685039353, -0.1574803149606299191, 1.919291338475149544 ) ) ;
#8260 = ORIENTED_EDGE ( 'NONE', *, *, #22232, .T. ) ;
#8261 = VECTOR ( 'NONE', #32210, 39.37007874015748143 ) ;
#8262 = FACE_OUTER_BOUND ( 'NONE', #7678, .T. ) ;
#8263 = ORIENTED_EDGE ( 'NONE', *, *, #20409, .F. ) ;
#8264 = CARTESIAN_POINT ( 'NONE',  ( 1.002407869896990045, 0.1264236179284866091, 0.9374999999462362288 ) ) ;
#8265 = CARTESIAN_POINT ( 'NONE',  ( 2.892866454678787531E-17, -0.08661417312081949593, 0.1574803149606299191 ) ) ;
#8266 = CARTESIAN_POINT ( 'NONE',  ( -0.8759842519685039353, -0.1787899950787401882, 1.316437007820252081 ) ) ;
#8267 = ORIENTED_EDGE ( 'NONE', *, *, #30354, .T. ) ;
#8268 = CARTESIAN_POINT ( 'NONE',  ( -0.8019270111902717657, 0.1787899950787401604, 0.3543307086076538659 ) ) ;
#8269 = CARTESIAN_POINT ( 'NONE',  ( 1.033464566929133799, 1.928577636452524610E-17, 4.498031496062992574 ) ) ;
#8270 = CARTESIAN_POINT ( 'NONE',  ( -0.7185039370078766252, -0.06523048226348168721, 1.872539369971213619 ) ) ;
#8271 = CARTESIAN_POINT ( 'NONE',  ( -0.1787899950787401604, -0.9637066453945932754, -0.07405724077823318263 ) ) ;
#8272 = ORIENTED_EDGE ( 'NONE', *, *, #20714, .F. ) ;
#8273 = CARTESIAN_POINT ( 'NONE',  ( 0.1264236179284866091, 0.01427165359707059308, 0.1264236179284866091 ) ) ;
#8274 = ORIENTED_EDGE ( 'NONE', *, *, #16350, .T. ) ;
#8275 = CARTESIAN_POINT ( 'NONE',  ( 0.005667817494309996054, -0.05302691243377098684, 0.1377926283226260096 ) ) ;
#8276 = DIRECTION ( 'NONE',  ( 0.000000000000000000, 0.000000000000000000, 1.000000000000000000 ) ) ;
#8277 = EDGE_CURVE ( 'NONE', #31032, #16139, #13244, .T. ) ;
#8278 = AXIS2_PLACEMENT_3D ( 'NONE', #43532, #6405, #21017 ) ;
#8279 = CARTESIAN_POINT ( 'NONE',  ( 0.8107537697050254399, 0.1574803149606300301, 1.823326771546017078 ) ) ;
#8280 = CARTESIAN_POINT ( 'NONE',  ( -0.1787899950787401604, -0.5147637794737950356, 0.07405724077823318263 ) ) ;
#8281 = VECTOR ( 'NONE', #12721, 39.37007874015748143 ) ;
#8282 = CARTESIAN_POINT ( 'NONE',  ( -0.9500414927467377701, -0.1787899950787401604, 0.2559055117572600624 ) ) ;
#8283 = CARTESIAN_POINT ( 'NONE',  ( -1.033464566929133799, 0.000000000000000000, 0.8366141732283465249 ) ) ;
#8284 = CARTESIAN_POINT ( 'NONE',  ( 0.07444174185955065859, -1.012346959189344808, 0.1797182628040039087 ) ) ;
#8285 = CARTESIAN_POINT ( 'NONE',  ( 0.8107537697050254399, -0.1574803149606297803, 1.099901574803150650 ) ) ;
#8286 = CARTESIAN_POINT ( 'NONE',  ( -0.7185039370078746268, 0.06523048226347956391, 1.552657480207433993 ) ) ;
#8287 = CARTESIAN_POINT ( 'NONE',  ( 1.054774247047244540, -0.07405724077823318263, 0.8907480314422986378 ) ) ;
#8288 = CARTESIAN_POINT ( 'NONE',  ( -0.7185039370078746268, 0.06523048226347956391, 0.4601377952755902889 ) ) ;
#8290 = DIRECTION ( 'NONE',  ( 0.000000000000000000, -0.8660254037844384856, 0.5000000000000003331 ) ) ;
#8289 = CARTESIAN_POINT ( 'NONE',  ( 0.7342868310752559413, 0.08092158428113763180, 1.981631876916298163 ) ) ;
#8291 = CARTESIAN_POINT ( 'NONE',  ( 0.4620708661417338714, 0.4133858267716533641, 0.9891732283464566011 ) ) ;
#8292 = CARTESIAN_POINT ( 'NONE',  ( -1.033464566929134687, 0.06523048226347956391, 1.547736220472440305 ) ) ;
#8294 = DIRECTION ( 'NONE',  ( 1.000000000000000000, 0.000000000000000000, 0.000000000000000000 ) ) ;
#8293 = CARTESIAN_POINT ( 'NONE',  ( 0.9500414927467377701, 0.1787899950787401604, 0.8169291338045038264 ) ) ;
#8295 = CARTESIAN_POINT ( 'NONE',  ( 1.054774247047244540, -0.07405724077823318263, 1.835629921206078485 ) ) ;
#8296 = CARTESIAN_POINT ( 'NONE',  ( 0.1264236179284866091, -0.7632874015210393548, -0.1264236179284866091 ) ) ;
#8297 = ORIENTED_EDGE ( 'NONE', *, *, #46580, .T. ) ;
#8298 = CARTESIAN_POINT ( 'NONE',  ( 0.8759842519685039353, -0.1574803149606299191, 0.4232283463491653963 ) ) ;
#8299 = CARTESIAN_POINT ( 'NONE',  ( -0.7185039370078739607, 1.928577636452523993E-17, 0.1377952754830242266 ) ) ;
#8300 = CARTESIAN_POINT ( 'NONE',  ( 1.054774247047244540, 0.07405724077823318263, 1.205708661363558365 ) ) ;
#8301 = CARTESIAN_POINT ( 'NONE',  ( -0.7185039370078746268, 0.06523048226347956391, 1.050688976377951889 ) ) ;
#8302 = CARTESIAN_POINT ( 'NONE',  ( 0.06523048226347956391, -1.708169291338582418, 0.1574803149606297803 ) ) ;
#8303 = ADVANCED_FACE ( 'NONE', ( #40490 ), #3385, .T. ) ;
#8304 = DIRECTION ( 'NONE',  ( 0.000000000000000000, 0.000000000000000000, 1.000000000000000000 ) ) ;
#8305 = AXIS2_PLACEMENT_3D ( 'NONE', #44176, #28907, #29406 ) ;
#8306 = ORIENTED_EDGE ( 'NONE', *, *, #40190, .F. ) ;
#8307 = DIRECTION ( 'NONE',  ( 0.000000000000000000, 0.000000000000000000, 1.000000000000000000 ) ) ;
#8308 = CARTESIAN_POINT ( 'NONE',  ( -0.7495606340400177148, 0.1264236179284866091, 0.2731299212060791515 ) ) ;
#8309 = ORIENTED_EDGE ( 'NONE', *, *, #40209, .F. ) ;
#8310 = VERTEX_POINT ( 'NONE', #46986 ) ;
#8311 = CARTESIAN_POINT ( 'NONE',  ( -1.094772975963752103E-17, 0.1028543307624250058, -0.1787899950787401882 ) ) ;
#8313 = CARTESIAN_POINT ( 'NONE',  ( 0.1264236179284866091, -1.565452755851747924, 0.1264236179284866091 ) ) ;
#8312 = CARTESIAN_POINT ( 'NONE',  ( 0.1113553986120547346, -0.3474409447743626589, -0.1113553986120547346 ) ) ;
#8314 = CARTESIAN_POINT ( 'NONE',  ( -0.8759842519685039353, 0.1787899950787401882, 1.764271653489543290 ) ) ;
#8315 = CARTESIAN_POINT ( 'NONE',  ( -0.9500414927467377701, -0.1787899950787401604, 0.9596456692375763264 ) ) ;
#8316 = VECTOR ( 'NONE', #13814, 39.37007874015748143 ) ;
#8317 = CARTESIAN_POINT ( 'NONE',  ( -0.8759842519685039353, 0.1787899950787401882, 0.5487204723871811352 ) ) ;
#8318 = DIRECTION ( 'NONE',  ( 0.000000000000000000, -0.7880107536067207930, 0.6156614753256598460 ) ) ;
#8319 = DIRECTION ( 'NONE',  ( 0.000000000000000000, -1.000000000000000000, 0.000000000000000000 ) ) ;
#8320 = DIRECTION ( 'NONE',  ( -1.000000000000000000, -0.000000000000000000, 0.000000000000000000 ) ) ;
#8321 = CARTESIAN_POINT ( 'NONE',  ( -0.1787899950787401604, -0.6044546768906556844, 0.07405724077823318263 ) ) ;
#8322 = CARTESIAN_POINT ( 'NONE',  ( -0.2379558572308452802, -0.08955967549845886277, -0.02966404366025586839 ) ) ;
#8323 = CARTESIAN_POINT ( 'NONE',  ( -0.7185039370078739607, 1.928577636452523993E-17, 1.909448818790110192 ) ) ;
#8324 = CARTESIAN_POINT ( 'NONE',  ( 0.9873396505805591694, -0.1113553986120547346, 1.934055118110236338 ) ) ;
#8325 = EDGE_CURVE ( 'NONE', #649, #29529, #26428, .T. ) ;
#8326 = EDGE_CURVE ( 'NONE', #39783, #20308, #41670, .T. ) ;
#8327 = CARTESIAN_POINT ( 'NONE',  ( 0.2559052849838401866, -0.08677120797266399399, -0.05804865129189421685 ) ) ;
#8328 = CARTESIAN_POINT ( 'NONE',  ( -1.002407869896990045, 0.1264236179284866091, 0.4601377952218267953 ) ) ;
#8329 = ( BOUNDED_CURVE ( )  B_SPLINE_CURVE ( 2, ( #44708, #27031, #29701, #44245, #26550, #44475, #41109, #8301, #37542 ),
 .UNSPECIFIED., .F., .T. ) 
 B_SPLINE_CURVE_WITH_KNOTS ( ( 3, 2, 2, 2, 3 ),
 ( 0.5200000000000000178, 0.5224999999999999645, 0.5250000000000000222, 0.5274999999999999689, 0.5300000000000000266 ),
 .UNSPECIFIED. ) 
 CURVE ( )  GEOMETRIC_REPRESENTATION_ITEM ( )  RATIONAL_B_SPLINE_CURVE ( ( 1.000000000000000000, 0.9238795325112869605, 1.000000000000000000, 0.9238795325112869605, 1.000000000000000000, 0.9238795325112869605, 1.000000000000000000, 0.9238795325112869605, 1.000000000000000000 ) ) 
 REPRESENTATION_ITEM ( '' )  ) ;
#8330 = LINE ( 'NONE', #38046, #9620 ) ;
#8331 = EDGE_CURVE ( 'NONE', #35982, #28497, #21673, .T. ) ;
#8332 = EDGE_LOOP ( 'NONE', ( #7283, #23510, #23532, #30825 ) ) ;
#8333 = DIRECTION ( 'NONE',  ( 0.000000000000000000, 0.000000000000000000, 1.000000000000000000 ) ) ;
#8334 = CARTESIAN_POINT ( 'NONE',  ( -0.9500414927467377701, -0.1787899950787401604, 1.515748031442299526 ) ) ;
#8335 = ORIENTED_EDGE ( 'NONE', *, *, #43402, .F. ) ;
#8336 = EDGE_CURVE ( 'NONE', #39972, #13132, #18470, .T. ) ;
#8337 = CARTESIAN_POINT ( 'NONE',  ( 0.1264236179284866091, -1.319389763725763665, -0.1264236179284866091 ) ) ;
#8338 = CARTESIAN_POINT ( 'NONE',  ( -0.1787899950787401882, -1.496555118056472677, 0.000000000000000000 ) ) ;
#8339 = CONICAL_SURFACE ( 'NONE', #33623, 0.1574803149606299191, 0.9599310885968735940 ) ;
#8340 = CARTESIAN_POINT ( 'NONE',  ( 0.1555687797274982465, 0.1458529223346498038, 0.02296587926509188748 ) ) ;
#8341 = DIRECTION ( 'NONE',  ( -0.8191520442890001252, 0.000000000000000000, -0.5735764363510340580 ) ) ;
#8342 = CARTESIAN_POINT ( 'NONE',  ( -0.9873396505805591694, 0.1113553986120547346, 1.067913385719243990 ) ) ;
#8343 = AXIS2_PLACEMENT_3D ( 'NONE', #13965, #43413, #10622 ) ;
#8344 = CARTESIAN_POINT ( 'NONE',  ( 0.9500414927467378812, -0.1787899950787401604, 0.5314960629383620461 ) ) ;
#8345 = CARTESIAN_POINT ( 'NONE',  ( 0.7108038354695511707, 0.06841997037041733232, 0.03937007863263043694 ) ) ;
#8347 = LINE ( 'NONE', #15570, #4802 ) ;
#8346 = CARTESIAN_POINT ( 'NONE',  ( 0.06523048226347956391, -0.2908464566929132578, 0.1574803149606297803 ) ) ;
#8348 = CARTESIAN_POINT ( 'NONE',  ( 0.9873396505805591694, 0.1113553986120547346, 1.894685039262551163 ) ) ;
#8349 = ORIENTED_EDGE ( 'NONE', *, *, #10464, .T. ) ;
#8350 = CYLINDRICAL_SURFACE ( 'NONE', #42905, 0.009842519685039286675 ) ;
#8351 = CARTESIAN_POINT ( 'NONE',  ( 0.9873396505805591694, 0.1113553986120547346, 0.9202755905511811330 ) ) ;
#8352 = AXIS2_PLACEMENT_3D ( 'NONE', #47298, #14475, #11126 ) ;
#8353 = CARTESIAN_POINT ( 'NONE',  ( 0.000000000000000000, -0.09842519685039370636, 0.000000000000000000 ) ) ;
#8354 = CARTESIAN_POINT ( 'NONE',  ( -0.1574803149606297803, -0.5664370077664889758, 0.06523048226347956391 ) ) ;
#8355 = CARTESIAN_POINT ( 'NONE',  ( -0.5555748031496021699, 1.332209862199694284, -0.06082000038405668829 ) ) ;
#8356 = CARTESIAN_POINT ( 'NONE',  ( 0.8759842519685039353, 0.1574803149606299191, 1.269685039262551163 ) ) ;
#8357 = CARTESIAN_POINT ( 'NONE',  ( -0.1697987809117319224, -0.08954398017175399516, -0.008892717904794893158 ) ) ;
#8358 = VERTEX_POINT ( 'NONE', #246 ) ;
#8359 = AXIS2_PLACEMENT_3D ( 'NONE', #862, #3769, #4221 ) ;
#8360 = CARTESIAN_POINT ( 'NONE',  ( -0.2984108399384687305, 0.08463831125274398626, 1.020725522217017955 ) ) ;
#8361 = VERTEX_POINT ( 'NONE', #39556 ) ;
#8362 = CARTESIAN_POINT ( 'NONE',  ( -0.8107537697050254399, 0.1574803149606300301, 1.783956692805859001 ) ) ;
#8363 = CARTESIAN_POINT ( 'NONE',  ( -0.7646288533564489232, 0.1113553986120547346, 0.4478346455617645550 ) ) ;
#8364 = CARTESIAN_POINT ( 'NONE',  ( 0.1264236179284866091, -1.718011810969858333, 0.1264236179284866091 ) ) ;
#8365 = CARTESIAN_POINT ( 'NONE',  ( 0.1787899950787401604, -0.8494094487651332459, -0.07405724077823318263 ) ) ;
#8366 = CARTESIAN_POINT ( 'NONE',  ( 0.1574803149606300301, -1.191437007874017073, 0.06523048226347956391 ) ) ;
#8367 = CARTESIAN_POINT ( 'NONE',  ( 0.7646288533564489232, 0.1113553986120547346, 1.156496062884598608 ) ) ;
#8368 = DIRECTION ( 'NONE',  ( -1.000000000000000000, 0.000000000000000000, 0.000000000000000000 ) ) ;
#8369 = ORIENTED_EDGE ( 'NONE', *, *, #27138, .F. ) ;
#8370 = ORIENTED_EDGE ( 'NONE', *, *, #4801, .F. ) ;
#8371 = CARTESIAN_POINT ( 'NONE',  ( -0.7495606340400177148, -0.1264236179284866091, 1.744586614119464807 ) ) ;
#8372 = CARTESIAN_POINT ( 'NONE',  ( 0.9500414927467378812, -0.1787899950787401604, 1.751968503883245765 ) ) ;
#8373 = CARTESIAN_POINT ( 'NONE',  ( -0.03734157890107612371, -0.2739282660277941317, -0.3031249188863139321 ) ) ;
#8374 = CARTESIAN_POINT ( 'NONE',  ( -0.9500414927467378812, -0.1787899950787401604, 1.313976377898992132 ) ) ;
#8375 = CARTESIAN_POINT ( 'NONE',  ( -1.002407869896990045, 0.1264236179284866091, 1.208169291284818980 ) ) ;
#8376 = CARTESIAN_POINT ( 'NONE',  ( -0.8019270111902717657, -0.1787899950787401604, 0.9153543306548987957 ) ) ;
#8377 = CARTESIAN_POINT ( 'NONE',  ( -0.6971942568897626646, -0.07405724077823297447, 0.04921259837143338034 ) ) ;
#8378 = VECTOR ( 'NONE', #27140, 39.37007874015748854 ) ;
#8379 = CARTESIAN_POINT ( 'NONE',  ( 0.09216395708618058125, 0.09383642490574123363, 0.2322221854328543611 ) ) ;
#8380 = CARTESIAN_POINT ( 'NONE',  ( -0.8759842519685039353, -0.1787899950787401882, 1.552657480261196765 ) ) ;
#8381 = CARTESIAN_POINT ( 'NONE',  ( -0.8019270111902717657, 0.1787899950787401604, 0.1181102361667090567 ) ) ;
#8382 = CARTESIAN_POINT ( 'NONE',  ( -0.3690944881889761109, 0.1864803149606356070, -0.06082000038405686176 ) ) ;
#8383 = CARTESIAN_POINT ( 'NONE',  ( -0.1476377952755905387, 0.06851622550196635741, -0.1414889043096673460 ) ) ;
#8384 = EDGE_CURVE ( 'NONE', #46509, #9744, #31012, .T. ) ;
#8385 = CARTESIAN_POINT ( 'NONE',  ( 1.002407869896990045, 0.1264236179284866091, 1.606791338528913426 ) ) ;
#8386 = CARTESIAN_POINT ( 'NONE',  ( -0.1222548325031484334, -0.09842519685039370636, 0.1962412971452039412 ) ) ;
#8387 = DIRECTION ( 'NONE',  ( 1.000000000000000000, 0.000000000000000000, 0.000000000000000000 ) ) ;
#8388 = ORIENTED_EDGE ( 'NONE', *, *, #7280, .F. ) ;
#8389 = AXIS2_PLACEMENT_3D ( 'NONE', #10279, #39485, #46918 ) ;
#8390 = ADVANCED_FACE ( 'NONE', ( #29552 ), #11067, .T. ) ;
#8391 = VERTEX_POINT ( 'NONE', #10596 ) ;
#8392 = ORIENTED_EDGE ( 'NONE', *, *, #22082, .T. ) ;
#8393 = AXIS2_PLACEMENT_3D ( 'NONE', #11175, #33231, #26505 ) ;
#8394 = CARTESIAN_POINT ( 'NONE',  ( -0.6971942568897648851, 0.07405724077823318263, 1.186023621993481658 ) ) ;
#8395 = ORIENTED_EDGE ( 'NONE', *, *, #7886, .T. ) ;
#8396 = CARTESIAN_POINT ( 'NONE',  ( -0.1787899950787401604, -0.9478346456155283262, 0.07405724077823318263 ) ) ;
#8397 = CARTESIAN_POINT ( 'NONE',  ( -0.07405724077823318263, -1.056102362150961982, 0.1787899950787401604 ) ) ;
#8398 = EDGE_CURVE ( 'NONE', #8725, #46340, #21021, .T. ) ;
#8399 = PRODUCT_RELATED_PRODUCT_CATEGORY ( 'part', '', ( #5156 ) ) ;
#8400 = CARTESIAN_POINT ( 'NONE',  ( 1.033464566929133799, 0.000000000000000000, 0.6003937007874016185 ) ) ;
#8401 = CARTESIAN_POINT ( 'NONE',  ( -0.1113553986120547346, 0.1250000000000000000, -0.1113553986120547346 ) ) ;
#8402 = CARTESIAN_POINT ( 'NONE',  ( 0.1264236179284866091, -0.1776574802611972648, -0.1264236179284866091 ) ) ;
#8403 = CARTESIAN_POINT ( 'NONE',  ( -0.7185039370078739607, 1.928577636452523993E-17, 1.082677165246803241 ) ) ;
#8404 = CARTESIAN_POINT ( 'NONE',  ( 0.8019270111902717657, 0.1787899950787401604, 0.7037401574265510495 ) ) ;
#8405 = VECTOR ( 'NONE', #406, 39.37007874015748854 ) ;
#8406 = CYLINDRICAL_SURFACE ( 'NONE', #40708, 0.1574803149606299191 ) ;
#8407 = CARTESIAN_POINT ( 'NONE',  ( -1.033464566929133799, 0.000000000000000000, 1.259842519577511810 ) ) ;
#8408 = CARTESIAN_POINT ( 'NONE',  ( -6.728203135043436585E-17, -8.878505979408855953E-16, -0.4940944881889759444 ) ) ;
#8409 = CARTESIAN_POINT ( 'NONE',  ( 1.054774247047244096, 0.000000000000000000, 1.798720472387181024 ) ) ;
#8410 = CARTESIAN_POINT ( 'NONE',  ( 0.8759842519685039353, -0.1574803149606299191, 0.1574803149606299191 ) ) ;
#8411 = LINE ( 'NONE', #4813, #12236 ) ;
#8412 = CARTESIAN_POINT ( 'NONE',  ( -0.1264236179284866091, -0.3941929133320630219, 0.1264236179284866091 ) ) ;
#8413 = CARTESIAN_POINT ( 'NONE',  ( 1.054774247047244096, 0.000000000000000000, 1.990649606245448844 ) ) ;
#8414 = CARTESIAN_POINT ( 'NONE',  ( 3.284318927891251994E-17, -1.211122047190330786, 0.1787899950787401882 ) ) ;
#8415 = CARTESIAN_POINT ( 'NONE',  ( 0.8019270111902717657, 0.1787899950787401604, 0.1968503936470238913 ) ) ;
#8416 = CARTESIAN_POINT ( 'NONE',  ( -1.054774247047244540, -0.07405724077823318263, 1.791338582623401177 ) ) ;
#8417 = ORIENTED_EDGE ( 'NONE', *, *, #28893, .F. ) ;
#8418 = ORIENTED_EDGE ( 'NONE', *, *, #25778, .F. ) ;
#8419 = CARTESIAN_POINT ( 'NONE',  ( -1.054774247047244096, 0.000000000000000000, 1.247539370024976391 ) ) ;
#8420 = CARTESIAN_POINT ( 'NONE',  ( -1.054774247047244540, -0.07405724077823318263, 0.5364173227808821665 ) ) ;
#8421 = CARTESIAN_POINT ( 'NONE',  ( 0.9500414927467378812, 0.1787899950787401604, 1.958661417269071947 ) ) ;
#8422 = CARTESIAN_POINT ( 'NONE',  ( -0.8019270111902717657, -0.1787899950787401604, 1.151574803095843036 ) ) ;
#8423 = EDGE_CURVE ( 'NONE', #29301, #5246, #44713, .T. ) ;
#8424 = CARTESIAN_POINT ( 'NONE',  ( 0.8107537697050254399, -0.1574803149606297803, 0.6569881888688504645 ) ) ;
#8425 = CARTESIAN_POINT ( 'NONE',  ( 0.02009753640170339889, -0.09839439123163033762, -0.1777236764612983022 ) ) ;
#8426 = CARTESIAN_POINT ( 'NONE',  ( -0.8759842519685039353, 0.000000000000000000, 0.000000000000000000 ) ) ;
#8427 = CARTESIAN_POINT ( 'NONE',  ( 0.8019270111902716547, 0.1787899950787401604, 0.5118110235682844511 ) ) ;
#8428 = CARTESIAN_POINT ( 'NONE',  ( -0.6971942568897637749, 2.189545951927499583E-17, 0.4355314960092284138 ) ) ;
#8429 = ORIENTED_EDGE ( 'NONE', *, *, #21536, .T. ) ;
#8430 = FACE_OUTER_BOUND ( 'NONE', #41982, .T. ) ;
#8431 = ORIENTED_EDGE ( 'NONE', *, *, #47080, .F. ) ;
#8432 = ORIENTED_EDGE ( 'NONE', *, *, #42070, .F. ) ;
#8433 = CARTESIAN_POINT ( 'NONE',  ( 1.054774247047244096, 0.000000000000000000, 0.9325787401037164415 ) ) ;
#8434 = CARTESIAN_POINT ( 'NONE',  ( -0.7185039370078746268, 0.06523048226347956391, 0.06643700787401589369 ) ) ;
#8435 = EDGE_CURVE ( 'NONE', #460, #11565, #1788, .T. ) ;
#8436 = CARTESIAN_POINT ( 'NONE',  ( 1.033464566929133799, 0.000000000000000000, 0.7086614172153071767 ) ) ;
#8437 = CARTESIAN_POINT ( 'NONE',  ( 0.8107537697050254399, 0.1574803149606300301, 1.311515747923968744 ) ) ;
#8438 = ORIENTED_EDGE ( 'NONE', *, *, #18015, .T. ) ;
#8439 = CARTESIAN_POINT ( 'NONE',  ( -0.9412147342319837628, -0.1574803149606297803, 1.301673228346455602 ) ) ;
#8440 = AXIS2_PLACEMENT_3D ( 'NONE', #31480, #39108, #6757 ) ;
#8441 = FACE_OUTER_BOUND ( 'NONE', #9696, .T. ) ;
#8442 = CARTESIAN_POINT ( 'NONE',  ( 0.4736248074375795647, 1.205832402325950792, -1.129708666049259902 ) ) ;
#8443 = CARTESIAN_POINT ( 'NONE',  ( 0.07405724077823318263, -1.485360188701679629, -0.1787899950787401604 ) ) ;
#8444 = ORIENTED_EDGE ( 'NONE', *, *, #5186, .F. ) ;
#8445 = CARTESIAN_POINT ( 'NONE',  ( -0.07405724077823318263, -0.4803149605761579677, -0.1787899950787401604 ) ) ;
#8446 = DIRECTION ( 'NONE',  ( 0.000000000000000000, 0.7880107536067221252, -0.6156614753256580697 ) ) ;
#8447 = VERTEX_POINT ( 'NONE', #32881 ) ;
#8448 = AXIS2_PLACEMENT_3D ( 'NONE', #2223, #41983, #20909 ) ;
#8449 = CARTESIAN_POINT ( 'NONE',  ( 0.7185039370078746268, 0.06523048226347956391, 1.601870078740158077 ) ) ;
#8450 = CIRCLE ( 'NONE', #45174, 0.1574803149606299191 ) ;
#8451 = CARTESIAN_POINT ( 'NONE',  ( -0.2066929133858267931, -0.2237541348899642346, -1.272196386806234925 ) ) ;
#8452 = CARTESIAN_POINT ( 'NONE',  ( 1.054774247047244096, 0.000000000000000000, 1.557578740103716441 ) ) ;
#8453 = CARTESIAN_POINT ( 'NONE',  ( 1.054774247047244096, 0.000000000000000000, 0.1008858267178899676 ) ) ;
#8454 = CARTESIAN_POINT ( 'NONE',  ( -0.07405724077823318263, -1.809055118056471123, 0.1787899950787401604 ) ) ;
#8455 = CARTESIAN_POINT ( 'NONE',  ( -0.1787899950787401882, 0.1126968504474643862, 0.000000000000000000 ) ) ;
#8456 = APPLICATION_PROTOCOL_DEFINITION ( 'draft international standard', 'automotive_design', 1998, #1229 ) ;
#8457 = CARTESIAN_POINT ( 'NONE',  ( 0.7185039370078739607, 1.928577636452523993E-17, 1.948818897530267602 ) ) ;
#8458 = CARTESIAN_POINT ( 'NONE',  ( -0.6971942568897648851, -0.07405724077823297447, 0.6003937007336389575 ) ) ;
#8460 = DIRECTION ( 'NONE',  ( -0.7986355100472960489, 0.000000000000000000, 0.6018150231520440485 ) ) ;
#8459 = CARTESIAN_POINT ( 'NONE',  ( -0.06523048226347956391, -0.6894685039370073154, 0.1574803149606297803 ) ) ;
#8461 = CARTESIAN_POINT ( 'NONE',  ( 0.07444174185955065859, -1.484787904071234843, 0.1797182628040039087 ) ) ;
#8462 = CARTESIAN_POINT ( 'NONE',  ( 0.1184675242425285574, -0.5708661417322835607, 1.224299699984021661 ) ) ;
#8463 = CARTESIAN_POINT ( 'NONE',  ( 0.1574803149606300301, -0.4335629920184572161, 0.06523048226347956391 ) ) ;
#8464 = DIRECTION ( 'NONE',  ( 1.000000000000000000, 0.000000000000000000, 0.000000000000000000 ) ) ;
#8465 = CARTESIAN_POINT ( 'NONE',  ( 0.6971942568897648851, 0.07405724077823318263, 1.343503936954111744 ) ) ;
#8466 = CARTESIAN_POINT ( 'NONE',  ( 1.054774247047244096, 0.000000000000000000, 1.833169291284818758 ) ) ;
#8467 = CARTESIAN_POINT ( 'NONE',  ( 0.8759842519685039353, -0.1787899950787401882, 0.2878937007336381804 ) ) ;
#8469 = VERTEX_POINT ( 'NONE', #36929 ) ;
#8468 = CARTESIAN_POINT ( 'NONE',  ( 0.8759842519685039353, 0.000000000000000000, 4.498031496062992574 ) ) ;
#8470 = CARTESIAN_POINT ( 'NONE',  ( -0.9412147342319837628, 0.1574803149606300301, 1.513287401574803681 ) ) ;
#8471 = DIRECTION ( 'NONE',  ( 0.000000000000000000, 0.000000000000000000, -1.000000000000000000 ) ) ;
#8472 = CARTESIAN_POINT ( 'NONE',  ( 0.1787899950787401604, -0.02263779522182706935, -0.07405724077823318263 ) ) ;
#8473 = CARTESIAN_POINT ( 'NONE',  ( 0.8759842519685039353, -0.1787899950787401882, 0.3272637794737956463 ) ) ;
#8474 = CARTESIAN_POINT ( 'NONE',  ( 0.2395294000716133853, 0.1968503937007874127, -0.4921259842519685179 ) ) ;
#8475 = CIRCLE ( 'NONE', #33010, 0.1864803149606299171 ) ;
#8476 = DIRECTION ( 'NONE',  ( 0.000000000000000000, -0.7880107536067184615, 0.6156614753256628436 ) ) ;
#8477 = CARTESIAN_POINT ( 'NONE',  ( 1.033464566929134687, 0.06523048226347956391, 0.8390748031496062520 ) ) ;
#8478 = CARTESIAN_POINT ( 'NONE',  ( -0.9412147342319837628, 0.1574803149606300301, 0.9522637794200313754 ) ) ;
#8479 = CARTESIAN_POINT ( 'NONE',  ( -0.6971942568897637749, 2.189545951927499583E-17, 1.301673228292692830 ) ) ;
#8480 = CARTESIAN_POINT ( 'NONE',  ( 0.7185039370078746268, 0.06523048226347956391, 0.8439960628845977197 ) ) ;
#8481 = EDGE_LOOP ( 'NONE', ( #25324, #21341, #648, #44306, #43812 ) ) ;
#8482 = CARTESIAN_POINT ( 'NONE',  ( -0.1699495073158193426, -0.4341647314679547565, -0.9728045006378999160 ) ) ;
#8483 = ORIENTED_EDGE ( 'NONE', *, *, #21818, .T. ) ;
#8484 = CARTESIAN_POINT ( 'NONE',  ( -0.1270800023317771588, 0.003893198290970204586, 0.1270800023317771588 ) ) ;
#8485 = CARTESIAN_POINT ( 'NONE',  ( -0.1264236179284866091, -1.270177165300566902, -0.1264236179284866091 ) ) ;
#8486 = CARTESIAN_POINT ( 'NONE',  ( -0.9873396505805591694, -0.1113553986120547346, 1.225393700787401619 ) ) ;
#8487 = CARTESIAN_POINT ( 'NONE',  ( 0.8759842519685039353, 0.1787899950787401882, 1.606791338528913426 ) ) ;
#8488 = CARTESIAN_POINT ( 'NONE',  ( -0.9412147342319837628, -0.1574803149606297803, 1.183562992125983593 ) ) ;
#8489 = ADVANCED_FACE ( 'NONE', ( #4081 ), #28823, .F. ) ;
#8490 = CARTESIAN_POINT ( 'NONE',  ( 0.8759842519685039353, 0.1574803149606299191, 0.5708661417322835607 ) ) ;
#8492 = DIRECTION ( 'NONE',  ( 2.055777091826793380E-15, 0.6220299971367094782, -0.7829934116339072325 ) ) ;
#8491 = CARTESIAN_POINT ( 'NONE',  ( -0.3980944881889759146, 0.2597269656108969760, 0.5511811023622046335 ) ) ;
#8493 = CARTESIAN_POINT ( 'NONE',  ( 0.7495606340400177148, 0.1264236179284866091, 0.04183070860765386589 ) ) ;
#8494 = AXIS2_PLACEMENT_3D ( 'NONE', #24924, #21803, #3584 ) ;
#8495 = VERTEX_POINT ( 'NONE', #1785 ) ;
#8496 = ADVANCED_FACE ( 'NONE', ( #14647 ), #43866, .T. ) ;
#8497 = CARTESIAN_POINT ( 'NONE',  ( -0.08995663987708611697, -0.09317336072452847562, -0.2334965874938852715 ) ) ;
#8498 = EDGE_CURVE ( 'NONE', #42416, #16713, #45273, .T. ) ;
#8499 = CARTESIAN_POINT ( 'NONE',  ( 0.9500414927467377701, -0.1787899950787401604, 0.9645669290800954476 ) ) ;
#8500 = CARTESIAN_POINT ( 'NONE',  ( -1.054774247047244540, -0.07405724077823318263, 1.555118110182457158 ) ) ;
#8501 = CARTESIAN_POINT ( 'NONE',  ( -0.1113553986120547346, -0.09153543296333917223, 0.1113553986120547346 ) ) ;
#8502 = CARTESIAN_POINT ( 'NONE',  ( -0.6971942568897637749, 2.189545951927499583E-17, 1.306594488135212728 ) ) ;
#8503 = ORIENTED_EDGE ( 'NONE', *, *, #30299, .T. ) ;
#8504 = EDGE_CURVE ( 'NONE', #1531, #10984, #11890, .T. ) ;
#8505 = ( BOUNDED_CURVE ( )  B_SPLINE_CURVE ( 2, ( #37811, #4724, #41596, #11711, #4964, #30189, #19591, #12178, #19348 ),
 .UNSPECIFIED., .F., .T. ) 
 B_SPLINE_CURVE_WITH_KNOTS ( ( 3, 2, 2, 2, 3 ),
 ( 0.04499999999999999833, 0.04750000000000000056, 0.05000000000000000278, 0.05249999999999999806, 0.05500000000000000028 ),
 .UNSPECIFIED. ) 
 CURVE ( )  GEOMETRIC_REPRESENTATION_ITEM ( )  RATIONAL_B_SPLINE_CURVE ( ( 1.000000000000000000, 0.9238795325112869605, 1.000000000000000000, 0.9238795325112869605, 1.000000000000000000, 0.9238795325112869605, 1.000000000000000000, 0.9238795325112869605, 1.000000000000000000 ) ) 
 REPRESENTATION_ITEM ( '' )  ) ;
#8506 = CARTESIAN_POINT ( 'NONE',  ( -1.033464566929134687, 0.06523048226347956391, 0.2386811022546777294 ) ) ;
#8507 = FACE_OUTER_BOUND ( 'NONE', #29134, .T. ) ;
#8508 = CARTESIAN_POINT ( 'NONE',  ( 0.3161444924769519216, 0.9382165298418937427, -1.070508272602716637 ) ) ;
#8509 = CARTESIAN_POINT ( 'NONE',  ( -0.1787899950787401604, -0.9981554642922296772, 0.07405724077823318263 ) ) ;
#8510 = ORIENTED_EDGE ( 'NONE', *, *, #37835, .T. ) ;
#8511 = CARTESIAN_POINT ( 'NONE',  ( -0.07405724077823318263, 0.03149606304588949135, -0.1787899950787401604 ) ) ;
#8512 = VERTEX_POINT ( 'NONE', #8626 ) ;
#8513 = ORIENTED_EDGE ( 'NONE', *, *, #26090, .T. ) ;
#8514 = CARTESIAN_POINT ( 'NONE',  ( -0.9412147342319837628, -0.1574803149606297803, 0.2682086613097955929 ) ) ;
#8515 = FACE_OUTER_BOUND ( 'NONE', #31429, .T. ) ;
#8516 = AXIS2_PLACEMENT_3D ( 'NONE', #37232, #26709, #30787 ) ;
#8517 = CARTESIAN_POINT ( 'NONE',  ( 0.7646288533564489232, 0.1113553986120547346, 1.825787401467275473 ) ) ;
#8518 = AXIS2_PLACEMENT_3D ( 'NONE', #584, #8024, #44202 ) ;
#8519 = CARTESIAN_POINT ( 'NONE',  ( 0.1787899950787401882, -0.6943897637257637756, -2.189545951927503898E-17 ) ) ;
#8520 = AXIS2_PLACEMENT_3D ( 'NONE', #24172, #34958, #42355 ) ;
#8521 = CARTESIAN_POINT ( 'NONE',  ( -1.054774247047244096, 0.000000000000000000, 0.1451771653005673179 ) ) ;
#8522 = CARTESIAN_POINT ( 'NONE',  ( -0.7185039370078739607, 1.928577636452523993E-17, 0.8562992125984251190 ) ) ;
#8523 = CARTESIAN_POINT ( 'NONE',  ( -0.07444174185955065859, -0.9385280615515501079, 0.1797182628040039087 ) ) ;
#8524 = DIRECTION ( 'NONE',  ( 0.000000000000000000, -1.000000000000000000, 0.000000000000000000 ) ) ;
#8525 = CARTESIAN_POINT ( 'NONE',  ( 0.8019270111902717657, -0.1787899950787401604, 0.9990157479777320715 ) ) ;
#8526 = DIRECTION ( 'NONE',  ( 0.000000000000000000, 0.000000000000000000, 1.000000000000000000 ) ) ;
#8527 = CARTESIAN_POINT ( 'NONE',  ( 1.033464566929134687, -0.06523048226347956391, 1.542814960629920851 ) ) ;
#8528 = EDGE_CURVE ( 'NONE', #19795, #17892, #29962, .T. ) ;
#8530 = CARTESIAN_POINT ( 'NONE',  ( -0.1387979473505290273, -0.2153574986361826149, -0.3148284977848752053 ) ) ;
#8529 = CARTESIAN_POINT ( 'NONE',  ( 0.7204945029520213318, 0.05328764782798792871, 1.982238686896746094 ) ) ;
#8531 = CYLINDRICAL_SURFACE ( 'NONE', #17474, 0.1574803149606299191 ) ;
#8532 = CARTESIAN_POINT ( 'NONE',  ( -0.07405724077823318263, 0.07086614178604697112, -0.1787899950787401604 ) ) ;
#8533 = DIRECTION ( 'NONE',  ( -1.000000000000000000, -0.000000000000000000, 0.000000000000000000 ) ) ;
#8534 = CARTESIAN_POINT ( 'NONE',  ( 0.8019270111902716547, -0.1787899950787401604, 0.9940944881352130613 ) ) ;
#8535 = CARTESIAN_POINT ( 'NONE',  ( 0.7495606340400177148, -0.1264236179284866091, 1.823326771599779406 ) ) ;
#8536 = CARTESIAN_POINT ( 'NONE',  ( -0.07405724077823318263, -0.9773622046706458288, 0.1787899950787401604 ) ) ;
#8537 = VERTEX_POINT ( 'NONE', #44559 ) ;
#8538 = PLANE ( 'NONE',  #12311 ) ;
#8539 = CARTESIAN_POINT ( 'NONE',  ( -0.02900000000000056352, 1.086379535891625059, -0.03715491745705514631 ) ) ;
#8540 = CARTESIAN_POINT ( 'NONE',  ( -0.1574803149606299191, -1.710629921152315047, 0.000000000000000000 ) ) ;
#8541 = DIRECTION ( 'NONE',  ( 1.000000000000000000, 0.000000000000000000, 0.000000000000000000 ) ) ;
#8542 = FACE_OUTER_BOUND ( 'NONE', #39707, .T. ) ;
#8543 = CARTESIAN_POINT ( 'NONE',  ( 0.8759842519685039353, 0.1787899950787401882, 1.134350393647023614 ) ) ;
#8544 = CARTESIAN_POINT ( 'NONE',  ( -0.7185039370078739607, 1.928577636452523993E-17, 1.171259842519684957 ) ) ;
#8545 = CARTESIAN_POINT ( 'NONE',  ( -0.06523048226347956391, -1.752460629921259505, 0.1574803149606297803 ) ) ;
#8546 = CARTESIAN_POINT ( 'NONE',  ( 1.181102362204724310, -0.3937007874015748254, 0.9842519685039370358 ) ) ;
#8547 = ADVANCED_FACE ( 'NONE', ( #5032 ), #11135, .T. ) ;
#8548 = VECTOR ( 'NONE', #1103, 39.37007874015748143 ) ;
#8549 = CARTESIAN_POINT ( 'NONE',  ( -0.6971942568897626646, -0.07405724077823297447, 0.2017716534895435399 ) ) ;
#8550 = VERTEX_POINT ( 'NONE', #38106 ) ;
#8551 = CARTESIAN_POINT ( 'NONE',  ( -0.1787899950787401604, -1.499015747977732627, 0.07405724077823318263 ) ) ;
#8552 = AXIS2_PLACEMENT_3D ( 'NONE', #39561, #7224, #32888 ) ;
#8553 = AXIS2_PLACEMENT_3D ( 'NONE', #43303, #40170, #14562 ) ;
#8554 = CARTESIAN_POINT ( 'NONE',  ( -1.002407869896990045, -0.1264236179284866091, 1.867618110182456714 ) ) ;
#8555 = CARTESIAN_POINT ( 'NONE',  ( -0.7495606340400177148, 0.1264236179284866091, 0.9424212597887559051 ) ) ;
#8556 = EDGE_CURVE ( 'NONE', #11697, #9878, #36385, .T. ) ;
#8557 = CARTESIAN_POINT ( 'NONE',  ( -1.054774247047244540, -0.07405724077823318263, 0.4970472440407249226 ) ) ;
#8558 = DIRECTION ( 'NONE',  ( -1.000000000000000000, 0.000000000000000000, 0.000000000000000000 ) ) ;
#8559 = FACE_OUTER_BOUND ( 'NONE', #22777, .T. ) ;
#8560 = LINE ( 'NONE', #38039, #32846 ) ;
#8561 = CARTESIAN_POINT ( 'NONE',  ( 0.1787899950787401882, -0.5478601887016795180, -2.189545951927503898E-17 ) ) ;
#8562 = CARTESIAN_POINT ( 'NONE',  ( -0.03314229022649078926, -0.08955993585198464280, 0.2197241657068637610 ) ) ;
#8563 = LINE ( 'NONE', #38275, #24910 ) ;
#8564 = LINE ( 'NONE', #37813, #20283 ) ;
#8565 = CYLINDRICAL_SURFACE ( 'NONE', #3501, 0.1574803149606299191 ) ;
#8566 = CARTESIAN_POINT ( 'NONE',  ( -0.8759842519685039353, -0.1787899950787401882, 0.4060039369541102450 ) ) ;
#8567 = CARTESIAN_POINT ( 'NONE',  ( 0.07405724077823318263, -1.800320818622939356, -0.1787899950787401604 ) ) ;
#8568 = VERTEX_POINT ( 'NONE', #37381 ) ;
#8569 = CARTESIAN_POINT ( 'NONE',  ( -0.6971942568897648851, -0.07405724077823297447, 1.466535433017102763 ) ) ;
#8570 = CARTESIAN_POINT ( 'NONE',  ( -0.1787899950787401604, -1.346456692859623550, -0.07405724077823318263 ) ) ;
#8571 = EDGE_CURVE ( 'NONE', #26504, #25961, #12011, .T. ) ;
#8572 = CARTESIAN_POINT ( 'NONE',  ( -0.1787899950787401604, -1.499015747977732627, -0.07405724077823318263 ) ) ;
#8573 = LENGTH_MEASURE_WITH_UNIT ( LENGTH_MEASURE( 0.02539999999999999897 ), #41373 ) ;
#8574 = CARTESIAN_POINT ( 'NONE',  ( 0.1611065205236515141, -0.07959249327126025064, 0.1378515872677678056 ) ) ;
#8575 = CARTESIAN_POINT ( 'NONE',  ( 0.9873396505805591694, 0.1113553986120547346, 0.4872047244094488416 ) ) ;
#8576 = DIRECTION ( 'NONE',  ( -1.000000000000000000, 0.000000000000000000, 0.000000000000000000 ) ) ;
#8577 = CARTESIAN_POINT ( 'NONE',  ( -0.7646288533564489232, 0.1113553986120547346, 1.077755905404283565 ) ) ;
#8578 = CARTESIAN_POINT ( 'NONE',  ( 1.002407869896990045, -0.1264236179284866091, 0.5733267715997795166 ) ) ;
#8580 = CARTESIAN_POINT ( 'NONE',  ( 0.000000000000000000, 0.000000000000000000, -0.1574803149606298636 ) ) ;
#8579 = CARTESIAN_POINT ( 'NONE',  ( -0.1113553986120547346, -0.3474409448818897572, -0.1113553986120547346 ) ) ;
#8581 = CIRCLE ( 'NONE', #24674, 0.1624015748031501782 ) ;
#8582 = CARTESIAN_POINT ( 'NONE',  ( 0.7185039370078746268, -0.06523048226347956391, 1.990649606191687404 ) ) ;
#8583 = ORIENTED_EDGE ( 'NONE', *, *, #34147, .T. ) ;
#8584 = APPLICATION_CONTEXT ( 'automotive_design' ) ;
#8585 = CARTESIAN_POINT ( 'NONE',  ( -0.4330708661417356775, 0.1864803149606299171, 1.186023622047243986 ) ) ;
#8586 = CARTESIAN_POINT ( 'NONE',  ( -0.9500414927467377701, 0.1787899950787401604, 1.136811023568283119 ) ) ;
#8587 = CARTESIAN_POINT ( 'NONE',  ( 0.9412147342319837628, 0.1574803149606300301, 1.158956692913385655 ) ) ;
#8588 = CARTESIAN_POINT ( 'NONE',  ( -0.9412147342319837628, 0.1574803149606300301, 0.7160433069790875793 ) ) ;
#8589 = CARTESIAN_POINT ( 'NONE',  ( 0.000000000000000000, 0.000000000000000000, -0.1436967020037460685 ) ) ;
#8590 = DIRECTION ( 'NONE',  ( -1.000000000000000000, 3.469446951953613794E-15, 1.144917494144692682E-16 ) ) ;
#8591 = CARTESIAN_POINT ( 'NONE',  ( -0.1330426644874648789, -0.08955887018083319440, 0.09370495055536537388 ) ) ;
#8592 = EDGE_LOOP ( 'NONE', ( #585, #35958, #30435 ) ) ;
#8593 = VECTOR ( 'NONE', #44466, 39.37007874015748143 ) ;
#8594 = CARTESIAN_POINT ( 'NONE',  ( -0.1476377952755905387, 0.07627223685636332073, -0.1475485644998805745 ) ) ;
#8595 = CARTESIAN_POINT ( 'NONE',  ( -0.2926984831716178959, 0.1026671379286196728, 0.7434188456247464716 ) ) ;
#8596 = CARTESIAN_POINT ( 'NONE',  ( 0.7495606340400177148, 0.1264236179284866091, 0.7455708660879684091 ) ) ;
#8597 = VERTEX_POINT ( 'NONE', #11777 ) ;
#8598 = DIRECTION ( 'NONE',  ( 0.000000000000000000, 0.000000000000000000, 1.000000000000000000 ) ) ;
#8599 = CARTESIAN_POINT ( 'NONE',  ( -0.1787899950787401604, -1.735236220418678643, -0.07405724077823318263 ) ) ;
#8600 = CARTESIAN_POINT ( 'NONE',  ( 0.07405724077823318263, -0.8444881889226140137, -0.1787899950787401604 ) ) ;
#8601 = CARTESIAN_POINT ( 'NONE',  ( -0.1113553986120547346, -1.203740157480315043, 0.1113553986120547346 ) ) ;
#8602 = CARTESIAN_POINT ( 'NONE',  ( 1.033464566929133799, 0.000000000000000000, 1.141732283357039357 ) ) ;
#8603 = CARTESIAN_POINT ( 'NONE',  ( -0.02899999999999994943, 0.5288907983920065892, -0.7507079620615685345 ) ) ;
#8604 = ADVANCED_FACE ( 'NONE', ( #30707 ), #27119, .F. ) ;
#8605 = EDGE_LOOP ( 'NONE', ( #33049, #4973, #37361, #41956, #25139, #21350, #12757, #7503, #44802, #17634, #628, #47163, #36650, #39885, #20740, #10995, #32932, #5513, #27263, #3440, #1104, #45665, #6850, #14399, #8349, #39659, #35638, #11486, #15552, #40241, #38182, #12734, #29611, #21707, #3520, #7729, #30823, #3539, #7794, #43869, #38460, #34740, #37029, #4114, #20709, #4343, #16186, #43390, #26998, #47028, #21347, #4342, #17819, #29615, #44742, #27599, #21043, #41999, #13668, #15761, #32327, #5657, #17873, #27703, #14305, #26070, #42264, #21699, #5192, #37382, #14413, #14050, #38297, #6023, #44380, #21802, #31804, #41530, #2527, #16777, #28880, #39062, #30618, #45677, #9468, #29265, #22997, #22516, #13248, #43571, #9139, #40186, #39374, #1575, #15618, #32532, #45090, #47445, #27938, #41398, #36015, #27873 ) ) ;
#8606 = VERTEX_POINT ( 'NONE', #8871 ) ;
#8607 = CARTESIAN_POINT ( 'NONE',  ( -0.8759842519685039353, 0.1787899950787401882, 1.769192913332062966 ) ) ;
#8608 = CARTESIAN_POINT ( 'NONE',  ( 0.6971942568897637749, 2.189545951927499583E-17, 1.897145669237574772 ) ) ;
#8609 = ORIENTED_EDGE ( 'NONE', *, *, #16733, .F. ) ;
#8610 = LINE ( 'NONE', #4286, #20278 ) ;
#8611 = CARTESIAN_POINT ( 'NONE',  ( 0.9500414927467378812, -0.1787899950787401604, 0.3740157479777325711 ) ) ;
#8612 = CARTESIAN_POINT ( 'NONE',  ( -0.9500414927467378812, 0.1787899950787401604, 1.328740157426552049 ) ) ;
#8613 = DIRECTION ( 'NONE',  ( 0.000000000000000000, -1.000000000000000000, 0.000000000000000000 ) ) ;
#8614 = CARTESIAN_POINT ( 'NONE',  ( -0.9500414927467377701, 0.1787899950787401604, 1.289370078686393750 ) ) ;
#8615 = EDGE_CURVE ( 'NONE', #3082, #5382, #950, .T. ) ;
#8616 = CARTESIAN_POINT ( 'NONE',  ( -0.8019270111902717657, -0.1787899950787401604, 0.8759842519147408302 ) ) ;
#8617 = FACE_OUTER_BOUND ( 'NONE', #21948, .T. ) ;
#8618 = ( BOUNDED_CURVE ( )  B_SPLINE_CURVE ( 2, ( #22489, #4037, #17306, #10370, #40676, #29510, #33546, #44279, #17778 ),
 .UNSPECIFIED., .F., .T. ) 
 B_SPLINE_CURVE_WITH_KNOTS ( ( 3, 2, 2, 2, 3 ),
 ( 0.2600000000000000089, 0.2625000000000000111, 0.2650000000000000133, 0.2675000000000000155, 0.2700000000000000178 ),
 .UNSPECIFIED. ) 
 CURVE ( )  GEOMETRIC_REPRESENTATION_ITEM ( )  RATIONAL_B_SPLINE_CURVE ( ( 1.000000000000000000, 0.9238795325112869605, 1.000000000000000000, 0.9238795325112869605, 1.000000000000000000, 0.9238795325112869605, 1.000000000000000000, 0.9238795325112869605, 1.000000000000000000 ) ) 
 REPRESENTATION_ITEM ( '' )  ) ;
#8619 = DIRECTION ( 'NONE',  ( 1.000000000000000000, 0.000000000000000000, 0.000000000000000000 ) ) ;
#8620 = CARTESIAN_POINT ( 'NONE',  ( -1.002407869896990045, 0.1264236179284866091, 1.764271653489543290 ) ) ;
#8621 = CARTESIAN_POINT ( 'NONE',  ( -0.7646288533564489232, 0.1113553986120547346, 1.983267716427905558 ) ) ;
#8622 = CARTESIAN_POINT ( 'NONE',  ( -0.9873396505805591694, -0.1113553986120547346, 1.697834645669291209 ) ) ;
#8623 = DIRECTION ( 'NONE',  ( 0.000000000000000000, 0.000000000000000000, -1.000000000000000000 ) ) ;
#8624 = CARTESIAN_POINT ( 'NONE',  ( 0.6971942568897648851, -0.07405724077823297447, 1.663385826717890925 ) ) ;
#8625 = CARTESIAN_POINT ( 'NONE',  ( -0.1150404479467348473, -0.09851383574764233098, 0.1176134116418862258 ) ) ;
#8626 = CARTESIAN_POINT ( 'NONE',  ( 0.1126279540338993995, 0.3740157480314960647, 1.206847064312612128 ) ) ;
#8627 = EDGE_LOOP ( 'NONE', ( #23487, #11973, #4025 ) ) ;
#8628 = CONICAL_SURFACE ( 'NONE', #6328, 0.09842519685039317900, 0.7853981633972921816 ) ;
#8629 = CARTESIAN_POINT ( 'NONE',  ( -1.002407869896990045, 0.1264236179284866091, 1.173720472387181246 ) ) ;
#8630 = ORIENTED_EDGE ( 'NONE', *, *, #13616, .F. ) ;
#8631 = CARTESIAN_POINT ( 'NONE',  ( -0.1787899950787401882, -0.9109251967966299768, 0.000000000000000000 ) ) ;
#8632 = ( BOUNDED_CURVE ( )  B_SPLINE_CURVE ( 2, ( #2649, #25676, #46499, #35740, #6964, #32147, #28816, #13678, #32873 ),
 .UNSPECIFIED., .F., .T. ) 
 B_SPLINE_CURVE_WITH_KNOTS ( ( 3, 2, 2, 2, 3 ),
 ( 0.4299999999999999933, 0.4324999999999999956, 0.4349999999999999978, 0.4375000000000000000, 0.4400000000000000022 ),
 .UNSPECIFIED. ) 
 CURVE ( )  GEOMETRIC_REPRESENTATION_ITEM ( )  RATIONAL_B_SPLINE_CURVE ( ( 1.000000000000000000, 0.9238795325112869605, 1.000000000000000000, 0.9238795325112869605, 1.000000000000000000, 0.9238795325112869605, 1.000000000000000000, 0.9238795325112869605, 1.000000000000000000 ) ) 
 REPRESENTATION_ITEM ( '' )  ) ;
#8633 = EDGE_CURVE ( 'NONE', #44803, #42642, #4300, .T. ) ;
#8634 = CARTESIAN_POINT ( 'NONE',  ( 0.1787899950787401604, -1.001968503883243988, -0.07405724077823318263 ) ) ;
#8635 = CARTESIAN_POINT ( 'NONE',  ( 0.6971942568897648851, 0.07405724077823318263, 1.850393700733638624 ) ) ;
#8636 = CARTESIAN_POINT ( 'NONE',  ( -0.1270800023317771588, -0.3504375103704472361, 0.1270800023317771588 ) ) ;
#8637 = DIRECTION ( 'NONE',  ( 0.000000000000000000, 0.000000000000000000, 1.000000000000000000 ) ) ;
#8638 = CARTESIAN_POINT ( 'NONE',  ( -0.7185039370078746268, -0.06523048226347956391, 0.8882874014672752505 ) ) ;
#8639 = CARTESIAN_POINT ( 'NONE',  ( 1.054774247047244540, -0.07405724077823318263, 0.7677165353793073965 ) ) ;
#8640 = VECTOR ( 'NONE', #41032, 39.37007874015748143 ) ;
#8642 = CARTESIAN_POINT ( 'NONE',  ( 0.000000000000000000, 0.000000000000000000, -0.3149606299212598381 ) ) ;
#8641 = CARTESIAN_POINT ( 'NONE',  ( -0.8107537697050254399, -0.1574803149606297803, 1.562499999892472013 ) ) ;
#8643 = CARTESIAN_POINT ( 'NONE',  ( 0.8759842519685039353, 0.1574803149606299191, 0.4527559055118110520 ) ) ;
#8644 = CARTESIAN_POINT ( 'NONE',  ( 0.7646288533564489232, -0.1113553986120547346, 0.1033464565853864231 ) ) ;
#8645 = EDGE_CURVE ( 'NONE', #1915, #38980, #31473, .T. ) ;
#8646 = PRODUCT_DEFINITION_FORMATION_WITH_SPECIFIED_SOURCE ( 'ANY', '', #1711, .NOT_KNOWN. ) ;
#8647 = CARTESIAN_POINT ( 'NONE',  ( 0.8759842519685039353, 0.1574803149606299191, 0.1377952755905511861 ) ) ;
#8648 = DIRECTION ( 'NONE',  ( 0.000000000000000000, 0.000000000000000000, 1.000000000000000000 ) ) ;
#8649 = CARTESIAN_POINT ( 'NONE',  ( 0.07405724077823318263, -0.4655511810485986057, 0.1787899950787401604 ) ) ;
#8650 = CARTESIAN_POINT ( 'NONE',  ( -0.07405724077823318263, -1.213582677111591623, 0.1787899950787401604 ) ) ;
#8651 = CARTESIAN_POINT ( 'NONE',  ( 1.054774247047244096, 0.000000000000000000, 0.2632874015210397434 ) ) ;
#8652 = CIRCLE ( 'NONE', #237, 0.09842519685039370636 ) ;
#8653 = EDGE_CURVE ( 'NONE', #43692, #16170, #6518, .T. ) ;
#8654 = CARTESIAN_POINT ( 'NONE',  ( -0.8019270111902717657, 0.1787899950787401604, 1.687992125930489307 ) ) ;
#8655 = EDGE_LOOP ( 'NONE', ( #8977, #47339, #8395, #28372 ) ) ;
#8656 = CARTESIAN_POINT ( 'NONE',  ( -0.6971942568897648851, -0.07405724077823297447, 1.348425196796630976 ) ) ;
#8657 = CARTESIAN_POINT ( 'NONE',  ( 0.8759842519685039353, -0.1787899950787401882, 1.355807086560409491 ) ) ;
#8658 = CARTESIAN_POINT ( 'NONE',  ( 0.8019270111902717657, -0.1787899950787401604, 0.09350393695411057804 ) ) ;
#8659 = CARTESIAN_POINT ( 'NONE',  ( -0.6971942568897648851, -0.07405724077823297447, 1.146653543253323582 ) ) ;
#8660 = CARTESIAN_POINT ( 'NONE',  ( 0.9412147342319837628, -0.1574803149606297803, 0.6619094487113718062 ) ) ;
#8661 = CARTESIAN_POINT ( 'NONE',  ( 0.06548250281709126763, -0.09842519584946800293, -0.1663669883860420806 ) ) ;
#8662 = CYLINDRICAL_SURFACE ( 'NONE', #15551, 0.1574803149606299191 ) ;
#8663 = CARTESIAN_POINT ( 'NONE',  ( 0.9500414927467377701, 0.1787899950787401604, 0.4675196849856070314 ) ) ;
#8664 = CARTESIAN_POINT ( 'NONE',  ( -0.8019270111902716547, -0.1787899950787401604, 0.4429133857730084833 ) ) ;
#8665 = EDGE_CURVE ( 'NONE', #21217, #5874, #1192, .T. ) ;
#8666 = CARTESIAN_POINT ( 'NONE',  ( -0.8759842519685039353, 0.1787899950787401882, 0.8193897637257637756 ) ) ;
#8667 = VERTEX_POINT ( 'NONE', #12245 ) ;
#8668 = CARTESIAN_POINT ( 'NONE',  ( 0.3000685424736224127, 4.466152701071653354E-17, 0.000000000000000000 ) ) ;
#8669 = ORIENTED_EDGE ( 'NONE', *, *, #10299, .T. ) ;
#8670 = CARTESIAN_POINT ( 'NONE',  ( 0.8019270111902717657, -0.1787899950787401604, 0.8809055117572599514 ) ) ;
#8671 = CARTESIAN_POINT ( 'NONE',  ( -0.7185039370078746268, 0.06523048226347956391, 0.2632874015748031260 ) ) ;
#8672 = CARTESIAN_POINT ( 'NONE',  ( 0.8019270111902716547, 0.1787899950787401604, 1.141732283410804349 ) ) ;
#8673 = CARTESIAN_POINT ( 'NONE',  ( 0.7185039370078739607, 1.928577636452523993E-17, 1.948818897530267602 ) ) ;
#8674 = CARTESIAN_POINT ( 'NONE',  ( 1.033464566929133799, 0.000000000000000000, 0.08858267716535432601 ) ) ;
#8675 = ORIENTED_EDGE ( 'NONE', *, *, #20352, .T. ) ;
#8676 = VECTOR ( 'NONE', #6460, 39.37007874015748143 ) ;
#8677 = FACE_OUTER_BOUND ( 'NONE', #35087, .T. ) ;
#8678 = CARTESIAN_POINT ( 'NONE',  ( -1.054774247047244540, 0.07405724077823318263, 0.9744094487651340231 ) ) ;
#8679 = CARTESIAN_POINT ( 'NONE',  ( 0.1637325577037128943, -0.07820587237429522942, -0.1401340067785763199 ) ) ;
#8680 = CARTESIAN_POINT ( 'NONE',  ( 0.9873396505805591694, -0.1113553986120547346, 0.3198818897637795700 ) ) ;
#8681 = CARTESIAN_POINT ( 'NONE',  ( -1.094772975963752103E-17, -1.482899558780419458, -0.1787899950787401882 ) ) ;
#8682 = ORIENTED_EDGE ( 'NONE', *, *, #23020, .F. ) ;
#8683 = CARTESIAN_POINT ( 'NONE',  ( -1.033464566929133799, 0.000000000000000000, 0.1574803148531029595 ) ) ;
#8684 = CARTESIAN_POINT ( 'NONE',  ( -0.1787899950787401604, -0.3917322834108032947, 0.07405724077823318263 ) ) ;
#8685 = CARTESIAN_POINT ( 'NONE',  ( -1.033464566929134687, -0.06523048226347956391, 0.08612204724409450174 ) ) ;
#8686 = ORIENTED_EDGE ( 'NONE', *, *, #45806, .T. ) ;
#8687 = CARTESIAN_POINT ( 'NONE',  ( 0.7495606340400177148, 0.1264236179284866091, 1.336122047190330786 ) ) ;
#8688 = CARTESIAN_POINT ( 'NONE',  ( 0.9412147342319837628, 0.1574803149606300301, 0.8833661417322832277 ) ) ;
#8689 = CARTESIAN_POINT ( 'NONE',  ( 0.8759842519685039353, 0.000000000000000000, 4.498031496062992574 ) ) ;
#8690 = CARTESIAN_POINT ( 'NONE',  ( 0.1264236179284866091, -0.2268700786863941110, 0.1264236179284866091 ) ) ;
#8691 = FACE_OUTER_BOUND ( 'NONE', #46644, .T. ) ;
#8692 = CARTESIAN_POINT ( 'NONE',  ( 0.9500414927467378812, -0.1787899950787401604, 1.628937007820252303 ) ) ;
#8693 = CARTESIAN_POINT ( 'NONE',  ( 0.8019270111902717657, 0.1787899950787401604, 0.1131889763241894359 ) ) ;
#8694 = CARTESIAN_POINT ( 'NONE',  ( 0.07405724077823318263, -1.764763779473795813, 0.1787899950787401604 ) ) ;
#8695 = DIRECTION ( 'NONE',  ( 0.000000000000000000, -1.000000000000000000, 0.000000000000000000 ) ) ;
#8696 = ADVANCED_FACE ( 'NONE', ( #26868 ), #31412, .F. ) ;
#8697 = CARTESIAN_POINT ( 'NONE',  ( 0.7185039370078739607, 1.928577636452523993E-17, 0.7775590551181102983 ) ) ;
#8698 = CARTESIAN_POINT ( 'NONE',  ( -0.8019270111902716547, 0.1787899950787401604, 0.6692913385289143147 ) ) ;
#8699 = EDGE_CURVE ( 'NONE', #860, #25910, #35000, .T. ) ;
#8701 = CYLINDRICAL_SURFACE ( 'NONE', #42969, 0.09842519685039370636 ) ;
#8700 = CARTESIAN_POINT ( 'NONE',  ( -0.1113553986120547346, -0.7017716535433071723, -0.1113553986120547346 ) ) ;
#8702 = CARTESIAN_POINT ( 'NONE',  ( 0.1270800023317771588, -1.511854833205092286, -0.1270800023317771588 ) ) ;
#8703 = LINE ( 'NONE', #8462, #27944 ) ;
#8704 = DIRECTION ( 'NONE',  ( 1.000000000000000000, 0.000000000000000000, -1.822029033848725275E-16 ) ) ;
#8705 = CARTESIAN_POINT ( 'NONE',  ( 0.9500414927467378812, 0.1787899950787401604, 1.333661417269071059 ) ) ;
#8706 = CARTESIAN_POINT ( 'NONE',  ( 0.9500414927467377701, 0.1787899950787401604, 1.879921259788756016 ) ) ;
#8707 = CARTESIAN_POINT ( 'NONE',  ( 1.002407869896990045, 0.1264236179284866091, 0.2632874015210397434 ) ) ;
#8708 = EDGE_CURVE ( 'NONE', #19538, #42619, #1912, .T. ) ;
#8709 = ORIENTED_EDGE ( 'NONE', *, *, #11424, .F. ) ;
#8711 = VERTEX_POINT ( 'NONE', #27360 ) ;
#8710 = CARTESIAN_POINT ( 'NONE',  ( -1.033464566929134687, -0.06523048226347956391, 0.1550196849318430659 ) ) ;
#8712 = LINE ( 'NONE', #24290, #2126 ) ;
#8713 = LINE ( 'NONE', #31024, #47389 ) ;
#8714 = CARTESIAN_POINT ( 'NONE',  ( 0.1787899950787401604, 0.09055118115612580121, 0.07405724077823318263 ) ) ;
#8715 = CARTESIAN_POINT ( 'NONE',  ( 1.054774247047244540, -0.07405724077823318263, 0.3740157479777325711 ) ) ;
#8717 = CARTESIAN_POINT ( 'NONE',  ( 1.229559056033039366E-16, -0.0009842519685041700977, 0.3937007874015748254 ) ) ;
#8716 = CARTESIAN_POINT ( 'NONE',  ( 0.7495606340400177148, 0.1264236179284866091, 1.296751968450173154 ) ) ;
#8718 = CARTESIAN_POINT ( 'NONE',  ( 0.9412147342319837628, 0.1574803149606300301, 0.8439960629921254842 ) ) ;
#8719 = CARTESIAN_POINT ( 'NONE',  ( -1.002407869896990045, -0.1264236179284866091, 1.355807086560409491 ) ) ;
#8720 = CARTESIAN_POINT ( 'NONE',  ( 0.9412147342319837628, -0.1574803149606297803, 0.7406496061916858498 ) ) ;
#8721 = ORIENTED_EDGE ( 'NONE', *, *, #11537, .T. ) ;
#8722 = CARTESIAN_POINT ( 'NONE',  ( -0.9412147342319837628, 0.1574803149606300301, 0.7947834644594015119 ) ) ;
#8723 = CARTESIAN_POINT ( 'NONE',  ( 0.06523048226347956391, -0.05462598425196848323, 0.1574803149606297803 ) ) ;
#8724 = VERTEX_POINT ( 'NONE', #42392 ) ;
#8725 = VERTEX_POINT ( 'NONE', #13196 ) ;
#8726 = CARTESIAN_POINT ( 'NONE',  ( -0.9412147342319837628, -0.1574803149606297803, 0.6225393699712132856 ) ) ;
#8727 = DIRECTION ( 'NONE',  ( 1.000000000000000000, 0.000000000000000000, -1.822029033848725275E-16 ) ) ;
#8728 = CARTESIAN_POINT ( 'NONE',  ( 1.054774247047244540, -0.07405724077823318263, 1.673228346402929834 ) ) ;
#8729 = CARTESIAN_POINT ( 'NONE',  ( -0.9873396505805591694, -0.1113553986120547346, 1.304133858267716661 ) ) ;
#8730 = CARTESIAN_POINT ( 'NONE',  ( -0.8759842519685039353, -0.1574803149606299191, 1.053149606191685184 ) ) ;
#8732 = CARTESIAN_POINT ( 'NONE',  ( -1.033464566929133799, 0.000000000000000000, 0.4429133858267716439 ) ) ;
#8731 = CARTESIAN_POINT ( 'NONE',  ( 0.5555748031496083872, 0.1864803149606326926, -0.7480314960629921295 ) ) ;
#8733 = CARTESIAN_POINT ( 'NONE',  ( 0.9412147342319837628, 0.1574803149606300301, 0.3617125983176697201 ) ) ;
#8734 = CARTESIAN_POINT ( 'NONE',  ( 0.9412147342319837628, 0.1574803149606300301, 1.385334645561763667 ) ) ;
#8735 = ORIENTED_EDGE ( 'NONE', *, *, #4876, .T. ) ;
#8736 = ORIENTED_EDGE ( 'NONE', *, *, #22775, .T. ) ;
#8737 = CARTESIAN_POINT ( 'NONE',  ( -0.3980944881889755260, 0.3833307086614208270, 0.7480314960629921295 ) ) ;
#8738 = AXIS2_PLACEMENT_3D ( 'NONE', #44808, #1430, #41675 ) ;
#8739 = CARTESIAN_POINT ( 'NONE',  ( 0.8759842519685039353, -0.1787899950787401882, 0.6865157479777322935 ) ) ;
#8740 = CARTESIAN_POINT ( 'NONE',  ( -1.054774247047244540, 0.07405724077823318263, 1.599409448765134911 ) ) ;
#8741 = CARTESIAN_POINT ( 'NONE',  ( -0.06523048226347956391, -0.06446850382948084157, -0.1574803149606300301 ) ) ;
#8742 = CARTESIAN_POINT ( 'NONE',  ( -0.9500414927467378812, 0.1787899950787401604, 1.333661417269071059 ) ) ;
#8743 = CARTESIAN_POINT ( 'NONE',  ( -0.7495606340400177148, 0.1264236179284866091, 0.3174212597887562382 ) ) ;
#8744 = CYLINDRICAL_SURFACE ( 'NONE', #11926, 0.1968503937007874405 ) ;
#8745 = CARTESIAN_POINT ( 'NONE',  ( -0.1787899950787401604, -0.9587853855520737101, 0.07405724077823318263 ) ) ;
#8746 = VERTEX_POINT ( 'NONE', #2831 ) ;
#8747 = CARTESIAN_POINT ( 'NONE',  ( -0.1787899950787401604, 0.07578740162856664742, -0.07405724077823318263 ) ) ;
#8748 = ORIENTED_EDGE ( 'NONE', *, *, #20509, .T. ) ;
#8749 = VERTEX_POINT ( 'NONE', #30945 ) ;
#8750 = DIRECTION ( 'NONE',  ( 0.000000000000000000, 0.000000000000000000, -1.000000000000000000 ) ) ;
#8751 = CARTESIAN_POINT ( 'NONE',  ( 0.7185039370078739607, 1.928577636452523993E-17, 0.09842519674286673292 ) ) ;
#8752 = AXIS2_PLACEMENT_3D ( 'NONE', #41547, #41794, #31293 ) ;
#8753 = CIRCLE ( 'NONE', #31734, 0.1870078740157481989 ) ;
#8754 = CARTESIAN_POINT ( 'NONE',  ( 0.1264236179284866091, -0.6500984251430865779, -0.1264236179284866091 ) ) ;
#8755 = EDGE_CURVE ( 'NONE', #30017, #38700, #39032, .T. ) ;
#8756 = EDGE_CURVE ( 'NONE', #35268, #16170, #24432, .T. ) ;
#8757 = CARTESIAN_POINT ( 'NONE',  ( -0.6971942568897626646, 0.07405724077823318263, 0.1624015747493861017 ) ) ;
#8758 = CARTESIAN_POINT ( 'NONE',  ( -0.8759842519685039353, -0.1574803149606299191, 0.9842519685039370358 ) ) ;
#8759 = DIRECTION ( 'NONE',  ( 0.000000000000000000, -1.000000000000000000, 0.000000000000000000 ) ) ;
#8760 = CARTESIAN_POINT ( 'NONE',  ( -0.1797182628040039087, -1.105850896197218658, -0.07444174185955065859 ) ) ;
#8761 = CARTESIAN_POINT ( 'NONE',  ( 0.1701422387595818708, 0.1299212598425197041, 0.05395700737448459045 ) ) ;
#8762 = CLOSED_SHELL ( 'NONE', ( #26435, #738, #32463, #29801, #29703, #38357, #37221, #36225, #1445, #6150, #37716, #20453 ) ) ;
#8763 = CARTESIAN_POINT ( 'NONE',  ( 0.8759842519685039353, 0.1787899950787401882, 0.8636811023084409733 ) ) ;
#8764 = EDGE_CURVE ( 'NONE', #11957, #7898, #46148, .T. ) ;
#8765 = EDGE_CURVE ( 'NONE', #24004, #23021, #36381, .T. ) ;
#8766 = CARTESIAN_POINT ( 'NONE',  ( 0.4736248074375590811, 1.914733266569315084, -0.6843357808987579061 ) ) ;
#8767 = CARTESIAN_POINT ( 'NONE',  ( 0.8107537697050253289, 0.1574803149606300301, 1.596948818897636402 ) ) ;
#8769 = CARTESIAN_POINT ( 'NONE',  ( -0.1586641775163213364, 1.495705267341508771, -0.3569552279982025622 ) ) ;
#8768 = CARTESIAN_POINT ( 'NONE',  ( 0.7172297754444691975, 0.04339135079164682662, 1.982441116835254036 ) ) ;
#8770 = CARTESIAN_POINT ( 'NONE',  ( 2.892866454678787531E-17, -0.09645669291338582196, 0.1574803149606299191 ) ) ;
#8771 = CARTESIAN_POINT ( 'NONE',  ( -1.033464566929134687, 0.06523048226347956391, 1.616633858160190229 ) ) ;
#8772 = CARTESIAN_POINT ( 'NONE',  ( -1.094772975963752103E-17, 0.06840551186478720236, -0.1787899950787401882 ) ) ;
#8773 = DIRECTION ( 'NONE',  ( 0.000000000000000000, 0.000000000000000000, -1.000000000000000000 ) ) ;
#8774 = CARTESIAN_POINT ( 'NONE',  ( 0.8759842519685039353, 0.1787899950787401882, 1.055610236166708793 ) ) ;
#8775 = CARTESIAN_POINT ( 'NONE',  ( 1.002407869896990045, -0.1264236179284866091, 1.833169291284818758 ) ) ;
#8776 = CARTESIAN_POINT ( 'NONE',  ( 0.7185039370078746268, -0.06523048226347956391, 0.4158464565853862704 ) ) ;
#8777 = VERTEX_POINT ( 'NONE', #34770 ) ;
#8778 = CARTESIAN_POINT ( 'NONE',  ( 1.033464566929134687, -0.06523048226347956391, 1.257381889656253193 ) ) ;
#8779 = CARTESIAN_POINT ( 'NONE',  ( 0.8759842519685039353, -0.1574803149606299191, 1.889763779527559251 ) ) ;
#8780 = CARTESIAN_POINT ( 'NONE',  ( -0.06523048226347956391, -1.703248031388535866, 0.1574803149606297803 ) ) ;
#8781 = CARTESIAN_POINT ( 'NONE',  ( -0.9873396505805591694, -0.1113553986120547346, 0.1919291337507405548 ) ) ;
#8782 = CARTESIAN_POINT ( 'NONE',  ( -0.4240551181102362177, -2.591110818884263559E-17, 0.000000000000000000 ) ) ;
#8783 = CARTESIAN_POINT ( 'NONE',  ( 0.6971942568897648851, 0.07405724077823318263, 1.141732283410804349 ) ) ;
#8784 = VECTOR ( 'NONE', #13903, 39.37007874015748143 ) ;
#8785 = DIRECTION ( 'NONE',  ( 1.000000000000000000, -0.000000000000000000, -0.000000000000000000 ) ) ;
#8786 = CARTESIAN_POINT ( 'NONE',  ( 0.07405724077823318263, 0.1446850394238423654, -0.1787899950787401604 ) ) ;
#8787 = CARTESIAN_POINT ( 'NONE',  ( -1.033464566929133799, 0.000000000000000000, 1.505905511811023612 ) ) ;
#8788 = CARTESIAN_POINT ( 'NONE',  ( -0.9500414927467378812, -0.1787899950787401604, 0.5265748030958428139 ) ) ;
#8789 = CARTESIAN_POINT ( 'NONE',  ( 0.7646288533564489232, -0.1113553986120547346, 1.363188976270427455 ) ) ;
#8790 = CARTESIAN_POINT ( 'NONE',  ( -0.9500414927467378812, -0.1787899950787401604, 0.2116141731745827814 ) ) ;
#8791 = ( BOUNDED_CURVE ( )  B_SPLINE_CURVE ( 2, ( #20968, #39180, #46845, #14036, #10451, #32504, #6826, #21446, #41055 ),
 .UNSPECIFIED., .F., .F. ) 
 B_SPLINE_CURVE_WITH_KNOTS ( ( 3, 2, 2, 2, 3 ),
 ( 0.7700000000000000178, 0.7724999999999999645, 0.7750000000000000222, 0.7774999999999999689, 0.7800000000000000266 ),
 .UNSPECIFIED. ) 
 CURVE ( )  GEOMETRIC_REPRESENTATION_ITEM ( )  RATIONAL_B_SPLINE_CURVE ( ( 1.000000000000000000, 0.9238795325112869605, 1.000000000000000000, 0.9238795325112869605, 1.000000000000000000, 0.9238795325112869605, 1.000000000000000000, 0.9238795325112869605, 1.000000000000000000 ) ) 
 REPRESENTATION_ITEM ( '' )  ) ;
#8793 = CARTESIAN_POINT ( 'NONE',  ( 0.07405724077823318263, -1.607283464513165949, 0.1787899950787401604 ) ) ;
#8792 = CARTESIAN_POINT ( 'NONE',  ( 0.06523048226347956391, -0.3449803148531030983, -0.1574803149606300301 ) ) ;
#8794 = CARTESIAN_POINT ( 'NONE',  ( -0.6971942568897648851, 0.07405724077823318263, 1.811023621993480548 ) ) ;
#8795 = CARTESIAN_POINT ( 'NONE',  ( -0.8759842519685039353, -0.1787899950787401882, 0.9965551180564724554 ) ) ;
#8796 = CARTESIAN_POINT ( 'NONE',  ( -1.002407869896990045, -0.1264236179284866091, 0.5339566928596221063 ) ) ;
#8797 = CARTESIAN_POINT ( 'NONE',  ( -0.2449982982381310737, 0.1540443988236174233, -0.2957398093694128538 ) ) ;
#8798 = DIRECTION ( 'NONE',  ( 0.000000000000000000, 1.000000000000000000, 0.000000000000000000 ) ) ;
#8799 = CARTESIAN_POINT ( 'NONE',  ( 0.07405724077823318263, -0.5404782989379000036, -0.1787899950787401604 ) ) ;
#8800 = CARTESIAN_POINT ( 'NONE',  ( 0.1203886723041954626, -0.08956011358862403515, 0.1770541383337161656 ) ) ;
#8801 = CARTESIAN_POINT ( 'NONE',  ( 0.8759842519685039353, 0.000000000000000000, 4.498031496062992574 ) ) ;
#8802 = CARTESIAN_POINT ( 'NONE',  ( -0.7185039370078739607, 0.000000000000000000, -2.869337061179095023E-17 ) ) ;
#8803 = CARTESIAN_POINT ( 'NONE',  ( 0.2559020992193656863, -0.1090393324022487509, -0.07498935245308939457 ) ) ;
#8804 = CARTESIAN_POINT ( 'NONE',  ( -1.002407869896990045, -0.1264236179284866091, 0.4109251967966299213 ) ) ;
#8805 = CARTESIAN_POINT ( 'NONE',  ( -1.094772975963752103E-17, -1.797860188701681183, -0.1787899950787401882 ) ) ;
#8806 = ORIENTED_EDGE ( 'NONE', *, *, #10241, .F. ) ;
#8807 = LINE ( 'NONE', #41369, #19495 ) ;
#8808 = CARTESIAN_POINT ( 'NONE',  ( -1.054774247047244540, 0.07405724077823318263, 1.525590551127339989 ) ) ;
#8809 = VECTOR ( 'NONE', #924, 39.37007874015748143 ) ;
#8810 = CARTESIAN_POINT ( 'NONE',  ( -0.1264236179284866091, -1.506397637741511586, -0.1264236179284866091 ) ) ;
#8811 = CARTESIAN_POINT ( 'NONE',  ( -0.1545411696117860445, -0.09842519685039370636, -0.08990488994085453489 ) ) ;
#8812 = EDGE_CURVE ( 'NONE', #33302, #30681, #3611, .T. ) ;
#8813 = PRESENTATION_STYLE_ASSIGNMENT (( #19602 ) ) ;
#8814 = CARTESIAN_POINT ( 'NONE',  ( 0.7185039370078746268, 0.06523048226347956391, 0.9719488188976379561 ) ) ;
#8815 = ORIENTED_EDGE ( 'NONE', *, *, #29231, .T. ) ;
#8816 = CARTESIAN_POINT ( 'NONE',  ( 0.7646288533564489232, -0.1113553986120547346, 0.4675196850393700809 ) ) ;
#8817 = CONICAL_SURFACE ( 'NONE', #14966, 0.08090551181102362266, 0.9599310885968742602 ) ;
#8818 = VECTOR ( 'NONE', #22006, 39.37007874015748854 ) ;
#8819 = DIRECTION ( 'NONE',  ( -3.469446951953612217E-15, -1.000000000000000000, 0.000000000000000000 ) ) ;
#8820 = CARTESIAN_POINT ( 'NONE',  ( -0.9412147342319837628, -0.1574803149606297803, 1.252460629813731741 ) ) ;
#8821 = CARTESIAN_POINT ( 'NONE',  ( 1.054774247047244096, 0.000000000000000000, 0.4995078739619842612 ) ) ;
#8822 = CARTESIAN_POINT ( 'NONE',  ( 1.054774247047244540, -0.07405724077823318263, 0.09842519679663024046 ) ) ;
#8824 = FACE_OUTER_BOUND ( 'NONE', #10383, .T. ) ;
#8823 = CARTESIAN_POINT ( 'NONE',  ( -0.1574803149606300301, -0.4237204724409446288, -0.06523048226347956391 ) ) ;
#8825 = VECTOR ( 'NONE', #27932, 39.37007874015748854 ) ;
#8826 = CARTESIAN_POINT ( 'NONE',  ( -0.9412147342319837628, 0.1574803149606300301, 0.4109251968503938590 ) ) ;
#8827 = ORIENTED_EDGE ( 'NONE', *, *, #25936, .F. ) ;
#8828 = ADVANCED_FACE ( 'NONE', ( #45748 ), #42613, .T. ) ;
#8829 = FACE_OUTER_BOUND ( 'NONE', #38501, .T. ) ;
#8830 = CARTESIAN_POINT ( 'NONE',  ( -0.6971942568897648851, -0.07405724077823297447, 1.072834645615528659 ) ) ;
#8831 = CARTESIAN_POINT ( 'NONE',  ( 0.9412147342319837628, -0.1574803149606297803, 1.065452755905511806 ) ) ;
#8832 = DIRECTION ( 'NONE',  ( -3.469446951953613794E-15, -1.000000000000000000, 0.000000000000000000 ) ) ;
#8833 = LINE ( 'NONE', #5223, #25116 ) ;
#8835 = CARTESIAN_POINT ( 'NONE',  ( -0.1377952755905509641, 0.000000000000000000, -0.2219368594840610276 ) ) ;
#8834 = FACE_OUTER_BOUND ( 'NONE', #6446, .T. ) ;
#8836 = CARTESIAN_POINT ( 'NONE',  ( -0.1066074665795045118, -0.08956136683350990335, 0.1197088631414433141 ) ) ;
#8837 = CARTESIAN_POINT ( 'NONE',  ( -0.07405724077823318263, -0.5049212597887556830, 0.1787899950787401604 ) ) ;
#8838 = ORIENTED_EDGE ( 'NONE', *, *, #15216, .T. ) ;
#8839 = CARTESIAN_POINT ( 'NONE',  ( 1.033464566929133799, 0.000000000000000000, 0.1968503935932602311 ) ) ;
#8840 = CARTESIAN_POINT ( 'NONE',  ( 0.7185039370078746268, -0.06523048226347956391, 0.2682086614173227468 ) ) ;
#8841 = CARTESIAN_POINT ( 'NONE',  ( 1.054774247047244540, -0.07405724077823318263, 0.6889763778989935750 ) ) ;
#8842 = CARTESIAN_POINT ( 'NONE',  ( -0.1235961452251413406, 0.09842519685039370636, -0.2140748031496062798 ) ) ;
#8843 = CARTESIAN_POINT ( 'NONE',  ( -0.7185039370078739607, 0.000000000000000000, -2.869337061179095023E-17 ) ) ;
#8844 = CARTESIAN_POINT ( 'NONE',  ( -0.1787899950787401604, -1.774606299158834277, -0.07405724077823318263 ) ) ;
#8845 = CARTESIAN_POINT ( 'NONE',  ( -0.1787899950787401882, -0.8715551180564724554, 0.000000000000000000 ) ) ;
#8846 = CARTESIAN_POINT ( 'NONE',  ( -9.642888182262618425E-18, -1.336614173228346525, -0.1574803149606299191 ) ) ;
#8847 = CARTESIAN_POINT ( 'NONE',  ( 0.7185039370078739607, 1.928577636452523993E-17, 1.161417322727118284 ) ) ;
#8848 = CARTESIAN_POINT ( 'NONE',  ( -0.9412147342319837628, 0.1574803149606300301, 1.857775590443653480 ) ) ;
#8849 = CARTESIAN_POINT ( 'NONE',  ( -0.8759842519685039353, 0.1787899950787401882, 0.4650590550643464716 ) ) ;
#8850 = VERTEX_POINT ( 'NONE', #24666 ) ;
#8851 = ORIENTED_EDGE ( 'NONE', *, *, #45281, .T. ) ;
#8852 = CARTESIAN_POINT ( 'NONE',  ( -0.6971942568897648851, -0.07405724077823297447, 1.781496062938362934 ) ) ;
#8853 = ORIENTED_EDGE ( 'NONE', *, *, #11923, .F. ) ;
#8854 = CARTESIAN_POINT ( 'NONE',  ( 0.6971942568897648851, 0.07405724077823318263, 1.894685039316315489 ) ) ;
#8855 = ORIENTED_EDGE ( 'NONE', *, *, #40556, .F. ) ;
#8856 = CARTESIAN_POINT ( 'NONE',  ( -0.1574803149606300301, -1.398129921152315935, -0.06523048226347956391 ) ) ;
#8857 = FACE_OUTER_BOUND ( 'NONE', #43000, .T. ) ;
#8858 = CARTESIAN_POINT ( 'NONE',  ( 0.6971942568897626646, 0.07405724077823318263, 0.3986220471903312301 ) ) ;
#8859 = CARTESIAN_POINT ( 'NONE',  ( -0.8759842519685039353, -0.1787899950787401882, 1.429625984198204858 ) ) ;
#8860 = VECTOR ( 'NONE', #22449, 39.37007874015748143 ) ;
#8861 = CARTESIAN_POINT ( 'NONE',  ( -1.033464566929133799, 0.000000000000000000, 1.624015748031496287 ) ) ;
#8862 = CARTESIAN_POINT ( 'NONE',  ( -0.8759842519685039353, -0.1787899950787401882, 0.8784448818360000022 ) ) ;
#8863 = CARTESIAN_POINT ( 'NONE',  ( -1.054774247047244540, 0.07405724077823318263, 0.02952755900135457801 ) ) ;
#8864 = CARTESIAN_POINT ( 'NONE',  ( -0.7185039370078746268, 0.06523048226347956391, 0.5782480314960627421 ) ) ;
#8865 = CARTESIAN_POINT ( 'NONE',  ( -0.6971942568897637749, 2.189545951927499583E-17, 1.700295275536787498 ) ) ;
#8866 = CARTESIAN_POINT ( 'NONE',  ( -0.6971942568897637749, 2.189545951927499583E-17, 0.08612204719033110523 ) ) ;
#8867 = CARTESIAN_POINT ( 'NONE',  ( -0.2471922904502826812, 0.03219022224904106305, 0.1427165354330708902 ) ) ;
#8868 = CARTESIAN_POINT ( 'NONE',  ( -0.7646288533564489232, 0.1113553986120547346, 1.678149606299212726 ) ) ;
#8869 = CARTESIAN_POINT ( 'NONE',  ( -1.033464566929133799, 0.000000000000000000, 0.9547244094488189781 ) ) ;
#8870 = CARTESIAN_POINT ( 'NONE',  ( 0.05241428596829866143, -0.09842519685039370636, -0.1860699077350574659 ) ) ;
#8871 = CARTESIAN_POINT ( 'NONE',  ( -0.1377952755905511861, 1.808041534174241898E-17, -0.09302377043719921301 ) ) ;
#8872 = ORIENTED_EDGE ( 'NONE', *, *, #47295, .T. ) ;
#8873 = CARTESIAN_POINT ( 'NONE',  ( 0.1279527559055118058, 0.2216206741968047289, -0.3149606299212598381 ) ) ;
#8874 = CIRCLE ( 'NONE', #28735, 0.1003937007874010356 ) ;
#8875 = AXIS2_PLACEMENT_3D ( 'NONE', #35351, #27478, #42029 ) ;
#8876 = ORIENTED_EDGE ( 'NONE', *, *, #20053, .F. ) ;
#8877 = VERTEX_POINT ( 'NONE', #39262 ) ;
#8878 = CARTESIAN_POINT ( 'NONE',  ( -0.1787899950787401882, -0.9896653542769447975, 0.000000000000000000 ) ) ;
#8879 = CARTESIAN_POINT ( 'NONE',  ( 0.07405724077823318263, -1.129921259788756682, 0.1787899950787401604 ) ) ;
#8880 = EDGE_CURVE ( 'NONE', #44147, #34498, #45506, .T. ) ;
#8881 = CARTESIAN_POINT ( 'NONE',  ( 0.1184675242425320824, -0.09842519685039370636, 1.713085361781127913 ) ) ;
#8882 = CARTESIAN_POINT ( 'NONE',  ( -0.1797182628040039365, -0.3159886914728094465, 0.000000000000000000 ) ) ;
#8883 = CARTESIAN_POINT ( 'NONE',  ( -0.7185039370078746268, -0.06523048226347956391, 0.8095472439869610959 ) ) ;
#8884 = CARTESIAN_POINT ( 'NONE',  ( 0.1574803149606300301, -0.01033464566929132716, 0.06523048226347956391 ) ) ;
#8885 = AXIS2_PLACEMENT_3D ( 'NONE', #11087, #7239, #11551 ) ;
#8886 = EDGE_CURVE ( 'NONE', #44444, #39, #34884, .T. ) ;
#8887 = FACE_OUTER_BOUND ( 'NONE', #45002, .T. ) ;
#8888 = CARTESIAN_POINT ( 'NONE',  ( 1.054774247047244096, 0.000000000000000000, 0.9670275590013542866 ) ) ;
#8889 = CARTESIAN_POINT ( 'NONE',  ( 2.219626494852212756E-16, 0.2954942322624074524, -0.1122047244094488277 ) ) ;
#8890 = CARTESIAN_POINT ( 'NONE',  ( 0.9412147342319837628, -0.1574803149606297803, 1.262303149606299746 ) ) ;
#8891 = CARTESIAN_POINT ( 'NONE',  ( 0.8759842519685039353, -0.1787899950787401882, 1.946358267662771757 ) ) ;
#8892 = ORIENTED_EDGE ( 'NONE', *, *, #30656, .T. ) ;
#8893 = CARTESIAN_POINT ( 'NONE',  ( 0.8759842519685039353, 0.1574803149606299191, 0.2165354330708661457 ) ) ;
#8894 = CARTESIAN_POINT ( 'NONE',  ( -0.7185039370078739607, 1.928577636452523993E-17, 1.643700787401574992 ) ) ;
#8895 = CARTESIAN_POINT ( 'NONE',  ( -0.1787899950787401882, -0.4778543306548976854, 0.000000000000000000 ) ) ;
#8896 = LINE ( 'NONE', #1449, #33944 ) ;
#8897 = CARTESIAN_POINT ( 'NONE',  ( 0.1787899950787401604, -1.198818897584032150, -0.07405724077823318263 ) ) ;
#8898 = ( BOUNDED_CURVE ( )  B_SPLINE_CURVE ( 2, ( #38140, #15408, #1231, #33874, #5070, #41939, #993, #44840, #23298 ),
 .UNSPECIFIED., .F., .T. ) 
 B_SPLINE_CURVE_WITH_KNOTS ( ( 3, 2, 2, 2, 3 ),
 ( 0.5999999999999999778, 0.6025000000000000355, 0.6049999999999999822, 0.6075000000000000400, 0.6099999999999999867 ),
 .UNSPECIFIED. ) 
 CURVE ( )  GEOMETRIC_REPRESENTATION_ITEM ( )  RATIONAL_B_SPLINE_CURVE ( ( 1.000000000000000000, 0.9238795325112869605, 1.000000000000000000, 0.9238795325112869605, 1.000000000000000000, 0.9238795325112869605, 1.000000000000000000, 0.9238795325112869605, 1.000000000000000000 ) ) 
 REPRESENTATION_ITEM ( '' )  ) ;
#8899 = CARTESIAN_POINT ( 'NONE',  ( -0.9500414927467378812, 0.1787899950787401604, 1.761811023568284007 ) ) ;
#8900 = EDGE_LOOP ( 'NONE', ( #43755, #36739, #4767, #8272 ) ) ;
#8901 = CARTESIAN_POINT ( 'NONE',  ( -0.9500414927467378812, -0.1787899950787401604, 1.279527559001355286 ) ) ;
#8902 = CARTESIAN_POINT ( 'NONE',  ( -0.9873396505805591694, 0.1113553986120547346, 1.313976377952756014 ) ) ;
#8903 = CARTESIAN_POINT ( 'NONE',  ( 0.6971942568897637749, 2.189545951927499583E-17, 1.424704724355685181 ) ) ;
#8904 = CARTESIAN_POINT ( 'NONE',  ( -0.1574803149606297803, -1.235728346349166840, 0.06523048226347956391 ) ) ;
#8905 = CARTESIAN_POINT ( 'NONE',  ( -1.054774247047244540, -0.07405724077823318263, 1.240157480261197431 ) ) ;
#8906 = CARTESIAN_POINT ( 'NONE',  ( 0.7646288533564489232, 0.1113553986120547346, 1.550196850286173156 ) ) ;
#8907 = CARTESIAN_POINT ( 'NONE',  ( 0.05897220410447782252, -0.09842522462652292248, -0.1687951425607464584 ) ) ;
#8908 = CARTESIAN_POINT ( 'NONE',  ( 0.9412147342319837628, 0.1574803149606300301, 0.04675196839640998608 ) ) ;
#8909 = CARTESIAN_POINT ( 'NONE',  ( 0.6971942568897637749, 2.189545951927499583E-17, 0.5979330708123780092 ) ) ;
#8910 = CARTESIAN_POINT ( 'NONE',  ( -0.8019270111902716547, -0.1787899950787401604, 0.3641732282926931630 ) ) ;
#8911 = EDGE_CURVE ( 'NONE', #25961, #37257, #29546, .T. ) ;
#8912 = CARTESIAN_POINT ( 'NONE',  ( -0.1006676817871263313, -0.09658349877441908815, 0.2273124399503319293 ) ) ;
#8913 = CARTESIAN_POINT ( 'NONE',  ( -9.642888182262618425E-18, -0.07677165354330708902, -0.1574803149606299191 ) ) ;
#8914 = VERTEX_POINT ( 'NONE', #46687 ) ;
#8915 = ORIENTED_EDGE ( 'NONE', *, *, #34012, .F. ) ;
#8916 = CARTESIAN_POINT ( 'NONE',  ( -0.7646288533564489232, -0.1113553986120547346, 0.2706692913385826960 ) ) ;
#8917 = CARTESIAN_POINT ( 'NONE',  ( 0.8019270111902716547, -0.1787899950787401604, 1.156496062938362046 ) ) ;
#8918 = CARTESIAN_POINT ( 'NONE',  ( -0.1275811598217675147, -0.09851385249697934554, -0.2189343593283228084 ) ) ;
#8919 = CARTESIAN_POINT ( 'NONE',  ( -0.2559055118110236671, -0.1005509620481576105, -0.06804208466526301402 ) ) ;
#8920 = B_SPLINE_CURVE_WITH_KNOTS ( 'NONE', 3,
 ( #40662, #15075, #41600, #8803, #16023, #7858, #30193, #8327, #26806, #36866, #19111, #40898, #11715, #27050, #4019, #26088, #33778, #887, #15547, #22476, #41365, #30645, #37092, #33530, #4240 ),
 .UNSPECIFIED., .F., .F.,
 ( 4, 2, 2, 1, 1, 1, 1, 2, 2, 2, 1, 1, 1, 2, 2, 4 ),
 ( 0.000000000000000000, 0.2499999999999949485, 0.3749999999999924505, 0.4374999999999911182, 0.4687499999999905631, 0.4843749999999902855, 0.4921874999999902855, 0.4960937499999901190, 0.4999999999999900080, 0.6249999999999911182, 0.6874999999999916733, 0.7187499999999920064, 0.7343749999999922284, 0.7421874999999924505, 0.7499999999999925615, 1.000000000000000000 ),
 .UNSPECIFIED. ) ;
#8921 = ORIENTED_EDGE ( 'NONE', *, *, #31084, .T. ) ;
#8922 = CARTESIAN_POINT ( 'NONE',  ( -0.6971942568897626646, -0.07405724077823297447, 0.9547244093950547628 ) ) ;
#8923 = ( BOUNDED_CURVE ( )  B_SPLINE_CURVE ( 2, ( #14245, #10172, #13996, #9704, #21170, #10416, #2948, #31754, #35804 ),
 .UNSPECIFIED., .F., .T. ) 
 B_SPLINE_CURVE_WITH_KNOTS ( ( 3, 2, 2, 2, 3 ),
 ( 0.3200000000000000067, 0.3225000000000000089, 0.3250000000000000111, 0.3275000000000000133, 0.3300000000000000155 ),
 .UNSPECIFIED. ) 
 CURVE ( )  GEOMETRIC_REPRESENTATION_ITEM ( )  RATIONAL_B_SPLINE_CURVE ( ( 1.000000000000000000, 0.9238795325112869605, 1.000000000000000000, 0.9238795325112869605, 1.000000000000000000, 0.9238795325112869605, 1.000000000000000000, 0.9238795325112869605, 1.000000000000000000 ) ) 
 REPRESENTATION_ITEM ( '' )  ) ;
#8924 = DIRECTION ( 'NONE',  ( 0.000000000000000000, 1.000000000000000000, 0.000000000000000000 ) ) ;
#8925 = CARTESIAN_POINT ( 'NONE',  ( -1.002407869896990045, 0.1264236179284866091, 0.06643700782025216411 ) ) ;
#8926 = CARTESIAN_POINT ( 'NONE',  ( -0.07405724077823318263, -1.583785385552072489, 0.1787899950787401604 ) ) ;
#8927 = ORIENTED_EDGE ( 'NONE', *, *, #45094, .F. ) ;
#8928 = PLANE ( 'NONE',  #6643 ) ;
#8929 = CARTESIAN_POINT ( 'NONE',  ( -0.1264236179284866091, -0.4778543306548976854, -0.1264236179284866091 ) ) ;
#8930 = CARTESIAN_POINT ( 'NONE',  ( -0.2644738720849207914, -0.1618167320693824351, 0.9199706799918920819 ) ) ;
#8931 = ORIENTED_EDGE ( 'NONE', *, *, #32872, .F. ) ;
#8932 = CARTESIAN_POINT ( 'NONE',  ( 0.7185039370078746268, 0.06523048226347956391, 0.8932086614173216921 ) ) ;
#8933 = CARTESIAN_POINT ( 'NONE',  ( 0.5962569168439626477, 4.766607801171850497E-17, 0.000000000000000000 ) ) ;
#8934 = CARTESIAN_POINT ( 'NONE',  ( -0.1787899950787401604, -0.2440944881352131168, -0.07405724077823318263 ) ) ;
#8935 = EDGE_CURVE ( 'NONE', #18734, #28644, #6673, .T. ) ;
#8936 = CYLINDRICAL_SURFACE ( 'NONE', #24169, 0.1574803149606299191 ) ;
#8937 = CARTESIAN_POINT ( 'NONE',  ( 0.1264236179284866091, 0.1263524097235171340, -0.1264236179284866091 ) ) ;
#8938 = CARTESIAN_POINT ( 'NONE',  ( 0.1264236179284866091, -1.796751968450173376, 0.1264236179284866091 ) ) ;
#8939 = PRODUCT_CONTEXT ( 'NONE', #43789, 'mechanical' ) ;
#8940 = CARTESIAN_POINT ( 'NONE',  ( 0.1335170321881475330, -0.09842519685039372024, 0.1069600103855054690 ) ) ;
#8941 = EDGE_CURVE ( 'NONE', #38112, #8361, #3324, .T. ) ;
#8942 = CARTESIAN_POINT ( 'NONE',  ( 0.9500414927467378812, -0.1787899950787401604, 0.4478346456155276045 ) ) ;
#8943 = CIRCLE ( 'NONE', #15084, 0.009842519685039376881 ) ;
#8944 = CARTESIAN_POINT ( 'NONE',  ( -1.002407869896990045, -0.1264236179284866091, 0.6914370078202519698 ) ) ;
#8946 = CARTESIAN_POINT ( 'NONE',  ( 1.033464566929134687, 0.06523048226347956391, 0.08120078729404769935 ) ) ;
#8945 = CARTESIAN_POINT ( 'NONE',  ( -0.1113553986120547346, -0.6919291338582677087, 0.1113553986120547346 ) ) ;
#8947 = CARTESIAN_POINT ( 'NONE',  ( 0.07444174185955046430, -1.588134360764147601, -0.1797182628040039087 ) ) ;
#8948 = DIRECTION ( 'NONE',  ( -1.000000000000000000, 0.000000000000000000, 0.000000000000000000 ) ) ;
#8949 = CARTESIAN_POINT ( 'NONE',  ( 0.07405724077823318263, -0.3671259841982050798, -0.1787899950787401604 ) ) ;
#8950 = CARTESIAN_POINT ( 'NONE',  ( 0.000000000000000000, 0.000000000000000000, 2.731847993664263218E-16 ) ) ;
#8951 = CARTESIAN_POINT ( 'NONE',  ( 0.8759842519685039353, 0.1787899950787401882, 1.532972440891118060 ) ) ;
#8952 = CARTESIAN_POINT ( 'NONE',  ( 1.054774247047244540, 0.07405724077823318263, 1.835629921206078485 ) ) ;
#8953 = CARTESIAN_POINT ( 'NONE',  ( 0.6971942568897626646, 0.07405724077823318263, 0.3149606298674962890 ) ) ;
#8954 = CARTESIAN_POINT ( 'NONE',  ( -0.9412147342319837628, -0.1574803149606297803, 0.1500984250893234173 ) ) ;
#8955 = DIRECTION ( 'NONE',  ( 0.000000000000000000, 0.000000000000000000, -1.000000000000000000 ) ) ;
#8956 = DIRECTION ( 'NONE',  ( 0.000000000000000000, 0.7880107536067179064, -0.6156614753256635098 ) ) ;
#8957 = CARTESIAN_POINT ( 'NONE',  ( 0.07405724077823318263, 0.08562992131360593062, 0.1787899950787401604 ) ) ;
#8958 = CARTESIAN_POINT ( 'NONE',  ( 0.7495606340400177148, -0.1264236179284866091, 0.5191929133320630774 ) ) ;
#8959 = CARTESIAN_POINT ( 'NONE',  ( 0.7576286657187201179, -0.1165239664453579099, 0.03937184544582203460 ) ) ;
#8960 = CARTESIAN_POINT ( 'NONE',  ( -0.7646288533564489232, 0.1113553986120547346, 1.717519685039369914 ) ) ;
#8961 = DIRECTION ( 'NONE',  ( -0.8191520442889947962, 0.4519843998600418522, -0.3531289150159164225 ) ) ;
#8962 = CARTESIAN_POINT ( 'NONE',  ( -0.7495606340400177148, 0.1264236179284866091, 1.336122047190330786 ) ) ;
#8963 = CARTESIAN_POINT ( 'NONE',  ( 0.9873396505805591694, 0.1113553986120547346, 0.7923228345381417848 ) ) ;
#8964 = VERTEX_POINT ( 'NONE', #28764 ) ;
#8965 = CARTESIAN_POINT ( 'NONE',  ( -1.054774247047244540, -0.07405724077823318263, 1.087598425143086578 ) ) ;
#8966 = CARTESIAN_POINT ( 'NONE',  ( 0.8019270111902717657, 0.1787899950787401604, 1.062992125930488418 ) ) ;
#8967 = CARTESIAN_POINT ( 'NONE',  ( 0.07405724077823318263, -1.371062992072219489, 0.1787899950787401604 ) ) ;
#8968 = CARTESIAN_POINT ( 'NONE',  ( -0.7646288533564489232, 0.1113553986120547346, 0.5265748030420794867 ) ) ;
#8969 = CARTESIAN_POINT ( 'NONE',  ( -0.8759842519685039353, -0.1574803149606299191, 1.220472440944881942 ) ) ;
#8970 = CARTESIAN_POINT ( 'NONE',  ( 1.054774247047244540, 0.07405724077823318263, 1.717519684985606476 ) ) ;
#8971 = CARTESIAN_POINT ( 'NONE',  ( -1.033464566929134687, 0.06523048226347956391, 1.232775590551179912 ) ) ;
#8972 = CARTESIAN_POINT ( 'NONE',  ( 0.000000000000000000, 0.000000000000000000, -0.2495040853978291451 ) ) ;
#8973 = CARTESIAN_POINT ( 'NONE',  ( -0.7185039370078739607, 1.928577636452523993E-17, 0.7381889763779527769 ) ) ;
#8974 = CARTESIAN_POINT ( 'NONE',  ( -0.9412147342319837628, -0.1574803149606297803, 0.5044291337507409434 ) ) ;
#8975 = CARTESIAN_POINT ( 'NONE',  ( 0.7646288533564489232, 0.1113553986120547346, 1.432086614065700925 ) ) ;
#8976 = ORIENTED_EDGE ( 'NONE', *, *, #7523, .F. ) ;
#8977 = ORIENTED_EDGE ( 'NONE', *, *, #6260, .F. ) ;
#8978 = CARTESIAN_POINT ( 'NONE',  ( 0.7185039370078739607, 0.000000000000000000, 4.498031496062993462 ) ) ;
#8979 = CARTESIAN_POINT ( 'NONE',  ( 0.7495606340400177148, 0.1264236179284866091, 0.9473425196312755814 ) ) ;
#8980 = CARTESIAN_POINT ( 'NONE',  ( -0.9500414927467377701, 0.1787899950787401604, 1.604330708607653921 ) ) ;
#8981 = CARTESIAN_POINT ( 'NONE',  ( 0.06523048226347956391, -0.06938976367200050399, -0.1574803149606300301 ) ) ;
#8982 = CARTESIAN_POINT ( 'NONE',  ( -0.9500414927467378812, 0.1787899950787401604, 1.491141732229701367 ) ) ;
#8983 = ORIENTED_EDGE ( 'NONE', *, *, #34003, .T. ) ;
#8984 = AXIS2_PLACEMENT_3D ( 'NONE', #43956, #15218, #33684 ) ;
#8985 = DIRECTION ( 'NONE',  ( 0.000000000000000000, 0.000000000000000000, 1.000000000000000000 ) ) ;
#8986 = CARTESIAN_POINT ( 'NONE',  ( -1.033464566929133799, 1.928577636452524610E-17, 2.869337061179095023E-17 ) ) ;
#8987 = CARTESIAN_POINT ( 'NONE',  ( -0.1787899950787401882, -1.118726330433962524, 0.000000000000000000 ) ) ;
#8988 = EDGE_LOOP ( 'NONE', ( #3445, #40701, #1381, #17064, #2300, #42339 ) ) ;
#8989 = CARTESIAN_POINT ( 'NONE',  ( -0.1264236179284866091, 0.04379921265218866822, 0.1264236179284866091 ) ) ;
#8990 = EDGE_LOOP ( 'NONE', ( #22295, #33327, #31614, #27327 ) ) ;
#8991 = ADVANCED_FACE ( 'NONE', ( #47414 ), #36863, .T. ) ;
#8992 = VERTEX_POINT ( 'NONE', #10294 ) ;
#8993 = CARTESIAN_POINT ( 'NONE',  ( -0.7646288533564489232, -0.1113553986120547346, 1.205708661309795371 ) ) ;
#8994 = DIRECTION ( 'NONE',  ( 1.000000000000000000, 0.000000000000000000, -1.822029033848725275E-16 ) ) ;
#8995 = PRODUCT_DEFINITION_SHAPE ( 'NONE', 'NONE',  #23955 ) ;
#8996 = CARTESIAN_POINT ( 'NONE',  ( 0.7185039370078746268, 0.06523048226347956391, 1.798720472440944462 ) ) ;
#8997 = CARTESIAN_POINT ( 'NONE',  ( 0.07405724077823318263, -0.6082677164816695514, -0.1787899950787401604 ) ) ;
#8998 = EDGE_CURVE ( 'NONE', #28190, #45599, #35622, .T. ) ;
#8999 = CARTESIAN_POINT ( 'NONE',  ( -0.8019270111902716547, 0.1787899950787401604, 0.1968503936470238636 ) ) ;
#9000 = CARTESIAN_POINT ( 'NONE',  ( -0.9873396505805591694, 0.1113553986120547346, 0.9990157480314961758 ) ) ;
#9001 = CARTESIAN_POINT ( 'NONE',  ( 3.301370929368692659E-17, -1.132917825331076767, 0.1797182628040039365 ) ) ;
#9002 = CARTESIAN_POINT ( 'NONE',  ( 0.1651804164989524593, 0.1299212598425196763, 0.06841997037041555596 ) ) ;
#9003 = CARTESIAN_POINT ( 'NONE',  ( 0.6971942568897648851, 0.07405724077823318263, 1.067913385773007651 ) ) ;
#9004 = CARTESIAN_POINT ( 'NONE',  ( -0.5555748031496040573, 0.7681739484881661140, -0.04983111751016786051 ) ) ;
#9005 = CARTESIAN_POINT ( 'NONE',  ( 0.9873396505805591694, -0.1113553986120547346, 1.619094488188976388 ) ) ;
#9007 = CARTESIAN_POINT ( 'NONE',  ( -0.1832342603886610577, -0.1897030460623687631, -0.3104511204119963508 ) ) ;
#9006 = CARTESIAN_POINT ( 'NONE',  ( 0.7619656079993829545, 0.1146971827241134723, 1.980798226884399327 ) ) ;
#9008 = CARTESIAN_POINT ( 'NONE',  ( 0.7646288533564489232, -0.1113553986120547346, 0.4576771652468039631 ) ) ;
#9009 = CARTESIAN_POINT ( 'NONE',  ( 0.1113553986120547346, -0.7116141731208188714, 0.1113553986120547346 ) ) ;
#9010 = CARTESIAN_POINT ( 'NONE',  ( -0.7646288533564489232, 0.1113553986120547346, 1.628937007766488199 ) ) ;
#9011 = CONICAL_SURFACE ( 'NONE', #26651, 0.1574803149606299191, 0.9599310885968603824 ) ;
#9012 = LINE ( 'NONE', #43832, #54 ) ;
#9013 = CARTESIAN_POINT ( 'NONE',  ( 1.002407869896990045, -0.1264236179284866091, 0.9621062991588346103 ) ) ;
#9014 = CARTESIAN_POINT ( 'NONE',  ( 0.6971942568897648851, -0.07405724077823297447, 1.860236220418677089 ) ) ;
#9015 = CARTESIAN_POINT ( 'NONE',  ( 1.033464566929134687, -0.06523048226347956391, 0.3518700786326304231 ) ) ;
#9016 = VERTEX_POINT ( 'NONE', #14827 ) ;
#9017 = DIRECTION ( 'NONE',  ( -0.000000000000000000, 1.000000000000000000, -0.000000000000000000 ) ) ;
#9018 = DIRECTION ( 'NONE',  ( 0.000000000000000000, -0.6156614753256639538, -0.7880107536067174623 ) ) ;
#9019 = CARTESIAN_POINT ( 'NONE',  ( -0.06523048226347956391, -1.639271653435778964, -0.1574803149606300301 ) ) ;
#9020 = DIRECTION ( 'NONE',  ( 1.000000000000000000, 0.000000000000000000, 0.000000000000000000 ) ) ;
#9021 = CARTESIAN_POINT ( 'NONE',  ( 0.6971942568897648851, -0.07405724077823297447, 1.343503936954111744 ) ) ;
#9022 = DIRECTION ( 'NONE',  ( 1.000000000000000000, 0.000000000000000000, 0.000000000000000000 ) ) ;
#9023 = DIMENSIONAL_EXPONENTS ( 1.000000000000000000, 0.000000000000000000, 0.000000000000000000, 0.000000000000000000, 0.000000000000000000, 0.000000000000000000, 0.000000000000000000 ) ;
#9024 = CARTESIAN_POINT ( 'NONE',  ( -0.1787899950787401604, 0.07578740162856664742, -0.07405724077823318263 ) ) ;
#9025 = CARTESIAN_POINT ( 'NONE',  ( -0.8759842519685039353, 0.1574803149606299191, 1.870078740157480324 ) ) ;
#9026 = CARTESIAN_POINT ( 'NONE',  ( -0.8019270111902717657, -0.1787899950787401604, 0.5216535432533228045 ) ) ;
#9027 = CARTESIAN_POINT ( 'NONE',  ( 0.2821522309711287368, 4.616380251121755931E-17, 0.000000000000000000 ) ) ;
#9028 = CARTESIAN_POINT ( 'NONE',  ( -0.04076295239693389361, 0.06762482675903896956, 0.2618985693268079396 ) ) ;
#9029 = EDGE_LOOP ( 'NONE', ( #32991, #10164, #38111, #16704 ) ) ;
#9030 = FACE_OUTER_BOUND ( 'NONE', #7042, .T. ) ;
#9031 = VERTEX_POINT ( 'NONE', #36169 ) ;
#9033 = CARTESIAN_POINT ( 'NONE',  ( 0.07405724077823318263, -1.567913385773008095, 0.1787899950787401604 ) ) ;
#9032 = CARTESIAN_POINT ( 'NONE',  ( -0.1113553986120547346, -0.3769685038294807167, -0.1113553986120547346 ) ) ;
#9034 = CARTESIAN_POINT ( 'NONE',  ( -1.054774247047244540, -0.07405724077823318263, 1.048228346402930944 ) ) ;
#9035 = CARTESIAN_POINT ( 'NONE',  ( -1.054774247047244540, -0.07405724077823318263, 1.830708661363559253 ) ) ;
#9036 = EDGE_CURVE ( 'NONE', #45117, #41157, #19530, .T. ) ;
#9037 = CARTESIAN_POINT ( 'NONE',  ( -0.6971942568897637749, 2.189545951927499583E-17, 0.7160433070328504623 ) ) ;
#9038 = ( BOUNDED_CURVE ( )  B_SPLINE_CURVE ( 2, ( #40897, #8091, #19110, #33775, #37812, #34235, #30643, #15545, #23668 ),
 .UNSPECIFIED., .F., .T. ) 
 B_SPLINE_CURVE_WITH_KNOTS ( ( 3, 2, 2, 2, 3 ),
 ( 0.9000000000000000222, 0.9024999999999999689, 0.9050000000000000266, 0.9074999999999999734, 0.9100000000000000311 ),
 .UNSPECIFIED. ) 
 CURVE ( )  GEOMETRIC_REPRESENTATION_ITEM ( )  RATIONAL_B_SPLINE_CURVE ( ( 1.000000000000000000, 0.9238795325112869605, 1.000000000000000000, 0.9238795325112869605, 1.000000000000000000, 0.9238795325112869605, 1.000000000000000000, 0.9238795325112869605, 1.000000000000000000 ) ) 
 REPRESENTATION_ITEM ( '' )  ) ;
#9040 = ORIENTED_EDGE ( 'NONE', *, *, #22181, .T. ) ;
#9039 = EDGE_CURVE ( 'NONE', #41713, #8606, #43565, .T. ) ;
#9041 = AXIS2_PLACEMENT_3D ( 'NONE', #29977, #19133, #11740 ) ;
#9042 = CARTESIAN_POINT ( 'NONE',  ( 0.1377952755905512139, 0.1574803149606299191, -0.9074803149606294195 ) ) ;
#9043 = CARTESIAN_POINT ( 'NONE',  ( 0.3000685424736224127, 0.09842519685039370636, 1.205361022782828805E-17 ) ) ;
#9044 = CARTESIAN_POINT ( 'NONE',  ( 0.1787899950787401882, -0.5872302674418370394, -2.189545951927503898E-17 ) ) ;
#9045 = CARTESIAN_POINT ( 'NONE',  ( 0.1441055234924401574, -0.08955999847834450467, 0.1574950935048799183 ) ) ;
#9046 = FACE_OUTER_BOUND ( 'NONE', #25909, .T. ) ;
#9047 = ADVANCED_FACE ( 'NONE', ( #25850 ), #40433, .F. ) ;
#9048 = EDGE_LOOP ( 'NONE', ( #24849, #890, #35106, #43245 ) ) ;
#9049 = CIRCLE ( 'NONE', #6738, 0.1787899950787401049 ) ;
#9050 = CARTESIAN_POINT ( 'NONE',  ( -0.9500414927467378812, 0.1787899950787401604, 0.5019685038832442103 ) ) ;
#9051 = DIRECTION ( 'NONE',  ( 1.000000000000000000, 0.000000000000000000, -1.822029033848725275E-16 ) ) ;
#9052 = ORIENTED_EDGE ( 'NONE', *, *, #2499, .T. ) ;
#9053 = CARTESIAN_POINT ( 'NONE',  ( 0.2471921406147994105, -0.06698952652786568929, 0.09859233283899719591 ) ) ;
#9054 = CARTESIAN_POINT ( 'NONE',  ( -0.9500414927467377701, 0.1787899950787401604, 1.530511810969859221 ) ) ;
#9055 = CARTESIAN_POINT ( 'NONE',  ( 0.1264236179284866091, -1.486712598371433103, 0.1264236179284866091 ) ) ;
#9056 = CARTESIAN_POINT ( 'NONE',  ( -0.5555748031496045014, 0.6449983665207589256, -0.06082000038405668829 ) ) ;
#9057 = DIRECTION ( 'NONE',  ( 0.000000000000000000, -1.000000000000000000, 0.000000000000000000 ) ) ;
#9058 = CARTESIAN_POINT ( 'NONE',  ( -1.033464566929133799, 0.000000000000000000, 1.466535433070866201 ) ) ;
#9059 = CARTESIAN_POINT ( 'NONE',  ( 0.7646288533564489232, 0.1113553986120547346, 0.4576771653543307283 ) ) ;
#9060 = CARTESIAN_POINT ( 'NONE',  ( 0.1797182628040039087, -0.7269138883232022508, -0.07444174185955065859 ) ) ;
#9061 = CARTESIAN_POINT ( 'NONE',  ( 0.2204724409448818867, 0.07955613945526338049, 0.1377952755905511861 ) ) ;
#9062 = CARTESIAN_POINT ( 'NONE',  ( -1.033464566929134687, -0.06523048226347956391, 1.178641732175937040 ) ) ;
#9063 = CARTESIAN_POINT ( 'NONE',  ( 0.6971942568897626646, 0.07405724077823318263, 0.6742125983714335469 ) ) ;
#9064 = CARTESIAN_POINT ( 'NONE',  ( 0.8759842519685039353, 0.1787899950787401882, 0.07135826766277185429 ) ) ;
#9066 = LINE ( 'NONE', #45698, #16335 ) ;
#9065 = CARTESIAN_POINT ( 'NONE',  ( -0.1113553986120547346, -0.4950787401574803237, 0.1113553986120547346 ) ) ;
#9067 = CARTESIAN_POINT ( 'NONE',  ( -0.7185039370078739607, 0.000000000000000000, -2.869337061179095023E-17 ) ) ;
#9068 = ORIENTED_EDGE ( 'NONE', *, *, #38837, .F. ) ;
#9069 = DIRECTION ( 'NONE',  ( 0.8191520442889991260, 1.003171929053533745E-16, -0.5735764363510355013 ) ) ;
#9070 = CARTESIAN_POINT ( 'NONE',  ( 0.8759842519685039353, 0.1574803149606299191, 1.122047244094488194 ) ) ;
#9071 = DIRECTION ( 'NONE',  ( 0.000000000000000000, 0.000000000000000000, 1.000000000000000000 ) ) ;
#9072 = DIRECTION ( 'NONE',  ( 1.000000000000000000, -0.000000000000000000, -1.144917494144692682E-16 ) ) ;
#9073 = CARTESIAN_POINT ( 'NONE',  ( -0.1113553986120547346, -0.5738188975302677131, -0.1113553986120547346 ) ) ;
#9075 = CARTESIAN_POINT ( 'NONE',  ( 0.9412147342319837628, -0.1574803149606297803, 1.685531495955465697 ) ) ;
#9074 = DIRECTION ( 'NONE',  ( -1.000000000000000000, -0.000000000000000000, 0.000000000000000000 ) ) ;
#9076 = VECTOR ( 'NONE', #40627, 39.37007874015748143 ) ;
#9077 = FACE_OUTER_BOUND ( 'NONE', #23461, .T. ) ;
#9078 = CARTESIAN_POINT ( 'NONE',  ( 0.1787899950787401604, -0.5344488188438744070, 0.07405724077823318263 ) ) ;
#9079 = VERTEX_POINT ( 'NONE', #7157 ) ;
#9080 = CARTESIAN_POINT ( 'NONE',  ( 0.8107537697050234415, -0.1574803149606297803, 0.2731299212598424231 ) ) ;
#9081 = CARTESIAN_POINT ( 'NONE',  ( 0.6971942568897637749, 2.189545951927499583E-17, 0.8292322834108031282 ) ) ;
#9082 = ORIENTED_EDGE ( 'NONE', *, *, #3992, .T. ) ;
#9083 = CARTESIAN_POINT ( 'NONE',  ( -0.4338976377952755703, -2.656856766417909227E-17, 0.000000000000000000 ) ) ;
#9084 = CARTESIAN_POINT ( 'NONE',  ( -1.033464566929133799, 1.928577636452524610E-17, 2.869337061179095023E-17 ) ) ;
#9085 = CARTESIAN_POINT ( 'NONE',  ( 3.284318927891251994E-17, -1.683562992072220599, 0.1787899950787401882 ) ) ;
#9086 = CARTESIAN_POINT ( 'NONE',  ( 3.284318927891251994E-17, -0.8617125983714329918, 0.1787899950787401882 ) ) ;
#9088 = AXIS2_PLACEMENT_3D ( 'NONE', #17462, #3071, #5968 ) ;
#9087 = CARTESIAN_POINT ( 'NONE',  ( 0.1574803149606300301, -1.388287401574803015, 0.06523048226347956391 ) ) ;
#9089 = CARTESIAN_POINT ( 'NONE',  ( 0.8759842519685039353, 0.1574803149606299191, 1.230314960522393752 ) ) ;
#9090 = VERTEX_POINT ( 'NONE', #24904 ) ;
#9091 = ORIENTED_EDGE ( 'NONE', *, *, #28013, .F. ) ;
#9092 = CARTESIAN_POINT ( 'NONE',  ( -0.9500414927467378812, -0.1787899950787401604, 1.948818897584033927 ) ) ;
#9093 = CARTESIAN_POINT ( 'NONE',  ( 0.9500414927467378812, -0.1787899950787401604, 1.830708661363559253 ) ) ;
#9094 = ORIENTED_EDGE ( 'NONE', *, *, #23438, .T. ) ;
#9095 = CARTESIAN_POINT ( 'NONE',  ( -0.9500414927467378812, -0.1787899950787401604, 0.8858267715997791836 ) ) ;
#9096 = CARTESIAN_POINT ( 'NONE',  ( 0.4208034506101054895, -0.09842519685039370636, 0.000000000000000000 ) ) ;
#9097 = CARTESIAN_POINT ( 'NONE',  ( 0.9500414927467378812, -0.1787899950787401604, 0.4921259841982048577 ) ) ;
#9098 = CARTESIAN_POINT ( 'NONE',  ( -1.054774247047244540, 0.07405724077823318263, 1.402559055064346971 ) ) ;
#9099 = CARTESIAN_POINT ( 'NONE',  ( 0.8759842519685039353, 0.000000000000000000, 4.498031496062992574 ) ) ;
#9100 = EDGE_CURVE ( 'NONE', #14069, #33762, #27232, .T. ) ;
#9101 = CARTESIAN_POINT ( 'NONE',  ( -1.002407869896990045, 0.1264236179284866091, 0.9719488188438739629 ) ) ;
#9102 = CARTESIAN_POINT ( 'NONE',  ( -1.002407869896990045, 0.1264236179284866091, 0.07135826766277185429 ) ) ;
#9103 = ADVANCED_FACE ( 'NONE', ( #35916 ), #17244, .T. ) ;
#9104 = CARTESIAN_POINT ( 'NONE',  ( 0.2944196465027555387, -0.09842519685039370636, 1.205361022782828805E-17 ) ) ;
#9105 = CARTESIAN_POINT ( 'NONE',  ( -0.8019270111902717657, 0.1787899950787401604, 1.811023621993480548 ) ) ;
#9106 = CARTESIAN_POINT ( 'NONE',  ( -0.8759842519685039353, 0.1574803149606299191, 1.978346456585385882 ) ) ;
#9107 = CARTESIAN_POINT ( 'NONE',  ( -7.939671275311751530E-17, -0.03219022224904082713, -0.2854330708661417804 ) ) ;
#9108 = CARTESIAN_POINT ( 'NONE',  ( -0.8759842519685039353, -0.1574803149606299191, 1.771653543307086576 ) ) ;
#9109 = CARTESIAN_POINT ( 'NONE',  ( -0.9873396505805591694, -0.1113553986120547346, 0.9498031496062993018 ) ) ;
#9110 = CARTESIAN_POINT ( 'NONE',  ( 0.8019270111902716547, 0.1787899950787401604, 1.732283464513166615 ) ) ;
#9111 = CARTESIAN_POINT ( 'NONE',  ( 0.2057643835732720639, -0.09842519685039370636, -0.01601721728994680988 ) ) ;
#9112 = CARTESIAN_POINT ( 'NONE',  ( -0.9873396505805591694, -0.1113553986120547346, 0.7431102361129447997 ) ) ;
#9113 = EDGE_CURVE ( 'NONE', #25448, #25968, #17465, .T. ) ;
#9114 = EDGE_CURVE ( 'NONE', #13081, #26397, #17703, .T. ) ;
#9115 = VECTOR ( 'NONE', #27201, 39.37007874015748143 ) ;
#9116 = ORIENTED_EDGE ( 'NONE', *, *, #33785, .T. ) ;
#9117 = VERTEX_POINT ( 'NONE', #21532 ) ;
#9118 = CARTESIAN_POINT ( 'NONE',  ( -0.1787899950787401604, -1.026574803095842370, 0.07405724077823318263 ) ) ;
#9119 = CIRCLE ( 'NONE', #35900, 0.09842519685039370636 ) ;
#9120 = CARTESIAN_POINT ( 'NONE',  ( 3.284318927891251994E-17, -1.171751968450173154, 0.1787899950787401882 ) ) ;
#9121 = FACE_OUTER_BOUND ( 'NONE', #21012, .T. ) ;
#9122 = ( CONVERSION_BASED_UNIT ( 'INCH', #27605 ) LENGTH_UNIT ( ) NAMED_UNIT ( #20041 ) ) ;
#9123 = CARTESIAN_POINT ( 'NONE',  ( 0.9500414927467378812, -0.1787899950787401604, 1.825787401521040243 ) ) ;
#9124 = CARTESIAN_POINT ( 'NONE',  ( -1.100456976456230270E-17, -0.5226816048586362395, -0.1797182628040039365 ) ) ;
#9125 = CARTESIAN_POINT ( 'NONE',  ( -0.8759842519685039353, 0.1574803149606299191, 0.8759842518609765039 ) ) ;
#9126 = CARTESIAN_POINT ( 'NONE',  ( 2.892866454678787531E-17, -0.05708661417322834220, 0.1574803149606299191 ) ) ;
#9127 = CARTESIAN_POINT ( 'NONE',  ( 0.9500414927467378812, -0.1787899950787401604, 0.9596456692375764375 ) ) ;
#9129 = CARTESIAN_POINT ( 'NONE',  ( 0.000000000000000000, 0.1193342091828950846, 0.06889763779527559306 ) ) ;
#9128 = CARTESIAN_POINT ( 'NONE',  ( 0.7646288533564489232, 0.1113553986120547346, 0.6151574803149606474 ) ) ;
#9130 = CARTESIAN_POINT ( 'NONE',  ( 0.6971942568897648851, 0.07405724077823318263, 1.973425196796630088 ) ) ;
#9131 = EDGE_LOOP ( 'NONE', ( #37475, #440, #37485, #22892 ) ) ;
#9132 = CARTESIAN_POINT ( 'NONE',  ( 0.1264236179284866091, -0.4532480314422991929, -0.1264236179284866091 ) ) ;
#9133 = DIRECTION ( 'NONE',  ( 0.8191520442889798082, 0.000000000000000000, 0.5735764363510631458 ) ) ;
#9134 = CARTESIAN_POINT ( 'NONE',  ( 3.284318927891251994E-17, -1.407972440891118282, 0.1787899950787401882 ) ) ;
#9135 = CARTESIAN_POINT ( 'NONE',  ( 0.6971942568897637749, 2.189545951927499583E-17, 0.3617125983714334359 ) ) ;
#9136 = DIRECTION ( 'NONE',  ( -0.000000000000000000, 1.000000000000000000, -0.000000000000000000 ) ) ;
#9137 = AXIS2_PLACEMENT_3D ( 'NONE', #36669, #14627, #21570 ) ;
#9138 = CARTESIAN_POINT ( 'NONE',  ( -1.002407869896990045, 0.1264236179284866091, 1.877460629867496067 ) ) ;
#9139 = ORIENTED_EDGE ( 'NONE', *, *, #16095, .T. ) ;
#9140 = CARTESIAN_POINT ( 'NONE',  ( -0.8759842519685039353, 0.1787899950787401882, 1.336122047190330786 ) ) ;
#9141 = CARTESIAN_POINT ( 'NONE',  ( 0.8759842519685039353, 0.1787899950787401882, 1.414862204670645829 ) ) ;
#9142 = CARTESIAN_POINT ( 'NONE',  ( 1.033464566929133799, 0.000000000000000000, 0.9448818896562519720 ) ) ;
#9143 = CARTESIAN_POINT ( 'NONE',  ( 0.6971942568897626646, -0.07405724077823297447, 0.08858267711159097113 ) ) ;
#9144 = CARTESIAN_POINT ( 'NONE',  ( -0.7495606340400177148, -0.1264236179284866091, 1.267224409395055096 ) ) ;
#9145 = CARTESIAN_POINT ( 'NONE',  ( 0.1574803149606299191, 3.616083068348484413E-17, -0.2952755905511810774 ) ) ;
#9146 = SURFACE_STYLE_USAGE ( .BOTH. , #39067 ) ;
#9147 = CARTESIAN_POINT ( 'NONE',  ( 0.8759842519685039353, -0.1787899950787401882, 0.6077755904974173617 ) ) ;
#9148 = CARTESIAN_POINT ( 'NONE',  ( -0.8759842519685039353, -0.1787899950787401882, 0.5634842519147401640 ) ) ;
#9149 = CARTESIAN_POINT ( 'NONE',  ( 0.1766724065111454356, -0.08549467455806485094, -0.1834299084079261122 ) ) ;
#9150 = EDGE_CURVE ( 'NONE', #34943, #15113, #36409, .T. ) ;
#9151 = CARTESIAN_POINT ( 'NONE',  ( -0.1184675242425147629, -0.5708661417322835607, 1.161904259418922170 ) ) ;
#9152 = ORIENTED_EDGE ( 'NONE', *, *, #15833, .F. ) ;
#9153 = CARTESIAN_POINT ( 'NONE',  ( -0.9873396505805591694, -0.1113553986120547346, 0.2805118110236220486 ) ) ;
#9154 = CARTESIAN_POINT ( 'NONE',  ( 1.002407869896990045, 0.1264236179284866091, 1.213090551127338435 ) ) ;
#9155 = CARTESIAN_POINT ( 'NONE',  ( -0.1397933335164911473, -0.09851385033795964641, 0.1854247136317299371 ) ) ;
#9156 = CARTESIAN_POINT ( 'NONE',  ( -0.2559055118110236671, -0.09125550413757829715, -0.06117675834108277783 ) ) ;
#9157 = ORIENTED_EDGE ( 'NONE', *, *, #40291, .T. ) ;
#9158 = ADVANCED_FACE ( 'NONE', ( #14588 ), #43805, .T. ) ;
#9159 = DIRECTION ( 'NONE',  ( 1.000000000000000000, 0.000000000000000000, 0.000000000000000000 ) ) ;
#9160 = CARTESIAN_POINT ( 'NONE',  ( -0.8759842519685039353, -0.1787899950787401882, 0.9227362204186770889 ) ) ;
#9161 = CARTESIAN_POINT ( 'NONE',  ( -0.8019270111902717657, -0.1787899950787401604, 0.2066929133320631329 ) ) ;
#9162 = CARTESIAN_POINT ( 'NONE',  ( 0.1787899950787401604, -1.569021606024515014, -0.07405724077823318263 ) ) ;
#9163 = ORIENTED_EDGE ( 'NONE', *, *, #9953, .F. ) ;
#9164 = CARTESIAN_POINT ( 'NONE',  ( 0.7185039370078739607, 1.928577636452523993E-17, 1.013779527559055094 ) ) ;
#9165 = CARTESIAN_POINT ( 'NONE',  ( -0.1264236179284866091, -0.5565944881352126172, -0.1264236179284866091 ) ) ;
#9166 = CARTESIAN_POINT ( 'NONE',  ( -0.2834275672170630811, -0.1259372798753287670, 0.9866696916589494659 ) ) ;
#9167 = ORIENTED_EDGE ( 'NONE', *, *, #19719, .T. ) ;
#9168 = CARTESIAN_POINT ( 'NONE',  ( 0.9500414927467378812, -0.1787899950787401604, 1.353346456639149986 ) ) ;
#9169 = CARTESIAN_POINT ( 'NONE',  ( -0.1476377952755905387, 0.06415291647593691915, -0.1630605872086743346 ) ) ;
#9170 = CONICAL_SURFACE ( 'NONE', #31403, 0.1574803149606299191, 0.9599310885968735940 ) ;
#9171 = CARTESIAN_POINT ( 'NONE',  ( 1.054774247047244096, 0.000000000000000000, 1.596948818843874074 ) ) ;
#9172 = CARTESIAN_POINT ( 'NONE',  ( -0.07405724077823318263, -0.02374601547333323251, -0.1787899950787401604 ) ) ;
#9173 = CARTESIAN_POINT ( 'NONE',  ( -1.094772975963752103E-17, -1.781988188922614347, -0.1787899950787401882 ) ) ;
#9174 = ITEM_DEFINED_TRANSFORMATION ( 'NONE', 'NONE', #10972,  #20860 ) ;
#9175 = DIRECTION ( 'NONE',  ( 0.000000000000000000, 0.000000000000000000, 1.000000000000000000 ) ) ;
#9176 = VECTOR ( 'NONE', #19339, 39.37007874015748143 ) ;
#9177 = ADVANCED_FACE ( 'NONE', ( #22473 ), #4218, .T. ) ;
#9178 = ( BOUNDED_CURVE ( )  B_SPLINE_CURVE ( 2, ( #35069, #24743, #20668, #39106, #6280, #46536, #23801, #13034, #2686 ),
 .UNSPECIFIED., .F., .T. ) 
 B_SPLINE_CURVE_WITH_KNOTS ( ( 3, 2, 2, 2, 3 ),
 ( 0.6099999999999999867, 0.6125000000000000444, 0.6149999999999999911, 0.6175000000000000488, 0.6199999999999999956 ),
 .UNSPECIFIED. ) 
 CURVE ( )  GEOMETRIC_REPRESENTATION_ITEM ( )  RATIONAL_B_SPLINE_CURVE ( ( 1.000000000000000000, 0.9238795325112899581, 1.000000000000000000, 0.9238795325112869605, 1.000000000000000000, 0.9238795325112869605, 1.000000000000000000, 0.9238795325112869605, 1.000000000000000000 ) ) 
 REPRESENTATION_ITEM ( '' )  ) ;
#9179 = CARTESIAN_POINT ( 'NONE',  ( -0.7495606340400177148, 0.1264236179284866091, 0.8292322834108031282 ) ) ;
#9181 = PLANE ( 'NONE',  #23201 ) ;
#9180 = CARTESIAN_POINT ( 'NONE',  ( 0.1574803149606300301, -0.9158464566929129802, 0.06523048226347956391 ) ) ;
#9183 = CARTESIAN_POINT ( 'NONE',  ( -0.8092022386113262300, -0.1589064940435495621, 1.986942102874373228 ) ) ;
#9182 = CARTESIAN_POINT ( 'NONE',  ( -0.1270800023317771588, -1.541382392260210565, -0.1270800023317771588 ) ) ;
#9184 = CARTESIAN_POINT ( 'NONE',  ( 0.07405724077823318263, -0.4064960629383624346, -0.1787899950787401604 ) ) ;
#9185 = CARTESIAN_POINT ( 'NONE',  ( 0.6971942568897648851, 0.07405724077823318263, 1.500984251914741607 ) ) ;
#9186 = CARTESIAN_POINT ( 'NONE',  ( 0.8019270111902716547, -0.1787899950787401604, 1.860236220418677089 ) ) ;
#9187 = CARTESIAN_POINT ( 'NONE',  ( 1.054774247047244540, -0.07405724077823318263, 0.3740157479777325711 ) ) ;
#9188 = LINE ( 'NONE', #1273, #10001 ) ;
#9189 = LINE ( 'NONE', #19966, #28958 ) ;
#9190 = LINE ( 'NONE', #19500, #9115 ) ;
#9191 = CARTESIAN_POINT ( 'NONE',  ( -0.1787899950787401604, 0.03641732288840918152, 0.07405724077823318263 ) ) ;
#9192 = CARTESIAN_POINT ( 'NONE',  ( 0.9500414927467378812, -0.1787899950787401604, 0.4084645668753704717 ) ) ;
#9193 = CARTESIAN_POINT ( 'NONE',  ( 0.8084376188356441340, -0.1475773522112547032, 0.03937232269030457865 ) ) ;
#9194 = CARTESIAN_POINT ( 'NONE',  ( -0.7185039370078746268, 0.06523048226347956391, 1.719980314960630086 ) ) ;
#9195 = CARTESIAN_POINT ( 'NONE',  ( 0.8107537697050254399, 0.1574803149606300301, 0.8489173228346468258 ) ) ;
#9196 = CARTESIAN_POINT ( 'NONE',  ( -0.7495606340400177148, -0.1264236179284866091, 1.503444881836000002 ) ) ;
#9197 = CARTESIAN_POINT ( 'NONE',  ( 1.033464566929134687, -0.06523048226347956391, 0.8636811022546767580 ) ) ;
#9198 = ORIENTED_EDGE ( 'NONE', *, *, #12903, .F. ) ;
#9199 = LINE ( 'NONE', #23817, #9249 ) ;
#9200 = CARTESIAN_POINT ( 'NONE',  ( 0.8019270111902717657, -0.1787899950787401604, 1.077755905458048113 ) ) ;
#9201 = ORIENTED_EDGE ( 'NONE', *, *, #27851, .F. ) ;
#9203 = CARTESIAN_POINT ( 'NONE',  ( 0.1264236179284866091, -1.398129921206078707, -0.1264236179284866091 ) ) ;
#9202 = CARTESIAN_POINT ( 'NONE',  ( -0.1574803149606297803, -1.078248031388536754, 0.06523048226347956391 ) ) ;
#9204 = CARTESIAN_POINT ( 'NONE',  ( -1.033464566929134687, -0.06523048226347956391, 0.6274606298137325178 ) ) ;
#9205 = CARTESIAN_POINT ( 'NONE',  ( -1.033464566929134687, -0.06523048226347956391, 1.227854330708661124 ) ) ;
#9206 = CARTESIAN_POINT ( 'NONE',  ( -0.9412147342319837628, -0.1574803149606297803, 1.380413385826771977 ) ) ;
#9207 = CARTESIAN_POINT ( 'NONE',  ( 1.033464566929134687, 0.06523048226347956391, 0.2386811022546777294 ) ) ;
#9209 = CARTESIAN_POINT ( 'NONE',  ( 1.033464566929134687, 0.06523048226347956391, 1.941437007874014187 ) ) ;
#9208 = DIRECTION ( 'NONE',  ( 1.000000000000000000, 0.000000000000000000, -1.822029033848725275E-16 ) ) ;
#9210 = CARTESIAN_POINT ( 'NONE',  ( 1.054774247047244540, -0.07405724077823318263, 0.1427165353793073133 ) ) ;
#9211 = CARTESIAN_POINT ( 'NONE',  ( 0.8107537697050253289, -0.1574803149606297803, 1.483759842412158525 ) ) ;
#9212 = ORIENTED_EDGE ( 'NONE', *, *, #11332, .F. ) ;
#9213 = VERTEX_POINT ( 'NONE', #15072 ) ;
#9214 = ( BOUNDED_CURVE ( )  B_SPLINE_CURVE ( 2, ( #22699, #11698, #33285, #32805, #33763, #25611, #40642, #19093, #872 ),
 .UNSPECIFIED., .F., .F. ) 
 B_SPLINE_CURVE_WITH_KNOTS ( ( 3, 2, 2, 2, 3 ),
 ( 0.2999999999999999889, 0.3024999999999999911, 0.3049999999999999933, 0.3074999999999999956, 0.3099999999999999978 ),
 .UNSPECIFIED. ) 
 CURVE ( )  GEOMETRIC_REPRESENTATION_ITEM ( )  RATIONAL_B_SPLINE_CURVE ( ( 1.000000000000000000, 0.9238795325112869605, 1.000000000000000000, 0.9238795325112869605, 1.000000000000000000, 0.9238795325112869605, 1.000000000000000000, 0.9238795325112869605, 1.000000000000000000 ) ) 
 REPRESENTATION_ITEM ( '' )  ) ;
#9215 = EDGE_CURVE ( 'NONE', #7112, #44436, #8505, .T. ) ;
#9216 = VECTOR ( 'NONE', #23052, 39.37007874015748143 ) ;
#9217 = CARTESIAN_POINT ( 'NONE',  ( 3.284318927891251994E-17, 0.1225393701325037388, 0.1787899950787401882 ) ) ;
#9218 = CARTESIAN_POINT ( 'NONE',  ( -0.06175619828051706617, -0.08093302715459128882, -0.2497778431879683070 ) ) ;
#9219 = DIRECTION ( 'NONE',  ( -1.151683635503274519E-16, -0.000000000000000000, -1.000000000000000000 ) ) ;
#9220 = CARTESIAN_POINT ( 'NONE',  ( 0.8019270111902717657, 0.1787899950787401604, 0.7086614172690703928 ) ) ;
#9221 = CARTESIAN_POINT ( 'NONE',  ( -1.054774247047244540, -0.07405724077823318263, 1.751968503883245987 ) ) ;
#9222 = CARTESIAN_POINT ( 'NONE',  ( 0.1113553986120547346, -0.1998031494987720369, 0.1113553986120547346 ) ) ;
#9223 = AXIS2_PLACEMENT_3D ( 'NONE', #8000, #18549, #29403 ) ;
#9224 = EDGE_CURVE ( 'NONE', #13621, #19295, #13423, .T. ) ;
#9225 = AXIS2_PLACEMENT_3D ( 'NONE', #11768, #26141, #26387 ) ;
#9226 = ORIENTED_EDGE ( 'NONE', *, *, #22462, .T. ) ;
#9227 = DIRECTION ( 'NONE',  ( 0.000000000000000000, 0.000000000000000000, -1.000000000000000000 ) ) ;
#9228 = CARTESIAN_POINT ( 'NONE',  ( 0.08946752424252873981, -0.5708661417322835607, 1.224299699984019663 ) ) ;
#9229 = CARTESIAN_POINT ( 'NONE',  ( -0.1264236179284866091, -1.163017669016639832, -0.1264236179284866091 ) ) ;
#9230 = ORIENTED_EDGE ( 'NONE', *, *, #38271, .T. ) ;
#9231 = CARTESIAN_POINT ( 'NONE',  ( 0.1264236179284866091, -0.1727362204186775607, -0.1264236179284866091 ) ) ;
#9232 = ORIENTED_EDGE ( 'NONE', *, *, #12641, .T. ) ;
#9233 = ORIENTED_EDGE ( 'NONE', *, *, #44717, .T. ) ;
#9234 = CARTESIAN_POINT ( 'NONE',  ( -0.2559055118110236116, -0.1477471161312047254, -0.2921040715117803055 ) ) ;
#9235 = CARTESIAN_POINT ( 'NONE',  ( -0.7646288533564489232, -0.1113553986120547346, 1.451771653543306950 ) ) ;
#9236 = CARTESIAN_POINT ( 'NONE',  ( 0.7185039370078739607, 1.928577636452523993E-17, 1.761811023622047223 ) ) ;
#9237 = CARTESIAN_POINT ( 'NONE',  ( -0.07405724077823318263, -0.6673228345919050009, 0.1787899950787401604 ) ) ;
#9238 = ADVANCED_FACE ( 'NONE', ( #18869 ), #29719, .F. ) ;
#9239 = AXIS2_PLACEMENT_3D ( 'NONE', #19213, #30507, #22810 ) ;
#9240 = CARTESIAN_POINT ( 'NONE',  ( -0.6971942568897637749, 2.189545951927499583E-17, 0.4010826771115905687 ) ) ;
#9241 = CARTESIAN_POINT ( 'NONE',  ( -0.8107537697050253289, -0.1574803149606297803, 1.060531496062992352 ) ) ;
#9242 = CARTESIAN_POINT ( 'NONE',  ( -0.1797182628040039087, -1.179669793835013358, 0.07444174185955065859 ) ) ;
#9243 = DIRECTION ( 'NONE',  ( -1.000000000000000000, 0.000000000000000000, 0.000000000000000000 ) ) ;
#9244 = CARTESIAN_POINT ( 'NONE',  ( 0.6971942568897648851, -0.07405724077823297447, 1.033464566875371027 ) ) ;
#9245 = CARTESIAN_POINT ( 'NONE',  ( 0.8019270111902716547, 0.1787899950787401604, 0.2312992125446618197 ) ) ;
#9246 = AXIS2_PLACEMENT_3D ( 'NONE', #3714, #10688, #21205 ) ;
#9247 = CARTESIAN_POINT ( 'NONE',  ( 0.7646288533564489232, -0.1113553986120547346, 1.609251968503937036 ) ) ;
#9248 = CARTESIAN_POINT ( 'NONE',  ( 0.8759842519685039353, -0.1574803149606299191, 1.417322834645669216 ) ) ;
#9249 = VECTOR ( 'NONE', #45372, 39.37007874015748143 ) ;
#9250 = FACE_OUTER_BOUND ( 'NONE', #45613, .T. ) ;
#9251 = CARTESIAN_POINT ( 'NONE',  ( 0.06523048226347956391, -0.7386811022546784233, -0.1574803149606300301 ) ) ;
#9252 = CARTESIAN_POINT ( 'NONE',  ( 0.4736248074375590811, 1.914733266569315084, -0.6843357808987579061 ) ) ;
#9253 = CARTESIAN_POINT ( 'NONE',  ( 0.9500414927467377701, 0.1787899950787401604, 1.053149606245450176 ) ) ;
#9254 = DIRECTION ( 'NONE',  ( -1.000000000000000000, 0.000000000000000000, 0.000000000000000000 ) ) ;
#9255 = CARTESIAN_POINT ( 'NONE',  ( 0.7646288533564489232, -0.1113553986120547346, 0.3789370077664886427 ) ) ;
#9256 = ORIENTED_EDGE ( 'NONE', *, *, #44505, .F. ) ;
#9257 = AXIS2_PLACEMENT_3D ( 'NONE', #3046, #24877, #43542 ) ;
#9258 = ADVANCED_FACE ( 'NONE', ( #643 ), #15789, .T. ) ;
#9259 = CARTESIAN_POINT ( 'NONE',  ( 0.7646288533564489232, -0.1113553986120547346, 1.245078740049952559 ) ) ;
#9260 = ADVANCED_FACE ( 'NONE', ( #1130 ), #26336, .T. ) ;
#9261 = CARTESIAN_POINT ( 'NONE',  ( 0.1574803149606300301, -1.649114173120819649, -0.06523048226347956391 ) ) ;
#9262 = CARTESIAN_POINT ( 'NONE',  ( -0.8107537697050234415, -0.1574803149606297803, 0.2239173227271187561 ) ) ;
#9263 = ORIENTED_EDGE ( 'NONE', *, *, #32223, .T. ) ;
#9264 = CARTESIAN_POINT ( 'NONE',  ( 0.07405724077823318263, -0.09153543301710270752, -0.1787899950787401604 ) ) ;
#9265 = CARTESIAN_POINT ( 'NONE',  ( 0.8759842519685039353, 0.1787899950787401882, 1.252460629867496067 ) ) ;
#9266 = CARTESIAN_POINT ( 'NONE',  ( 0.9873396505805591694, 0.1113553986120547346, 1.225393700679874076 ) ) ;
#9267 = CARTESIAN_POINT ( 'NONE',  ( -0.1787899950787401604, 0.08070866147108628208, 0.07405724077823318263 ) ) ;
#9268 = CARTESIAN_POINT ( 'NONE',  ( 0.2759478392031586291, -0.5708661417322835607, 1.224299699984019663 ) ) ;
#9269 = ADVANCED_FACE ( 'NONE', ( #26571 ), #37564, .T. ) ;
#9270 = CARTESIAN_POINT ( 'NONE',  ( -0.8759842519685039353, -0.1787899950787401882, 0.6422244093950550958 ) ) ;
#9271 = CARTESIAN_POINT ( 'NONE',  ( 0.9873396505805591694, -0.1113553986120547346, 1.373031495955464587 ) ) ;
#9272 = CYLINDRICAL_SURFACE ( 'NONE', #7760, 0.1864803149606299171 ) ;
#9273 = ORIENTED_EDGE ( 'NONE', *, *, #10464, .F. ) ;
#9274 = ORIENTED_EDGE ( 'NONE', *, *, #33152, .F. ) ;
#9275 = CARTESIAN_POINT ( 'NONE',  ( 3.284318927891251994E-17, -1.727854330654897685, 0.1787899950787401882 ) ) ;
#9276 = CARTESIAN_POINT ( 'NONE',  ( -1.002407869896990045, 0.1264236179284866091, 0.9374999999462362288 ) ) ;
#9277 = CARTESIAN_POINT ( 'NONE',  ( -0.8107537697050234415, -0.1574803149606297803, 0.03690944881889771101 ) ) ;
#9278 = ORIENTED_EDGE ( 'NONE', *, *, #32814, .T. ) ;
#9279 = CARTESIAN_POINT ( 'NONE',  ( -0.7495606340400177148, 0.1264236179284866091, 0.6323818897100157432 ) ) ;
#9280 = ORIENTED_EDGE ( 'NONE', *, *, #28375, .F. ) ;
#9281 = VECTOR ( 'NONE', #45470, 39.37007874015748143 ) ;
#9282 = ADVANCED_FACE ( 'NONE', ( #40548, #4138, #18759 ), #764, .F. ) ;
#9283 = LINE ( 'NONE', #4958, #22201 ) ;
#9284 = CARTESIAN_POINT ( 'NONE',  ( -0.3100393700787401619, 3.218313930830148909E-16, -1.043307086614172707 ) ) ;
#9285 = CARTESIAN_POINT ( 'NONE',  ( 0.1787899950787401604, -0.7471712123237258529, 0.07405724077823318263 ) ) ;
#9286 = EDGE_LOOP ( 'NONE', ( #33720, #2563, #822, #27835 ) ) ;
#9287 = CARTESIAN_POINT ( 'NONE',  ( -0.1531176995717757894, -0.08956120967700866020, -0.08476774985902559012 ) ) ;
#9288 = DIRECTION ( 'NONE',  ( 0.000000000000000000, 0.000000000000000000, -1.000000000000000000 ) ) ;
#9289 = ORIENTED_EDGE ( 'NONE', *, *, #15332, .F. ) ;
#9290 = DIRECTION ( 'NONE',  ( 0.000000000000000000, -1.000000000000000000, 0.000000000000000000 ) ) ;
#9291 = AXIS2_PLACEMENT_3D ( 'NONE', #25082, #39674, #39920 ) ;
#9292 = CARTESIAN_POINT ( 'NONE',  ( -1.033464566929134687, -0.06523048226347956391, 1.178641732175937040 ) ) ;
#9293 = CARTESIAN_POINT ( 'NONE',  ( -0.9500414927467378812, 0.1787899950787401604, 0.4232283464029293896 ) ) ;
#9294 = CARTESIAN_POINT ( 'NONE',  ( 0.7185039370078714072, 0.06523048226347728795, 1.355807086506647829 ) ) ;
#9295 = ORIENTED_EDGE ( 'NONE', *, *, #6320, .T. ) ;
#9296 = CARTESIAN_POINT ( 'NONE',  ( -0.6971942568897648851, 0.07405724077823318263, 1.697834645615527771 ) ) ;
#9297 = CARTESIAN_POINT ( 'NONE',  ( -1.094772975963752103E-17, -1.432578740103716664, -0.1787899950787401882 ) ) ;
#9298 = LINE ( 'NONE', #23677, #1944 ) ;
#9299 = CARTESIAN_POINT ( 'NONE',  ( 1.033464566929134687, 0.06523048226347956391, 0.5634842519685042683 ) ) ;
#9300 = CARTESIAN_POINT ( 'NONE',  ( -0.1797182628040039087, -0.7465989276932815111, 0.07444174185955065859 ) ) ;
#9301 = CARTESIAN_POINT ( 'NONE',  ( 0.7646288533564489232, -0.1113553986120547346, 0.9399606299212598381 ) ) ;
#9302 = CARTESIAN_POINT ( 'NONE',  ( -1.033464566929134687, 0.06523048226347956391, 1.301673228238930502 ) ) ;
#9304 = CARTESIAN_POINT ( 'NONE',  ( 0.8759842519685039353, -0.1574803149606299191, 0.3543307086614173040 ) ) ;
#9303 = CARTESIAN_POINT ( 'NONE',  ( 2.892866454678787531E-17, -0.4114173228346456601, 0.1574803149606299191 ) ) ;
#9305 = CARTESIAN_POINT ( 'NONE',  ( -0.7185039370078739607, 1.928577636452523993E-17, 1.200787401467275695 ) ) ;
#9306 = EDGE_LOOP ( 'NONE', ( #20771, #689, #35472, #31335 ) ) ;
#9307 = EDGE_CURVE ( 'NONE', #12155, #29873, #41016, .T. ) ;
#9308 = CARTESIAN_POINT ( 'NONE',  ( -0.3161444924769509779, 1.449372585305507943, -0.3207561694859686896 ) ) ;
#9309 = CARTESIAN_POINT ( 'NONE',  ( -0.8019270111902716547, -0.1787899950787401604, 1.117125984198206412 ) ) ;
#9310 = CARTESIAN_POINT ( 'NONE',  ( 0.7185039370078746268, -0.06523048226347956391, 1.055610236220473341 ) ) ;
#9311 = CARTESIAN_POINT ( 'NONE',  ( 0.1574803149606300301, 0.08316929144610965552, -0.06523048226347956391 ) ) ;
#9313 = CARTESIAN_POINT ( 'NONE',  ( -0.4338976377952755703, -2.656856766417909227E-17, 0.000000000000000000 ) ) ;
#9312 = DIRECTION ( 'NONE',  ( 1.000000000000000000, 0.000000000000000000, 0.000000000000000000 ) ) ;
#9314 = DIRECTION ( 'NONE',  ( 0.000000000000000000, 0.000000000000000000, -1.000000000000000000 ) ) ;
#9315 = CARTESIAN_POINT ( 'NONE',  ( 0.1113553986120547346, -0.5935039369003465293, 0.1113553986120547346 ) ) ;
#9316 = AXIS2_PLACEMENT_3D ( 'NONE', #15688, #19252, #25590 ) ;
#9318 = CARTESIAN_POINT ( 'NONE',  ( -1.033464566929134687, -0.06523048226347956391, 1.966043306979087246 ) ) ;
#9317 = DIRECTION ( 'NONE',  ( -1.000000000000000000, 0.000000000000000000, 0.000000000000000000 ) ) ;
#9319 = FACE_BOUND ( 'NONE', #13609, .T. ) ;
#9320 = CARTESIAN_POINT ( 'NONE',  ( -1.094772975963752103E-17, -0.6008858267178898149, -0.1787899950787401882 ) ) ;
#9321 = CARTESIAN_POINT ( 'NONE',  ( 0.3425196850393700809, 4.616380251121755931E-17, 0.000000000000000000 ) ) ;
#9322 = ORIENTED_EDGE ( 'NONE', *, *, #2905, .F. ) ;
#9323 = ADVANCED_FACE ( 'NONE', ( #5563 ), #20414, .F. ) ;
#9324 = CYLINDRICAL_SURFACE ( 'NONE', #6911, 0.2362204724409448231 ) ;
#9325 = CIRCLE ( 'NONE', #27719, 0.09842519685039370636 ) ;
#9326 = CARTESIAN_POINT ( 'NONE',  ( 1.033464566929133799, 0.000000000000000000, 1.151574803149606474 ) ) ;
#9327 = CARTESIAN_POINT ( 'NONE',  ( 1.002407869896990045, 0.1264236179284866091, 0.7750984251430865779 ) ) ;
#9328 = ORIENTED_EDGE ( 'NONE', *, *, #2433, .F. ) ;
#9329 = CARTESIAN_POINT ( 'NONE',  ( 1.033464566929134687, -0.06523048226347956391, 1.306594488188977055 ) ) ;
#9330 = CARTESIAN_POINT ( 'NONE',  ( -0.7185039370078739607, 1.928577636452523993E-17, 0.4527559054042842868 ) ) ;
#9331 = CARTESIAN_POINT ( 'NONE',  ( -0.1264236179284866091, -1.737696850339937038, -0.1264236179284866091 ) ) ;
#9332 = CARTESIAN_POINT ( 'NONE',  ( 0.1787899950787401604, -1.085629921206079374, -0.07405724077823318263 ) ) ;
#9333 = VECTOR ( 'NONE', #19848, 39.37007874015748143 ) ;
#9334 = CARTESIAN_POINT ( 'NONE',  ( -9.642888182262618425E-18, -1.375984251968504157, -0.1574803149606299191 ) ) ;
#9335 = SHAPE_REPRESENTATION ( 'Handle Arm Right', ( #20860 ), #27025 ) ;
#9336 = CARTESIAN_POINT ( 'NONE',  ( 0.9412147342319837628, -0.1574803149606297803, 1.173720472333417586 ) ) ;
#9337 = ORIENTED_EDGE ( 'NONE', *, *, #2269, .T. ) ;
#9338 = ORIENTED_EDGE ( 'NONE', *, *, #14169, .T. ) ;
#9339 = CARTESIAN_POINT ( 'NONE',  ( -0.6971942568897648851, -0.07405724077823297447, 1.978346456639149320 ) ) ;
#9340 = CARTESIAN_POINT ( 'NONE',  ( 0.7495606340400177148, -0.1264236179284866091, 1.783956692859621995 ) ) ;
#9341 = ORIENTED_EDGE ( 'NONE', *, *, #35036, .T. ) ;
#9342 = CARTESIAN_POINT ( 'NONE',  ( 0.7646288533564489232, -0.1113553986120547346, 1.766732283464566899 ) ) ;
#9343 = CARTESIAN_POINT ( 'NONE',  ( -0.8759842519685039353, 0.1787899950787401882, 1.331200787347811110 ) ) ;
#9344 = CARTESIAN_POINT ( 'NONE',  ( 0.08209939101888709401, 0.2480946695747454911, -0.3118411609178523558 ) ) ;
#9345 = CARTESIAN_POINT ( 'NONE',  ( -0.8759842519685039353, -0.1787899950787401882, 0.9965551180564724554 ) ) ;
#9346 = CARTESIAN_POINT ( 'NONE',  ( -0.6971942568897626646, 0.07405724077823318263, 0.2411417322297011168 ) ) ;
#9347 = CARTESIAN_POINT ( 'NONE',  ( 1.033464566929133799, 0.000000000000000000, 1.584645669291338654 ) ) ;
#9348 = CARTESIAN_POINT ( 'NONE',  ( -0.8019270111902717657, 0.1787899950787401604, 1.771653543253322249 ) ) ;
#9349 = CARTESIAN_POINT ( 'NONE',  ( -0.7646288533564489232, 0.1113553986120547346, 1.796259842519684957 ) ) ;
#9350 = CARTESIAN_POINT ( 'NONE',  ( -0.8107537697050254399, -0.1574803149606297803, 0.9424212598425207865 ) ) ;
#9351 = CARTESIAN_POINT ( 'NONE',  ( -0.1264236179284866091, -0.3264034957882941401, 0.1264236179284866091 ) ) ;
#9352 = CARTESIAN_POINT ( 'NONE',  ( 1.054774247047244540, -0.07405724077823318263, 1.717519684985606476 ) ) ;
#9353 = CARTESIAN_POINT ( 'NONE',  ( 0.03860301396976173471, -0.09842519685039370636, 0.2192022649856606165 ) ) ;
#9354 = DIRECTION ( 'NONE',  ( -1.000000000000000000, 0.000000000000000000, 0.000000000000000000 ) ) ;
#9355 = ORIENTED_EDGE ( 'NONE', *, *, #38409, .T. ) ;
#9356 = CARTESIAN_POINT ( 'NONE',  ( -0.7495606340400177148, 0.1264236179284866091, 1.262303149552535420 ) ) ;
#9357 = EDGE_LOOP ( 'NONE', ( #42900, #18936, #1403, #37679 ) ) ;
#9358 = AXIS2_PLACEMENT_3D ( 'NONE', #28001, #13588, #10249 ) ;
#9359 = CIRCLE ( 'NONE', #16274, 0.01968503937007874335 ) ;
#9360 = CARTESIAN_POINT ( 'NONE',  ( 0.07405724077823318263, -1.080708661363559919, -0.1787899950787401604 ) ) ;
#9361 = CARTESIAN_POINT ( 'NONE',  ( -0.07405724077823318263, -1.213582677111591623, 0.1787899950787401604 ) ) ;
#9362 = CARTESIAN_POINT ( 'NONE',  ( 0.4208034506101054895, 4.466152701071653354E-17, 0.000000000000000000 ) ) ;
#9363 = CARTESIAN_POINT ( 'NONE',  ( 0.6971942568897637749, 2.189545951927499583E-17, 0.3961614172690708924 ) ) ;
#9364 = CARTESIAN_POINT ( 'NONE',  ( -0.1797182628040039365, -0.4734690064334394211, 0.000000000000000000 ) ) ;
#9365 = CARTESIAN_POINT ( 'NONE',  ( -0.06523048226347956391, -1.796751968396409271, -0.1574803149606300301 ) ) ;
#9366 = CARTESIAN_POINT ( 'NONE',  ( -1.033464566929134687, -0.06523048226347956391, 0.7849409447743628254 ) ) ;
#9367 = CARTESIAN_POINT ( 'NONE',  ( 0.1574803149606300301, 0.06840551181102358380, 0.06523048226347956391 ) ) ;
#9368 = EDGE_CURVE ( 'NONE', #35620, #42894, #38630, .T. ) ;
#9369 = CARTESIAN_POINT ( 'NONE',  ( 0.7495606340400177148, -0.1264236179284866091, 0.8735236219934803259 ) ) ;
#9370 = EDGE_CURVE ( 'NONE', #5180, #25679, #5804, .T. ) ;
#9372 = DIRECTION ( 'NONE',  ( -1.000000000000000000, 0.000000000000000000, 0.000000000000000000 ) ) ;
#9371 = CARTESIAN_POINT ( 'NONE',  ( 0.1030451738609210743, 0.2360010733951117545, -0.03001342526389711579 ) ) ;
#9373 = CARTESIAN_POINT ( 'NONE',  ( 1.033464566929133799, 0.000000000000000000, 0.07874015737278799998 ) ) ;
#9374 = ADVANCED_FACE ( 'NONE', ( #16598 ), #27650, .T. ) ;
#9375 = ORIENTED_EDGE ( 'NONE', *, *, #32024, .T. ) ;
#9376 = EDGE_CURVE ( 'NONE', #27462, #21477, #41957, .T. ) ;
#9377 = FACE_BOUND ( 'NONE', #18186, .T. ) ;
#9378 = CARTESIAN_POINT ( 'NONE',  ( -0.07405724077823318263, -0.5098425196312756924, 0.1787899950787401604 ) ) ;
#9379 = LINE ( 'NONE', #12270, #39265 ) ;
#9380 = CARTESIAN_POINT ( 'NONE',  ( -0.1264236179284866091, -1.343996062938362268, -0.1264236179284866091 ) ) ;
#9381 = CARTESIAN_POINT ( 'NONE',  ( 0.9500414927467378812, -0.1787899950787401604, 0.3346456692375748831 ) ) ;
#9382 = PLANE ( 'NONE',  #21599 ) ;
#9383 = CARTESIAN_POINT ( 'NONE',  ( -0.9500414927467378812, 0.1787899950787401604, 1.919291338528913871 ) ) ;
#9384 = ORIENTED_EDGE ( 'NONE', *, *, #43378, .T. ) ;
#9385 = ORIENTED_EDGE ( 'NONE', *, *, #43935, .F. ) ;
#9386 = CARTESIAN_POINT ( 'NONE',  ( -0.8759842519685039353, 0.1787899950787401882, 1.414862204670645829 ) ) ;
#9387 = CARTESIAN_POINT ( 'NONE',  ( 1.054774247047244540, 0.07405724077823318263, 1.446850393647023614 ) ) ;
#9388 = DIRECTION ( 'NONE',  ( 0.000000000000000000, 0.000000000000000000, -1.000000000000000000 ) ) ;
#9389 = CIRCLE ( 'NONE', #26999, 0.08090551181102362266 ) ;
#9390 = CARTESIAN_POINT ( 'NONE',  ( -1.054774247047244096, 0.000000000000000000, 1.242618110182456714 ) ) ;
#9391 = CARTESIAN_POINT ( 'NONE',  ( 0.1776925020132069377, -0.09842519685039378963, -0.02072179724286548827 ) ) ;
#9392 = CARTESIAN_POINT ( 'NONE',  ( 1.054774247047244540, 0.07405724077823318263, 0.5413385826234012876 ) ) ;
#9393 = CARTESIAN_POINT ( 'NONE',  ( -0.8019270111902716547, -0.1787899950787401604, 0.5610236219934807700 ) ) ;
#9394 = B_SPLINE_CURVE_WITH_KNOTS ( 'NONE', 3,
 ( #25534, #34955, #2334, #28007, #40100, #38770, #35187, #77, #35423, #42352, #14725, #2561, #47068, #14259, #29398, #2100, #16730, #31366 ),
 .UNSPECIFIED., .F., .F.,
 ( 4, 2, 2, 2, 2, 2, 2, 2, 4 ),
 ( 0.000000000000000000, 0.1250000000000001110, 0.2500000000000002220, 0.5000000000000004441, 0.5625000000000003331, 0.6250000000000003331, 0.7500000000000002220, 0.8750000000000001110, 1.000000000000000000 ),
 .UNSPECIFIED. ) ;
#9395 = CARTESIAN_POINT ( 'NONE',  ( 0.2471922904502826812, -0.03219022224904106305, 0.1427165354330708902 ) ) ;
#9396 = CARTESIAN_POINT ( 'NONE',  ( -0.8759842519685039353, 0.000000000000000000, 0.000000000000000000 ) ) ;
#9397 = ORIENTED_EDGE ( 'NONE', *, *, #34588, .T. ) ;
#9398 = PRODUCT ( 'U-Bolt', 'U-Bolt', '', ( #33198 ) ) ;
#9399 = CYLINDRICAL_SURFACE ( 'NONE', #23345, 0.7874015748031495399 ) ;
#9400 = AXIS2_PLACEMENT_3D ( 'NONE', #4318, #8832, #12694 ) ;
#9401 = CARTESIAN_POINT ( 'NONE',  ( -0.7185039370078739607, 1.928577636452523993E-17, 0.3051181102362204856 ) ) ;
#9402 = CARTESIAN_POINT ( 'NONE',  ( 1.054774247047244096, 0.000000000000000000, 1.247539370024976391 ) ) ;
#9403 = CARTESIAN_POINT ( 'NONE',  ( -0.1713386234961888077, -0.09851385174780474818, 0.1582058536542151617 ) ) ;
#9404 = ORIENTED_EDGE ( 'NONE', *, *, #12026, .T. ) ;
#9405 = CARTESIAN_POINT ( 'NONE',  ( -0.8019270111902717657, -0.1787899950787401604, 0.9596456692375764375 ) ) ;
#9406 = CARTESIAN_POINT ( 'NONE',  ( 0.1787899950787401604, -1.608391684764673091, -0.07405724077823318263 ) ) ;
#9407 = ORIENTED_EDGE ( 'NONE', *, *, #4150, .F. ) ;
#9408 = CARTESIAN_POINT ( 'NONE',  ( -0.8759842519685039353, 0.1574803149606299191, 1.387795275483023616 ) ) ;
#9409 = CARTESIAN_POINT ( 'NONE',  ( 0.07405724077823318263, -0.6427165353793066194, -0.1787899950787401604 ) ) ;
#9410 = CARTESIAN_POINT ( 'NONE',  ( -0.3100393700787403284, -0.01116717051762142893, 1.043307086614172929 ) ) ;
#9411 = VERTEX_POINT ( 'NONE', #16818 ) ;
#9412 = CARTESIAN_POINT ( 'NONE',  ( 0.6971942568897648851, -0.07405724077823297447, 1.382874015694268044 ) ) ;
#9413 = AXIS2_PLACEMENT_3D ( 'NONE', #20140, #34786, #45763 ) ;
#9414 = CARTESIAN_POINT ( 'NONE',  ( -0.09806891812766166394, 0.2388741431483011879, -0.3136338785706627164 ) ) ;
#9415 = CARTESIAN_POINT ( 'NONE',  ( -0.1264236179284866091, -0.3646653542769452971, -0.1264236179284866091 ) ) ;
#9416 = CARTESIAN_POINT ( 'NONE',  ( 0.07405724077823318263, -0.6968503936470246130, 0.1787899950787401604 ) ) ;
#9417 = AXIS2_PLACEMENT_3D ( 'NONE', #29370, #3185, #14231 ) ;
#9418 = DIRECTION ( 'NONE',  ( -1.000000000000000000, 0.000000000000000000, 0.000000000000000000 ) ) ;
#9419 = DIRECTION ( 'NONE',  ( -1.000000000000000000, 0.000000000000000000, 0.000000000000000000 ) ) ;
#9420 = CARTESIAN_POINT ( 'NONE',  ( 0.8759842519685039353, 0.1787899950787401882, 1.646161417269070837 ) ) ;
#9421 = ( GEOMETRIC_REPRESENTATION_CONTEXT ( 3 ) GLOBAL_UNCERTAINTY_ASSIGNED_CONTEXT ( ( #10162 ) ) GLOBAL_UNIT_ASSIGNED_CONTEXT ( ( #26700, #30090, #23331 ) ) REPRESENTATION_CONTEXT ( 'NONE', 'WORKASPACE' ) ) ;
#9422 = VECTOR ( 'NONE', #20147, 39.37007874015748854 ) ;
#9423 = CARTESIAN_POINT ( 'NONE',  ( -1.094772975963752103E-17, 0.09190359082587953865, -0.1787899950787401882 ) ) ;
#9424 = CARTESIAN_POINT ( 'NONE',  ( -0.07405724077823318263, 0.1200787402112438867, 0.1787899950787401604 ) ) ;
#9425 = CARTESIAN_POINT ( 'NONE',  ( 0.09212567409445292232, -0.09842519685039373412, 0.1397575628899831168 ) ) ;
#9426 = EDGE_CURVE ( 'NONE', #32512, #37199, #19834, .T. ) ;
#9427 = CARTESIAN_POINT ( 'NONE',  ( -0.9500414927467377701, 0.1787899950787401604, 0.7824803149068668695 ) ) ;
#9429 = CARTESIAN_POINT ( 'NONE',  ( 0.9873396505805591694, 0.1113553986120547346, 0.08366141721530767628 ) ) ;
#9428 = CARTESIAN_POINT ( 'NONE',  ( 0.1574803149606300301, -0.8321850393700797044, -0.06523048226347956391 ) ) ;
#9431 = CARTESIAN_POINT ( 'NONE',  ( -0.8003469732030862316, -0.1545552040134573757, 1.986757990405105145 ) ) ;
#9430 = CARTESIAN_POINT ( 'NONE',  ( 0.1270800023317771588, -1.521697352890131638, 0.1270800023317771588 ) ) ;
#9432 = CARTESIAN_POINT ( 'NONE',  ( 0.07405724077823318263, -0.3277559054580475584, -0.1787899950787401604 ) ) ;
#9433 = DIRECTION ( 'NONE',  ( 1.000000000000000000, 0.000000000000000000, 0.000000000000000000 ) ) ;
#9434 = CARTESIAN_POINT ( 'NONE',  ( 0.6971942568897648851, -0.07405724077823297447, 1.505905511757261284 ) ) ;
#9435 = CARTESIAN_POINT ( 'NONE',  ( 0.1550283333641064298, 0.09383642490574126138, -0.1959274208663558947 ) ) ;
#9436 = CARTESIAN_POINT ( 'NONE',  ( 1.002407869896990045, 0.1264236179284866091, 0.3420275590013546751 ) ) ;
#9437 = EDGE_LOOP ( 'NONE', ( #4819, #14648, #41256, #14511, #33723 ) ) ;
#9439 = ORIENTED_EDGE ( 'NONE', *, *, #44066, .T. ) ;
#9438 = LINE ( 'NONE', #19497, #11544 ) ;
#9440 = EDGE_CURVE ( 'NONE', #36149, #20507, #24737, .T. ) ;
#9441 = CARTESIAN_POINT ( 'NONE',  ( 3.060083392313581123E-15, 0.9310112235910578127, -1.064878870394357468 ) ) ;
#9442 = FACE_OUTER_BOUND ( 'NONE', #15304, .T. ) ;
#9444 = CARTESIAN_POINT ( 'NONE',  ( -0.1787899950787401604, 0.07086614178604697112, -0.07405724077823318263 ) ) ;
#9443 = CARTESIAN_POINT ( 'NONE',  ( 0.1113553986120547346, -0.8690944880814488460, 0.1113553986120547346 ) ) ;
#9445 = CARTESIAN_POINT ( 'NONE',  ( 1.002407869896990045, -0.1264236179284866091, 0.4109251967966299213 ) ) ;
#9446 = CARTESIAN_POINT ( 'NONE',  ( -0.07405724077823318263, -0.9527559054580476694, -0.1787899950787401604 ) ) ;
#9447 = CARTESIAN_POINT ( 'NONE',  ( 0.7609004089021561557, -0.1193751119366993352, 0.03937007863495575050 ) ) ;
#9449 = CARTESIAN_POINT ( 'NONE',  ( 1.033464566929134687, 0.06523048226347956391, 1.970964566821606034 ) ) ;
#9448 = CARTESIAN_POINT ( 'NONE',  ( 1.054774247047244096, 0.000000000000000000, 1.321358267662771757 ) ) ;
#9450 = CARTESIAN_POINT ( 'NONE',  ( -0.6971942568897637749, 2.189545951927499583E-17, 1.380413385773007873 ) ) ;
#9451 = CARTESIAN_POINT ( 'NONE',  ( 1.033464566929133799, 0.000000000000000000, 0.7480314959554645871 ) ) ;
#9452 = ORIENTED_EDGE ( 'NONE', *, *, #40711, .F. ) ;
#9453 = CARTESIAN_POINT ( 'NONE',  ( 0.1574803149606300023, -0.2237541348899636795, -1.272196386806235813 ) ) ;
#9454 = CARTESIAN_POINT ( 'NONE',  ( 0.7495606340400177148, -0.1264236179284866091, 0.9571850393163149340 ) ) ;
#9455 = EDGE_LOOP ( 'NONE', ( #17080, #1314, #13723, #45795 ) ) ;
#9456 = CARTESIAN_POINT ( 'NONE',  ( -0.8107537697050253289, 0.1574803149606300301, 0.6422244093412926569 ) ) ;
#9457 = CARTESIAN_POINT ( 'NONE',  ( -0.7185039370078746268, -0.06523048226347956391, 1.370570866141733291 ) ) ;
#9458 = CARTESIAN_POINT ( 'NONE',  ( -0.7185039370078739607, 1.928577636452523993E-17, 0.5314960628845992741 ) ) ;
#9460 = DIRECTION ( 'NONE',  ( 0.000000000000000000, -1.000000000000000000, 0.000000000000000000 ) ) ;
#9459 = CARTESIAN_POINT ( 'NONE',  ( 0.4330708661417322913, 0.000000000000000000, 0.000000000000000000 ) ) ;
#9461 = CARTESIAN_POINT ( 'NONE',  ( 0.8019270111902716547, 0.1787899950787401604, 0.07874015742655143812 ) ) ;
#9462 = CARTESIAN_POINT ( 'NONE',  ( -0.9500414927467377701, 0.1787899950787401604, 0.1082677164816695514 ) ) ;
#9463 = CARTESIAN_POINT ( 'NONE',  ( 0.9412147342319837628, -0.1574803149606297803, 1.409940944774363825 ) ) ;
#9464 = VERTEX_POINT ( 'NONE', #16370 ) ;
#9465 = ORIENTED_EDGE ( 'NONE', *, *, #40868, .F. ) ;
#9466 = CARTESIAN_POINT ( 'NONE',  ( 0.4620708661417330387, 0.1864803149606299171, 1.186023622047243986 ) ) ;
#9467 = CARTESIAN_POINT ( 'NONE',  ( 0.2314997995717387735, -0.1618377606623210563, -0.08364281214761010164 ) ) ;
#9468 = ORIENTED_EDGE ( 'NONE', *, *, #11817, .T. ) ;
#9469 = CARTESIAN_POINT ( 'NONE',  ( -0.6971942568897648851, 0.07405724077823318263, 1.653543307032850462 ) ) ;
#9470 = AXIS2_PLACEMENT_3D ( 'NONE', #43818, #18194, #47190 ) ;
#9471 = ORIENTED_EDGE ( 'NONE', *, *, #5862, .F. ) ;
#9472 = CARTESIAN_POINT ( 'NONE',  ( -1.033464566929133799, 0.000000000000000000, 1.899606299212598604 ) ) ;
#9473 = CARTESIAN_POINT ( 'NONE',  ( -0.1673228346456692994, 0.06245656531175331622, -0.1492449156640640040 ) ) ;
#9474 = CARTESIAN_POINT ( 'NONE',  ( 1.033464566929133799, 1.928577636452524610E-17, 4.498031496062992574 ) ) ;
#9475 = CARTESIAN_POINT ( 'NONE',  ( 0.07405724077823318263, -1.091659401300105747, -0.1787899950787401604 ) ) ;
#9476 = ORIENTED_EDGE ( 'NONE', *, *, #21119, .T. ) ;
#9477 = CARTESIAN_POINT ( 'NONE',  ( -0.1787899950787401604, -0.1948818897100161873, 0.07405724077823318263 ) ) ;
#9478 = VERTEX_POINT ( 'NONE', #34572 ) ;
#9479 = VERTEX_POINT ( 'NONE', #1725 ) ;
#9480 = CARTESIAN_POINT ( 'NONE',  ( 0.7185039370078714072, 0.06523048226347728795, 1.749507873908221045 ) ) ;
#9481 = CARTESIAN_POINT ( 'NONE',  ( -1.033464566929134687, -0.06523048226347956391, 0.4306102361129448552 ) ) ;
#9482 = ( BOUNDED_CURVE ( )  B_SPLINE_CURVE ( 2, ( #45724, #17223, #13178, #16986, #12712, #24191, #13404, #5951, #34749 ),
 .UNSPECIFIED., .F., .T. ) 
 B_SPLINE_CURVE_WITH_KNOTS ( ( 3, 2, 2, 2, 3 ),
 ( 0.6999999999999999556, 0.7025000000000000133, 0.7049999999999999600, 0.7075000000000000178, 0.7099999999999999645 ),
 .UNSPECIFIED. ) 
 CURVE ( )  GEOMETRIC_REPRESENTATION_ITEM ( )  RATIONAL_B_SPLINE_CURVE ( ( 1.000000000000000000, 0.9238795325112899581, 1.000000000000000000, 0.9238795325112869605, 1.000000000000000000, 0.9238795325112869605, 1.000000000000000000, 0.9238795325112869605, 1.000000000000000000 ) ) 
 REPRESENTATION_ITEM ( '' )  ) ;
#9483 = CARTESIAN_POINT ( 'NONE',  ( 0.9412147342319837628, 0.1574803149606300301, 1.788877952755905332 ) ) ;
#9484 = CARTESIAN_POINT ( 'NONE',  ( 0.07405724077823318263, -0.5836614172690718361, 0.1787899950787401604 ) ) ;
#9485 = ADVANCED_FACE ( 'NONE', ( #41477 ), #8928, .T. ) ;
#9486 = CARTESIAN_POINT ( 'NONE',  ( -1.054774247047244540, 0.07405724077823318263, 0.3838582676627718127 ) ) ;
#9487 = CARTESIAN_POINT ( 'NONE',  ( 0.07444174185955046430, -1.115693415882259121, -0.1797182628040039087 ) ) ;
#9488 = CARTESIAN_POINT ( 'NONE',  ( 0.7495606340400177148, -0.1264236179284866091, 1.114665354276944909 ) ) ;
#9489 = CARTESIAN_POINT ( 'NONE',  ( 0.8019270111902716547, 0.1787899950787401604, 1.412401574749386990 ) ) ;
#9490 = CARTESIAN_POINT ( 'NONE',  ( 1.002407869896990045, 0.1264236179284866091, 0.1845472440407248116 ) ) ;
#9491 = EDGE_CURVE ( 'NONE', #9213, #5917, #45332, .T. ) ;
#9492 = CARTESIAN_POINT ( 'NONE',  ( 0.8107537697050253289, -0.1574803149606297803, 1.493602362204724754 ) ) ;
#9493 = CYLINDRICAL_SURFACE ( 'NONE', #1713, 0.3912448816427701037 ) ;
#9494 = CARTESIAN_POINT ( 'NONE',  ( -0.7185039370078739607, 1.928577636452523993E-17, 0.7381889763779527769 ) ) ;
#9495 = CARTESIAN_POINT ( 'NONE',  ( -9.642888182262618425E-18, -0.7362204723334173639, -0.1574803149606299191 ) ) ;
#9496 = ( BOUNDED_CURVE ( )  B_SPLINE_CURVE ( 2, ( #46978, #43858, #31918, #21102, #42885, #3378, #47226, #40251, #35969 ),
 .UNSPECIFIED., .F., .T. ) 
 B_SPLINE_CURVE_WITH_KNOTS ( ( 3, 2, 2, 2, 3 ),
 ( 0.5699999999999999512, 0.5725000000000000089, 0.5749999999999999556, 0.5775000000000000133, 0.5799999999999999600 ),
 .UNSPECIFIED. ) 
 CURVE ( )  GEOMETRIC_REPRESENTATION_ITEM ( )  RATIONAL_B_SPLINE_CURVE ( ( 1.000000000000000000, 0.9238795325112899581, 1.000000000000000000, 0.9238795325112869605, 1.000000000000000000, 0.9238795325112869605, 1.000000000000000000, 0.9238795325112869605, 1.000000000000000000 ) ) 
 REPRESENTATION_ITEM ( '' )  ) ;
#9497 = CARTESIAN_POINT ( 'NONE',  ( -0.8759842519685039353, 0.1574803149606299191, 1.555118110236220597 ) ) ;
#9498 = CARTESIAN_POINT ( 'NONE',  ( 0.6971942568897648851, -0.07405724077823297447, 0.9891732282926936071 ) ) ;
#9499 = CARTESIAN_POINT ( 'NONE',  ( 1.054774247047244096, 0.000000000000000000, 1.916830708607653477 ) ) ;
#9500 = CARTESIAN_POINT ( 'NONE',  ( 0.7646288533564489232, -0.1113553986120547346, 0.3001968502861740440 ) ) ;
#9501 = ORIENTED_EDGE ( 'NONE', *, *, #17469, .T. ) ;
#9502 = CARTESIAN_POINT ( 'NONE',  ( -0.3980944881889745268, 0.6449983665207583705, -0.06082000038405668829 ) ) ;
#9503 = CARTESIAN_POINT ( 'NONE',  ( -0.1574803149606297803, -1.708169291231055098, 0.06523048226347956391 ) ) ;
#9504 = CARTESIAN_POINT ( 'NONE',  ( -0.9412147342319837628, 0.1574803149606300301, 0.3223425195775121432 ) ) ;
#9505 = FACE_OUTER_BOUND ( 'NONE', #42659, .T. ) ;
#9506 = CARTESIAN_POINT ( 'NONE',  ( 0.8019270111902717657, -0.1787899950787401604, 1.348425196796630976 ) ) ;
#9508 = DIRECTION ( 'NONE',  ( 0.000000000000000000, -1.000000000000000000, -0.000000000000000000 ) ) ;
#9507 = CARTESIAN_POINT ( 'NONE',  ( 0.09216094027010306167, -0.09383642490574117812, 0.2322237458739927762 ) ) ;
#9509 = CARTESIAN_POINT ( 'NONE',  ( -0.07405724077823318263, 0.1102362205262043815, -0.1787899950787401604 ) ) ;
#9510 = DIRECTION ( 'NONE',  ( 0.000000000000000000, 0.000000000000000000, -1.000000000000000000 ) ) ;
#9511 = CARTESIAN_POINT ( 'NONE',  ( -0.7495606340400177148, 0.1264236179284866091, 0.6274606298674959559 ) ) ;
#9512 = CARTESIAN_POINT ( 'NONE',  ( 0.7185039370078739607, 1.928577636452523993E-17, 0.2657480314960630197 ) ) ;
#9513 = CARTESIAN_POINT ( 'NONE',  ( -0.08776479879009549401, 0.09247100924357742890, 0.2347620406593067532 ) ) ;
#9514 = ORIENTED_EDGE ( 'NONE', *, *, #37383, .F. ) ;
#9515 = ORIENTED_EDGE ( 'NONE', *, *, #5867, .F. ) ;
#9516 = CARTESIAN_POINT ( 'NONE',  ( -0.8019270111902716547, 0.1787899950787401604, 1.333661417269071281 ) ) ;
#9517 = CARTESIAN_POINT ( 'NONE',  ( -0.1264236179284866091, -1.732775590497417362, 0.1264236179284866091 ) ) ;
#9518 = CARTESIAN_POINT ( 'NONE',  ( -0.6971942568897626646, 0.07405724077823318263, 0.9891732282926934960 ) ) ;
#9519 = CARTESIAN_POINT ( 'NONE',  ( -0.7646288533564489232, 0.1113553986120547346, 0.06397637795275590289 ) ) ;
#9520 = ORIENTED_EDGE ( 'NONE', *, *, #21130, .T. ) ;
#9521 = CARTESIAN_POINT ( 'NONE',  ( -0.6971942568897626646, -0.07405724077823297447, 0.6003937007336389575 ) ) ;
#9522 = EDGE_CURVE ( 'NONE', #10631, #955, #39422, .T. ) ;
#9523 = DIRECTION ( 'NONE',  ( 1.000000000000000000, -3.469446951953614189E-15, -0.000000000000000000 ) ) ;
#9524 = FACE_OUTER_BOUND ( 'NONE', #43286, .T. ) ;
#9525 = CARTESIAN_POINT ( 'NONE',  ( 0.07405724077823318263, -0.6979586138985296451, -0.1787899950787401604 ) ) ;
#9526 = EDGE_LOOP ( 'NONE', ( #34107, #20828 ) ) ;
#9527 = CARTESIAN_POINT ( 'NONE',  ( 0.2038110898043921371, -0.08956021042321613002, 0.02011050427597645823 ) ) ;
#9528 = DIRECTION ( 'NONE',  ( -1.665334536937734071E-16, -0.6156614753256598460, -0.7880107536067206819 ) ) ;
#9529 = EDGE_LOOP ( 'NONE', ( #20596, #40473, #7345, #33549, #13880 ) ) ;
#9530 = LINE ( 'NONE', #30886, #30281 ) ;
#9531 = CARTESIAN_POINT ( 'NONE',  ( -1.033464566929133799, 0.000000000000000000, 1.181102362097196989 ) ) ;
#9532 = CARTESIAN_POINT ( 'NONE',  ( -0.6971942568897626646, 0.07405724077823318263, 0.6299212597887560161 ) ) ;
#9533 = DIRECTION ( 'NONE',  ( 0.000000000000000000, 0.000000000000000000, 1.000000000000000000 ) ) ;
#9534 = CONICAL_SURFACE ( 'NONE', #37054, 0.1574803149606299191, 1.047197551196598297 ) ;
#9535 = EDGE_CURVE ( 'NONE', #22060, #40552, #13007, .T. ) ;
#9536 = CARTESIAN_POINT ( 'NONE',  ( -0.8019270111902716547, 0.1787899950787401604, 1.692913385773008539 ) ) ;
#9537 = CARTESIAN_POINT ( 'NONE',  ( 0.7185039370078739607, 0.000000000000000000, 4.498031496062992574 ) ) ;
#9538 = EDGE_CURVE ( 'NONE', #9783, #43175, #20880, .T. ) ;
#9539 = CARTESIAN_POINT ( 'NONE',  ( -1.033464566929133799, 0.000000000000000000, 1.427165354330708569 ) ) ;
#9540 = DIRECTION ( 'NONE',  ( 0.000000000000000000, 1.000000000000000000, 0.000000000000000000 ) ) ;
#9541 = CARTESIAN_POINT ( 'NONE',  ( 0.8107537697050253289, 0.1574803149606300301, 0.5733267716535435099 ) ) ;
#9542 = CARTESIAN_POINT ( 'NONE',  ( 0.1797182628040039365, -0.6506343607641476012, -2.200913952912460540E-17 ) ) ;
#9543 = CARTESIAN_POINT ( 'NONE',  ( 0.2471922904502826812, 0.07945684066378068400, 0.07439773916327693803 ) ) ;
#9544 = CARTESIAN_POINT ( 'NONE',  ( -0.7185039370078746268, 0.06523048226347956391, 1.237696850286174044 ) ) ;
#9545 = DIRECTION ( 'NONE',  ( 1.000000000000000000, 0.000000000000000000, 0.000000000000000000 ) ) ;
#9547 = CARTESIAN_POINT ( 'NONE',  ( -9.642888182262618425E-18, 0.04133858267716535029, -0.1574803149606299191 ) ) ;
#9546 = CARTESIAN_POINT ( 'NONE',  ( 0.1113553986120547346, -0.3966535433070866312, -0.1113553986120547346 ) ) ;
#9548 = CARTESIAN_POINT ( 'NONE',  ( 0.000000000000000000, 0.08719492171395729074, -0.5641677032617165022 ) ) ;
#9549 = ORIENTED_EDGE ( 'NONE', *, *, #13640, .T. ) ;
#9550 = CARTESIAN_POINT ( 'NONE',  ( 0.1574803149606299191, 0.03149606299212598381, -1.928577636452523993E-17 ) ) ;
#9551 = EDGE_CURVE ( 'NONE', #19046, #2019, #3330, .T. ) ;
#9552 = CARTESIAN_POINT ( 'NONE',  ( 1.033464566929134687, 0.06523048226347956391, 1.075295275590550048 ) ) ;
#9554 = SURFACE_STYLE_FILL_AREA ( #28238 ) ;
#9553 = DIRECTION ( 'NONE',  ( 6.679788269418529283E-17, -1.000000000000000000, 0.000000000000000000 ) ) ;
#9555 = CYLINDRICAL_SURFACE ( 'NONE', #44220, 0.1574803149606299191 ) ;
#9556 = EDGE_CURVE ( 'NONE', #40732, #23920, #11599, .T. ) ;
#9557 = DIRECTION ( 'NONE',  ( 0.000000000000000000, 0.000000000000000000, 1.000000000000000000 ) ) ;
#9558 = CARTESIAN_POINT ( 'NONE',  ( 0.5314960629921260393, 0.000000000000000000, 4.842519685039370358 ) ) ;
#9560 = AXIS2_PLACEMENT_3D ( 'NONE', #34298, #1669, #15609 ) ;
#9559 = CARTESIAN_POINT ( 'NONE',  ( -0.1264236179284866091, -0.5172244093950552069, -0.1264236179284866091 ) ) ;
#9561 = FACE_OUTER_BOUND ( 'NONE', #20700, .T. ) ;
#9562 = ORIENTED_EDGE ( 'NONE', *, *, #14466, .F. ) ;
#9563 = CARTESIAN_POINT ( 'NONE',  ( 0.1651804164989524593, 0.1299212598425196763, 0.06841997037041555596 ) ) ;
#9564 = VECTOR ( 'NONE', #8047, 39.37007874015748143 ) ;
#9565 = CARTESIAN_POINT ( 'NONE',  ( 0.9873396505805591694, -0.1113553986120547346, 0.8710629921259842590 ) ) ;
#9566 = CARTESIAN_POINT ( 'NONE',  ( 0.8759842519685039353, 0.1787899950787401882, 0.7800196849856062542 ) ) ;
#9567 = CARTESIAN_POINT ( 'NONE',  ( 0.9873396505805591694, -0.1113553986120547346, 1.304133858267716661 ) ) ;
#9568 = CARTESIAN_POINT ( 'NONE',  ( 0.7185039370078746268, -0.06523048226347956391, 0.6914370077664891978 ) ) ;
#9569 = CARTESIAN_POINT ( 'NONE',  ( 3.301370929368692659E-17, 0.08755461561380492586, 0.1797182628040039365 ) ) ;
#9570 = CARTESIAN_POINT ( 'NONE',  ( 0.07405724077823318263, -1.001968503883243988, -0.1787899950787401604 ) ) ;
#9571 = CARTESIAN_POINT ( 'NONE',  ( 2.892866454678787531E-17, -1.316929133858267820, 0.1574803149606299191 ) ) ;
#9572 = CARTESIAN_POINT ( 'NONE',  ( 0.8759842519685039353, -0.1574803149606299191, 1.249999999892472236 ) ) ;
#9573 = CARTESIAN_POINT ( 'NONE',  ( -0.4620708661417322616, 0.6529540528279709211, 0.4629603087243971959 ) ) ;
#9574 = ORIENTED_EDGE ( 'NONE', *, *, #8812, .T. ) ;
#9575 = CARTESIAN_POINT ( 'NONE',  ( -0.6971942568897648851, 0.07405724077823318263, 1.973425196796630088 ) ) ;
#9576 = CARTESIAN_POINT ( 'NONE',  ( 1.002407869896990045, -0.1264236179284866091, 1.872539370024976391 ) ) ;
#9577 = ORIENTED_EDGE ( 'NONE', *, *, #41668, .F. ) ;
#9578 = CARTESIAN_POINT ( 'NONE',  ( 0.8107537697050254399, -0.1574803149606297803, 0.5487204724409447953 ) ) ;
#9579 = CARTESIAN_POINT ( 'NONE',  ( -0.9500414927467378812, -0.1787899950787401604, 1.510826771599780294 ) ) ;
#9580 = LINE ( 'NONE', #45494, #8281 ) ;
#9581 = CARTESIAN_POINT ( 'NONE',  ( -1.002407869896990045, -0.1264236179284866091, 0.9621062991588346103 ) ) ;
#9582 = CARTESIAN_POINT ( 'NONE',  ( -0.8019270111902717657, 0.1787899950787401604, 0.2755905511273391006 ) ) ;
#9583 = CARTESIAN_POINT ( 'NONE',  ( 0.9412147342319837628, -0.1574803149606297803, 1.577263779527559917 ) ) ;
#9584 = CARTESIAN_POINT ( 'NONE',  ( -1.054774247047244096, 0.000000000000000000, 1.838090551127338657 ) ) ;
#9585 = CARTESIAN_POINT ( 'NONE',  ( 0.01929052294527547340, -0.05062618494071648156, -0.2742915362215330721 ) ) ;
#9586 = CARTESIAN_POINT ( 'NONE',  ( -0.8759842519685039353, 0.1574803149606299191, 1.751968503937007871 ) ) ;
#9587 = LINE ( 'NONE', #9824, #2161 ) ;
#9588 = CARTESIAN_POINT ( 'NONE',  ( 0.1264236179284866091, -0.2673483776780578580, -0.1264236179284866091 ) ) ;
#9589 = CARTESIAN_POINT ( 'NONE',  ( -0.09380120751742244967, -0.09842519685039370636, 0.2089111925752385746 ) ) ;
#9590 = CARTESIAN_POINT ( 'NONE',  ( -0.1574803149606300301, 0.009350393700787397108, -0.06523048226347956391 ) ) ;
#9591 = DIRECTION ( 'NONE',  ( 1.822029033848725028E-16, 0.000000000000000000, 1.000000000000000000 ) ) ;
#9592 = AXIS2_PLACEMENT_3D ( 'NONE', #3354, #17731, #47207 ) ;
#9593 = ORIENTED_EDGE ( 'NONE', *, *, #37545, .F. ) ;
#9594 = AXIS2_PLACEMENT_3D ( 'NONE', #1366, #16020, #41126 ) ;
#9595 = EDGE_CURVE ( 'NONE', #42642, #11723, #41070, .T. ) ;
#9596 = CARTESIAN_POINT ( 'NONE',  ( -1.002407869896990045, -0.1264236179284866091, 1.242618110182456714 ) ) ;
#9597 = VECTOR ( 'NONE', #12429, 39.37007874015748143 ) ;
#9598 = CARTESIAN_POINT ( 'NONE',  ( -0.1264236179284866091, -0.9847440944344251212, 0.1264236179284866091 ) ) ;
#9599 = CARTESIAN_POINT ( 'NONE',  ( 0.1787899950787401604, -1.164370078686393306, 0.07405724077823318263 ) ) ;
#9600 = LINE ( 'NONE', #9833, #24085 ) ;
#9601 = CARTESIAN_POINT ( 'NONE',  ( 1.054774247047244540, 0.07405724077823318263, 0.4183070865604097133 ) ) ;
#9602 = CARTESIAN_POINT ( 'NONE',  ( 0.1797182628040039365, -0.4537839670633606604, -2.200913952912460540E-17 ) ) ;
#9603 = FACE_OUTER_BOUND ( 'NONE', #3747, .T. ) ;
#9604 = CARTESIAN_POINT ( 'NONE',  ( -1.033464566929134687, -0.06523048226347956391, 0.7160433070866151217 ) ) ;
#9605 = CARTESIAN_POINT ( 'NONE',  ( 0.1574803149606300301, -0.04970472440944883469, 0.06523048226347956391 ) ) ;
#9606 = CARTESIAN_POINT ( 'NONE',  ( -1.044119406988188947, 0.000000000000000000, 1.984498031469181134 ) ) ;
#9607 = EDGE_CURVE ( 'NONE', #32653, #5495, #38053, .T. ) ;
#9608 = CARTESIAN_POINT ( 'NONE',  ( 1.054774247047244096, 0.000000000000000000, 0.8882874015210394658 ) ) ;
#9609 = SHAPE_REPRESENTATION ( 'MAS-231', ( #16338, #13260, #30894, #40786, #31647, #10972, #4067, #28595, #36984, #228, #7119, #9470, #30128, #36219, #20143, #39264, #973, #3326, #19356, #46932 ), #9421 ) ;
#9610 = EDGE_CURVE ( 'NONE', #35682, #43583, #26307, .T. ) ;
#9612 = CARTESIAN_POINT ( 'NONE',  ( 0.003857550520849534464, 0.09763768210239696932, 0.1064941629722592487 ) ) ;
#9611 = CARTESIAN_POINT ( 'NONE',  ( 0.1635016310872748624, 0.2010965215412253426, -0.03441347972012011314 ) ) ;
#9613 = CARTESIAN_POINT ( 'NONE',  ( 0.9500414927467378812, 0.1787899950787401604, 1.924212598371433325 ) ) ;
#9614 = CARTESIAN_POINT ( 'NONE',  ( 1.033464566929133799, 0.000000000000000000, 0.7086614172153071767 ) ) ;
#9616 = CARTESIAN_POINT ( 'NONE',  ( -0.1264236179284866091, -0.5615157479777322935, -0.1264236179284866091 ) ) ;
#9615 = CARTESIAN_POINT ( 'NONE',  ( -0.1574803149606299191, -1.001968503829480328, 0.000000000000000000 ) ) ;
#9617 = CARTESIAN_POINT ( 'NONE',  ( -0.1787899950787401882, -1.457185039316315045, 0.000000000000000000 ) ) ;
#9618 = CARTESIAN_POINT ( 'NONE',  ( -0.8019270111902717657, -0.1787899950787401604, 1.899606299158834943 ) ) ;
#9619 = VERTEX_POINT ( 'NONE', #8436 ) ;
#9620 = VECTOR ( 'NONE', #45449, 39.37007874015748143 ) ;
#9621 = CARTESIAN_POINT ( 'NONE',  ( -0.6971942568897648851, -0.07405724077823297447, 1.427165354276944687 ) ) ;
#9622 = CARTESIAN_POINT ( 'NONE',  ( 0.6971942568897648851, 0.07405724077823318263, 1.343503936954111744 ) ) ;
#9623 = AXIS2_PLACEMENT_3D ( 'NONE', #46288, #16605, #20183 ) ;
#9624 = CARTESIAN_POINT ( 'NONE',  ( -0.6195511811023656223, 0.8070866141732282451, 0.5854071585544579071 ) ) ;
#9625 = CARTESIAN_POINT ( 'NONE',  ( -0.1574803149606299191, -1.238188976270425012, 0.000000000000000000 ) ) ;
#9626 = CARTESIAN_POINT ( 'NONE',  ( -0.8019270111902717657, 0.1787899950787401604, 0.5905511810485987167 ) ) ;
#9627 = DIRECTION ( 'NONE',  ( -3.469446951953613794E-15, -1.000000000000000000, 0.000000000000000000 ) ) ;
#9628 = DIRECTION ( 'NONE',  ( 3.469446951953608272E-15, 1.000000000000000000, 0.000000000000000000 ) ) ;
#9629 = CARTESIAN_POINT ( 'NONE',  ( 0.9500414927467377701, -0.1787899950787401604, 0.6889763778989936860 ) ) ;
#9630 = CARTESIAN_POINT ( 'NONE',  ( -0.8019270111902716547, -0.1787899950787401604, 0.6003937007336380693 ) ) ;
#9631 = CARTESIAN_POINT ( 'NONE',  ( 0.2090839795229337272, -0.06563552548666866382, 0.1647146447861778384 ) ) ;
#9632 = DIRECTION ( 'NONE',  ( 1.000000000000000000, 0.000000000000000000, 0.000000000000000000 ) ) ;
#9633 = ORIENTED_EDGE ( 'NONE', *, *, #47238, .F. ) ;
#9634 = CARTESIAN_POINT ( 'NONE',  ( 0.000000000000000000, -5.122214988120488358E-16, -8.878505979408856939E-16 ) ) ;
#9635 = CARTESIAN_POINT ( 'NONE',  ( -0.7646288533564489232, -0.1113553986120547346, 0.3494094488188976277 ) ) ;
#9636 = CARTESIAN_POINT ( 'NONE',  ( 0.9500414927467377701, 0.1787899950787401604, 1.333661417269071281 ) ) ;
#9637 = CARTESIAN_POINT ( 'NONE',  ( 0.2072130438524933116, -0.09851384797483406230, -0.0004152610389529299054 ) ) ;
#9638 = VERTEX_POINT ( 'NONE', #15185 ) ;
#9639 = EDGE_CURVE ( 'NONE', #35496, #36366, #504, .T. ) ;
#9640 = CARTESIAN_POINT ( 'NONE',  ( -1.002407869896990045, 0.1264236179284866091, 0.9768700786863937502 ) ) ;
#9641 = EDGE_CURVE ( 'NONE', #1718, #5180, #8943, .T. ) ;
#9642 = CARTESIAN_POINT ( 'NONE',  ( 0.1264236179284866091, -1.537033417048135897, 0.1264236179284866091 ) ) ;
#9643 = ORIENTED_EDGE ( 'NONE', *, *, #26702, .F. ) ;
#9644 = CARTESIAN_POINT ( 'NONE',  ( 1.033464566929133799, 0.000000000000000000, 0.9940944881889764995 ) ) ;
#9645 = CARTESIAN_POINT ( 'NONE',  ( -1.094772975963752103E-17, -0.6008858267178898149, -0.1787899950787401882 ) ) ;
#9646 = ADVANCED_FACE ( 'NONE', ( #757 ), #19693, .T. ) ;
#9647 = CARTESIAN_POINT ( 'NONE',  ( 0.1574803149606319730, 0.4667239666988196034, -0.7023826619074858835 ) ) ;
#9648 = ORIENTED_EDGE ( 'NONE', *, *, #29660, .T. ) ;
#9649 = VECTOR ( 'NONE', #1346, 39.37007874015748143 ) ;
#9650 = CARTESIAN_POINT ( 'NONE',  ( 0.1476377952755906220, -0.5010918323780657602, -0.8705539716229625524 ) ) ;
#9651 = CARTESIAN_POINT ( 'NONE',  ( -0.1787899950787401604, -0.3179133857730082058, 0.07405724077823318263 ) ) ;
#9652 = CARTESIAN_POINT ( 'NONE',  ( -0.1787899950787401882, -0.7091535432533228045, 0.000000000000000000 ) ) ;
#9653 = CARTESIAN_POINT ( 'NONE',  ( 0.7185039370078739607, 1.928577636452523993E-17, 1.879921259842519676 ) ) ;
#9654 = CARTESIAN_POINT ( 'NONE',  ( 1.033464566929133799, 0.000000000000000000, 1.732283464459401623 ) ) ;
#9655 = VECTOR ( 'NONE', #24616, 39.37007874015748143 ) ;
#9656 = CARTESIAN_POINT ( 'NONE',  ( -0.07405724077823318263, 0.09436422074713922414, -0.1787899950787401604 ) ) ;
#9657 = CARTESIAN_POINT ( 'NONE',  ( -0.07405724077823318263, 0.04133858273092887170, 0.1787899950787401604 ) ) ;
#9658 = SHAPE_DEFINITION_REPRESENTATION ( #7317, #30762 ) ;
#9659 = CARTESIAN_POINT ( 'NONE',  ( 0.2559055118110236116, -0.1477471161312049197, -0.2921040715117803055 ) ) ;
#9660 = CARTESIAN_POINT ( 'NONE',  ( 0.7495606340400177148, -0.1264236179284866091, 0.5191929133320630774 ) ) ;
#9661 = CARTESIAN_POINT ( 'NONE',  ( -0.8759842519685039353, -0.1787899950787401882, 0.8833661416785196785 ) ) ;
#9662 = CARTESIAN_POINT ( 'NONE',  ( -0.9873396505805591694, -0.1113553986120547346, 1.294291338475149544 ) ) ;
#9664 = DIRECTION ( 'NONE',  ( -1.000000000000000000, 0.000000000000000000, -0.000000000000000000 ) ) ;
#9663 = CARTESIAN_POINT ( 'NONE',  ( 0.1113553986120547346, -0.8789370078740158521, 0.1113553986120547346 ) ) ;
#9666 = CARTESIAN_POINT ( 'NONE',  ( -0.8102569175943972191, -0.1593853870594618694, 1.986963696465253726 ) ) ;
#9665 = CARTESIAN_POINT ( 'NONE',  ( 3.301370929368692659E-17, -1.526618612732651314, 0.1797182628040039365 ) ) ;
#9667 = CARTESIAN_POINT ( 'NONE',  ( -0.07405724077823318263, -0.4015748030958427028, -0.1787899950787401604 ) ) ;
#9668 = CARTESIAN_POINT ( 'NONE',  ( 1.002407869896990045, -0.1264236179284866091, 1.478838582623401399 ) ) ;
#9670 = CARTESIAN_POINT ( 'NONE',  ( 0.1602931993194444682, 0.1591122789105269553, 0.000000000000000000 ) ) ;
#9669 = CARTESIAN_POINT ( 'NONE',  ( 0.1292751490962095184, 0.09842519685039370636, -0.2107960287359162133 ) ) ;
#9671 = CARTESIAN_POINT ( 'NONE',  ( 0.6971942568897648851, -0.07405724077823297447, 0.3986220471903311746 ) ) ;
#9672 = ORIENTED_EDGE ( 'NONE', *, *, #27582, .F. ) ;
#9673 = DIRECTION ( 'NONE',  ( 1.000000000000000000, 0.000000000000000000, 0.000000000000000000 ) ) ;
#9674 = CARTESIAN_POINT ( 'NONE',  ( 0.7185039370078760701, -0.06523048226348075740, 0.8489173227271181732 ) ) ;
#9675 = CARTESIAN_POINT ( 'NONE',  ( 0.4736248074375818407, 1.495705267341505884, -0.3569552279982035614 ) ) ;
#9676 = CARTESIAN_POINT ( 'NONE',  ( 0.1787899950787401604, -0.1062992125446616531, 0.07405724077823318263 ) ) ;
#9677 = CARTESIAN_POINT ( 'NONE',  ( 3.284318927891251994E-17, -0.06938976372576398377, 0.1787899950787401882 ) ) ;
#9678 = CARTESIAN_POINT ( 'NONE',  ( 0.7495606340400177148, 0.1264236179284866091, 0.4699803149068661479 ) ) ;
#9679 = CARTESIAN_POINT ( 'NONE',  ( -0.07405724077823318263, -0.9133858267178897039, -0.1787899950787401604 ) ) ;
#9680 = CYLINDRICAL_SURFACE ( 'NONE', #26153, 0.1574803149606299191 ) ;
#9681 = DIRECTION ( 'NONE',  ( 1.000000000000000000, 0.000000000000000000, 0.000000000000000000 ) ) ;
#9682 = CARTESIAN_POINT ( 'NONE',  ( -0.8759842519685039353, -0.1787899950787401882, 1.468996062938362046 ) ) ;
#9683 = ORIENTED_EDGE ( 'NONE', *, *, #4574, .F. ) ;
#9684 = CARTESIAN_POINT ( 'NONE',  ( 0.8019270111902717657, -0.1787899950787401604, 0.9596456692375764375 ) ) ;
#9685 = ORIENTED_EDGE ( 'NONE', *, *, #34425, .F. ) ;
#9686 = CARTESIAN_POINT ( 'NONE',  ( -0.1264236179284866091, -1.339074803095842592, 0.1264236179284866091 ) ) ;
#9687 = CARTESIAN_POINT ( 'NONE',  ( -0.8759842519685039353, 0.1574803149606299191, 0.5216535431995598104 ) ) ;
#9688 = DIRECTION ( 'NONE',  ( 0.000000000000000000, 1.000000000000000000, 0.000000000000000000 ) ) ;
#9689 = AXIS2_PLACEMENT_3D ( 'NONE', #5127, #15950, #9208 ) ;
#9690 = CARTESIAN_POINT ( 'NONE',  ( -1.054774247047244540, -0.07405724077823318263, 0.9645669290800953366 ) ) ;
#9691 = CARTESIAN_POINT ( 'NONE',  ( -0.8107537697050254399, 0.1574803149606300301, 0.5241141731208195376 ) ) ;
#9692 = FACE_OUTER_BOUND ( 'NONE', #1956, .T. ) ;
#9693 = CARTESIAN_POINT ( 'NONE',  ( 0.9500414927467377701, 0.1787899950787401604, 0.1919291338045042705 ) ) ;
#9694 = CARTESIAN_POINT ( 'NONE',  ( 0.9873396505805591694, 0.1113553986120547346, 1.461614173120818760 ) ) ;
#9695 = ORIENTED_EDGE ( 'NONE', *, *, #3795, .F. ) ;
#9696 = EDGE_LOOP ( 'NONE', ( #2494, #36190, #1222, #13297 ) ) ;
#9697 = CYLINDRICAL_SURFACE ( 'NONE', #33664, 0.1574803149606299191 ) ;
#9698 = CARTESIAN_POINT ( 'NONE',  ( 0.2071276943281756266, -0.1759090021854102237, -0.06129781628411451466 ) ) ;
#9699 = CARTESIAN_POINT ( 'NONE',  ( -0.8759842519685039353, 0.1787899950787401882, 1.685531496009228469 ) ) ;
#9700 = ORIENTED_EDGE ( 'NONE', *, *, #20244, .T. ) ;
#9701 = VERTEX_POINT ( 'NONE', #36101 ) ;
#9702 = EDGE_CURVE ( 'NONE', #3252, #29740, #31199, .T. ) ;
#9703 = B_SPLINE_CURVE_WITH_KNOTS ( 'NONE', 3,
 ( #6155, #36120, #31362, #13152, #31825, #46412, #24620, #27786, #35876, #42347, #17660, #32058, #9543, #24388, #32309, #39220, #14075, #6632, #28228 ),
 .UNSPECIFIED., .F., .F.,
 ( 4, 1, 1, 1, 2, 2, 1, 1, 1, 1, 2, 2, 4 ),
 ( 0.000000000000000000, 0.1250000000000007494, 0.1875000000000011102, 0.2187500000000013045, 0.2343750000000013600, 0.2500000000000013878, 0.3750000000000005551, 0.4375000000000001110, 0.4687500000000000000, 0.4843749999999998890, 0.4921874999999998335, 0.4999999999999997780, 1.000000000000000000 ),
 .UNSPECIFIED. ) ;
#9704 = CARTESIAN_POINT ( 'NONE',  ( -0.9412147342319837628, 0.1574803149606300301, 0.6471456692913394315 ) ) ;
#9705 = LINE ( 'NONE', #6078, #36691 ) ;
#9706 = CARTESIAN_POINT ( 'NONE',  ( -0.1787899950787401604, -1.155635779252861983, 0.07405724077823318263 ) ) ;
#9707 = ORIENTED_EDGE ( 'NONE', *, *, #36916, .F. ) ;
#9708 = CARTESIAN_POINT ( 'NONE',  ( 0.07405724077823318263, -0.1309055117572600901, -0.1787899950787401604 ) ) ;
#9709 = ORIENTED_EDGE ( 'NONE', *, *, #25272, .T. ) ;
#9710 = EDGE_CURVE ( 'NONE', #18061, #11722, #40144, .T. ) ;
#9711 = EDGE_LOOP ( 'NONE', ( #39011, #25189, #17501, #7564, #28436, #3615, #21717 ) ) ;
#9712 = EDGE_CURVE ( 'NONE', #45034, #36603, #36082, .T. ) ;
#9713 = CARTESIAN_POINT ( 'NONE',  ( -0.2558999865593800660, -0.1227734792635908206, -0.2989668550287328808 ) ) ;
#9714 = CYLINDRICAL_SURFACE ( 'NONE', #17689, 0.02900000000000001882 ) ;
#9715 = CARTESIAN_POINT ( 'NONE',  ( 0.9873396505805591694, -0.1113553986120547346, 1.815944881889763884 ) ) ;
#9716 = CARTESIAN_POINT ( 'NONE',  ( 0.1787899950787401882, -0.7337598424659212970, -2.189545951927503898E-17 ) ) ;
#9717 = CARTESIAN_POINT ( 'NONE',  ( -0.8759842519685039353, -0.1787899950787401882, 0.2928149605761578567 ) ) ;
#9718 = CARTESIAN_POINT ( 'NONE',  ( -0.7185039370078739607, 1.928577636452523993E-17, 0.9744094488188976833 ) ) ;
#9719 = CARTESIAN_POINT ( 'NONE',  ( -0.1797182628040039087, -1.184591053677534811, -0.07444174185955065859 ) ) ;
#9720 = CARTESIAN_POINT ( 'NONE',  ( -0.1994795808946366045, 0.1803246425350550075, -0.05524818609632883848 ) ) ;
#9721 = CARTESIAN_POINT ( 'NONE',  ( 0.6971942568897648851, -0.07405724077823297447, 1.151574803095843036 ) ) ;
#9722 = CARTESIAN_POINT ( 'NONE',  ( 0.7495606340400177148, 0.1264236179284866091, 1.454232283410803017 ) ) ;
#9723 = CARTESIAN_POINT ( 'NONE',  ( 0.6971942568897626646, -0.07405724077823297447, 0.2411417322297010890 ) ) ;
#9724 = FACE_OUTER_BOUND ( 'NONE', #8988, .T. ) ;
#9726 = FACE_OUTER_BOUND ( 'NONE', #29954, .T. ) ;
#9725 = DIRECTION ( 'NONE',  ( 0.000000000000000000, 0.7907053606985338101, -0.6121968903568536513 ) ) ;
#9727 = LINE ( 'NONE', #24116, #21300 ) ;
#9728 = CARTESIAN_POINT ( 'NONE',  ( -0.8107537697050254399, -0.1574803149606297803, 0.6963582676090083190 ) ) ;
#9729 = CARTESIAN_POINT ( 'NONE',  ( 0.8019270111902716547, -0.1787899950787401604, 1.072834645615528659 ) ) ;
#9730 = CARTESIAN_POINT ( 'NONE',  ( 0.7495606340400177148, -0.1264236179284866091, 1.941437007820252081 ) ) ;
#9731 = CARTESIAN_POINT ( 'NONE',  ( 0.8759842519685039353, 0.1574803149606299191, 0.4035433069790866356 ) ) ;
#9732 = ORIENTED_EDGE ( 'NONE', *, *, #46737, .T. ) ;
#9733 = CARTESIAN_POINT ( 'NONE',  ( -0.1476377952755905387, -0.2237541348899639571, -1.272196386806235813 ) ) ;
#9734 = ORIENTED_EDGE ( 'NONE', *, *, #15700, .T. ) ;
#9735 = CARTESIAN_POINT ( 'NONE',  ( -0.9873396505805591694, -0.1113553986120547346, 0.2312992124908980207 ) ) ;
#9736 = ORIENTED_EDGE ( 'NONE', *, *, #7462, .T. ) ;
#9737 = CARTESIAN_POINT ( 'NONE',  ( 0.9500414927467378812, 0.1787899950787401604, 1.368110236166710125 ) ) ;
#9738 = ORIENTED_EDGE ( 'NONE', *, *, #31992, .T. ) ;
#9740 = DIRECTION ( 'NONE',  ( -1.000000000000000000, 0.000000000000000000, 0.000000000000000000 ) ) ;
#9739 = CARTESIAN_POINT ( 'NONE',  ( 4.681852760415787419E-17, -0.03219022224904102836, 0.2854330708661417804 ) ) ;
#9741 = CARTESIAN_POINT ( 'NONE',  ( -0.1264236179284866091, 0.08316929139234625901, 0.1264236179284866091 ) ) ;
#9742 = VECTOR ( 'NONE', #34745, 39.37007874015748143 ) ;
#9743 = CARTESIAN_POINT ( 'NONE',  ( -0.8107537697050254399, 0.1574803149606300301, 1.872539370078740495 ) ) ;
#9744 = VERTEX_POINT ( 'NONE', #28458 ) ;
#9745 = CARTESIAN_POINT ( 'NONE',  ( 0.1916154494608395820, 0.07733267719194271417, 0.1748038395390349997 ) ) ;
#9746 = DIRECTION ( 'NONE',  ( 1.000000000000000000, 0.000000000000000000, 0.000000000000000000 ) ) ;
#9747 = ORIENTED_EDGE ( 'NONE', *, *, #4094, .T. ) ;
#9748 = CARTESIAN_POINT ( 'NONE',  ( -0.8019270111902716547, -0.1787899950787401604, 1.387795275536786610 ) ) ;
#9749 = EDGE_CURVE ( 'NONE', #7257, #5433, #43761, .T. ) ;
#9750 = CARTESIAN_POINT ( 'NONE',  ( -0.1787899950787401882, -1.619586614119464585, 0.000000000000000000 ) ) ;
#9751 = CARTESIAN_POINT ( 'NONE',  ( -0.6971942568897626646, 0.07405724077823318263, 0.9498031495525356416 ) ) ;
#9752 = CARTESIAN_POINT ( 'NONE',  ( -1.033464566929133799, 0.000000000000000000, 0.009842519685039369942 ) ) ;
#9753 = ORIENTED_EDGE ( 'NONE', *, *, #7218, .F. ) ;
#9754 = CARTESIAN_POINT ( 'NONE',  ( -0.6971942568897648851, -0.07405724077823297447, 0.9891732282926936071 ) ) ;
#9755 = CARTESIAN_POINT ( 'NONE',  ( -1.054774247047244540, -0.07405724077823318263, 0.6151574802611974313 ) ) ;
#9756 = ( BOUNDED_CURVE ( )  B_SPLINE_CURVE ( 2, ( #27490, #15504, #4681, #41088, #5163, #5394, #42041, #23398, #38002 ),
 .UNSPECIFIED., .F., .T. ) 
 B_SPLINE_CURVE_WITH_KNOTS ( ( 3, 2, 2, 2, 3 ),
 ( 0.2000000000000000111, 0.2025000000000000133, 0.2049999999999999878, 0.2074999999999999900, 0.2099999999999999922 ),
 .UNSPECIFIED. ) 
 CURVE ( )  GEOMETRIC_REPRESENTATION_ITEM ( )  RATIONAL_B_SPLINE_CURVE ( ( 1.000000000000000000, 0.9238795325112869605, 1.000000000000000000, 0.9238795325112869605, 1.000000000000000000, 0.9238795325112869605, 1.000000000000000000, 0.9238795325112869605, 1.000000000000000000 ) ) 
 REPRESENTATION_ITEM ( '' )  ) ;
#9757 = ADVANCED_FACE ( 'NONE', ( #4839 ), #12039, .F. ) ;
#9758 = CARTESIAN_POINT ( 'NONE',  ( 0.1498865323622342038, 0.1262053965888239315, -0.06565210875279572922 ) ) ;
#9759 = DIRECTION ( 'NONE',  ( 0.000000000000000000, 0.000000000000000000, -1.000000000000000000 ) ) ;
#9760 = CARTESIAN_POINT ( 'NONE',  ( 0.1787899950787401882, -0.7053405036623090485, -2.189545951927503898E-17 ) ) ;
#9761 = ORIENTED_EDGE ( 'NONE', *, *, #34147, .F. ) ;
#9762 = CARTESIAN_POINT ( 'NONE',  ( -0.02921664450966929283, -0.08956076947073877970, -0.1825412823646976601 ) ) ;
#9763 = CARTESIAN_POINT ( 'NONE',  ( 0.3551574803149606385, -0.1574803149606299191, 0.000000000000000000 ) ) ;
#9764 = VERTEX_POINT ( 'NONE', #760 ) ;
#9765 = CARTESIAN_POINT ( 'NONE',  ( -0.7185039370078739607, 1.928577636452523993E-17, 0.3346456691838114450 ) ) ;
#9766 = EDGE_CURVE ( 'NONE', #5874, #15306, #1210, .T. ) ;
#9767 = DIRECTION ( 'NONE',  ( -1.000000000000000000, 0.000000000000000000, 0.000000000000000000 ) ) ;
#9768 = CARTESIAN_POINT ( 'NONE',  ( -1.054774247047244540, -0.07405724077823318263, 0.6889763778989935750 ) ) ;
#9769 = CARTESIAN_POINT ( 'NONE',  ( 0.4736248074376000483, 2.177585298233984279, -3.731703755406948986 ) ) ;
#9770 = CARTESIAN_POINT ( 'NONE',  ( -1.002407869896990045, 0.1264236179284866091, 1.724901574749385880 ) ) ;
#9771 = DIRECTION ( 'NONE',  ( 0.000000000000000000, 0.000000000000000000, 1.000000000000000000 ) ) ;
#9772 = VECTOR ( 'NONE', #7784, 39.37007874015748143 ) ;
#9773 = ( BOUNDED_CURVE ( )  B_SPLINE_CURVE ( 2, ( #44233, #26304, #33023, #40400, #18147, #32790, #15042, #47385, #14557 ),
 .UNSPECIFIED., .F., .F. ) 
 B_SPLINE_CURVE_WITH_KNOTS ( ( 3, 2, 2, 2, 3 ),
 ( 0.7700000000000000178, 0.7724999999999999645, 0.7750000000000000222, 0.7774999999999999689, 0.7800000000000000266 ),
 .UNSPECIFIED. ) 
 CURVE ( )  GEOMETRIC_REPRESENTATION_ITEM ( )  RATIONAL_B_SPLINE_CURVE ( ( 1.000000000000000000, 0.9238795325112899581, 1.000000000000000000, 0.9238795325112869605, 1.000000000000000000, 0.9238795325112869605, 1.000000000000000000, 0.9238795325112869605, 1.000000000000000000 ) ) 
 REPRESENTATION_ITEM ( '' )  ) ;
#9774 = CARTESIAN_POINT ( 'NONE',  ( -1.033464566929134687, 0.06523048226347956391, 0.1205708660342053040 ) ) ;
#9775 = CARTESIAN_POINT ( 'NONE',  ( 0.8759842519685039353, -0.1574803149606299191, 0.5511811023622047445 ) ) ;
#9776 = CARTESIAN_POINT ( 'NONE',  ( 0.1797182628040039087, -0.6481737308428884292, -0.07444174185955065859 ) ) ;
#9777 = PLANE ( 'NONE',  #27130 ) ;
#9778 = ( BOUNDED_CURVE ( )  B_SPLINE_CURVE ( 2, ( #24341, #39398, #16684, #21194, #2974, #43234, #13102, #5650, #2049 ),
 .UNSPECIFIED., .F., .T. ) 
 B_SPLINE_CURVE_WITH_KNOTS ( ( 3, 2, 2, 2, 3 ),
 ( 0.7099999999999999645, 0.7125000000000000222, 0.7149999999999999689, 0.7175000000000000266, 0.7199999999999999734 ),
 .UNSPECIFIED. ) 
 CURVE ( )  GEOMETRIC_REPRESENTATION_ITEM ( )  RATIONAL_B_SPLINE_CURVE ( ( 1.000000000000000000, 0.9238795325112939549, 1.000000000000000000, 0.9238795325112869605, 1.000000000000000000, 0.9238795325112869605, 1.000000000000000000, 0.9238795325112869605, 1.000000000000000000 ) ) 
 REPRESENTATION_ITEM ( '' )  ) ;
#9779 = CARTESIAN_POINT ( 'NONE',  ( -0.8759842519685039353, -0.1574803149606299191, 1.249999999892472236 ) ) ;
#9781 = DIRECTION ( 'NONE',  ( 7.155734338404322954E-15, 0.000000000000000000, 1.000000000000000000 ) ) ;
#9780 = CARTESIAN_POINT ( 'NONE',  ( 0.1113553986120547346, -0.3671259842519685179, 0.1113553986120547346 ) ) ;
#9782 = FACE_BOUND ( 'NONE', #35849, .T. ) ;
#9783 = VERTEX_POINT ( 'NONE', #7346 ) ;
#9784 = CARTESIAN_POINT ( 'NONE',  ( 1.033464566929133799, 0.000000000000000000, 1.387795275590551158 ) ) ;
#9785 = CARTESIAN_POINT ( 'NONE',  ( 0.8759842519685039353, 0.1574803149606299191, 1.279527559055118280 ) ) ;
#9787 = CARTESIAN_POINT ( 'NONE',  ( 1.229559056033039366E-16, -0.0009842519685041700977, 0.3937007874015748254 ) ) ;
#9786 = DIRECTION ( 'NONE',  ( 0.000000000000000000, -1.000000000000000000, 0.000000000000000000 ) ) ;
#9789 = ADVANCED_FACE ( 'NONE', ( #15899 ), #37687, .T. ) ;
#9788 = CARTESIAN_POINT ( 'NONE',  ( -0.1113553986120547346, -0.6033464565853857708, 0.1113553986120547346 ) ) ;
#9791 = CARTESIAN_POINT ( 'NONE',  ( 1.033464566929133799, 0.000000000000000000, 1.692913385719244213 ) ) ;
#9790 = CARTESIAN_POINT ( 'NONE',  ( -0.1574803149606299191, -0.9875035750853327077, -1.463737590216208861 ) ) ;
#9792 = CARTESIAN_POINT ( 'NONE',  ( -0.1607166238174611572, -0.08956082419875868728, -0.06572622029918266662 ) ) ;
#9793 = CARTESIAN_POINT ( 'NONE',  ( 0.1787899950787401604, -0.6525590550643474153, 0.07405724077823318263 ) ) ;
#9794 = LINE ( 'NONE', #28022, #12413 ) ;
#9795 = ORIENTED_EDGE ( 'NONE', *, *, #18705, .F. ) ;
#9796 = ( REPRESENTATION_RELATIONSHIP ('NONE','NONE', #9609, #20643 ) REPRESENTATION_RELATIONSHIP_WITH_TRANSFORMATION ( #47177 )SHAPE_REPRESENTATION_RELATIONSHIP( ) ) ;
#9797 = CARTESIAN_POINT ( 'NONE',  ( -9.870935133357111912E-18, 0.1176498932187669128, -0.07181495862114489759 ) ) ;
#9798 = CARTESIAN_POINT ( 'NONE',  ( 0.6971942568897626646, -0.07405724077823297447, 0.8710629920722218200 ) ) ;
#9799 = DIRECTION ( 'NONE',  ( 0.000000000000000000, 0.000000000000000000, 1.000000000000000000 ) ) ;
#9800 = CARTESIAN_POINT ( 'NONE',  ( 0.8070866141732283561, -0.0009842519685049383633, 0.7574803149606299524 ) ) ;
#9801 = CARTESIAN_POINT ( 'NONE',  ( -0.07444174185955065859, 0.03096012742482846455, -0.1797182628040039087 ) ) ;
#9802 = CARTESIAN_POINT ( 'NONE',  ( -0.1264236179284866091, -1.063484251914740275, 0.1264236179284866091 ) ) ;
#9803 = CARTESIAN_POINT ( 'NONE',  ( 0.1574803149606299191, -1.385826771653543510, -1.928577636452523993E-17 ) ) ;
#9804 = B_SPLINE_CURVE_WITH_KNOTS ( 'NONE', 3,
 ( #6048, #13964, #24987, #24289, #42930, #24749, #39583, #20674, #21140, #31957, #6762, #40460, #7644, #22259, #36894, #46776, #38884, #39344, #28614, #35316, #2455, #17081, #46311 ),
 .UNSPECIFIED., .F., .F.,
 ( 4, 2, 2, 1, 1, 1, 2, 2, 2, 1, 1, 2, 2, 4 ),
 ( 0.000000000000000000, 0.2500000000000052736, 0.3750000000000077161, 0.4375000000000087153, 0.4687500000000093814, 0.4843750000000096589, 0.4921875000000093814, 0.5000000000000091038, 0.6250000000000042188, 0.6875000000000016653, 0.7187500000000007772, 0.7343750000000004441, 0.7500000000000000000, 1.000000000000000000 ),
 .UNSPECIFIED. ) ;
#9805 = CARTESIAN_POINT ( 'NONE',  ( 0.8759842519685039353, -0.1574803149606299191, 1.289370078632629868 ) ) ;
#9806 = CARTESIAN_POINT ( 'NONE',  ( 0.1645760587280559184, 0.1627877146821090915, 0.0008175030223464901328 ) ) ;
#9807 = CIRCLE ( 'NONE', #4390, 0.1003937007874011050 ) ;
#9808 = CARTESIAN_POINT ( 'NONE',  ( -0.8759842519685039353, 0.1787899950787401882, 1.847933070812378009 ) ) ;
#9809 = CARTESIAN_POINT ( 'NONE',  ( -0.7185039370078746268, -0.06523048226347956391, 0.8095472439869610959 ) ) ;
#9810 = ORIENTED_EDGE ( 'NONE', *, *, #39428, .T. ) ;
#9811 = CARTESIAN_POINT ( 'NONE',  ( -0.9412147342319837628, 0.1574803149606300301, 0.4798228345381422288 ) ) ;
#9812 = CARTESIAN_POINT ( 'NONE',  ( -1.054774247047244540, 0.07405724077823318263, 1.520669291284818758 ) ) ;
#9813 = CARTESIAN_POINT ( 'NONE',  ( 0.06073293532416072088, 0.2604299181697357635, -0.3083162604245326399 ) ) ;
#9814 = ADVANCED_FACE ( 'NONE', ( #33647 ), #40386, .F. ) ;
#9815 = CARTESIAN_POINT ( 'NONE',  ( -0.6971942568897648851, -0.07405724077823297447, 1.028543307032851795 ) ) ;
#9816 = EDGE_CURVE ( 'NONE', #34943, #24486, #47225, .T. ) ;
#9817 = VECTOR ( 'NONE', #45261, 39.37007874015748143 ) ;
#9818 = CARTESIAN_POINT ( 'NONE',  ( -0.9500414927467378812, -0.1787899950787401604, 0.2952755904974176393 ) ) ;
#9819 = ADVANCED_FACE ( 'NONE', ( #8441 ), #41236, .T. ) ;
#9820 = CARTESIAN_POINT ( 'NONE',  ( -0.1588215770322243259, 0.09266989036297293425, -0.1937373906134662316 ) ) ;
#9821 = CARTESIAN_POINT ( 'NONE',  ( -1.054774247047244096, 0.000000000000000000, 1.916830708607653477 ) ) ;
#9822 = CARTESIAN_POINT ( 'NONE',  ( 0.9412147342319837628, -0.1574803149606297803, 1.409940944774363603 ) ) ;
#9823 = CARTESIAN_POINT ( 'NONE',  ( -0.7185039370078746268, -0.06523048226347956391, 1.921751968503937480 ) ) ;
#9824 = CARTESIAN_POINT ( 'NONE',  ( 1.737901732061166719E-16, 0.1574803149606340824, 0.2933070866141737065 ) ) ;
#9825 = CARTESIAN_POINT ( 'NONE',  ( 0.07405724077823318263, -0.2255176690166402764, -0.1787899950787401604 ) ) ;
#9826 = CARTESIAN_POINT ( 'NONE',  ( -0.002278514610727500403, -0.09842519685039370636, 0.2245093560007807021 ) ) ;
#9827 = CARTESIAN_POINT ( 'NONE',  ( 2.892866454678787531E-17, 0.02165354330708661734, 0.1574803149606299191 ) ) ;
#9828 = EDGE_CURVE ( 'NONE', #38514, #18242, #23912, .T. ) ;
#9829 = ORIENTED_EDGE ( 'NONE', *, *, #32167, .T. ) ;
#9830 = EDGE_LOOP ( 'NONE', ( #11499, #41064, #11584, #46993 ) ) ;
#9831 = CARTESIAN_POINT ( 'NONE',  ( 0.07405724077823318263, -1.272637795221826629, -0.1787899950787401604 ) ) ;
#9832 = AXIS2_PLACEMENT_3D ( 'NONE', #8353, #37587, #11029 ) ;
#9833 = CARTESIAN_POINT ( 'NONE',  ( -0.3161444924769509779, 2.559880088878760951, -3.648497683167374550 ) ) ;
#9834 = CARTESIAN_POINT ( 'NONE',  ( -0.1797182628040039365, -0.5128390851735968869, 0.000000000000000000 ) ) ;
#9835 = CARTESIAN_POINT ( 'NONE',  ( -0.9873396505805591694, -0.1113553986120547346, 0.2411417322834645827 ) ) ;
#9836 = CARTESIAN_POINT ( 'NONE',  ( -0.7646288533564489232, 0.1113553986120547346, 0.8415354329633386588 ) ) ;
#9837 = CARTESIAN_POINT ( 'NONE',  ( -0.1574803149606297803, 0.05364173228346464511, 0.06523048226347956391 ) ) ;
#9838 = CARTESIAN_POINT ( 'NONE',  ( 0.8759842519685039353, -0.1787899950787401882, 0.8784448818360000022 ) ) ;
#9840 = CARTESIAN_POINT ( 'NONE',  ( 0.1017711380106645219, -0.2367366383362172477, -0.03112915705353833454 ) ) ;
#9839 = CIRCLE ( 'NONE', #37389, 0.09842519685039370636 ) ;
#9841 = CARTESIAN_POINT ( 'NONE',  ( -0.7185039370078746268, 0.06523048226347956391, 1.247539370078740273 ) ) ;
#9843 = CARTESIAN_POINT ( 'NONE',  ( 0.1564139474900951288, -0.1282476652664072125, -0.05864041697619068461 ) ) ;
#9842 = CYLINDRICAL_SURFACE ( 'NONE', #29404, 0.09842519685039370636 ) ;
#9844 = CARTESIAN_POINT ( 'NONE',  ( 1.033464566929134687, -0.06523048226347956391, 0.1943897636720004762 ) ) ;
#9845 = FACE_OUTER_BOUND ( 'NONE', #19297, .T. ) ;
#9846 = CARTESIAN_POINT ( 'NONE',  ( 1.033464566929134687, -0.06523048226347956391, 0.3912401573727880555 ) ) ;
#9847 = CARTESIAN_POINT ( 'NONE',  ( -0.1787899950787401604, -0.5935039369541101895, 0.07405724077823318263 ) ) ;
#9848 = CARTESIAN_POINT ( 'NONE',  ( -0.07405724077823318263, -1.371062992072219489, 0.1787899950787401604 ) ) ;
#9849 = CARTESIAN_POINT ( 'NONE',  ( 0.9500414927467378812, -0.1787899950787401604, 0.3740157479777325711 ) ) ;
#9850 = CARTESIAN_POINT ( 'NONE',  ( -1.002407869896990045, -0.1264236179284866091, 1.906988188922614125 ) ) ;
#9851 = VERTEX_POINT ( 'NONE', #26122 ) ;
#9852 = ORIENTED_EDGE ( 'NONE', *, *, #7901, .F. ) ;
#9853 = CARTESIAN_POINT ( 'NONE',  ( -1.054774247047244096, 0.000000000000000000, 1.483759842465921075 ) ) ;
#9854 = EDGE_CURVE ( 'NONE', #42441, #38536, #40463, .T. ) ;
#9855 = CARTESIAN_POINT ( 'NONE',  ( 0.8759842519685039353, -0.1787899950787401882, 1.592027559001354398 ) ) ;
#9856 = EDGE_LOOP ( 'NONE', ( #26678, #40769, #33923, #32439, #35317 ) ) ;
#9857 = DIRECTION ( 'NONE',  ( -1.000000000000000000, 3.469446951953613794E-15, 1.144917494144692682E-16 ) ) ;
#9858 = CARTESIAN_POINT ( 'NONE',  ( -0.8759842519685039353, -0.1787899950787401882, 0.6865157479777322935 ) ) ;
#9859 = CARTESIAN_POINT ( 'NONE',  ( 0.8759842519685039353, -0.1787899950787401882, 0.1747047243556852092 ) ) ;
#9860 = CARTESIAN_POINT ( 'NONE',  ( 0.1338895052746215397, -0.09842531827051598237, -0.1184899159207936509 ) ) ;
#9861 = CARTESIAN_POINT ( 'NONE',  ( 0.9500414927467377701, 0.1787899950787401604, 0.5462598424659214080 ) ) ;
#9862 = CARTESIAN_POINT ( 'NONE',  ( -0.6971942568897637749, 2.189545951927499583E-17, 0.5930118109698583329 ) ) ;
#9863 = CYLINDRICAL_SURFACE ( 'NONE', #42946, 0.1574803149606299191 ) ;
#9864 = ADVANCED_FACE ( 'NONE', ( #6535 ), #31963, .T. ) ;
#9865 = AXIS2_PLACEMENT_3D ( 'NONE', #44234, #3760, #29462 ) ;
#9866 = CARTESIAN_POINT ( 'NONE',  ( -0.1476377952755905387, 0.3648440108500937140, -3.619166627704267558 ) ) ;
#9867 = EDGE_LOOP ( 'NONE', ( #18578, #37880, #46875, #24819, #35262, #26001 ) ) ;
#9868 = CARTESIAN_POINT ( 'NONE',  ( -0.9500414927467378812, 0.1787899950787401604, 1.451771653489543290 ) ) ;
#9869 = EDGE_LOOP ( 'NONE', ( #5731, #22652, #45000, #25793 ) ) ;
#9870 = CARTESIAN_POINT ( 'NONE',  ( -0.8107537697050253289, -0.1574803149606297803, 0.4306102362204725642 ) ) ;
#9871 = CARTESIAN_POINT ( 'NONE',  ( 0.9500414927467377701, 0.1787899950787401604, 1.373031496009229357 ) ) ;
#9872 = CARTESIAN_POINT ( 'NONE',  ( -0.2395769297574236179, -0.09851385218651377562, 0.02158642379462074462 ) ) ;
#9873 = VERTEX_POINT ( 'NONE', #40693 ) ;
#9874 = DIRECTION ( 'NONE',  ( 1.822029033848725028E-16, 0.000000000000000000, 1.000000000000000000 ) ) ;
#9875 = VECTOR ( 'NONE', #36098, 39.37007874015748143 ) ;
#9876 = PRODUCT_RELATED_PRODUCT_CATEGORY ( 'part', '', ( #1711 ) ) ;
#9877 = CARTESIAN_POINT ( 'NONE',  ( 0.1264236179284866091, -1.615773574528450940, 0.1264236179284866091 ) ) ;
#9878 = VERTEX_POINT ( 'NONE', #11269 ) ;
#9879 = CARTESIAN_POINT ( 'NONE',  ( 3.284318927891251994E-17, -0.5812007873478111097, 0.1787899950787401882 ) ) ;
#9880 = CARTESIAN_POINT ( 'NONE',  ( 0.7185039370078739607, 1.928577636452523993E-17, 0.8169291338582678197 ) ) ;
#9881 = ORIENTED_EDGE ( 'NONE', *, *, #33255, .F. ) ;
#9882 = CARTESIAN_POINT ( 'NONE',  ( -0.1787899950787401604, -0.3228346456155278266, -0.07405724077823318263 ) ) ;
#9883 = ( BOUNDED_CURVE ( )  B_SPLINE_CURVE ( 2, ( #7238, #3639, #14201, #21858, #36485, #6275, #22554, #37400, #43886 ),
 .UNSPECIFIED., .F., .T. ) 
 B_SPLINE_CURVE_WITH_KNOTS ( ( 3, 2, 2, 2, 3 ),
 ( 0.5600000000000000533, 0.5625000000000000000, 0.5649999999999999467, 0.5675000000000000044, 0.5699999999999999512 ),
 .UNSPECIFIED. ) 
 CURVE ( )  GEOMETRIC_REPRESENTATION_ITEM ( )  RATIONAL_B_SPLINE_CURVE ( ( 1.000000000000000000, 0.9238795325112869605, 1.000000000000000000, 0.9238795325112869605, 1.000000000000000000, 0.9238795325112869605, 1.000000000000000000, 0.9238795325112829637, 1.000000000000000000 ) ) 
 REPRESENTATION_ITEM ( '' )  ) ;
#9884 = CARTESIAN_POINT ( 'NONE',  ( -0.2471922904502826812, -0.09842519685039372024, -0.006644306898575463166 ) ) ;
#9885 = DIRECTION ( 'NONE',  ( 0.000000000000000000, 1.000000000000000000, 0.000000000000000000 ) ) ;
#9886 = CARTESIAN_POINT ( 'NONE',  ( 1.054774247047244096, 0.000000000000000000, 0.2977362204186775885 ) ) ;
#9887 = CARTESIAN_POINT ( 'NONE',  ( -1.094772975963752103E-17, -0.02620664539459307413, -0.1787899950787401882 ) ) ;
#9888 = CARTESIAN_POINT ( 'NONE',  ( 0.07405724077823318263, 0.006889763833291078637, 0.1787899950787401604 ) ) ;
#9889 = APPLICATION_PROTOCOL_DEFINITION ( 'draft international standard', 'automotive_design', 1998, #7348 ) ;
#9890 = FACE_OUTER_BOUND ( 'NONE', #21294, .T. ) ;
#9891 = CARTESIAN_POINT ( 'NONE',  ( 0.6971942568897626646, -0.07405724077823297447, 0.4773622046706456068 ) ) ;
#9892 = CARTESIAN_POINT ( 'NONE',  ( -1.054774247047244540, -0.07405724077823318263, 0.7726377952218266287 ) ) ;
#9894 = LINE ( 'NONE', #25470, #28521 ) ;
#9893 = CARTESIAN_POINT ( 'NONE',  ( 0.1574803149606299191, -0.8346456692913386544, -1.928577636452523993E-17 ) ) ;
#9896 = CARTESIAN_POINT ( 'NONE',  ( -0.7701193937251510357, -0.1341754852037822243, 1.986078545504829984 ) ) ;
#9895 = CARTESIAN_POINT ( 'NONE',  ( -1.100456976456230270E-17, -1.703783967063360105, -0.1797182628040039365 ) ) ;
#9897 = CARTESIAN_POINT ( 'NONE',  ( -0.07405724077823318263, -0.3228346456155278266, -0.1787899950787401604 ) ) ;
#9898 = CARTESIAN_POINT ( 'NONE',  ( 0.8019270111902717657, -0.1787899950787401604, 1.668307086560410157 ) ) ;
#9900 = LINE ( 'NONE', #43410, #3250 ) ;
#9899 = CARTESIAN_POINT ( 'NONE',  ( 0.6971942568897648851, -0.07405724077823297447, 1.934055118056471567 ) ) ;
#9901 = CARTESIAN_POINT ( 'NONE',  ( 1.054774247047244540, -0.07405724077823318263, 0.4133858267178901480 ) ) ;
#9902 = ORIENTED_EDGE ( 'NONE', *, *, #2794, .F. ) ;
#9904 = VERTEX_POINT ( 'NONE', #10149 ) ;
#9903 = EDGE_CURVE ( 'NONE', #43974, #18113, #34244, .T. ) ;
#9905 = LINE ( 'NONE', #39113, #37079 ) ;
#9906 = FACE_OUTER_BOUND ( 'NONE', #18880, .T. ) ;
#9907 = CARTESIAN_POINT ( 'NONE',  ( 0.1787899950787401604, -0.1801181101824570474, -0.07405724077823318263 ) ) ;
#9908 = CONICAL_SURFACE ( 'NONE', #22135, 0.1377952755905509363, 0.9599310885968960205 ) ;
#9909 = CARTESIAN_POINT ( 'NONE',  ( 0.7495606340400177148, -0.1264236179284866091, 0.5979330708123780092 ) ) ;
#9910 = CARTESIAN_POINT ( 'NONE',  ( 0.7704837865233213900, -0.1271003095796768290, 0.03936944523697429726 ) ) ;
#9911 = LINE ( 'NONE', #32448, #34646 ) ;
#9912 = CARTESIAN_POINT ( 'NONE',  ( -0.8759842519685039353, -0.1787899950787401882, 1.429625984198204858 ) ) ;
#9913 = ORIENTED_EDGE ( 'NONE', *, *, #34116, .T. ) ;
#9915 = VECTOR ( 'NONE', #5783, 39.37007874015748854 ) ;
#9914 = CARTESIAN_POINT ( 'NONE',  ( -0.3053278657842540267, -0.05482723079889029877, -1.034448866034457293 ) ) ;
#9916 = ADVANCED_FACE ( 'NONE', ( #3820 ), #46548, .F. ) ;
#9917 = CARTESIAN_POINT ( 'NONE',  ( 1.054774247047244540, -0.07405724077823318263, 1.048228346402930944 ) ) ;
#9918 = VERTEX_POINT ( 'NONE', #18440 ) ;
#9919 = CARTESIAN_POINT ( 'NONE',  ( -0.9412147342319837628, 0.1574803149606300301, 0.6766732282389293918 ) ) ;
#9920 = LINE ( 'NONE', #21643, #21001 ) ;
#9921 = CARTESIAN_POINT ( 'NONE',  ( 0.6971942568897648851, -0.07405724077823297447, 1.855314960576157635 ) ) ;
#9922 = CARTESIAN_POINT ( 'NONE',  ( -0.8759842519685039353, -0.1574803149606299191, 1.456692913385826849 ) ) ;
#9923 = CARTESIAN_POINT ( 'NONE',  ( -0.8019270111902717657, 0.1787899950787401604, 0.8218503936470251681 ) ) ;
#9924 = FACE_OUTER_BOUND ( 'NONE', #14575, .T. ) ;
#9925 = CARTESIAN_POINT ( 'NONE',  ( -0.8081549416023995347, -0.1479449179857115215, 0.03937007874015843734 ) ) ;
#9926 = CARTESIAN_POINT ( 'NONE',  ( 0.8019270111902716547, -0.1787899950787401604, 0.09350393695411057804 ) ) ;
#9927 = CARTESIAN_POINT ( 'NONE',  ( -0.8759842519685039353, 0.1787899950787401882, 0.1500984251430870220 ) ) ;
#9928 = EDGE_CURVE ( 'NONE', #6940, #40417, #30646, .T. ) ;
#9929 = CARTESIAN_POINT ( 'NONE',  ( 0.7185039370078746268, 0.06523048226347956391, 1.513287401467275917 ) ) ;
#9930 = VERTEX_POINT ( 'NONE', #17561 ) ;
#9931 = CARTESIAN_POINT ( 'NONE',  ( -0.1264236179284866091, 0.1077755906049446960, -0.1264236179284866091 ) ) ;
#9932 = VERTEX_POINT ( 'NONE', #44072 ) ;
#9933 = CARTESIAN_POINT ( 'NONE',  ( -0.9500414927467377701, 0.1787899950787401604, 1.643700787347811998 ) ) ;
#9934 = VERTEX_POINT ( 'NONE', #212 ) ;
#9935 = CARTESIAN_POINT ( 'NONE',  ( -0.2471922904502826812, 0.09842519685039370636, -0.006585516632646069672 ) ) ;
#9936 = CIRCLE ( 'NONE', #36707, 0.02900000000000062597 ) ;
#9937 = DIRECTION ( 'NONE',  ( -1.000000000000000000, 3.469446951953614189E-15, 0.000000000000000000 ) ) ;
#9938 = CARTESIAN_POINT ( 'NONE',  ( -0.1787899950787401604, -1.160557039095381437, -0.07405724077823318263 ) ) ;
#9939 = VERTEX_POINT ( 'NONE', #33562 ) ;
#9940 = CARTESIAN_POINT ( 'NONE',  ( -0.1264236179284866091, -0.08415354325332302654, -0.1264236179284866091 ) ) ;
#9941 = ORIENTED_EDGE ( 'NONE', *, *, #19582, .F. ) ;
#9942 = DIRECTION ( 'NONE',  ( 0.000000000000000000, -1.000000000000000000, 0.000000000000000000 ) ) ;
#9943 = CARTESIAN_POINT ( 'NONE',  ( 1.033464566929134687, -0.06523048226347956391, 1.857775590551181244 ) ) ;
#9944 = CIRCLE ( 'NONE', #16086, 0.02900000000000009515 ) ;
#9945 = CARTESIAN_POINT ( 'NONE',  ( -0.1270800023317771588, -0.1929571954098172892, 0.1270800023317771588 ) ) ;
#9946 = CARTESIAN_POINT ( 'NONE',  ( -0.1787899950787401604, -0.7559055117572593963, -0.07405724077823318263 ) ) ;
#9947 = CARTESIAN_POINT ( 'NONE',  ( -1.002407869896990045, 0.1264236179284866091, 0.3469488188438744070 ) ) ;
#9948 = CARTESIAN_POINT ( 'NONE',  ( -0.1270800023317771588, -1.334689478874383717, 0.1270800023317771588 ) ) ;
#9949 = CARTESIAN_POINT ( 'NONE',  ( -0.2011713568916721762, 0.1793478952077579847, -0.05654496252297641634 ) ) ;
#9950 = CARTESIAN_POINT ( 'NONE',  ( 0.8019270111902717657, 0.1787899950787401604, 1.102362204670646495 ) ) ;
#9951 = CARTESIAN_POINT ( 'NONE',  ( 0.8759842519685039353, -0.1787899950787401882, 1.547736220418677089 ) ) ;
#9953 = EDGE_CURVE ( 'NONE', #815, #45828, #29130, .T. ) ;
#9952 = FACE_OUTER_BOUND ( 'NONE', #13689, .T. ) ;
#9954 = CARTESIAN_POINT ( 'NONE',  ( 0.9412147342319837628, -0.1574803149606297803, 1.695374015748031482 ) ) ;
#9956 = CARTESIAN_POINT ( 'NONE',  ( 0.7185039370078766252, -0.06523048226348168721, 1.518208661309796481 ) ) ;
#9955 = CARTESIAN_POINT ( 'NONE',  ( 0.7612901950597569245, 0.1140645495863889802, 1.980815085937517317 ) ) ;
#9957 = DIRECTION ( 'NONE',  ( 0.000000000000000000, -0.8660254037844383745, 0.5000000000000003331 ) ) ;
#9958 = CARTESIAN_POINT ( 'NONE',  ( -1.033464566929133799, 0.000000000000000000, 1.732283464459401623 ) ) ;
#9959 = CARTESIAN_POINT ( 'NONE',  ( 1.054774247047244540, 0.07405724077823318263, 0.1820866141194649179 ) ) ;
#9960 = EDGE_CURVE ( 'NONE', #21404, #25167, #8176, .T. ) ;
#9961 = CARTESIAN_POINT ( 'NONE',  ( -0.9412147342319837628, -0.1574803149606297803, 0.7012795274515276622 ) ) ;
#9963 = CYLINDRICAL_SURFACE ( 'NONE', #7018, 0.1574803149606299191 ) ;
#9962 = CARTESIAN_POINT ( 'NONE',  ( 0.7495606340400177148, -0.1264236179284866091, 1.109744094434425232 ) ) ;
#9964 = AXIS2_PLACEMENT_3D ( 'NONE', #44477, #33280, #4947 ) ;
#9965 = CARTESIAN_POINT ( 'NONE',  ( -1.033464566929133799, 0.000000000000000000, 0.1574803148531029595 ) ) ;
#9966 = CARTESIAN_POINT ( 'NONE',  ( 0.7185039370078746268, -0.06523048226347956391, 0.4945866140657015353 ) ) ;
#9967 = EDGE_LOOP ( 'NONE', ( #29933, #39210, #38756, #569 ) ) ;
#9968 = CARTESIAN_POINT ( 'NONE',  ( -0.9873396505805591694, 0.1113553986120547346, 1.117125984251968518 ) ) ;
#9969 = ADVANCED_FACE ( 'NONE', ( #2701 ), #13973, .F. ) ;
#9970 = CARTESIAN_POINT ( 'NONE',  ( -0.8107537697050234415, -0.1574803149606297803, 0.3420275589475912925 ) ) ;
#9971 = CARTESIAN_POINT ( 'NONE',  ( -0.1377952755905511861, 1.808041534174241898E-17, -0.1321438491773566926 ) ) ;
#9972 = CARTESIAN_POINT ( 'NONE',  ( 0.8759842519685039353, 0.1787899950787401882, 1.331200787347811110 ) ) ;
#9973 = EDGE_CURVE ( 'NONE', #38897, #13902, #35803, .T. ) ;
#9974 = DIRECTION ( 'NONE',  ( 0.000000000000000000, 0.000000000000000000, -1.000000000000000000 ) ) ;
#9976 = CIRCLE ( 'NONE', #36756, 0.09842519685039370636 ) ;
#9975 = CARTESIAN_POINT ( 'NONE',  ( -0.07405724077823318263, 0.03149606304588949135, -0.1787899950787401604 ) ) ;
#9977 = CARTESIAN_POINT ( 'NONE',  ( -0.8759842519685039353, 0.000000000000000000, 0.000000000000000000 ) ) ;
#9978 = CARTESIAN_POINT ( 'NONE',  ( 1.033464566929133799, 0.000000000000000000, 0.5216535433070865757 ) ) ;
#9979 = CARTESIAN_POINT ( 'NONE',  ( 4.801428276353606495E-17, 0.03219022224904102836, 0.2854330708661417804 ) ) ;
#9980 = CARTESIAN_POINT ( 'NONE',  ( 1.002407869896990045, -0.1264236179284866091, 0.4158464566391496531 ) ) ;
#9981 = ORIENTED_EDGE ( 'NONE', *, *, #1438, .T. ) ;
#9982 = CARTESIAN_POINT ( 'NONE',  ( -0.6971942568897648851, -0.07405724077823297447, 1.422244094434425898 ) ) ;
#9984 = CARTESIAN_POINT ( 'NONE',  ( -0.1264236179284866091, -1.654035433017102319, 0.1264236179284866091 ) ) ;
#9983 = CARTESIAN_POINT ( 'NONE',  ( -0.06523048226347956391, -0.4187992124908984093, -0.1574803149606300301 ) ) ;
#9985 = CARTESIAN_POINT ( 'NONE',  ( -0.7495606340400177148, -0.1264236179284866091, 1.897145669237574772 ) ) ;
#9986 = ORIENTED_EDGE ( 'NONE', *, *, #33414, .T. ) ;
#9987 = CARTESIAN_POINT ( 'NONE',  ( -0.8759842519685039353, 0.1787899950787401882, 1.134350393647023614 ) ) ;
#9988 = CARTESIAN_POINT ( 'NONE',  ( -0.8019270111902717657, -0.1787899950787401604, 0.6840551180564720113 ) ) ;
#9989 = CARTESIAN_POINT ( 'NONE',  ( 2.700008691033534577E-17, 0.09842519685039370636, 0.2204724409448818867 ) ) ;
#9990 = DIRECTION ( 'NONE',  ( 0.000000000000000000, 0.000000000000000000, 1.000000000000000000 ) ) ;
#9991 = CARTESIAN_POINT ( 'NONE',  ( 0.1264236179284866091, -0.7102617635048287248, 0.1264236179284866091 ) ) ;
#9992 = ORIENTED_EDGE ( 'NONE', *, *, #14895, .T. ) ;
#9993 = CARTESIAN_POINT ( 'NONE',  ( 0.09519241326698858752, -0.08956226547226790735, 0.1092664699140651619 ) ) ;
#9994 = EDGE_LOOP ( 'NONE', ( #40118, #33466, #32292, #46814, #13595 ) ) ;
#9995 = DIRECTION ( 'NONE',  ( -1.000000000000000000, 0.000000000000000000, 0.000000000000000000 ) ) ;
#9996 = CARTESIAN_POINT ( 'NONE',  ( -0.9873396505805591694, 0.1113553986120547346, 0.5561023620971968784 ) ) ;
#9997 = CARTESIAN_POINT ( 'NONE',  ( -1.054774247047244540, -0.07405724077823318263, 0.5708661416785201226 ) ) ;
#9998 = DIRECTION ( 'NONE',  ( -1.000000000000000000, 0.000000000000000000, 0.000000000000000000 ) ) ;
#9999 = ORIENTED_EDGE ( 'NONE', *, *, #45991, .F. ) ;
#10000 = CARTESIAN_POINT ( 'NONE',  ( -1.002407869896990045, 0.1264236179284866091, 1.685531496009228469 ) ) ;
#10001 = VECTOR ( 'NONE', #5106, 39.37007874015748143 ) ;
#10002 = VECTOR ( 'NONE', #1068, 39.37007874015748854 ) ;
#10003 = SURFACE_SIDE_STYLE ('',( #35180 ) ) ;
#10004 = ORIENTED_EDGE ( 'NONE', *, *, #45038, .T. ) ;
#10005 = CARTESIAN_POINT ( 'NONE',  ( 0.7185039370078739607, 1.928577636452523993E-17, 0.5807086614173228023 ) ) ;
#10006 = CARTESIAN_POINT ( 'NONE',  ( 0.1797182628040039087, -0.7318351481657215940, 0.07444174185955046430 ) ) ;
#10007 = CARTESIAN_POINT ( 'NONE',  ( -0.8107537697050254399, 0.1574803149606300301, 0.9670275590551187239 ) ) ;
#10008 = CARTESIAN_POINT ( 'NONE',  ( -0.8107537697050253289, -0.1574803149606297803, 1.405019684931842816 ) ) ;
#10009 = CARTESIAN_POINT ( 'NONE',  ( 0.7495606340400177148, -0.1264236179284866091, 0.6422244093950550958 ) ) ;
#10010 = CARTESIAN_POINT ( 'NONE',  ( -0.1574803149606299191, -0.5787401574803149318, 0.000000000000000000 ) ) ;
#10011 = CARTESIAN_POINT ( 'NONE',  ( -0.1574205454495407608, 0.1252972266898419451, -0.04195140859584962911 ) ) ;
#10012 = LINE ( 'NONE', #14554, #44486 ) ;
#10013 = CARTESIAN_POINT ( 'NONE',  ( 0.8759842519685039353, 0.1574803149606299191, 1.200787401574803237 ) ) ;
#10014 = CARTESIAN_POINT ( 'NONE',  ( 0.7185039370078739607, 1.928577636452523993E-17, 1.830708661309795149 ) ) ;
#10015 = DIRECTION ( 'NONE',  ( 1.000000000000000000, 0.000000000000000000, 0.000000000000000000 ) ) ;
#10016 = EDGE_CURVE ( 'NONE', #22696, #29244, #19626, .T. ) ;
#10018 = DIRECTION ( 'NONE',  ( 0.000000000000000000, 0.000000000000000000, -1.000000000000000000 ) ) ;
#10017 = CARTESIAN_POINT ( 'NONE',  ( 1.002407869896990045, -0.1264236179284866091, 0.6077755904974173617 ) ) ;
#10019 = CARTESIAN_POINT ( 'NONE',  ( 0.1555687797274980522, -0.05303742630350873760, 0.1377952755905511861 ) ) ;
#10020 = CARTESIAN_POINT ( 'NONE',  ( 0.8759842519685039353, 0.1574803149606299191, 1.555118110236220597 ) ) ;
#10021 = EDGE_LOOP ( 'NONE', ( #45602, #31757, #42780, #40812 ) ) ;
#10022 = DIRECTION ( 'NONE',  ( 0.7071067811865450192, -0.7071067811865500152, 8.659560562354959975E-17 ) ) ;
#10023 = CARTESIAN_POINT ( 'NONE',  ( 0.6971942568897637749, 2.189545951927499583E-17, 0.7504921259304880854 ) ) ;
#10024 = EDGE_CURVE ( 'NONE', #4670, #36616, #7652, .T. ) ;
#10025 = FACE_OUTER_BOUND ( 'NONE', #46277, .T. ) ;
#10026 = CARTESIAN_POINT ( 'NONE',  ( -0.9412147342319837628, 0.1574803149606300301, 0.5290354330708663122 ) ) ;
#10027 = CARTESIAN_POINT ( 'NONE',  ( -1.100456976456230270E-17, 0.1466097337240411524, -0.1797182628040039365 ) ) ;
#10028 = CARTESIAN_POINT ( 'NONE',  ( -0.1264236179284866091, -0.9847440944344251212, 0.1264236179284866091 ) ) ;
#10029 = CARTESIAN_POINT ( 'NONE',  ( 0.1113553986120547346, -1.577755905511811108, -0.1113553986120547346 ) ) ;
#10030 = CARTESIAN_POINT ( 'NONE',  ( 1.033464566929134687, 0.06523048226347956391, 1.262303149498772425 ) ) ;
#10031 = DIRECTION ( 'NONE',  ( 0.000000000000000000, 1.000000000000000000, 0.000000000000000000 ) ) ;
#10032 = AXIS2_PLACEMENT_3D ( 'NONE', #5224, #19854, #27798 ) ;
#10033 = ORIENTED_EDGE ( 'NONE', *, *, #35938, .F. ) ;
#10034 = CARTESIAN_POINT ( 'NONE',  ( -0.7495606340400177148, 0.1264236179284866091, 1.892224409395055096 ) ) ;
#10035 = FACE_OUTER_BOUND ( 'NONE', #3646, .T. ) ;
#10036 = ORIENTED_EDGE ( 'NONE', *, *, #8331, .F. ) ;
#10037 = CARTESIAN_POINT ( 'NONE',  ( -9.642888182262618425E-18, -1.444881889656252083, -0.1574803149606299191 ) ) ;
#10038 = CARTESIAN_POINT ( 'NONE',  ( -0.7495606340400177148, -0.1264236179284866091, 1.941437007820252081 ) ) ;
#10039 = COLOUR_RGB ( '', 0.08235294, 0.09019608, 0.10196078) ;
#10040 = CARTESIAN_POINT ( 'NONE',  ( -0.7495606340400177148, 0.1264236179284866091, 1.532972440891118060 ) ) ;
#10041 = CARTESIAN_POINT ( 'NONE',  ( 0.1171103306478391837, 0.2278805513379908998, -0.3149606299212597826 ) ) ;
#10042 = CARTESIAN_POINT ( 'NONE',  ( -0.8759842519685039353, 0.1787899950787401882, 1.016240157426551161 ) ) ;
#10043 = CIRCLE ( 'NONE', #12356, 0.1003937007874010356 ) ;
#10044 = CARTESIAN_POINT ( 'NONE',  ( -0.8019270111902717657, -0.1787899950787401604, 0.1722440944344256208 ) ) ;
#10045 = CARTESIAN_POINT ( 'NONE',  ( -0.1674339218907005267, 0.08959396230939166428, -0.1887650509910711871 ) ) ;
#10046 = CARTESIAN_POINT ( 'NONE',  ( -1.002407869896990045, 0.1264236179284866091, 1.843011810969858333 ) ) ;
#10047 = DIRECTION ( 'NONE',  ( 0.000000000000000000, 0.000000000000000000, -1.000000000000000000 ) ) ;
#10048 = CARTESIAN_POINT ( 'NONE',  ( 0.1787899950787401604, -0.3091790863394751065, -0.07405724077823318263 ) ) ;
#10049 = CARTESIAN_POINT ( 'NONE',  ( -0.02050543330604039441, -0.09842519685039370636, 0.1561122773925366081 ) ) ;
#10050 = DIRECTION ( 'NONE',  ( 0.8191520442890534159, 1.003171929053600305E-16, -0.5735764363509581187 ) ) ;
#10051 = DIRECTION ( 'NONE',  ( 1.000000000000000000, 0.000000000000000000, 0.000000000000000000 ) ) ;
#10052 = ADVANCED_FACE ( 'NONE', ( #12217 ), #32715, .T. ) ;
#10053 = ( BOUNDED_CURVE ( )  B_SPLINE_CURVE ( 2, ( #45491, #41888, #19875, #16533, #13410, #1408, #5253, #27104, #20348 ),
 .UNSPECIFIED., .F., .T. ) 
 B_SPLINE_CURVE_WITH_KNOTS ( ( 3, 2, 2, 2, 3 ),
 ( 0.06500000000000000222, 0.06750000000000000444, 0.07000000000000000666, 0.07249999999999999500, 0.07499999999999999722 ),
 .UNSPECIFIED. ) 
 CURVE ( )  GEOMETRIC_REPRESENTATION_ITEM ( )  RATIONAL_B_SPLINE_CURVE ( ( 1.000000000000000000, 0.9238795325112869605, 1.000000000000000000, 0.9238795325112869605, 1.000000000000000000, 0.9238795325112869605, 1.000000000000000000, 0.9238795325112869605, 1.000000000000000000 ) ) 
 REPRESENTATION_ITEM ( '' )  ) ;
#10054 = CARTESIAN_POINT ( 'NONE',  ( -0.6971942568897626646, 0.07405724077823318263, 0.1968503936470238913 ) ) ;
#10055 = ORIENTED_EDGE ( 'NONE', *, *, #3183, .T. ) ;
#10056 = CARTESIAN_POINT ( 'NONE',  ( -0.6971942568897637749, 2.189545951927499583E-17, 1.267224409395055096 ) ) ;
#10057 = ORIENTED_EDGE ( 'NONE', *, *, #30937, .T. ) ;
#10058 = CARTESIAN_POINT ( 'NONE',  ( -0.1787899950787401604, -1.302165354276944242, -0.07405724077823318263 ) ) ;
#10059 = AXIS2_PLACEMENT_3D ( 'NONE', #33792, #24392, #27791 ) ;
#10060 = CARTESIAN_POINT ( 'NONE',  ( -0.1270800023317771588, -0.4685477465909196892, 0.1270800023317771588 ) ) ;
#10061 = CARTESIAN_POINT ( 'NONE',  ( -0.7185039370078746268, 0.06523048226347956391, 0.9621062991050720603 ) ) ;
#10062 = CARTESIAN_POINT ( 'NONE',  ( -0.7185039370078739607, 1.928577636452523993E-17, 0.6988188976377952555 ) ) ;
#10063 = CARTESIAN_POINT ( 'NONE',  ( 0.1574803149606300301, -0.2022637795275592509, -0.06523048226347956391 ) ) ;
#10064 = VECTOR ( 'NONE', #12133, 39.37007874015748143 ) ;
#10065 = COLOUR_RGB ( '', 0.31764706, 0.68627451, 0.89019608) ;
#10066 = CARTESIAN_POINT ( 'NONE',  ( 0.9873396505805591694, 0.1113553986120547346, 1.855314960522393530 ) ) ;
#10067 = CARTESIAN_POINT ( 'NONE',  ( 0.8107537697050253289, 0.1574803149606300301, 0.7308070866141725963 ) ) ;
#10068 = AXIS2_PLACEMENT_3D ( 'NONE', #34199, #41558, #19785 ) ;
#10069 = CARTESIAN_POINT ( 'NONE',  ( 0.1660477163177032645, -0.1996265385480603394, -0.03544556188505140759 ) ) ;
#10070 = CARTESIAN_POINT ( 'NONE',  ( -0.1574803149606300301, -0.06938976377952764396, -0.06523048226347956391 ) ) ;
#10071 = ADVANCED_FACE ( 'NONE', ( #30221 ), #45660, .F. ) ;
#10073 = CARTESIAN_POINT ( 'NONE',  ( 0.1644020957507539848, -0.1623118080249112138, 7.560884646099310910E-18 ) ) ;
#10072 = CARTESIAN_POINT ( 'NONE',  ( 0.1541343738003257691, 0.2065047100574138594, -0.03112915705353490325 ) ) ;
#10074 = CARTESIAN_POINT ( 'NONE',  ( 1.033464566929134687, -0.06523048226347956391, 1.099901574695623108 ) ) ;
#10075 = CARTESIAN_POINT ( 'NONE',  ( 0.7646288533564489232, -0.1113553986120547346, 0.1427165353255439029 ) ) ;
#10076 = ORIENTED_EDGE ( 'NONE', *, *, #44341, .F. ) ;
#10077 = EDGE_CURVE ( 'NONE', #1642, #35490, #37322, .T. ) ;
#10078 = CARTESIAN_POINT ( 'NONE',  ( 0.7646288533564489232, -0.1113553986120547346, 0.2312992125984252023 ) ) ;
#10079 = CARTESIAN_POINT ( 'NONE',  ( 1.033464566929133799, 1.928577636452524610E-17, 4.498031496062992574 ) ) ;
#10080 = CARTESIAN_POINT ( 'NONE',  ( 0.8759842519685039353, 0.1574803149606299191, 0.7185039369003465293 ) ) ;
#10081 = CARTESIAN_POINT ( 'NONE',  ( -0.1787899950787401604, -0.6328740156942683770, 0.07405724077823318263 ) ) ;
#10082 = CARTESIAN_POINT ( 'NONE',  ( -0.07405724077823318263, -1.425196850339937482, -0.1787899950787401604 ) ) ;
#10083 = CARTESIAN_POINT ( 'NONE',  ( -1.002407869896990045, 0.1264236179284866091, 1.916830708607653477 ) ) ;
#10084 = ORIENTED_EDGE ( 'NONE', *, *, #31884, .T. ) ;
#10085 = CARTESIAN_POINT ( 'NONE',  ( -1.054774247047244096, 0.000000000000000000, 1.444389763725763665 ) ) ;
#10086 = CARTESIAN_POINT ( 'NONE',  ( 0.7495606340400177148, 0.1264236179284866091, 1.498523621993480326 ) ) ;
#10087 = ORIENTED_EDGE ( 'NONE', *, *, #15948, .F. ) ;
#10088 = DIRECTION ( 'NONE',  ( 0.000000000000000000, 0.000000000000000000, 1.000000000000000000 ) ) ;
#10089 = CARTESIAN_POINT ( 'NONE',  ( -0.9500414927467378812, 0.1787899950787401604, 0.5856299212060785964 ) ) ;
#10090 = CARTESIAN_POINT ( 'NONE',  ( 0.09110444530572323063, -0.09842520415008684798, -0.1538371768615053592 ) ) ;
#10091 = CARTESIAN_POINT ( 'NONE',  ( 0.9500414927467377701, -0.1787899950787401604, 0.7677165353793073965 ) ) ;
#10092 = CARTESIAN_POINT ( 'NONE',  ( -1.002407869896990045, 0.1264236179284866091, 0.6176181101824566033 ) ) ;
#10093 = CIRCLE ( 'NONE', #36871, 0.009842519685039382085 ) ;
#10094 = DIRECTION ( 'NONE',  ( 1.000000000000000000, 0.000000000000000000, 0.000000000000000000 ) ) ;
#10095 = CIRCLE ( 'NONE', #1672, 0.08090551181102362266 ) ;
#10096 = CYLINDRICAL_SURFACE ( 'NONE', #36718, 0.1574803149606299191 ) ;
#10097 = ORIENTED_EDGE ( 'NONE', *, *, #19204, .T. ) ;
#10098 = CARTESIAN_POINT ( 'NONE',  ( -0.06523048226347956391, -0.1284448817822367028, 0.1574803149606297803 ) ) ;
#10099 = CARTESIAN_POINT ( 'NONE',  ( -0.8019270111902717657, -0.1787899950787401604, 1.392716535379308285 ) ) ;
#10100 = CARTESIAN_POINT ( 'NONE',  ( -1.033464566929134687, 0.06523048226347956391, 1.508366141732284449 ) ) ;
#10101 = CARTESIAN_POINT ( 'NONE',  ( -0.9873396505805591694, -0.1113553986120547346, 0.3986220472440945017 ) ) ;
#10102 = CARTESIAN_POINT ( 'NONE',  ( 0.9500414927467377701, -0.1787899950787401604, 1.358267716481669662 ) ) ;
#10103 = CARTESIAN_POINT ( 'NONE',  ( 0.1762355013749781762, -0.09851384352596320726, -0.09845540268461337730 ) ) ;
#10104 = AXIS2_PLACEMENT_3D ( 'NONE', #15674, #44861, #30080 ) ;
#10105 = VERTEX_POINT ( 'NONE', #16056 ) ;
#10106 = AXIS2_PLACEMENT_3D ( 'NONE', #25599, #17436, #17672 ) ;
#10107 = DIRECTION ( 'NONE',  ( -2.943801717310650128E-16, 1.000000000000000000, 2.355041373848525230E-15 ) ) ;
#10108 = ORIENTED_EDGE ( 'NONE', *, *, #41904, .T. ) ;
#10109 = CARTESIAN_POINT ( 'NONE',  ( 0.1264236179284866091, -1.684671212323726630, -0.1264236179284866091 ) ) ;
#10110 = EDGE_LOOP ( 'NONE', ( #18965, #34973, #46917, #11242, #12130, #14378, #16039, #23716 ) ) ;
#10111 = CARTESIAN_POINT ( 'NONE',  ( -0.1264236179284866091, -0.5861220471903307860, 0.1264236179284866091 ) ) ;
#10112 = CARTESIAN_POINT ( 'NONE',  ( 0.8107537697050254399, 0.1574803149606300301, 0.4945866141732282451 ) ) ;
#10113 = ORIENTED_EDGE ( 'NONE', *, *, #22172, .F. ) ;
#10114 = CYLINDRICAL_SURFACE ( 'NONE', #35396, 0.1574803149606299191 ) ;
#10115 = CARTESIAN_POINT ( 'NONE',  ( 0.1264236179284866091, -0.3449803149068665364, 0.1264236179284866091 ) ) ;
#10116 = CARTESIAN_POINT ( 'NONE',  ( -1.094772975963752103E-17, -0.7189960629383621571, -0.1787899950787401882 ) ) ;
#10117 = CARTESIAN_POINT ( 'NONE',  ( 0.000000000000000000, 0.9876813667277571929, 0.7893767492247212303 ) ) ;
#10118 = CARTESIAN_POINT ( 'NONE',  ( 0.1610681406152271733, -0.1591122530826964421, -4.473511402309723835E-08 ) ) ;
#10119 = CARTESIAN_POINT ( 'NONE',  ( 0.7495606340400177148, 0.1264236179284866091, 1.690452755851748146 ) ) ;
#10120 = CARTESIAN_POINT ( 'NONE',  ( 0.8759842519685039353, -0.1787899950787401882, 0.2878937007336381804 ) ) ;
#10121 = EDGE_CURVE ( 'NONE', #40935, #23379, #10503, .T. ) ;
#10122 = EDGE_CURVE ( 'NONE', #9701, #18496, #26607, .T. ) ;
#10123 = CARTESIAN_POINT ( 'NONE',  ( -0.1787899950787401604, -0.01882475563081354580, -0.07405724077823318263 ) ) ;
#10124 = ITEM_DEFINED_TRANSFORMATION ( 'NONE', 'NONE', #36219,  #20860 ) ;
#10125 = DIRECTION ( 'NONE',  ( -1.000000000000000000, 0.000000000000000000, 0.000000000000000000 ) ) ;
#10126 = CARTESIAN_POINT ( 'NONE',  ( -0.7185039370078778465, -0.06523048226348396317, 1.478838582569639071 ) ) ;
#10127 = CARTESIAN_POINT ( 'NONE',  ( 0.9500414927467378812, -0.1787899950787401604, 0.6053149605761579677 ) ) ;
#10128 = AXIS2_PLACEMENT_3D ( 'NONE', #1388, #16047, #34031 ) ;
#10129 = CARTESIAN_POINT ( 'NONE',  ( -1.054774247047244540, 0.07405724077823318263, 0.7775590550643457499 ) ) ;
#10130 = EDGE_CURVE ( 'NONE', #28079, #2953, #12467, .T. ) ;
#10132 = DIRECTION ( 'NONE',  ( 0.000000000000000000, 0.000000000000000000, -1.000000000000000000 ) ) ;
#10131 = CARTESIAN_POINT ( 'NONE',  ( 2.892866454678787531E-17, -0.8838582677165355284, 0.1574803149606299191 ) ) ;
#10134 = CARTESIAN_POINT ( 'NONE',  ( -0.8453766735112447916, -0.1708762415285247638, 1.987646152247962927 ) ) ;
#10133 = CARTESIAN_POINT ( 'NONE',  ( -0.1270800023317771588, -1.738232785960998061, -0.1270800023317771588 ) ) ;
#10135 = CARTESIAN_POINT ( 'NONE',  ( 1.054774247047244540, -0.07405724077823318263, 1.638779527505292988 ) ) ;
#10137 = CARTESIAN_POINT ( 'NONE',  ( -0.9873396505805591694, -0.1113553986120547346, 1.815944881889763884 ) ) ;
#10136 = CARTESIAN_POINT ( 'NONE',  ( 0.7495606340400177148, -0.1264236179284866091, 1.975885826717889815 ) ) ;
#10138 = CARTESIAN_POINT ( 'NONE',  ( 0.9500414927467377701, -0.1787899950787401604, 0.4084645668753704162 ) ) ;
#10139 = CIRCLE ( 'NONE', #43786, 0.3814023619577306956 ) ;
#10140 = APPLICATION_CONTEXT ( 'automotive_design' ) ;
#10141 = ADVANCED_FACE ( 'NONE', ( #38081 ), #31176, .F. ) ;
#10142 = CARTESIAN_POINT ( 'NONE',  ( 0.1871882013110628684, -0.1874210200766982803, -0.3098131533094808931 ) ) ;
#10143 = CARTESIAN_POINT ( 'NONE',  ( 0.1787899950787401604, -0.06200787396198446239, -0.07405724077823318263 ) ) ;
#10144 = CARTESIAN_POINT ( 'NONE',  ( 0.6971942568897626646, 0.07405724077823318263, 0.5905511810485987167 ) ) ;
#10145 = CARTESIAN_POINT ( 'NONE',  ( 3.284318927891251994E-17, -0.8567913385289133155, 0.1787899950787401882 ) ) ;
#10146 = CARTESIAN_POINT ( 'NONE',  ( 1.054774247047244540, 0.07405724077823318263, 0.1476377952218269618 ) ) ;
#10147 = DIRECTION ( 'NONE',  ( 0.000000000000000000, -0.7880107536067207930, 0.6156614753256598460 ) ) ;
#10148 = CARTESIAN_POINT ( 'NONE',  ( 0.8759842519685039353, 0.1787899950787401882, 0.5437992125446614589 ) ) ;
#10149 = CARTESIAN_POINT ( 'NONE',  ( 0.4453382816733590377, 0.09842519685039370636, 0.000000000000000000 ) ) ;
#10150 = CARTESIAN_POINT ( 'NONE',  ( -1.002407869896990045, 0.1264236179284866091, 1.483759842465921075 ) ) ;
#10151 = ORIENTED_EDGE ( 'NONE', *, *, #40985, .T. ) ;
#10152 = CIRCLE ( 'NONE', #11696, 0.1968503937007874127 ) ;
#10153 = CARTESIAN_POINT ( 'NONE',  ( -0.3069380822740675474, -0.04406989549021587960, -0.7144743529967967355 ) ) ;
#10154 = CARTESIAN_POINT ( 'NONE',  ( 0.6971942568897637749, 2.189545951927499583E-17, 1.109744094434425232 ) ) ;
#10155 = DIRECTION ( 'NONE',  ( -1.000000000000000000, 0.000000000000000000, 0.000000000000000000 ) ) ;
#10156 = CARTESIAN_POINT ( 'NONE',  ( 1.054774247047244096, 0.000000000000000000, 1.754429133804503715 ) ) ;
#10157 = CARTESIAN_POINT ( 'NONE',  ( -0.8759842519685039353, -0.1574803149606299191, 1.338582677165354395 ) ) ;
#10158 = CARTESIAN_POINT ( 'NONE',  ( -0.6971942568897626646, -0.07405724077823297447, 0.9104330708123776761 ) ) ;
#10159 = CARTESIAN_POINT ( 'NONE',  ( -0.7185039370078746268, 0.06523048226347956391, 0.5290354329633386588 ) ) ;
#10160 = CARTESIAN_POINT ( 'NONE',  ( -0.7184511836828970655, -0.06596510897976094745, 0.03937007874015842346 ) ) ;
#10161 = CARTESIAN_POINT ( 'NONE',  ( 0.6971942568897626646, 0.07405724077823318263, 0.2017716534895435399 ) ) ;
#10162 = UNCERTAINTY_MEASURE_WITH_UNIT (LENGTH_MEASURE( 1.000000000000000082E-05 ), #26700, 'distance_accuracy_value', 'NONE') ;
#10163 = CARTESIAN_POINT ( 'NONE',  ( 1.033464566929134687, 0.06523048226347956391, 1.577263779420032153 ) ) ;
#10164 = ORIENTED_EDGE ( 'NONE', *, *, #8101, .T. ) ;
#10165 = CARTESIAN_POINT ( 'NONE',  ( -0.1787899950787401882, 0.03395669296714932950, 0.000000000000000000 ) ) ;
#10166 = ORIENTED_EDGE ( 'NONE', *, *, #20083, .F. ) ;
#10167 = CARTESIAN_POINT ( 'NONE',  ( 0.8759842519685039353, -0.1787899950787401882, 0.8046259841982047467 ) ) ;
#10168 = CARTESIAN_POINT ( 'NONE',  ( -0.8019270111902716547, 0.1787899950787401604, 1.727362204670645385 ) ) ;
#10169 = CARTESIAN_POINT ( 'NONE',  ( 0.1787899950787401604, -1.474409448765133801, -0.07405724077823318263 ) ) ;
#10170 = ( BOUNDED_CURVE ( )  B_SPLINE_CURVE ( 2, ( #15431, #19714, #540, #22605, #41249, #4851, #15196, #30534, #45096 ),
 .UNSPECIFIED., .F., .F. ) 
 B_SPLINE_CURVE_WITH_KNOTS ( ( 3, 2, 2, 2, 3 ),
 ( 0.7199999999999999734, 0.7225000000000000311, 0.7249999999999999778, 0.7275000000000000355, 0.7299999999999999822 ),
 .UNSPECIFIED. ) 
 CURVE ( )  GEOMETRIC_REPRESENTATION_ITEM ( )  RATIONAL_B_SPLINE_CURVE ( ( 1.000000000000000000, 0.9238795325112869605, 1.000000000000000000, 0.9238795325112869605, 1.000000000000000000, 0.9238795325112869605, 1.000000000000000000, 0.9238795325112869605, 1.000000000000000000 ) ) 
 REPRESENTATION_ITEM ( '' )  ) ;
#10171 = CIRCLE ( 'NONE', #26266, 0.09842519685039370636 ) ;
#10172 = CARTESIAN_POINT ( 'NONE',  ( -1.033464566929134687, 0.06523048226347956391, 0.6422244094488180899 ) ) ;
#10173 = CARTESIAN_POINT ( 'NONE',  ( -0.8107537697050254399, -0.1574803149606297803, 0.7849409448818904789 ) ) ;
#10174 = CARTESIAN_POINT ( 'NONE',  ( 0.1787899950787401882, -1.256521606024513904, -2.189545951927503898E-17 ) ) ;
#10175 = ORIENTED_EDGE ( 'NONE', *, *, #3361, .T. ) ;
#10176 = CARTESIAN_POINT ( 'NONE',  ( -0.07405724077823318263, -0.1112204723871813017, 0.1787899950787401604 ) ) ;
#10177 = EDGE_LOOP ( 'NONE', ( #40262, #3767, #11982, #12660 ) ) ;
#10178 = ( GEOMETRIC_REPRESENTATION_CONTEXT ( 3 ) GLOBAL_UNCERTAINTY_ASSIGNED_CONTEXT ( ( #42710 ) ) GLOBAL_UNIT_ASSIGNED_CONTEXT ( ( #26645, #38118, #23027 ) ) REPRESENTATION_CONTEXT ( 'NONE', 'WORKASPACE' ) ) ;
#10179 = AXIS2_PLACEMENT_3D ( 'NONE', #41044, #19015, #4164 ) ;
#10180 = EDGE_CURVE ( 'NONE', #29530, #18116, #12708, .T. ) ;
#10181 = DIRECTION ( 'NONE',  ( -1.000000000000000000, 0.000000000000000000, 0.000000000000000000 ) ) ;
#10182 = CARTESIAN_POINT ( 'NONE',  ( 0.7646288533564489232, -0.1113553986120547346, 1.924212598425196985 ) ) ;
#10183 = EDGE_CURVE ( 'NONE', #33815, #26576, #28117, .T. ) ;
#10184 = CARTESIAN_POINT ( 'NONE',  ( -0.07405724077823318263, -1.415354330654897019, 0.1787899950787401604 ) ) ;
#10185 = CARTESIAN_POINT ( 'NONE',  ( -1.094772975963752103E-17, -0.7632874015210393548, -0.1787899950787401882 ) ) ;
#10186 = ( BOUNDED_CURVE ( )  B_SPLINE_CURVE ( 2, ( #28728, #3035, #6638, #36598, #18378, #46418, #17666, #14083, #10498 ),
 .UNSPECIFIED., .F., .F. ) 
 B_SPLINE_CURVE_WITH_KNOTS ( ( 3, 2, 2, 2, 3 ),
 ( 0.05999999999999999778, 0.06250000000000000000, 0.06500000000000000222, 0.06750000000000000444, 0.07000000000000000666 ),
 .UNSPECIFIED. ) 
 CURVE ( )  GEOMETRIC_REPRESENTATION_ITEM ( )  RATIONAL_B_SPLINE_CURVE ( ( 1.000000000000000000, 0.9238795325112869605, 1.000000000000000000, 0.9238795325112869605, 1.000000000000000000, 0.9238795325112869605, 1.000000000000000000, 0.9238795325112869605, 1.000000000000000000 ) ) 
 REPRESENTATION_ITEM ( '' )  ) ;
#10187 = CARTESIAN_POINT ( 'NONE',  ( -0.6971942568897626646, 0.07405724077823318263, 0.3198818897100159098 ) ) ;
#10188 = CARTESIAN_POINT ( 'NONE',  ( 0.07444174185955046430, -1.273173730842887208, -0.1797182628040039087 ) ) ;
#10189 = DIRECTION ( 'NONE',  ( -1.000000000000000000, 3.469446951953613794E-15, 0.000000000000000000 ) ) ;
#10190 = CARTESIAN_POINT ( 'NONE',  ( 0.9500414927467378812, 0.1787899950787401604, 1.215551181048599272 ) ) ;
#10191 = CARTESIAN_POINT ( 'NONE',  ( 0.7495606340400177148, 0.1264236179284866091, 1.493602362150960650 ) ) ;
#10192 = CARTESIAN_POINT ( 'NONE',  ( -0.2066929133858267931, 0.08669520607260541856, -0.1182208702464773997 ) ) ;
#10193 = AXIS2_PLACEMENT_3D ( 'NONE', #33375, #26885, #4556 ) ;
#10195 = CARTESIAN_POINT ( 'NONE',  ( 0.7646288533564489232, -0.1113553986120547346, 1.520669291231054876 ) ) ;
#10194 = CARTESIAN_POINT ( 'NONE',  ( 0.1645805304145094572, 0.08212604421147362554, 0.1405696318538273704 ) ) ;
#10196 = CARTESIAN_POINT ( 'NONE',  ( -1.033464566929134687, -0.06523048226347956391, 1.690452755797984929 ) ) ;
#10197 = CARTESIAN_POINT ( 'NONE',  ( 0.07405724077823318263, 0.02657480320336980464, -0.1787899950787401604 ) ) ;
#10198 = CARTESIAN_POINT ( 'NONE',  ( 0.9500414927467378812, 0.1787899950787401604, 0.2263779527021421711 ) ) ;
#10199 = MECHANICAL_DESIGN_GEOMETRIC_PRESENTATION_REPRESENTATION (  '', ( #25515 ), #31637 ) ;
#10200 = CARTESIAN_POINT ( 'NONE',  ( -0.9412147342319837628, 0.1574803149606300301, 1.552657480314961758 ) ) ;
#10202 = CARTESIAN_POINT ( 'NONE',  ( -0.9873396505805591694, -0.1113553986120547346, 0.5462598424121581919 ) ) ;
#10201 = CARTESIAN_POINT ( 'NONE',  ( 0.7495606340400177148, 0.1264236179284866091, 1.099901574749385880 ) ) ;
#10203 = ADVANCED_FACE ( 'NONE', ( #45719 ), #12935, .T. ) ;
#10204 = CARTESIAN_POINT ( 'NONE',  ( 0.8070866141732283561, -0.3937007874015746034, -0.7574803149606299524 ) ) ;
#10205 = CARTESIAN_POINT ( 'NONE',  ( 0.7185039370078746268, 0.06523048226347956391, 0.5684055117034967353 ) ) ;
#10206 = ORIENTED_EDGE ( 'NONE', *, *, #12485, .F. ) ;
#10207 = CARTESIAN_POINT ( 'NONE',  ( 0.9652740342186406641, 0.1428087511534603948, 0.03937007787513571028 ) ) ;
#10208 = AXIS2_PLACEMENT_3D ( 'NONE', #192, #433, #17944 ) ;
#10209 = VECTOR ( 'NONE', #4959, 39.37007874015748143 ) ;
#10210 = CARTESIAN_POINT ( 'NONE',  ( -0.8759842519685039353, 0.1574803149606299191, 0.4429133857192448787 ) ) ;
#10211 = EDGE_LOOP ( 'NONE', ( #4768, #46041, #20532, #19612 ) ) ;
#10212 = CARTESIAN_POINT ( 'NONE',  ( 1.002407869896990045, -0.1264236179284866091, 1.513287401521039355 ) ) ;
#10213 = CARTESIAN_POINT ( 'NONE',  ( -0.8759842519685039353, 0.1574803149606299191, 1.633858267716535639 ) ) ;
#10214 = CARTESIAN_POINT ( 'NONE',  ( 0.07405724077823318263, 0.05118110241596821736, 0.1787899950787401604 ) ) ;
#10215 = ORIENTED_EDGE ( 'NONE', *, *, #47297, .T. ) ;
#10216 = CARTESIAN_POINT ( 'NONE',  ( 0.1377952755905509641, 1.687505431895956722E-17, -0.06545654452343109553 ) ) ;
#10217 = ORIENTED_EDGE ( 'NONE', *, *, #34003, .F. ) ;
#10218 = CARTESIAN_POINT ( 'NONE',  ( 0.1235961452251413406, 0.09842519685039370636, 0.2140748031496062798 ) ) ;
#10219 = CARTESIAN_POINT ( 'NONE',  ( 0.5236220472440944462, 4.616380251121755931E-17, 0.000000000000000000 ) ) ;
#10220 = ORIENTED_EDGE ( 'NONE', *, *, #42560, .T. ) ;
#10221 = CARTESIAN_POINT ( 'NONE',  ( 0.6971942568897637749, 2.189545951927499583E-17, 0.5979330708123780092 ) ) ;
#10222 = VERTEX_POINT ( 'NONE', #38556 ) ;
#10223 = CARTESIAN_POINT ( 'NONE',  ( 0.07405724077823318263, -1.710629921206078041, -0.1787899950787401604 ) ) ;
#10224 = CARTESIAN_POINT ( 'NONE',  ( -0.9500414927467378812, -0.1787899950787401604, 1.200787401521039355 ) ) ;
#10225 = CARTESIAN_POINT ( 'NONE',  ( -0.8759842519685039353, -0.1787899950787401882, 1.941437007820252081 ) ) ;
#10226 = ORIENTED_EDGE ( 'NONE', *, *, #27723, .T. ) ;
#10227 = CARTESIAN_POINT ( 'NONE',  ( -1.002407869896990045, 0.1264236179284866091, 1.129429133804503937 ) ) ;
#10228 = CARTESIAN_POINT ( 'NONE',  ( -1.054774247047244540, 0.07405724077823318263, 0.7775590550643479704 ) ) ;
#10229 = CARTESIAN_POINT ( 'NONE',  ( -0.8759842519685039353, 0.000000000000000000, 0.000000000000000000 ) ) ;
#10230 = DIRECTION ( 'NONE',  ( 0.000000000000000000, 0.000000000000000000, -1.000000000000000000 ) ) ;
#10231 = CARTESIAN_POINT ( 'NONE',  ( -1.094772975963752103E-17, -0.7348680627174272173, -0.1787899950787401882 ) ) ;
#10232 = ORIENTED_EDGE ( 'NONE', *, *, #10750, .F. ) ;
#10233 = CARTESIAN_POINT ( 'NONE',  ( -1.033464566929134687, 0.06523048226347956391, 1.459153543199560144 ) ) ;
#10234 = CARTESIAN_POINT ( 'NONE',  ( 2.892866454678787531E-17, -0.08661417312081949593, 0.1574803149606299191 ) ) ;
#10235 = ORIENTED_EDGE ( 'NONE', *, *, #11655, .T. ) ;
#10236 = DIRECTION ( 'NONE',  ( 0.000000000000000000, -1.000000000000000000, 0.000000000000000000 ) ) ;
#10237 = EDGE_CURVE ( 'NONE', #1846, #26918, #46456, .T. ) ;
#10238 = CARTESIAN_POINT ( 'NONE',  ( -1.033464566929133799, 0.000000000000000000, 0.5511811022546772021 ) ) ;
#10239 = CARTESIAN_POINT ( 'NONE',  ( -0.9500414927467378812, 0.1787899950787401604, 0.6988188975840318173 ) ) ;
#10240 = CARTESIAN_POINT ( 'NONE',  ( 0.1574803149606300301, 0.06840551181102358380, 0.06523048226347956391 ) ) ;
#10241 = EDGE_CURVE ( 'NONE', #22983, #44566, #24277, .T. ) ;
#10242 = B_SPLINE_CURVE_WITH_KNOTS ( 'NONE', 3,
 ( #39959, #44489, #175, #33054, #22001, #880, #36404, #25844, #10772, #36858, #18175, #29943 ),
 .UNSPECIFIED., .F., .F.,
 ( 4, 2, 2, 2, 2, 4 ),
 ( 0.000000000000000000, 0.2500000000000002220, 0.3750000000000004441, 0.4375000000000005551, 0.5000000000000006661, 1.000000000000000000 ),
 .UNSPECIFIED. ) ;
#10243 = EDGE_CURVE ( 'NONE', #44955, #14452, #31944, .T. ) ;
#10244 = CARTESIAN_POINT ( 'NONE',  ( -0.8019270111902716547, 0.1787899950787401604, 1.653543307032850462 ) ) ;
#10245 = AXIS2_PLACEMENT_3D ( 'NONE', #40673, #18652, #33310 ) ;
#10246 = EDGE_CURVE ( 'NONE', #41905, #6896, #24201, .T. ) ;
#10247 = DIRECTION ( 'NONE',  ( -1.000000000000000000, 0.000000000000000000, 0.000000000000000000 ) ) ;
#10248 = CARTESIAN_POINT ( 'NONE',  ( 0.000000000000000000, 0.000000000000000000, -0.3149606299212598381 ) ) ;
#10249 = DIRECTION ( 'NONE',  ( 0.000000000000000000, 0.000000000000000000, 1.000000000000000000 ) ) ;
#10250 = CARTESIAN_POINT ( 'NONE',  ( -0.1797182628040039087, -0.8253390851735974421, 0.07444174185955065859 ) ) ;
#10251 = FACE_OUTER_BOUND ( 'NONE', #10712, .T. ) ;
#10252 = VECTOR ( 'NONE', #11306, 39.37007874015748143 ) ;
#10253 = CARTESIAN_POINT ( 'NONE',  ( 0.7495606340400177148, 0.1264236179284866091, 0.7504921259304880854 ) ) ;
#10254 = CARTESIAN_POINT ( 'NONE',  ( 2.892866454678787531E-17, -0.5295275590551181688, 0.1574803149606299191 ) ) ;
#10255 = CARTESIAN_POINT ( 'NONE',  ( -0.03350953465935899850, 0.1209034135645020575, -0.1556370229766415314 ) ) ;
#10256 = ORIENTED_EDGE ( 'NONE', *, *, #31779, .F. ) ;
#10257 = CARTESIAN_POINT ( 'NONE',  ( -0.3690944881889761109, 0.1864803149606358568, -0.7480314960629921295 ) ) ;
#10258 = CARTESIAN_POINT ( 'NONE',  ( 1.033464566929133799, 0.000000000000000000, 1.230314960629921295 ) ) ;
#10260 = CARTESIAN_POINT ( 'NONE',  ( 0.1574803149606299191, -5.122214988120488358E-16, -8.878505979408856939E-16 ) ) ;
#10259 = CARTESIAN_POINT ( 'NONE',  ( 0.9317429405948658427, -0.1672133690053895227, 1.989191746694990881 ) ) ;
#10261 = CARTESIAN_POINT ( 'NONE',  ( 0.7646288533564489232, -0.1113553986120547346, 1.963582677165354395 ) ) ;
#10263 = CARTESIAN_POINT ( 'NONE',  ( -0.1377952755905511861, 0.1564960629921283985, -0.8070866141732283561 ) ) ;
#10262 = CARTESIAN_POINT ( 'NONE',  ( 0.7495606340400177148, -0.1264236179284866091, 0.6373031495525354195 ) ) ;
#10264 = FACE_OUTER_BOUND ( 'NONE', #15590, .T. ) ;
#10265 = DIRECTION ( 'NONE',  ( 1.000000000000000000, 0.000000000000000000, -0.000000000000000000 ) ) ;
#10266 = CARTESIAN_POINT ( 'NONE',  ( 0.1564216623530369499, 0.006801955215764789002, -0.1403857474672217109 ) ) ;
#10267 = CARTESIAN_POINT ( 'NONE',  ( 0.6971942568897626646, -0.07405724077823297447, 0.9498031495525356416 ) ) ;
#10268 = VERTEX_POINT ( 'NONE', #3049 ) ;
#10269 = CARTESIAN_POINT ( 'NONE',  ( -1.033464566929133799, 1.928577636452524610E-17, 2.869337061179095023E-17 ) ) ;
#10270 = DIRECTION ( 'NONE',  ( -0.000000000000000000, 1.000000000000000000, -0.000000000000000000 ) ) ;
#10271 = CARTESIAN_POINT ( 'NONE',  ( -0.1797182628040039365, 0.1564522534090805050, 0.000000000000000000 ) ) ;
#10272 = CARTESIAN_POINT ( 'NONE',  ( 0.1264236179284866091, -1.053641732229700700, 0.1264236179284866091 ) ) ;
#10273 = CARTESIAN_POINT ( 'NONE',  ( 0.1113553986120547346, -1.459645669291338432, -0.1113553986120547346 ) ) ;
#10274 = LINE ( 'NONE', #7140, #25258 ) ;
#10275 = ORIENTED_EDGE ( 'NONE', *, *, #33628, .F. ) ;
#10276 = CARTESIAN_POINT ( 'NONE',  ( -1.054774247047244096, 0.000000000000000000, 0.02214566923757503927 ) ) ;
#10277 = ORIENTED_EDGE ( 'NONE', *, *, #21912, .T. ) ;
#10278 = ORIENTED_EDGE ( 'NONE', *, *, #6147, .T. ) ;
#10279 = CARTESIAN_POINT ( 'NONE',  ( -0.1476377952755905387, -0.2274162997038010614, -0.9219983537151217323 ) ) ;
#10280 = ORIENTED_EDGE ( 'NONE', *, *, #22414, .T. ) ;
#10281 = CARTESIAN_POINT ( 'NONE',  ( -0.1574803149606297803, -1.432578740049952781, 0.06523048226347956391 ) ) ;
#10282 = CARTESIAN_POINT ( 'NONE',  ( -1.054774247047244540, -0.07405724077823318263, 1.874999999946236784 ) ) ;
#10283 = CARTESIAN_POINT ( 'NONE',  ( -0.7495606340400177148, 0.1264236179284866091, 1.493602362150960650 ) ) ;
#10284 = CARTESIAN_POINT ( 'NONE',  ( 1.002407869896990045, 0.1264236179284866091, 0.8193897637257637756 ) ) ;
#10285 = CARTESIAN_POINT ( 'NONE',  ( -1.054774247047244540, -0.07405724077823318263, 1.082677165300567346 ) ) ;
#10286 = ADVANCED_FACE ( 'NONE', ( #13611 ), #21031, .T. ) ;
#10287 = CARTESIAN_POINT ( 'NONE',  ( -1.002407869896990045, -0.1264236179284866091, 0.2189960629383626012 ) ) ;
#10288 = CARTESIAN_POINT ( 'NONE',  ( -0.2471922904502825702, 0.07695608958885592765, 0.07926021241888449309 ) ) ;
#10289 = CARTESIAN_POINT ( 'NONE',  ( -0.6971942568897637749, 2.189545951927499583E-17, 1.975885826717889815 ) ) ;
#10290 = CARTESIAN_POINT ( 'NONE',  ( -0.7185039370078739607, 1.928577636452523993E-17, 0.3051181102362204856 ) ) ;
#10291 = CARTESIAN_POINT ( 'NONE',  ( -0.7646288533564489232, -0.1113553986120547346, 1.884842519685039353 ) ) ;
#10292 = CARTESIAN_POINT ( 'NONE',  ( 0.2559053792588102949, 0.1035705208482406714, -0.06897712937227379326 ) ) ;
#10293 = CARTESIAN_POINT ( 'NONE',  ( -1.094772975963752103E-17, -0.2230570390953807158, -0.1787899950787401882 ) ) ;
#10294 = CARTESIAN_POINT ( 'NONE',  ( 0.2066929133858268486, -0.3022687907404924545, -1.075852903322848331 ) ) ;
#10295 = DIRECTION ( 'NONE',  ( 0.000000000000000000, -0.6156614753256598460, -0.7880107536067207930 ) ) ;
#10296 = CARTESIAN_POINT ( 'NONE',  ( -0.9500414927467378812, 0.1787899950787401604, 0.1082677164816695514 ) ) ;
#10297 = ADVANCED_FACE ( 'NONE', ( #2580 ), #20337, .T. ) ;
#10298 = EDGE_LOOP ( 'NONE', ( #19771, #29545, #36806, #30252 ) ) ;
#10299 = EDGE_CURVE ( 'NONE', #39650, #9619, #1486, .T. ) ;
#10300 = CARTESIAN_POINT ( 'NONE',  ( -0.7495606340400177148, 0.1264236179284866091, 1.222933070812378009 ) ) ;
#10301 = ORIENTED_EDGE ( 'NONE', *, *, #45389, .F. ) ;
#10302 = ADVANCED_FACE ( 'NONE', ( #42588 ), #28156, .T. ) ;
#10303 = CARTESIAN_POINT ( 'NONE',  ( -0.1264236179284866091, -1.152066929080094448, -0.1264236179284866091 ) ) ;
#10304 = CARTESIAN_POINT ( 'NONE',  ( -0.1787899950787401882, -1.457185039316315045, 0.000000000000000000 ) ) ;
#10305 = DIRECTION ( 'NONE',  ( -1.000000000000000000, 0.000000000000000000, 0.000000000000000000 ) ) ;
#10306 = CARTESIAN_POINT ( 'NONE',  ( 0.000000000000000000, -0.5708661417322835607, -6.991093932140394160E-17 ) ) ;
#10307 = CARTESIAN_POINT ( 'NONE',  ( -0.7646288533564489232, -0.1113553986120547346, 0.8907480313885355327 ) ) ;
#10308 = CARTESIAN_POINT ( 'NONE',  ( -0.9873396505805591694, 0.1113553986120547346, 0.7234251968503936370 ) ) ;
#10309 = CARTESIAN_POINT ( 'NONE',  ( 0.1113553986120547346, -0.08169291338582677919, -0.1113553986120547346 ) ) ;
#10310 = VECTOR ( 'NONE', #30547, 39.37007874015748143 ) ;
#10311 = CARTESIAN_POINT ( 'NONE',  ( 0.7185039370078746268, -0.06523048226347956391, 1.793799212490897244 ) ) ;
#10312 = EDGE_LOOP ( 'NONE', ( #22832, #36137, #15653, #27504 ) ) ;
#10313 = DIRECTION ( 'NONE',  ( 0.000000000000000000, 0.000000000000000000, -1.000000000000000000 ) ) ;
#10314 = CARTESIAN_POINT ( 'NONE',  ( 1.033464566929134687, 0.06523048226347956391, 0.8390748031496061410 ) ) ;
#10315 = CARTESIAN_POINT ( 'NONE',  ( 0.05824109077986203142, -0.2618687228227581376, -0.05388431474956601602 ) ) ;
#10316 = CARTESIAN_POINT ( 'NONE',  ( -0.06523048226347956391, -0.05954724409448820810, 0.1574803149606297803 ) ) ;
#10318 = CARTESIAN_POINT ( 'NONE',  ( 0.8759842519685039353, 0.1574803149606299191, 1.515748031496062964 ) ) ;
#10317 = CARTESIAN_POINT ( 'NONE',  ( 1.033464566929133799, 0.000000000000000000, 0.2362204723334177248 ) ) ;
#10319 = CARTESIAN_POINT ( 'NONE',  ( 0.7185039370078739607, 1.928577636452523993E-17, 0.2165354329633393804 ) ) ;
#10320 = ORIENTED_EDGE ( 'NONE', *, *, #36131, .T. ) ;
#10321 = ADVANCED_FACE ( 'NONE', ( #14099 ), #31620, .T. ) ;
#10322 = CARTESIAN_POINT ( 'NONE',  ( -0.9412147342319837628, -0.1574803149606297803, 0.6225393699712132856 ) ) ;
#10323 = CARTESIAN_POINT ( 'NONE',  ( -9.642888182262618425E-18, -1.523622047136566682, -0.1574803149606299191 ) ) ;
#10324 = CARTESIAN_POINT ( 'NONE',  ( 0.1787899950787401882, -0.6156496062454488438, -2.189545951927503898E-17 ) ) ;
#10325 = CARTESIAN_POINT ( 'NONE',  ( 0.1113553986120547346, -1.065944881889763662, -0.1113553986120547346 ) ) ;
#10326 = CARTESIAN_POINT ( 'NONE',  ( 0.7646288533564489232, 0.1113553986120547346, 0.9596456691838111119 ) ) ;
#10327 = CARTESIAN_POINT ( 'NONE',  ( 0.1574803149606299746, 0.1473293504822046074, -0.9532488779249699284 ) ) ;
#10328 = CARTESIAN_POINT ( 'NONE',  ( -0.7495606340400177148, -0.1264236179284866091, 0.4010826771115905687 ) ) ;
#10329 = ORIENTED_EDGE ( 'NONE', *, *, #42294, .T. ) ;
#10330 = ORIENTED_EDGE ( 'NONE', *, *, #30656, .F. ) ;
#10331 = CARTESIAN_POINT ( 'NONE',  ( -0.8019270111902717657, 0.1787899950787401604, 1.535433070812378675 ) ) ;
#10332 = CARTESIAN_POINT ( 'NONE',  ( 0.8759842519685039353, 0.1787899950787401882, 1.493602362150960650 ) ) ;
#10333 = ORIENTED_EDGE ( 'NONE', *, *, #16196, .F. ) ;
#10334 = CARTESIAN_POINT ( 'NONE',  ( 0.7185039370078739607, 1.928577636452523993E-17, 1.082677165246803241 ) ) ;
#10335 = CARTESIAN_POINT ( 'NONE',  ( -1.054774247047244096, 0.000000000000000000, 0.6176181101824566033 ) ) ;
#10336 = CARTESIAN_POINT ( 'NONE',  ( 0.7495606340400177148, -0.1264236179284866091, 0.2091535432533232486 ) ) ;
#10337 = CONICAL_SURFACE ( 'NONE', #34066, 0.1003937007874011050, 0.7853981633973787790 ) ;
#10338 = CARTESIAN_POINT ( 'NONE',  ( -0.8759842519685039353, 0.1574803149606299191, 0.2559055118110236116 ) ) ;
#10339 = CARTESIAN_POINT ( 'NONE',  ( -0.6971942568897648851, 0.07405724077823318263, 0.7086614172690703928 ) ) ;
#10340 = CARTESIAN_POINT ( 'NONE',  ( 0.8759842519685039353, -0.1574803149606299191, 0.6299212598425196763 ) ) ;
#10341 = ( BOUNDED_CURVE ( )  B_SPLINE_CURVE ( 2, ( #34464, #16264, #30898, #45454, #12676, #21004, #43040, #39452, #32055 ),
 .UNSPECIFIED., .F., .T. ) 
 B_SPLINE_CURVE_WITH_KNOTS ( ( 3, 2, 2, 2, 3 ),
 ( 0.5000000000000000000, 0.5024999999999999467, 0.5050000000000000044, 0.5074999999999999512, 0.5100000000000000089 ),
 .UNSPECIFIED. ) 
 CURVE ( )  GEOMETRIC_REPRESENTATION_ITEM ( )  RATIONAL_B_SPLINE_CURVE ( ( 1.000000000000000000, 0.9238795325112869605, 1.000000000000000000, 0.9238795325112869605, 1.000000000000000000, 0.9238795325112869605, 1.000000000000000000, 0.9238795325112869605, 1.000000000000000000 ) ) 
 REPRESENTATION_ITEM ( '' )  ) ;
#10342 = FACE_OUTER_BOUND ( 'NONE', #17265, .T. ) ;
#10343 = CARTESIAN_POINT ( 'NONE',  ( 0.06523048226347956391, -0.2268700786326303398, -0.1574803149606300301 ) ) ;
#10344 = CARTESIAN_POINT ( 'NONE',  ( -1.054774247047244096, 0.000000000000000000, 1.365649606245448844 ) ) ;
#10345 = AXIS2_PLACEMENT_3D ( 'NONE', #40477, #7661, #18917 ) ;
#10346 = CARTESIAN_POINT ( 'NONE',  ( -0.8759842519685039353, -0.1574803149606299191, 0.5118110236220472231 ) ) ;
#10347 = CARTESIAN_POINT ( 'NONE',  ( 0.7495606340400177148, 0.1264236179284866091, 1.341043307032850462 ) ) ;
#10348 = CARTESIAN_POINT ( 'NONE',  ( -0.05992402829640944978, -0.09851383910125414978, -0.1770211755185344404 ) ) ;
#10349 = AXIS2_PLACEMENT_3D ( 'NONE', #30423, #23674, #38281 ) ;
#10350 = AXIS2_PLACEMENT_3D ( 'NONE', #44745, #4980, #9057 ) ;
#10351 = ORIENTED_EDGE ( 'NONE', *, *, #11409, .T. ) ;
#10352 = CARTESIAN_POINT ( 'NONE',  ( -0.8107537697050254399, -0.1574803149606297803, 0.6274606299212601712 ) ) ;
#10353 = EDGE_CURVE ( 'NONE', #3953, #40227, #17444, .T. ) ;
#10354 = CARTESIAN_POINT ( 'NONE',  ( 0.07405724077823318263, -1.736344440670183120, 0.1787899950787401604 ) ) ;
#10355 = ORIENTED_EDGE ( 'NONE', *, *, #5473, .F. ) ;
#10356 = CARTESIAN_POINT ( 'NONE',  ( 0.1787899950787401882, -0.6894685038832439883, -2.189545951927503898E-17 ) ) ;
#10357 = CARTESIAN_POINT ( 'NONE',  ( -0.1574803149606299191, 0.7443365962042343131, -3.523993443072799270 ) ) ;
#10358 = EDGE_LOOP ( 'NONE', ( #22529, #42334, #12122, #27521 ) ) ;
#10359 = EDGE_CURVE ( 'NONE', #22756, #27408, #46200, .T. ) ;
#10360 = FACE_OUTER_BOUND ( 'NONE', #35417, .T. ) ;
#10361 = CARTESIAN_POINT ( 'NONE',  ( -0.1264236179284866091, -0.3252952755367877757, -0.1264236179284866091 ) ) ;
#10362 = CARTESIAN_POINT ( 'NONE',  ( -0.1264236179284866091, -0.8321850393163149340, -0.1264236179284866091 ) ) ;
#10363 = DIRECTION ( 'NONE',  ( 0.000000000000000000, 0.000000000000000000, -1.000000000000000000 ) ) ;
#10364 = CARTESIAN_POINT ( 'NONE',  ( 0.1643592525012025352, -0.1621847908751006817, -1.511614865314615023E-06 ) ) ;
#10365 = CARTESIAN_POINT ( 'NONE',  ( 0.6971942568897648851, -0.07405724077823297447, 1.697834645615527771 ) ) ;
#10366 = CARTESIAN_POINT ( 'NONE',  ( 1.002407869896990045, 0.1264236179284866091, 0.3026574802611972648 ) ) ;
#10367 = PRODUCT_DEFINITION_SHAPE ( 'NONE', 'NONE',  #47475 ) ;
#10368 = CARTESIAN_POINT ( 'NONE',  ( -0.07405724077823318263, -0.06311609421349069493, -0.1787899950787401604 ) ) ;
#10369 = CARTESIAN_POINT ( 'NONE',  ( 0.1476377952755906220, -0.4872761608334559846, -0.8688576204587790119 ) ) ;
#10370 = CARTESIAN_POINT ( 'NONE',  ( 0.9412147342319837628, 0.1574803149606300301, 0.5585629920184573827 ) ) ;
#10371 = CARTESIAN_POINT ( 'NONE',  ( -0.9500414927467377701, -0.1787899950787401604, 0.9645669290800954476 ) ) ;
#10373 = CARTESIAN_POINT ( 'NONE',  ( 0.8107537697050254399, 0.1574803149606300301, 1.705216535325545069 ) ) ;
#10372 = CARTESIAN_POINT ( 'NONE',  ( -1.033464566929135131, 1.928577636452536319E-17, 0.03937007874015843040 ) ) ;
#10374 = CARTESIAN_POINT ( 'NONE',  ( 3.301370929368692659E-17, -1.802209163913756296, 0.1797182628040039365 ) ) ;
#10375 = AXIS2_PLACEMENT_3D ( 'NONE', #11828, #26451, #37448 ) ;
#10376 = CARTESIAN_POINT ( 'NONE',  ( 0.8759842519685039353, 0.1787899950787401882, 1.651082677111590513 ) ) ;
#10378 = CARTESIAN_POINT ( 'NONE',  ( -1.033464566929133799, 1.928577636452524610E-17, 2.869337061179095023E-17 ) ) ;
#10377 = FACE_OUTER_BOUND ( 'NONE', #26749, .T. ) ;
#10379 = CARTESIAN_POINT ( 'NONE',  ( 1.002407869896990045, -0.1264236179284866091, 0.5290354330171024300 ) ) ;
#10380 = AXIS2_PLACEMENT_3D ( 'NONE', #37456, #23326, #18767 ) ;
#10381 = AXIS2_PLACEMENT_3D ( 'NONE', #4782, #5027, #19408 ) ;
#10382 = VERTEX_POINT ( 'NONE', #46431 ) ;
#10383 = EDGE_LOOP ( 'NONE', ( #3908, #1884, #46345, #35752 ) ) ;
#10384 = CARTESIAN_POINT ( 'NONE',  ( 0.1951724573785894035, -0.1828112239219444324, -0.3083162604244762406 ) ) ;
#10385 = CARTESIAN_POINT ( 'NONE',  ( 3.284318927891251994E-17, -0.1924212597887563214, 0.1787899950787401882 ) ) ;
#10386 = CARTESIAN_POINT ( 'NONE',  ( 0.7495606340400177148, 0.1264236179284866091, 0.5487204723871811352 ) ) ;
#10387 = ADVANCED_FACE ( 'NONE', ( #13399 ), #46667, .F. ) ;
#10388 = CARTESIAN_POINT ( 'NONE',  ( 0.1264236179284866091, -1.009350393647023614, 0.1264236179284866091 ) ) ;
#10389 = CARTESIAN_POINT ( 'NONE',  ( 1.054774247047244540, 0.07405724077823318263, 0.02952755900135457801 ) ) ;
#10390 = CARTESIAN_POINT ( 'NONE',  ( -0.7185039370078739607, 1.928577636452523993E-17, 0.9251968502861732668 ) ) ;
#10391 = CARTESIAN_POINT ( 'NONE',  ( -0.6971942568897648851, 0.07405724077823318263, 1.574803149552536530 ) ) ;
#10392 = EDGE_LOOP ( 'NONE', ( #41113, #47055, #6073, #18093 ) ) ;
#10393 = CARTESIAN_POINT ( 'NONE',  ( -1.054774247047244540, 0.07405724077823318263, 1.092519684985605810 ) ) ;
#10394 = CARTESIAN_POINT ( 'NONE',  ( 0.8759842519685039353, -0.1574803149606299191, 0.1574803149606299191 ) ) ;
#10395 = CARTESIAN_POINT ( 'NONE',  ( 0.8019270111902717657, -0.1787899950787401604, 1.235236220418678199 ) ) ;
#10396 = ORIENTED_EDGE ( 'NONE', *, *, #40796, .T. ) ;
#10397 = CARTESIAN_POINT ( 'NONE',  ( -0.9412147342319837628, -0.1574803149606297803, 0.6619094487113696967 ) ) ;
#10398 = DIRECTION ( 'NONE',  ( -1.000000000000000000, -0.000000000000000000, -0.000000000000000000 ) ) ;
#10399 = CARTESIAN_POINT ( 'NONE',  ( 0.8019270111902717657, 0.1787899950787401604, 1.806102362150961316 ) ) ;
#10400 = CARTESIAN_POINT ( 'NONE',  ( -1.033464566929134687, 0.06523048226347956391, 0.6028543307086614567 ) ) ;
#10401 = CARTESIAN_POINT ( 'NONE',  ( -0.8019270111902717657, -0.1787899950787401604, 0.8366141731745828647 ) ) ;
#10402 = CARTESIAN_POINT ( 'NONE',  ( -0.8107537697050254399, -0.1574803149606297803, 1.611712598425196319 ) ) ;
#10403 = CARTESIAN_POINT ( 'NONE',  ( -0.7412252283027040978, -0.1004855783171688804, 0.03937007874015844427 ) ) ;
#10404 = CARTESIAN_POINT ( 'NONE',  ( 0.9500414927467377701, 0.1787899950787401604, 0.2706692912848194243 ) ) ;
#10405 = CARTESIAN_POINT ( 'NONE',  ( -0.9500414927467377701, -0.1787899950787401604, 0.1722440944344254543 ) ) ;
#10406 = CARTESIAN_POINT ( 'NONE',  ( -0.8759842519685039353, -0.1787899950787401882, 0.6028543306548976854 ) ) ;
#10407 = CARTESIAN_POINT ( 'NONE',  ( 1.033464566929133799, 0.000000000000000000, 1.614173228238929170 ) ) ;
#10408 = ORIENTED_EDGE ( 'NONE', *, *, #31937, .F. ) ;
#10409 = CARTESIAN_POINT ( 'NONE',  ( 0.07405724077823318263, 0.006889763833291078637, 0.1787899950787401604 ) ) ;
#10410 = LINE ( 'NONE', #6309, #7633 ) ;
#10411 = CARTESIAN_POINT ( 'NONE',  ( 0.9500414927467378812, 0.1787899950787401604, 0.7824803149068669805 ) ) ;
#10412 = CARTESIAN_POINT ( 'NONE',  ( -0.8019270111902716547, -0.1787899950787401604, 1.820866141678520789 ) ) ;
#10413 = VECTOR ( 'NONE', #26784, 39.37007874015748143 ) ;
#10414 = EDGE_CURVE ( 'NONE', #40492, #2870, #12602, .T. ) ;
#10415 = EDGE_CURVE ( 'NONE', #41713, #13286, #41853, .T. ) ;
#10416 = CARTESIAN_POINT ( 'NONE',  ( -0.8107537697050254399, 0.1574803149606300301, 0.6520669291338587747 ) ) ;
#10417 = CARTESIAN_POINT ( 'NONE',  ( 0.8107537697050254399, 0.1574803149606300301, 1.321358267716534751 ) ) ;
#10418 = CARTESIAN_POINT ( 'NONE',  ( 0.07405724077823318263, -1.367249952481208064, -0.1787899950787401604 ) ) ;
#10419 = VERTEX_POINT ( 'NONE', #11397 ) ;
#10420 = CARTESIAN_POINT ( 'NONE',  ( 0.07405724077823318263, -0.2244094487651340231, 0.1787899950787401604 ) ) ;
#10421 = AXIS2_PLACEMENT_3D ( 'NONE', #778, #15437, #2788 ) ;
#10422 = ORIENTED_EDGE ( 'NONE', *, *, #22465, .T. ) ;
#10423 = EDGE_CURVE ( 'NONE', #3332, #17493, #40356, .T. ) ;
#10424 = CARTESIAN_POINT ( 'NONE',  ( 0.2559055118110236116, 0.000000000000000000, -0.3149606299212598381 ) ) ;
#10425 = CARTESIAN_POINT ( 'NONE',  ( -0.7185039370078739607, 1.928577636452523993E-17, 1.003937007766488199 ) ) ;
#10426 = CARTESIAN_POINT ( 'NONE',  ( 0.7185039370078746268, 0.06523048226347956391, 1.916830708661418248 ) ) ;
#10427 = CARTESIAN_POINT ( 'NONE',  ( -0.07405724077823318263, -1.548228346402928723, -0.1787899950787401604 ) ) ;
#10428 = CARTESIAN_POINT ( 'NONE',  ( -0.1787899950787401604, -0.7952755904974174728, -0.07405724077823318263 ) ) ;
#10429 = CARTESIAN_POINT ( 'NONE',  ( -1.054774247047244540, 0.07405724077823318263, 0.5019685038832443214 ) ) ;
#10430 = CARTESIAN_POINT ( 'NONE',  ( -0.1270800023317771588, -1.305161919819265659, -0.1270800023317771588 ) ) ;
#10431 = CARTESIAN_POINT ( 'NONE',  ( -0.2460099227178286496, 0.1534603371579498221, -0.09996720075268322736 ) ) ;
#10432 = CARTESIAN_POINT ( 'NONE',  ( 0.9500414927467378812, -0.1787899950787401604, 1.200787401521039355 ) ) ;
#10433 = CARTESIAN_POINT ( 'NONE',  ( 1.054774247047244540, -0.07405724077823318263, 1.555118110182457158 ) ) ;
#10434 = CIRCLE ( 'NONE', #37206, 0.1574803149606299191 ) ;
#10436 = CARTESIAN_POINT ( 'NONE',  ( -0.7646288533564489232, -0.1113553986120547346, 1.097440944881889813 ) ) ;
#10435 = CARTESIAN_POINT ( 'NONE',  ( -1.033464566929133799, 1.928577636452524610E-17, 2.869337061179095023E-17 ) ) ;
#10437 = CARTESIAN_POINT ( 'NONE',  ( 1.033464566929133799, 0.000000000000000000, 0.6692913384751496553 ) ) ;
#10438 = CARTESIAN_POINT ( 'NONE',  ( -0.1574803149606300301, -0.7682086613097959260, -0.06523048226347956391 ) ) ;
#10439 = CARTESIAN_POINT ( 'NONE',  ( -0.8759842519685039353, -0.1574803149606299191, 1.761811023514519459 ) ) ;
#10440 = CARTESIAN_POINT ( 'NONE',  ( -0.1264236179284866091, 0.03395669296714932950, -0.1264236179284866091 ) ) ;
#10441 = CARTESIAN_POINT ( 'NONE',  ( 0.8019270111902717657, -0.1787899950787401604, 0.2066929133320631329 ) ) ;
#10442 = CARTESIAN_POINT ( 'NONE',  ( 0.7132454508862760001, -0.05294806947096847988, 0.03937007859770621371 ) ) ;
#10444 = CARTESIAN_POINT ( 'NONE',  ( 0.06801279071809869514, 0.3740157480314960647, 1.224299699984025658 ) ) ;
#10443 = CARTESIAN_POINT ( 'NONE',  ( 1.054774247047244096, 0.000000000000000000, 1.124507873961984261 ) ) ;
#10445 = CARTESIAN_POINT ( 'NONE',  ( -0.7185039370078739607, 1.928577636452523993E-17, 1.909448818790110192 ) ) ;
#10446 = CARTESIAN_POINT ( 'NONE',  ( 0.8107537697050253289, 0.1574803149606300301, 0.5241141731208195376 ) ) ;
#10447 = ORIENTED_EDGE ( 'NONE', *, *, #43269, .T. ) ;
#10448 = CARTESIAN_POINT ( 'NONE',  ( -0.02899999999999994943, 1.086379535891617509, -0.03715491745705647858 ) ) ;
#10449 = CARTESIAN_POINT ( 'NONE',  ( 0.8755199539507505513, 0.1745681463551092827, 0.03936728564635524202 ) ) ;
#10450 = CARTESIAN_POINT ( 'NONE',  ( -0.7646288533564489232, 0.1113553986120547346, 0.4084645668216063119 ) ) ;
#10451 = CARTESIAN_POINT ( 'NONE',  ( -0.8759842519685039353, -0.1574803149606299191, 1.535433070866141669 ) ) ;
#10452 = CARTESIAN_POINT ( 'NONE',  ( 0.9500414927467378812, 0.1787899950787401604, 1.525590551127340433 ) ) ;
#10454 = CARTESIAN_POINT ( 'NONE',  ( -0.08091701073424917290, 0.3740157480314960647, 1.112073044918590048 ) ) ;
#10453 = CYLINDRICAL_SURFACE ( 'NONE', #40226, 0.1624015748031507056 ) ;
#10455 = CARTESIAN_POINT ( 'NONE',  ( -0.1264236179284866091, -0.005413385773008149403, -0.1264236179284866091 ) ) ;
#10456 = VERTEX_POINT ( 'NONE', #22399 ) ;
#10457 = DIRECTION ( 'NONE',  ( 1.000000000000000000, 1.751623080406019977E-46, -7.049916206369740876E-15 ) ) ;
#10458 = ( BOUNDED_CURVE ( )  B_SPLINE_CURVE ( 2, ( #32746, #26013, #7783, #25554, #22398, #33228, #37027, #26261, #108 ),
 .UNSPECIFIED., .F., .T. ) 
 B_SPLINE_CURVE_WITH_KNOTS ( ( 3, 2, 2, 2, 3 ),
 ( 0.8399999999999999689, 0.8425000000000000266, 0.8449999999999999734, 0.8475000000000000311, 0.8499999999999999778 ),
 .UNSPECIFIED. ) 
 CURVE ( )  GEOMETRIC_REPRESENTATION_ITEM ( )  RATIONAL_B_SPLINE_CURVE ( ( 1.000000000000000000, 0.9238795325112869605, 1.000000000000000000, 0.9238795325112869605, 1.000000000000000000, 0.9238795325112869605, 1.000000000000000000, 0.9238795325112869605, 1.000000000000000000 ) ) 
 REPRESENTATION_ITEM ( '' )  ) ;
#10459 = VERTEX_POINT ( 'NONE', #23593 ) ;
#10460 = CARTESIAN_POINT ( 'NONE',  ( 0.3690944881889771101, 0.1864803149606328037, -0.7480314960629921295 ) ) ;
#10461 = DIRECTION ( 'NONE',  ( -1.000000000000000000, 0.000000000000000000, 0.000000000000000000 ) ) ;
#10462 = CARTESIAN_POINT ( 'NONE',  ( 0.8019270111902717657, -0.1787899950787401604, 0.5659448818360001132 ) ) ;
#10463 = B_SPLINE_CURVE_WITH_KNOTS ( 'NONE', 3,
 ( #26318, #44247, #40874, #37796, #15055 ),
 .UNSPECIFIED., .F., .F.,
 ( 4, 1, 4 ),
 ( 0.000000000000000000, 0.002020725942163689639, 0.004041451884327384482 ),
 .UNSPECIFIED. ) ;
#10464 = EDGE_CURVE ( 'NONE', #1535, #15970, #17458, .T. ) ;
#10465 = ORIENTED_EDGE ( 'NONE', *, *, #39731, .F. ) ;
#10466 = CARTESIAN_POINT ( 'NONE',  ( -0.6971942568897648851, -0.07405724077823297447, 1.382874015694267822 ) ) ;
#10467 = CARTESIAN_POINT ( 'NONE',  ( -0.1264236179284866091, -1.781988188922614347, -0.1264236179284866091 ) ) ;
#10468 = CARTESIAN_POINT ( 'NONE',  ( -1.002407869896990045, 0.1264236179284866091, 1.094980314906866203 ) ) ;
#10469 = CARTESIAN_POINT ( 'NONE',  ( -0.7185039370078746268, -0.06523048226347956391, 0.1107283464566929249 ) ) ;
#10470 = ORIENTED_EDGE ( 'NONE', *, *, #20770, .T. ) ;
#10471 = CARTESIAN_POINT ( 'NONE',  ( -0.8019270111902716547, -0.1787899950787401604, 1.151574803095843036 ) ) ;
#10472 = CARTESIAN_POINT ( 'NONE',  ( -0.9500414927467378812, 0.1787899950787401604, 0.8218503936470251681 ) ) ;
#10473 = EDGE_CURVE ( 'NONE', #8877, #35682, #45293, .T. ) ;
#10474 = CARTESIAN_POINT ( 'NONE',  ( -0.9500414927467378812, 0.1787899950787401604, 0.2312992125446618197 ) ) ;
#10475 = CYLINDRICAL_SURFACE ( 'NONE', #40456, 0.1574803149606299191 ) ;
#10476 = CARTESIAN_POINT ( 'NONE',  ( 0.1787899950787401604, -0.7865412910638841515, 0.07405724077823318263 ) ) ;
#10477 = ORIENTED_EDGE ( 'NONE', *, *, #35036, .F. ) ;
#10478 = FACE_OUTER_BOUND ( 'NONE', #8990, .T. ) ;
#10479 = ORIENTED_EDGE ( 'NONE', *, *, #6205, .T. ) ;
#10480 = ORIENTED_EDGE ( 'NONE', *, *, #19100, .F. ) ;
#10481 = EDGE_CURVE ( 'NONE', #11244, #19795, #4654, .T. ) ;
#10482 = DIRECTION ( 'NONE',  ( -1.000000000000000000, 0.000000000000000000, 0.000000000000000000 ) ) ;
#10483 = ( BOUNDED_CURVE ( )  B_SPLINE_CURVE ( 2, ( #15749, #12145, #18605, #610, #19316, #44930, #15508, #8288, #1092 ),
 .UNSPECIFIED., .F., .T. ) 
 B_SPLINE_CURVE_WITH_KNOTS ( ( 3, 2, 2, 2, 3 ),
 ( 0.2200000000000000011, 0.2225000000000000033, 0.2250000000000000056, 0.2275000000000000078, 0.2300000000000000100 ),
 .UNSPECIFIED. ) 
 CURVE ( )  GEOMETRIC_REPRESENTATION_ITEM ( )  RATIONAL_B_SPLINE_CURVE ( ( 1.000000000000000000, 0.9238795325112869605, 1.000000000000000000, 0.9238795325112869605, 1.000000000000000000, 0.9238795325112869605, 1.000000000000000000, 0.9238795325112869605, 1.000000000000000000 ) ) 
 REPRESENTATION_ITEM ( '' )  ) ;
#10484 = CARTESIAN_POINT ( 'NONE',  ( -1.002407869896990045, -0.1264236179284866091, 0.6471456692375747721 ) ) ;
#10485 = ORIENTED_EDGE ( 'NONE', *, *, #23784, .F. ) ;
#10486 = CARTESIAN_POINT ( 'NONE',  ( -1.054774247047244096, 0.000000000000000000, 1.798720472387181024 ) ) ;
#10487 = CYLINDRICAL_SURFACE ( 'NONE', #25712, 0.07874015748031489015 ) ;
#10488 = CARTESIAN_POINT ( 'NONE',  ( -0.8759842519685039353, 0.1787899950787401882, 0.1156496062454492185 ) ) ;
#10489 = ORIENTED_EDGE ( 'NONE', *, *, #9370, .T. ) ;
#10490 = CARTESIAN_POINT ( 'NONE',  ( 0.7185039370078746268, -0.06523048226347956391, 0.6619094488188971281 ) ) ;
#10491 = CARTESIAN_POINT ( 'NONE',  ( 0.1797182628040039087, -0.8056540458035184038, -0.07444174185955065859 ) ) ;
#10492 = CARTESIAN_POINT ( 'NONE',  ( -1.033464566929134687, 0.06523048226347956391, 0.9571850393700783721 ) ) ;
#10493 = CARTESIAN_POINT ( 'NONE',  ( -0.8107537697050253289, -0.1574803149606297803, 1.444389763672000671 ) ) ;
#10494 = CARTESIAN_POINT ( 'NONE',  ( 1.002407869896990045, -0.1264236179284866091, 0.7308070865604093802 ) ) ;
#10495 = CARTESIAN_POINT ( 'NONE',  ( -0.1113553986120547346, -0.5836614173228346081, -0.1113553986120547346 ) ) ;
#10496 = CARTESIAN_POINT ( 'NONE',  ( -0.1527835536277865613, 0.1279265601668728991, 0.06534438871128525617 ) ) ;
#10497 = VERTEX_POINT ( 'NONE', #22650 ) ;
#10498 = CARTESIAN_POINT ( 'NONE',  ( 0.7185039370078739607, 1.928577636452523993E-17, 0.1771653542231816925 ) ) ;
#10499 = CARTESIAN_POINT ( 'NONE',  ( 0.9412147342319837628, -0.1574803149606297803, 1.183562992125983593 ) ) ;
#10501 = DIRECTION ( 'NONE',  ( 1.217491584052838080E-15, 0.6156614753256588468, 0.7880107536067214591 ) ) ;
#10500 = CARTESIAN_POINT ( 'NONE',  ( 0.8478354771968141801, -0.1713848073773632519, 1.987689202509897557 ) ) ;
#10502 = CARTESIAN_POINT ( 'NONE',  ( -0.6195511811023656223, 0.1864803149606299171, -1.186023622047243986 ) ) ;
#10503 = CIRCLE ( 'NONE', #25025, 0.08090551181102362266 ) ;
#10505 = DIRECTION ( 'NONE',  ( -1.000000000000000000, -0.000000000000000000, -0.000000000000000000 ) ) ;
#10504 = CARTESIAN_POINT ( 'NONE',  ( 0.8759842519685039353, 0.1787899950787401882, 0.7012795275052913224 ) ) ;
#10506 = CARTESIAN_POINT ( 'NONE',  ( -0.1787899950787401882, -0.6697834645131652831, 0.000000000000000000 ) ) ;
#10507 = CARTESIAN_POINT ( 'NONE',  ( 0.7185039370078739607, 1.928577636452523993E-17, 1.564960629921259949 ) ) ;
#10508 = CARTESIAN_POINT ( 'NONE',  ( 0.1637019648159556695, 0.08049521775124826584, 0.1394218183822737434 ) ) ;
#10509 = CARTESIAN_POINT ( 'NONE',  ( 0.8107537697050253289, -0.1574803149606297803, 1.729822834645670548 ) ) ;
#10510 = CARTESIAN_POINT ( 'NONE',  ( 1.033464566929133799, 0.000000000000000000, 0.7185039370078739607 ) ) ;
#10511 = CARTESIAN_POINT ( 'NONE',  ( 0.8019270111902717657, 0.1787899950787401604, 1.018700787347811110 ) ) ;
#10512 = EDGE_CURVE ( 'NONE', #40086, #45750, #44935, .T. ) ;
#10513 = CYLINDRICAL_SURFACE ( 'NONE', #36435, 0.1003937007874010356 ) ;
#10514 = CARTESIAN_POINT ( 'NONE',  ( 0.07444174185955065859, 0.05064516679490722179, 0.1797182628040039087 ) ) ;
#10515 = CARTESIAN_POINT ( 'NONE',  ( 0.07405724077823318263, -1.174212598371433769, 0.1787899950787401604 ) ) ;
#10516 = CARTESIAN_POINT ( 'NONE',  ( 0.1574803149606300301, -1.545767716535432879, 0.06523048226347956391 ) ) ;
#10517 = CARTESIAN_POINT ( 'NONE',  ( 0.7646288533564489232, 0.1113553986120547346, 1.245078740157480324 ) ) ;
#10518 = ORIENTED_EDGE ( 'NONE', *, *, #47008, .T. ) ;
#10519 = CARTESIAN_POINT ( 'NONE',  ( -1.054774247047244540, -0.07405724077823318263, 0.09842519679663024046 ) ) ;
#10520 = EDGE_CURVE ( 'NONE', #2780, #43175, #39143, .T. ) ;
#10521 = CARTESIAN_POINT ( 'NONE',  ( 1.002407869896990045, -0.1264236179284866091, 1.951279527505291433 ) ) ;
#10522 = ORIENTED_EDGE ( 'NONE', *, *, #44505, .T. ) ;
#10523 = CARTESIAN_POINT ( 'NONE',  ( -0.9500414927467377701, 0.1787899950787401604, 1.884842519631275026 ) ) ;
#10524 = CARTESIAN_POINT ( 'NONE',  ( -0.8019270111902717657, 0.1787899950787401604, 1.648622047190331230 ) ) ;
#10525 = CARTESIAN_POINT ( 'NONE',  ( 0.6971942568897648851, -0.07405724077823297447, 0.8366141731745828647 ) ) ;
#10526 = CARTESIAN_POINT ( 'NONE',  ( -1.002407869896990045, 0.1264236179284866091, 0.8144685038832440993 ) ) ;
#10527 = CARTESIAN_POINT ( 'NONE',  ( -0.8759842519685039353, -0.1787899950787401882, 1.114665354276944909 ) ) ;
#10528 = CARTESIAN_POINT ( 'NONE',  ( -0.8019270111902717657, -0.1787899950787401604, 0.4084645668753704717 ) ) ;
#10529 = CARTESIAN_POINT ( 'NONE',  ( -0.8107537697050254399, -0.1574803149606297803, 1.798720472333418918 ) ) ;
#10530 = CARTESIAN_POINT ( 'NONE',  ( -1.054774247047244540, -0.07405724077823318263, 1.874999999946236784 ) ) ;
#10531 = CARTESIAN_POINT ( 'NONE',  ( 0.08774906724789779955, -0.09246610911303654312, -0.2347711071351356593 ) ) ;
#10532 = CARTESIAN_POINT ( 'NONE',  ( -0.8107537697050253289, -0.1574803149606297803, 1.966043307086614567 ) ) ;
#10533 = CARTESIAN_POINT ( 'NONE',  ( -0.8107537697050254399, -0.1574803149606297803, 1.887303149606298414 ) ) ;
#10534 = CARTESIAN_POINT ( 'NONE',  ( 0.1264236179284866091, -0.3953011335835693307, 0.1264236179284866091 ) ) ;
#10535 = CONTEXT_DEPENDENT_SHAPE_REPRESENTATION ( #47435, #22643 ) ;
#10536 = CARTESIAN_POINT ( 'NONE',  ( -0.1377952755905510751, 1.687505431895957647E-17, -0.3149606299212598381 ) ) ;
#10537 = CARTESIAN_POINT ( 'NONE',  ( 0.7646288533564489232, -0.1113553986120547346, 1.048228346349165507 ) ) ;
#10538 = CONICAL_SURFACE ( 'NONE', #8984, 0.08090551181102362266, 0.9599310885968742602 ) ;
#10539 = CARTESIAN_POINT ( 'NONE',  ( -0.6971942568897637749, 2.189545951927499583E-17, 0.08120078734781142893 ) ) ;
#10540 = EDGE_LOOP ( 'NONE', ( #5002, #23357 ) ) ;
#10541 = CARTESIAN_POINT ( 'NONE',  ( -0.6971942568897637749, 2.189545951927499583E-17, 1.345964566875370139 ) ) ;
#10542 = ORIENTED_EDGE ( 'NONE', *, *, #6270, .T. ) ;
#10543 = CARTESIAN_POINT ( 'NONE',  ( 0.1264236179284866091, -1.240649606245448622, -0.1264236179284866091 ) ) ;
#10544 = CARTESIAN_POINT ( 'NONE',  ( -0.1264236179284866091, -1.304625984198204636, -0.1264236179284866091 ) ) ;
#10545 = CARTESIAN_POINT ( 'NONE',  ( -0.7185039370078714072, 0.06523048226347728795, 1.552657480207434659 ) ) ;
#10546 = ( NAMED_UNIT ( * ) SI_UNIT ( $, .STERADIAN. ) SOLID_ANGLE_UNIT ( ) ) ;
#10547 = CARTESIAN_POINT ( 'NONE',  ( 0.7185039370078746268, 0.06523048226347956391, 0.3813976377952755237 ) ) ;
#10548 = DIRECTION ( 'NONE',  ( 0.000000000000000000, 0.000000000000000000, 1.000000000000000000 ) ) ;
#10549 = CARTESIAN_POINT ( 'NONE',  ( -1.033464566929134687, 0.06523048226347956391, 0.9473425195775121432 ) ) ;
#10550 = CARTESIAN_POINT ( 'NONE',  ( -0.9412147342319837628, -0.1574803149606297803, 0.7898622047244097111 ) ) ;
#10551 = CARTESIAN_POINT ( 'NONE',  ( 1.054774247047244540, 0.07405724077823318263, 0.3838582676627718127 ) ) ;
#10552 = CARTESIAN_POINT ( 'NONE',  ( -0.1574803149606297803, -0.1038385826771653780, 0.06523048226347956391 ) ) ;
#10553 = CARTESIAN_POINT ( 'NONE',  ( 0.8759842519685039353, -0.1574803149606299191, 1.879921259734992134 ) ) ;
#10554 = VERTEX_POINT ( 'NONE', #37740 ) ;
#10555 = CARTESIAN_POINT ( 'NONE',  ( -0.8107537697050254399, 0.1574803149606300301, 1.429625984144440531 ) ) ;
#10556 = CARTESIAN_POINT ( 'NONE',  ( 0.8107537697050253289, -0.1574803149606297803, 0.8636811023622045225 ) ) ;
#10557 = CARTESIAN_POINT ( 'NONE',  ( 0.09118578515492269110, -0.2428480946569469834, -0.03489849683095880284 ) ) ;
#10558 = LINE ( 'NONE', #25157, #23309 ) ;
#10559 = VECTOR ( 'NONE', #43712, 39.37007874015748143 ) ;
#10561 = CARTESIAN_POINT ( 'NONE',  ( 0.8107537697050254399, 0.1574803149606300301, 1.518208661417322913 ) ) ;
#10560 = DIRECTION ( 'NONE',  ( 0.000000000000000000, 0.2126700594527842492, -0.9771240687918547607 ) ) ;
#10562 = CARTESIAN_POINT ( 'NONE',  ( 0.7646288533564489232, -0.1113553986120547346, 0.2608267715460165226 ) ) ;
#10563 = CARTESIAN_POINT ( 'NONE',  ( -0.1264236179284866091, -0.03494094482812625663, 0.1264236179284866091 ) ) ;
#10564 = EDGE_CURVE ( 'NONE', #10722, #27975, #38096, .T. ) ;
#10565 = ORIENTED_EDGE ( 'NONE', *, *, #37045, .T. ) ;
#10566 = DIRECTION ( 'NONE',  ( -0.000000000000000000, 1.000000000000000000, -0.000000000000000000 ) ) ;
#10567 = CARTESIAN_POINT ( 'NONE',  ( 0.1574803149606300301, -1.496555118002708795, 0.06523048226347956391 ) ) ;
#10568 = CARTESIAN_POINT ( 'NONE',  ( -0.1787899950787401604, -0.5984251967966303098, -0.07405724077823318263 ) ) ;
#10570 = AXIS2_PLACEMENT_3D ( 'NONE', #939, #4522, #33578 ) ;
#10569 = CARTESIAN_POINT ( 'NONE',  ( 0.1113553986120547346, -1.036417322834645827, 0.1113553986120547346 ) ) ;
#10571 = CARTESIAN_POINT ( 'NONE',  ( 0.8759842519685039353, 0.1574803149606299191, 0.9153543306011338032 ) ) ;
#10572 = EDGE_CURVE ( 'NONE', #46402, #43921, #23530, .T. ) ;
#10573 = CARTESIAN_POINT ( 'NONE',  ( -0.1586641775163213364, 1.914733266569311532, -0.6843357808987579061 ) ) ;
#10574 = CARTESIAN_POINT ( 'NONE',  ( -0.6971942568897626646, 0.07405724077823318263, 0.3937007873478115538 ) ) ;
#10575 = ORIENTED_EDGE ( 'NONE', *, *, #20495, .T. ) ;
#10576 = ORIENTED_EDGE ( 'NONE', *, *, #46842, .F. ) ;
#10577 = ORIENTED_EDGE ( 'NONE', *, *, #42871, .T. ) ;
#10578 = CARTESIAN_POINT ( 'NONE',  ( -0.6971942568897648851, 0.07405724077823318263, 1.658464566875369472 ) ) ;
#10579 = EDGE_LOOP ( 'NONE', ( #8735, #5384, #25391, #35500, #31388, #43849, #20696 ) ) ;
#10580 = EDGE_CURVE ( 'NONE', #3855, #8749, #44902, .T. ) ;
#10581 = CARTESIAN_POINT ( 'NONE',  ( 0.7495606340400177148, 0.1264236179284866091, 1.577263779473795369 ) ) ;
#10582 = VERTEX_POINT ( 'NONE', #41292 ) ;
#10583 = CARTESIAN_POINT ( 'NONE',  ( -0.8019270111902717657, -0.1787899950787401604, 0.7627952755367881643 ) ) ;
#10584 = EDGE_CURVE ( 'NONE', #1283, #31809, #22351, .T. ) ;
#10585 = CARTESIAN_POINT ( 'NONE',  ( -0.8070866141732283561, -0.3937007874015746034, 0.7574803149606299524 ) ) ;
#10586 = CARTESIAN_POINT ( 'NONE',  ( 0.9500414927467377701, 0.1787899950787401604, 0.7824803149068668695 ) ) ;
#10587 = CARTESIAN_POINT ( 'NONE',  ( -0.6971942568897648851, -0.07405724077823297447, 0.7135826771115916234 ) ) ;
#10588 = CYLINDRICAL_SURFACE ( 'NONE', #24608, 0.1574803149606299191 ) ;
#10589 = CYLINDRICAL_SURFACE ( 'NONE', #29892, 0.1574803149606299191 ) ;
#10590 = CARTESIAN_POINT ( 'NONE',  ( -0.1574803149606297803, -0.2121062991050713942, 0.06523048226347956391 ) ) ;
#10591 = CARTESIAN_POINT ( 'NONE',  ( -1.002407869896990045, -0.1264236179284866091, 1.360728346402929168 ) ) ;
#10592 = CARTESIAN_POINT ( 'NONE',  ( -0.8759842519685039353, 0.1574803149606299191, 1.476377952755905554 ) ) ;
#10593 = CARTESIAN_POINT ( 'NONE',  ( -0.7646288533564489232, 0.1113553986120547346, 0.4576771653543307283 ) ) ;
#10594 = CARTESIAN_POINT ( 'NONE',  ( 0.8759842519685039353, 0.1787899950787401882, 1.454232283410803017 ) ) ;
#10595 = CARTESIAN_POINT ( 'NONE',  ( -0.02491398756834440828, -0.09851384158024625859, -0.1871469785078783421 ) ) ;
#10596 = CARTESIAN_POINT ( 'NONE',  ( -1.033464566929133799, 0.000000000000000000, 0.3149606298137326843 ) ) ;
#10597 = ORIENTED_EDGE ( 'NONE', *, *, #26040, .F. ) ;
#10598 = AXIS2_PLACEMENT_3D ( 'NONE', #30908, #45951, #12925 ) ;
#10599 = CARTESIAN_POINT ( 'NONE',  ( -1.094772975963752103E-17, -1.679749952481206954, -0.1787899950787401882 ) ) ;
#10600 = VERTEX_POINT ( 'NONE', #24576 ) ;
#10601 = CARTESIAN_POINT ( 'NONE',  ( 0.9873396505805591694, 0.1113553986120547346, 0.4872047244094488416 ) ) ;
#10602 = ORIENTED_EDGE ( 'NONE', *, *, #33847, .F. ) ;
#10603 = CARTESIAN_POINT ( 'NONE',  ( 0.2944196465027555387, -3.032960542342102697E-32, 0.09842519685039370636 ) ) ;
#10604 = AXIS2_PLACEMENT_3D ( 'NONE', #12008, #16314, #12490 ) ;
#10605 = CARTESIAN_POINT ( 'NONE',  ( -0.1787899950787401882, -0.9847440944344251212, 0.000000000000000000 ) ) ;
#10606 = DIRECTION ( 'NONE',  ( 1.822029033848725028E-16, 0.000000000000000000, 1.000000000000000000 ) ) ;
#10607 = CARTESIAN_POINT ( 'NONE',  ( 1.054774247047244096, 0.000000000000000000, 0.3371062991588349989 ) ) ;
#10608 = CARTESIAN_POINT ( 'NONE',  ( -0.1787899950787401604, -0.1369349918512859643, -0.07405724077823318263 ) ) ;
#10609 = CARTESIAN_POINT ( 'NONE',  ( 0.1264236179284866091, 0.009350393754550925460, 0.1264236179284866091 ) ) ;
#10610 = CONTEXT_DEPENDENT_SHAPE_REPRESENTATION ( #18656, #11543 ) ;
#10611 = PLANE ( 'NONE',  #19599 ) ;
#10612 = CARTESIAN_POINT ( 'NONE',  ( 0.9500414927467378812, 0.1787899950787401604, 0.5807086613635594752 ) ) ;
#10613 = CARTESIAN_POINT ( 'NONE',  ( -1.002407869896990045, -0.1264236179284866091, 0.8882874015210394658 ) ) ;
#10615 = LINE ( 'NONE', #2909, #36919 ) ;
#10614 = CARTESIAN_POINT ( 'NONE',  ( 0.4142125984251969206, 3.008340040661385896E-17, 0.000000000000000000 ) ) ;
#10616 = CARTESIAN_POINT ( 'NONE',  ( -0.1797182628040039365, -1.733311526118478385, 0.000000000000000000 ) ) ;
#10617 = CARTESIAN_POINT ( 'NONE',  ( 0.7646288533564489232, -0.1113553986120547346, 1.687992125984252079 ) ) ;
#10618 = CARTESIAN_POINT ( 'NONE',  ( 0.8019270111902717657, -0.1787899950787401604, 1.707677165300566235 ) ) ;
#10619 = CARTESIAN_POINT ( 'NONE',  ( -0.1478661631957976508, -0.09575019180979005284, 0.2000608872904859059 ) ) ;
#10620 = EDGE_LOOP ( 'NONE', ( #3058, #29074, #26688, #21328 ) ) ;
#10621 = CARTESIAN_POINT ( 'NONE',  ( 0.7185039370078746268, 0.06523048226347956391, 0.02706692913385832025 ) ) ;
#10622 = DIRECTION ( 'NONE',  ( 0.000000000000000000, 0.000000000000000000, 1.000000000000000000 ) ) ;
#10623 = DIRECTION ( 'NONE',  ( -1.000000000000000000, 0.000000000000000000, 0.000000000000000000 ) ) ;
#10624 = CARTESIAN_POINT ( 'NONE',  ( 0.1787899950787401604, -0.1407480314422995815, -0.07405724077823318263 ) ) ;
#10625 = CARTESIAN_POINT ( 'NONE',  ( 0.7495606340400177148, -0.1264236179284866091, 0.5585629920722204877 ) ) ;
#10626 = CARTESIAN_POINT ( 'NONE',  ( 3.284318927891251994E-17, -1.053641732229700700, 0.1787899950787401882 ) ) ;
#10627 = CARTESIAN_POINT ( 'NONE',  ( 1.054774247047244096, 0.000000000000000000, 0.1058070865604096300 ) ) ;
#10628 = EDGE_CURVE ( 'NONE', #13680, #25085, #6110, .T. ) ;
#10629 = CARTESIAN_POINT ( 'NONE',  ( 0.6971942568897648851, 0.07405724077823318263, 0.5905511810485987167 ) ) ;
#10630 = CARTESIAN_POINT ( 'NONE',  ( -1.002407869896990045, 0.1264236179284866091, 1.601870078686393750 ) ) ;
#10631 = VERTEX_POINT ( 'NONE', #9965 ) ;
#10632 = CARTESIAN_POINT ( 'NONE',  ( 0.8759842519685039353, -0.1787899950787401882, 1.158956692859621995 ) ) ;
#10633 = ORIENTED_EDGE ( 'NONE', *, *, #30492, .F. ) ;
#10634 = CARTESIAN_POINT ( 'NONE',  ( -0.9412147342319837628, 0.1574803149606300301, 0.7160433069790875793 ) ) ;
#10635 = LINE ( 'NONE', #39827, #23210 ) ;
#10636 = CARTESIAN_POINT ( 'NONE',  ( 0.8019270111902717657, 0.1787899950787401604, 1.884842519631275026 ) ) ;
#10637 = CARTESIAN_POINT ( 'NONE',  ( -0.8107537697050253289, 0.1574803149606300301, 0.6126968503937006982 ) ) ;
#10638 = CARTESIAN_POINT ( 'NONE',  ( -0.7495606340400177148, 0.1264236179284866091, 0.9424212597887559051 ) ) ;
#10639 = ADVANCED_FACE ( 'NONE', ( #35374 ), #17144, .T. ) ;
#10640 = CARTESIAN_POINT ( 'NONE',  ( 0.6971942568897626646, 0.07405724077823318263, 0.2411417322297010890 ) ) ;
#10641 = CARTESIAN_POINT ( 'NONE',  ( -0.7495606340400177148, -0.1264236179284866091, 0.2436023621509610382 ) ) ;
#10642 = CARTESIAN_POINT ( 'NONE',  ( -0.8759842519685039353, -0.1787899950787401882, 0.7603346456155274380 ) ) ;
#10643 = CARTESIAN_POINT ( 'NONE',  ( 0.8107537697050253289, 0.1574803149606300301, 1.626476377845228694 ) ) ;
#10644 = ORIENTED_EDGE ( 'NONE', *, *, #4803, .F. ) ;
#10645 = CARTESIAN_POINT ( 'NONE',  ( 0.1787899950787401604, -0.02263779522182706588, -0.07405724077823318263 ) ) ;
#10646 = ORIENTED_EDGE ( 'NONE', *, *, #17959, .F. ) ;
#10647 = CARTESIAN_POINT ( 'NONE',  ( 0.8019270111902717657, 0.1787899950787401604, 0.7874015747493863238 ) ) ;
#10648 = CARTESIAN_POINT ( 'NONE',  ( 1.054774247047244540, -0.07405724077823318263, 1.008858267662772423 ) ) ;
#10649 = CARTESIAN_POINT ( 'NONE',  ( -0.8019270111902716547, 0.1787899950787401604, 1.924212598371433325 ) ) ;
#10650 = CARTESIAN_POINT ( 'NONE',  ( 0.6971942568897648851, 0.07405724077823318263, 1.929133858213952335 ) ) ;
#10651 = CARTESIAN_POINT ( 'NONE',  ( 0.1574803149606299746, 0.9876813667277571929, 0.7893767492247212303 ) ) ;
#10652 = CARTESIAN_POINT ( 'NONE',  ( -0.1787899950787401604, -1.278667275315853002, -0.07405724077823318263 ) ) ;
#10653 = ORIENTED_EDGE ( 'NONE', *, *, #1913, .F. ) ;
#10654 = CARTESIAN_POINT ( 'NONE',  ( -0.1264236179284866091, -0.2022637794737956740, -0.1264236179284866091 ) ) ;
#10655 = ORIENTED_EDGE ( 'NONE', *, *, #33529, .T. ) ;
#10656 = CARTESIAN_POINT ( 'NONE',  ( 0.9500414927467378812, 0.1787899950787401604, 1.053149606245450176 ) ) ;
#10657 = DIRECTION ( 'NONE',  ( -1.000000000000000000, 3.469446951953614189E-15, 0.000000000000000000 ) ) ;
#10658 = EDGE_CURVE ( 'NONE', #41311, #14850, #32012, .T. ) ;
#10659 = CARTESIAN_POINT ( 'NONE',  ( -0.8107537697050254399, 0.1574803149606300301, 0.9965551180027086842 ) ) ;
#10660 = CIRCLE ( 'NONE', #23649, 0.09842519685039317900 ) ;
#10661 = CARTESIAN_POINT ( 'NONE',  ( 0.6971942568897626646, 0.07405724077823318263, 0.03937007868639404856 ) ) ;
#10662 = AXIS2_PLACEMENT_3D ( 'NONE', #34606, #6049, #41506 ) ;
#10663 = CARTESIAN_POINT ( 'NONE',  ( 0.07405724077823318263, -1.592519684985606254, -0.1787899950787401604 ) ) ;
#10664 = CARTESIAN_POINT ( 'NONE',  ( -0.1787899950787401882, -0.7140748030958424808, 0.000000000000000000 ) ) ;
#10665 = AXIS2_PLACEMENT_3D ( 'NONE', #20000, #45152, #12369 ) ;
#10666 = CARTESIAN_POINT ( 'NONE',  ( -0.9500414927467377701, -0.1787899950787401604, 0.4527559054580477249 ) ) ;
#10667 = CARTESIAN_POINT ( 'NONE',  ( 0.3980944881889786346, 0.6449983665207558170, -0.06082000038405668829 ) ) ;
#10668 = CARTESIAN_POINT ( 'NONE',  ( -0.7109468291419211994, -0.02418920431224856268, 1.983709381215293721 ) ) ;
#10669 = DIRECTION ( 'NONE',  ( -0.000000000000000000, 0.000000000000000000, -1.000000000000000000 ) ) ;
#10670 = CARTESIAN_POINT ( 'NONE',  ( 0.6971942568897637749, 2.189545951927499583E-17, 1.227854330654897685 ) ) ;
#10671 = AXIS2_PLACEMENT_3D ( 'NONE', #20154, #9857, #24467 ) ;
#10672 = CARTESIAN_POINT ( 'NONE',  ( 0.7495606340400177148, 0.1264236179284866091, 1.572342519631275692 ) ) ;
#10673 = DIRECTION ( 'NONE',  ( 0.000000000000000000, 0.000000000000000000, 1.000000000000000000 ) ) ;
#10674 = CARTESIAN_POINT ( 'NONE',  ( -0.1026092249587055166, 0.1299212598425196763, 0.1321676130798911386 ) ) ;
#10675 = CARTESIAN_POINT ( 'NONE',  ( 1.614954907737318939E-16, 0.1564960629921311464, 0.3937007874015748254 ) ) ;
#10676 = CARTESIAN_POINT ( 'NONE',  ( -0.1476377952755905387, 0.3743908788525359133, -3.616772362661642592 ) ) ;
#10677 = CARTESIAN_POINT ( 'NONE',  ( 0.1574803149606299191, -0.7854330707586142379, -1.928577636452523993E-17 ) ) ;
#10678 = CARTESIAN_POINT ( 'NONE',  ( -0.8107537697050253289, -0.1574803149606297803, 1.759350393593260842 ) ) ;
#10679 = CARTESIAN_POINT ( 'NONE',  ( 0.7495606340400177148, -0.1264236179284866091, 0.1254921259304885850 ) ) ;
#10680 = CARTESIAN_POINT ( 'NONE',  ( 0.7013878823978492161, 0.0007829370750213354322, 0.03936334417628854776 ) ) ;
#10681 = EDGE_CURVE ( 'NONE', #20094, #24250, #43403, .T. ) ;
#10683 = CARTESIAN_POINT ( 'NONE',  ( 0.8759842519685039353, 0.000000000000000000, 4.498031496062992574 ) ) ;
#10682 = CARTESIAN_POINT ( 'NONE',  ( 0.8019270111902716547, -0.1787899950787401604, 1.151574803095843036 ) ) ;
#10684 = CARTESIAN_POINT ( 'NONE',  ( 0.7185039370078746268, -0.06523048226347956391, 1.213090551181103427 ) ) ;
#10685 = CARTESIAN_POINT ( 'NONE',  ( -0.8759842519685039353, 0.1787899950787401882, 1.252460629867496067 ) ) ;
#10686 = CARTESIAN_POINT ( 'NONE',  ( 0.8107537697050253289, 0.1574803149606300301, 0.4847440943806614055 ) ) ;
#10687 = ORIENTED_EDGE ( 'NONE', *, *, #7218, .T. ) ;
#10688 = DIRECTION ( 'NONE',  ( 1.000000000000000000, -0.000000000000000000, -0.000000000000000000 ) ) ;
#10689 = CARTESIAN_POINT ( 'NONE',  ( 0.8898084847641706263, 0.1731449922679708653, 0.03937008185983620345 ) ) ;
#10690 = VERTEX_POINT ( 'NONE', #2982 ) ;
#10691 = CARTESIAN_POINT ( 'NONE',  ( -0.7646288533564489232, 0.1113553986120547346, 0.3690944880814492901 ) ) ;
#10692 = EDGE_LOOP ( 'NONE', ( #2925, #17829, #35491, #8429, #28059 ) ) ;
#10693 = CARTESIAN_POINT ( 'NONE',  ( 1.054774247047244540, 0.07405724077823318263, 1.402559055064346971 ) ) ;
#10694 = EDGE_CURVE ( 'NONE', #5036, #9764, #29693, .T. ) ;
#10695 = CARTESIAN_POINT ( 'NONE',  ( -1.033464566929133799, 1.928577636452524610E-17, 2.869337061179095023E-17 ) ) ;
#10697 = CARTESIAN_POINT ( 'NONE',  ( 0.7646288533564489232, 0.1113553986120547346, 1.914370078740157632 ) ) ;
#10696 = DIRECTION ( 'NONE',  ( 1.000000000000000000, 0.000000000000000000, 0.000000000000000000 ) ) ;
#10698 = CARTESIAN_POINT ( 'NONE',  ( 0.1264236179284866091, -0.05462598419820496182, -0.1264236179284866091 ) ) ;
#10699 = ORIENTED_EDGE ( 'NONE', *, *, #27847, .T. ) ;
#10700 = CARTESIAN_POINT ( 'NONE',  ( 0.7185039370078739607, 1.928577636452523993E-17, 1.318897637687747926 ) ) ;
#10701 = AXIS2_PLACEMENT_3D ( 'NONE', #2167, #28300, #46012 ) ;
#10702 = ORIENTED_EDGE ( 'NONE', *, *, #2224, .T. ) ;
#10703 = CARTESIAN_POINT ( 'NONE',  ( 0.7185039370078739607, 1.928577636452523993E-17, 1.279527558947590515 ) ) ;
#10704 = CARTESIAN_POINT ( 'NONE',  ( 0.1572356565281126384, -0.09317336072454235341, -0.1946530291195974205 ) ) ;
#10705 = ORIENTED_EDGE ( 'NONE', *, *, #9376, .T. ) ;
#10706 = CARTESIAN_POINT ( 'NONE',  ( 1.002407869896990045, -0.1264236179284866091, 0.5339566928596221063 ) ) ;
#10707 = ORIENTED_EDGE ( 'NONE', *, *, #15433, .F. ) ;
#10708 = CARTESIAN_POINT ( 'NONE',  ( -0.6971942568897648851, 0.07405724077823318263, 1.456692913332062522 ) ) ;
#10709 = CARTESIAN_POINT ( 'NONE',  ( 2.892866454678787531E-17, 0.1102362205799679168, 0.1574803149606299191 ) ) ;
#10710 = CARTESIAN_POINT ( 'NONE',  ( -1.054774247047244540, -0.07405724077823318263, 1.126968503883244654 ) ) ;
#10711 = CARTESIAN_POINT ( 'NONE',  ( -0.7185039370078746268, -0.06523048226347956391, 0.1500984251968505434 ) ) ;
#10712 = EDGE_LOOP ( 'NONE', ( #16886, #31747 ) ) ;
#10713 = CARTESIAN_POINT ( 'NONE',  ( -0.7495606340400177148, 0.1264236179284866091, 1.139271653489543290 ) ) ;
#10714 = CARTESIAN_POINT ( 'NONE',  ( -1.002407869896990045, 0.1264236179284866091, 0.2682086613635594752 ) ) ;
#10715 = CARTESIAN_POINT ( 'NONE',  ( -0.1296641775163207277, 1.495705267341506772, -0.3569552279982053378 ) ) ;
#10716 = DIRECTION ( 'NONE',  ( -1.000000000000000000, 0.000000000000000000, 0.000000000000000000 ) ) ;
#10717 = CARTESIAN_POINT ( 'NONE',  ( 0.1264236179284866091, -0.8677420784654585884, 0.1264236179284866091 ) ) ;
#10718 = EDGE_LOOP ( 'NONE', ( #6894, #42010, #16054, #42598 ) ) ;
#10719 = DIRECTION ( 'NONE',  ( 8.659560562353054383E-17, 0.7071067811867007835, -0.7071067811863941399 ) ) ;
#10720 = AXIS2_PLACEMENT_3D ( 'NONE', #40829, #14522, #36566 ) ;
#10721 = CARTESIAN_POINT ( 'NONE',  ( 0.7931922328058882421, 0.1592273191109241925, 0.03937007863263045776 ) ) ;
#10722 = VERTEX_POINT ( 'NONE', #11155 ) ;
#10723 = CARTESIAN_POINT ( 'NONE',  ( 0.7185039370078739607, 0.000000000000000000, 4.498031496062992574 ) ) ;
#10724 = PLANE ( 'NONE',  #17174 ) ;
#10725 = EDGE_CURVE ( 'NONE', #22756, #28803, #40345, .T. ) ;
#10726 = CARTESIAN_POINT ( 'NONE',  ( -0.6971942568897637749, 2.189545951927499583E-17, 0.7504921259304880854 ) ) ;
#10727 = CARTESIAN_POINT ( 'NONE',  ( -0.7185039370078746268, -0.06523048226347956391, 0.5733267715460159675 ) ) ;
#10728 = ORIENTED_EDGE ( 'NONE', *, *, #22778, .F. ) ;
#10729 = CARTESIAN_POINT ( 'NONE',  ( -0.6971942568897648851, -0.07405724077823297447, 1.742125984198204858 ) ) ;
#10730 = ORIENTED_EDGE ( 'NONE', *, *, #3795, .T. ) ;
#10731 = CARTESIAN_POINT ( 'NONE',  ( -0.7646288533564489232, -0.1113553986120547346, 1.126968503829480328 ) ) ;
#10732 = VECTOR ( 'NONE', #3999, 39.37007874015748143 ) ;
#10733 = CARTESIAN_POINT ( 'NONE',  ( -0.7495606340400177148, 0.1264236179284866091, 0.1205708660879689087 ) ) ;
#10734 = CARTESIAN_POINT ( 'NONE',  ( 0.9873396505805591694, -0.1113553986120547346, 0.6742125984251968740 ) ) ;
#10735 = CARTESIAN_POINT ( 'NONE',  ( -0.1270800023317771588, -0.8622485339924941261, 0.1270800023317771588 ) ) ;
#10736 = CARTESIAN_POINT ( 'NONE',  ( -0.7185039370078746268, 0.06523048226347956391, 0.4109251967428667052 ) ) ;
#10737 = CARTESIAN_POINT ( 'NONE',  ( -1.033464566929134687, -0.06523048226347956391, 1.336122047136566904 ) ) ;
#10738 = EDGE_CURVE ( 'NONE', #1339, #34984, #46486, .T. ) ;
#10739 = CARTESIAN_POINT ( 'NONE',  ( 1.002407869896990045, -0.1264236179284866091, 0.6914370078202519698 ) ) ;
#10740 = CARTESIAN_POINT ( 'NONE',  ( 0.06523048226347956391, -0.5123031496062991907, -0.1574803149606300301 ) ) ;
#10741 = EDGE_CURVE ( 'NONE', #65, #38861, #7461, .T. ) ;
#10742 = CARTESIAN_POINT ( 'NONE',  ( -0.1157464095645248381, 0.1295232178076358986, 0.1214645533880106126 ) ) ;
#10743 = DIRECTION ( 'NONE',  ( -1.000000000000000000, 0.000000000000000000, 0.000000000000000000 ) ) ;
#10744 = CARTESIAN_POINT ( 'NONE',  ( 0.7646288533564489232, 0.1113553986120547346, 1.245078740157480324 ) ) ;
#10746 = CARTESIAN_POINT ( 'NONE',  ( 0.5555748031496114958, 1.061695335278752150, -0.02376411959061622975 ) ) ;
#10745 = CARTESIAN_POINT ( 'NONE',  ( 0.8020464063513640385, -0.1557015648984066136, 1.986795982854316467 ) ) ;
#10747 = AXIS2_PLACEMENT_3D ( 'NONE', #29942, #22224, #33053 ) ;
#10748 = CARTESIAN_POINT ( 'NONE',  ( 0.7185039370078746268, -0.06523048226347956391, 1.724901574803149540 ) ) ;
#10749 = ( BOUNDED_CURVE ( )  B_SPLINE_CURVE ( 2, ( #30675, #12460, #19617, #31380, #4752, #23470, #41153, #34482, #15813 ),
 .UNSPECIFIED., .F., .T. ) 
 B_SPLINE_CURVE_WITH_KNOTS ( ( 3, 2, 2, 2, 3 ),
 ( 0.6300000000000000044, 0.6324999999999999512, 0.6350000000000000089, 0.6374999999999999556, 0.6400000000000000133 ),
 .UNSPECIFIED. ) 
 CURVE ( )  GEOMETRIC_REPRESENTATION_ITEM ( )  RATIONAL_B_SPLINE_CURVE ( ( 1.000000000000000000, 0.9238795325112869605, 1.000000000000000000, 0.9238795325112869605, 1.000000000000000000, 0.9238795325112869605, 1.000000000000000000, 0.9238795325112869605, 1.000000000000000000 ) ) 
 REPRESENTATION_ITEM ( '' )  ) ;
#10750 = EDGE_CURVE ( 'NONE', #9904, #26132, #18182, .T. ) ;
#10752 = DIRECTION ( 'NONE',  ( 1.000000000000000000, 0.000000000000000000, 0.000000000000000000 ) ) ;
#10751 = CARTESIAN_POINT ( 'NONE',  ( 0.8759842519685039353, -0.1787899950787401882, 0.6028543306548976854 ) ) ;
#10753 = CARTESIAN_POINT ( 'NONE',  ( 3.284318927891251994E-17, -0.6205708660879685201, 0.1787899950787401882 ) ) ;
#10754 = CYLINDRICAL_SURFACE ( 'NONE', #10870, 0.2204724409448818867 ) ;
#10755 = DIRECTION ( 'NONE',  ( -1.020425574104001164E-16, 1.020425574104001164E-16, -1.000000000000000000 ) ) ;
#10756 = CARTESIAN_POINT ( 'NONE',  ( 0.9873396505805591694, -0.1113553986120547346, 0.7135826771653542844 ) ) ;
#10757 = CARTESIAN_POINT ( 'NONE',  ( 0.9500414927467378812, -0.1787899950787401604, 0.9202755904974182499 ) ) ;
#10758 = CARTESIAN_POINT ( 'NONE',  ( -0.1574803149606299191, 0.000000000000000000, -0.2748405511811023438 ) ) ;
#10759 = CARTESIAN_POINT ( 'NONE',  ( 3.284318927891251994E-17, -1.176673228292692830, 0.1787899950787401882 ) ) ;
#10760 = CARTESIAN_POINT ( 'NONE',  ( -0.1574803149606299191, -1.562992125984252079, 0.000000000000000000 ) ) ;
#10761 = CARTESIAN_POINT ( 'NONE',  ( -1.181102362204724310, 0.000000000000000000, -0.9842519685039370358 ) ) ;
#10762 = ADVANCED_FACE ( 'NONE', ( #40578 ), #39639, .T. ) ;
#10763 = CARTESIAN_POINT ( 'NONE',  ( -1.054774247047244540, 0.07405724077823318263, 0.1427165353793072855 ) ) ;
#10764 = ORIENTED_EDGE ( 'NONE', *, *, #14364, .T. ) ;
#10765 = FACE_OUTER_BOUND ( 'NONE', #14917, .T. ) ;
#10766 = ORIENTED_EDGE ( 'NONE', *, *, #26845, .T. ) ;
#10767 = CARTESIAN_POINT ( 'NONE',  ( -0.6971942568897648851, 0.07405724077823318263, 1.973425196796630088 ) ) ;
#10768 = CARTESIAN_POINT ( 'NONE',  ( -1.002407869896990045, -0.1264236179284866091, 1.710137795221826851 ) ) ;
#10769 = CARTESIAN_POINT ( 'NONE',  ( -0.8019270111902717657, 0.1787899950787401604, 0.3937007873478115538 ) ) ;
#10770 = ( BOUNDED_CURVE ( )  B_SPLINE_CURVE ( 2, ( #11863, #44646, #18564, #15706, #33451, #4884, #800, #4639, #345 ),
 .UNSPECIFIED., .F., .T. ) 
 B_SPLINE_CURVE_WITH_KNOTS ( ( 3, 2, 2, 2, 3 ),
 ( 0.8800000000000000044, 0.8824999999999999512, 0.8850000000000000089, 0.8874999999999999556, 0.8900000000000000133 ),
 .UNSPECIFIED. ) 
 CURVE ( )  GEOMETRIC_REPRESENTATION_ITEM ( )  RATIONAL_B_SPLINE_CURVE ( ( 1.000000000000000000, 0.9238795325112869605, 1.000000000000000000, 0.9238795325112869605, 1.000000000000000000, 0.9238795325112869605, 1.000000000000000000, 0.9238795325112869605, 1.000000000000000000 ) ) 
 REPRESENTATION_ITEM ( '' )  ) ;
#10771 = CARTESIAN_POINT ( 'NONE',  ( -0.7185039370078739607, 1.928577636452523993E-17, 0.6594488188976378451 ) ) ;
#10772 = CARTESIAN_POINT ( 'NONE',  ( 0.1587185860253795822, 0.04237460976003461915, 0.1404529029258638206 ) ) ;
#10773 = CARTESIAN_POINT ( 'NONE',  ( -1.033464566929134687, -0.06523048226347956391, 1.857775590551181244 ) ) ;
#10774 = CARTESIAN_POINT ( 'NONE',  ( -0.3010001048904012433, 0.07502508536398735939, -1.025940429181291913 ) ) ;
#10775 = CARTESIAN_POINT ( 'NONE',  ( 0.1787899950787401604, -0.4715806611426248129, 0.07405724077823318263 ) ) ;
#10776 = CARTESIAN_POINT ( 'NONE',  ( -0.01524090226806027598, -0.09842519685039370636, 0.1563540702671338822 ) ) ;
#10777 = CARTESIAN_POINT ( 'NONE',  ( 0.000000000000000000, 0.6926248950869576815, -0.5411378750921725933 ) ) ;
#10778 = DIRECTION ( 'NONE',  ( 0.000000000000000000, 0.000000000000000000, 1.000000000000000000 ) ) ;
#10779 = VECTOR ( 'NONE', #21921, 39.37007874015748854 ) ;
#10780 = AXIS2_PLACEMENT_3D ( 'NONE', #6314, #2718, #6561 ) ;
#10781 = CARTESIAN_POINT ( 'NONE',  ( -0.9500414927467378812, 0.1787899950787401604, 0.1870078739619845387 ) ) ;
#10782 = ORIENTED_EDGE ( 'NONE', *, *, #6811, .F. ) ;
#10783 = CARTESIAN_POINT ( 'NONE',  ( -1.002407869896990045, 0.1264236179284866091, 1.409940944828126153 ) ) ;
#10784 = ORIENTED_EDGE ( 'NONE', *, *, #6381, .T. ) ;
#10785 = EDGE_CURVE ( 'NONE', #21227, #42479, #25852, .T. ) ;
#10786 = CARTESIAN_POINT ( 'NONE',  ( 0.07405724077823318263, -1.134842519631275914, 0.1787899950787401604 ) ) ;
#10787 = CARTESIAN_POINT ( 'NONE',  ( 0.07405724077823318263, -1.405511810969858999, 0.1787899950787401604 ) ) ;
#10788 = SURFACE_STYLE_USAGE ( .BOTH. , #40670 ) ;
#10789 = DIRECTION ( 'NONE',  ( 0.000000000000000000, 1.000000000000000078E-15, -1.000000000000000000 ) ) ;
#10790 = CARTESIAN_POINT ( 'NONE',  ( 0.9873396505805591694, 0.1113553986120547346, 0.3690944881889763884 ) ) ;
#10791 = CARTESIAN_POINT ( 'NONE',  ( 0.07444174185955065859, -0.6186461717877695943, 0.1797182628040039087 ) ) ;
#10792 = CARTESIAN_POINT ( 'NONE',  ( 0.8759842519685039353, 0.000000000000000000, 4.498031496062992574 ) ) ;
#10793 = CARTESIAN_POINT ( 'NONE',  ( -0.8759842519685039353, -0.1574803149606299191, 0.9744094487113701408 ) ) ;
#10794 = EDGE_CURVE ( 'NONE', #19295, #9411, #5861, .T. ) ;
#10795 = CARTESIAN_POINT ( 'NONE',  ( -0.1113553986120547346, -0.1801181102362204856, 0.1113553986120547346 ) ) ;
#10796 = CARTESIAN_POINT ( 'NONE',  ( 0.7185039370078746268, 0.06523048226347956391, 1.749507873908222155 ) ) ;
#10797 = VERTEX_POINT ( 'NONE', #14274 ) ;
#10798 = CARTESIAN_POINT ( 'NONE',  ( 0.7185039370078739607, 1.928577636452523993E-17, 0.2165354329633393804 ) ) ;
#10799 = CARTESIAN_POINT ( 'NONE',  ( 0.8759842519685039353, -0.1574803149606299191, 0.7874015748031496509 ) ) ;
#10800 = CYLINDRICAL_SURFACE ( 'NONE', #24101, 0.1574803149606299191 ) ;
#10801 = AXIS2_PLACEMENT_3D ( 'NONE', #37533, #37781, #30158 ) ;
#10803 = LINE ( 'NONE', #29032, #21582 ) ;
#10802 = DIRECTION ( 'NONE',  ( -1.000000000000000000, 0.000000000000000000, 0.000000000000000000 ) ) ;
#10804 = CARTESIAN_POINT ( 'NONE',  ( 0.8107537697050234415, -0.1574803149606297803, 0.1451771652468037688 ) ) ;
#10805 = MECHANICAL_DESIGN_GEOMETRIC_PRESENTATION_REPRESENTATION (  '', ( #19186 ), #41362 ) ;
#10806 = CARTESIAN_POINT ( 'NONE',  ( 0.2642359194686346169, -3.032960542342102697E-32, 0.09842519685039370636 ) ) ;
#10807 = CARTESIAN_POINT ( 'NONE',  ( -0.7185039370078746268, -0.06523048226347956391, 0.7701771652468031304 ) ) ;
#10808 = CARTESIAN_POINT ( 'NONE',  ( 0.06523048226347956391, -1.501476377845230248, 0.1574803149606297803 ) ) ;
#10809 = CARTESIAN_POINT ( 'NONE',  ( -0.1264236179284866091, -0.7485236219934803259, 0.1264236179284866091 ) ) ;
#10810 = CARTESIAN_POINT ( 'NONE',  ( -0.8759842519685039353, 0.1574803149606299191, 0.08858267705782735257 ) ) ;
#10811 = AXIS2_PLACEMENT_3D ( 'NONE', #13382, #2337, #23931 ) ;
#10812 = CARTESIAN_POINT ( 'NONE',  ( 0.1574803149606300301, -1.033956692913387210, 0.06523048226347956391 ) ) ;
#10813 = CARTESIAN_POINT ( 'NONE',  ( 0.9873396505805591694, -0.1113553986120547346, 0.9793307085538898171 ) ) ;
#10814 = CARTESIAN_POINT ( 'NONE',  ( -0.7495606340400177148, 0.1264236179284866091, 0.4306102361667086820 ) ) ;
#10815 = VERTEX_POINT ( 'NONE', #21440 ) ;
#10816 = ORIENTED_EDGE ( 'NONE', *, *, #9607, .F. ) ;
#10817 = CARTESIAN_POINT ( 'NONE',  ( -0.7495606340400177148, -0.1264236179284866091, 1.626476377898992132 ) ) ;
#10818 = ORIENTED_EDGE ( 'NONE', *, *, #19148, .T. ) ;
#10819 = CARTESIAN_POINT ( 'NONE',  ( 0.06523048226347956391, -1.289862204616882169, -0.1574803149606300301 ) ) ;
#10820 = CARTESIAN_POINT ( 'NONE',  ( -0.6971942568897626646, 0.07405724077823318263, 0.7923228345919055560 ) ) ;
#10821 = CARTESIAN_POINT ( 'NONE',  ( -0.4330708661417340677, 0.1574803149606330277, -1.186023622047243986 ) ) ;
#10822 = CARTESIAN_POINT ( 'NONE',  ( -0.9500414927467377701, -0.1787899950787401604, 0.7627952755367883864 ) ) ;
#10823 = CARTESIAN_POINT ( 'NONE',  ( 9.848703297471225088E-18, -0.1176498932187602098, 0.07181495862115655493 ) ) ;
#10824 = CARTESIAN_POINT ( 'NONE',  ( -0.8759842519685039353, 0.000000000000000000, 0.000000000000000000 ) ) ;
#10825 = CARTESIAN_POINT ( 'NONE',  ( 0.1113553986120547346, -0.2785433069790869687, 0.1113553986120547346 ) ) ;
#10826 = CARTESIAN_POINT ( 'NONE',  ( -0.7646288533564489232, 0.1113553986120547346, 1.904527558947590515 ) ) ;
#10827 = ORIENTED_EDGE ( 'NONE', *, *, #35976, .T. ) ;
#10828 = CARTESIAN_POINT ( 'NONE',  ( -0.9873396505805591694, -0.1113553986120547346, 1.500984251968503935 ) ) ;
#10829 = CARTESIAN_POINT ( 'NONE',  ( -0.9873396505805591694, 0.1113553986120547346, 0.4478346456692913202 ) ) ;
#10830 = CARTESIAN_POINT ( 'NONE',  ( 1.002407869896990045, 0.1264236179284866091, 1.409940944828126153 ) ) ;
#10831 = CARTESIAN_POINT ( 'NONE',  ( 0.4330708661417329020, 0.1864803149606300281, -1.186023622047243986 ) ) ;
#10832 = ORIENTED_EDGE ( 'NONE', *, *, #18438, .F. ) ;
#10833 = AXIS2_PLACEMENT_3D ( 'NONE', #29514, #44060, #25868 ) ;
#10834 = ORIENTED_EDGE ( 'NONE', *, *, #22025, .F. ) ;
#10835 = DIRECTION ( 'NONE',  ( 1.000000000000000000, 0.000000000000000000, 0.000000000000000000 ) ) ;
#10836 = ORIENTED_EDGE ( 'NONE', *, *, #26096, .F. ) ;
#10837 = AXIS2_PLACEMENT_3D ( 'NONE', #34188, #41795, #8994 ) ;
#10838 = CIRCLE ( 'NONE', #16207, 0.1574803149606299191 ) ;
#10839 = ADVANCED_FACE ( 'NONE', ( #21929 ), #14502, .T. ) ;
#10840 = VECTOR ( 'NONE', #2796, 39.37007874015748143 ) ;
#10841 = DIRECTION ( 'NONE',  ( 1.822029033848725028E-16, 0.000000000000000000, 1.000000000000000000 ) ) ;
#10842 = EDGE_CURVE ( 'NONE', #7744, #18975, #47081, .T. ) ;
#10843 = CARTESIAN_POINT ( 'NONE',  ( 0.1264236179284866091, -0.8813976377415118080, -0.1264236179284866091 ) ) ;
#10844 = CARTESIAN_POINT ( 'NONE',  ( 0.7185039370078739607, 1.928577636452523993E-17, 1.053149606299212504 ) ) ;
#10845 = CARTESIAN_POINT ( 'NONE',  ( -1.033464566929133799, 1.928577636452524610E-17, 2.869337061179095023E-17 ) ) ;
#10846 = CARTESIAN_POINT ( 'NONE',  ( 1.054774247047244096, 0.000000000000000000, 1.754429133804503715 ) ) ;
#10847 = CARTESIAN_POINT ( 'NONE',  ( 0.7495606340400177148, -0.1264236179284866091, 0.3617125983714334359 ) ) ;
#10848 = CARTESIAN_POINT ( 'NONE',  ( -0.1797182628040039087, -0.1609690064334393378, -0.07444174185955065859 ) ) ;
#10849 = EDGE_CURVE ( 'NONE', #36693, #45011, #930, .T. ) ;
#10850 = CARTESIAN_POINT ( 'NONE',  ( -0.07405724077823318263, -0.1664625509064040221, 0.1787899950787401604 ) ) ;
#10851 = CARTESIAN_POINT ( 'NONE',  ( 0.1787899950787401882, -0.2563976377415121966, -2.189545951927503898E-17 ) ) ;
#10852 = CARTESIAN_POINT ( 'NONE',  ( -0.1787899950787401604, -0.007874015694267972806, -0.07405724077823318263 ) ) ;
#10853 = LINE ( 'NONE', #25466, #1977 ) ;
#10854 = ADVANCED_FACE ( 'NONE', ( #36549 ), #10538, .T. ) ;
#10855 = CARTESIAN_POINT ( 'NONE',  ( 0.8759842519685039353, 0.1787899950787401882, 0.5831692912848189803 ) ) ;
#10857 = DIRECTION ( 'NONE',  ( 0.000000000000000000, -1.000000000000000000, 0.000000000000000000 ) ) ;
#10856 = CARTESIAN_POINT ( 'NONE',  ( -0.9418700712360449367, 0.1575712691376264796, 0.03937007874015843734 ) ) ;
#10858 = CARTESIAN_POINT ( 'NONE',  ( -0.1797182628040039087, -1.691480817457061914, 0.07444174185955065859 ) ) ;
#10859 = CARTESIAN_POINT ( 'NONE',  ( 0.7495606340400177148, 0.1264236179284866091, 1.734744094434425232 ) ) ;
#10861 = CARTESIAN_POINT ( 'NONE',  ( 1.033464566929134687, 0.06523048226347956391, 0.1205708660342053040 ) ) ;
#10860 = FACE_OUTER_BOUND ( 'NONE', #8592, .T. ) ;
#10862 = ORIENTED_EDGE ( 'NONE', *, *, #15795, .T. ) ;
#10863 = CARTESIAN_POINT ( 'NONE',  ( 0.8759842519685039353, -0.1574803149606299191, 1.328740157372787278 ) ) ;
#10864 = CARTESIAN_POINT ( 'NONE',  ( -0.1787899950787401604, -0.3228346456155278266, -0.07405724077823318263 ) ) ;
#10866 = CARTESIAN_POINT ( 'NONE',  ( 0.9873396505805591694, 0.1113553986120547346, 0.4773622046168818911 ) ) ;
#10865 = CARTESIAN_POINT ( 'NONE',  ( -1.054774247047244096, 0.000000000000000000, 0.4207677164816693294 ) ) ;
#10867 = CARTESIAN_POINT ( 'NONE',  ( 0.1787899950787401604, -1.080708661363559919, -0.07405724077823318263 ) ) ;
#10868 = FACE_OUTER_BOUND ( 'NONE', #7726, .T. ) ;
#10869 = DIRECTION ( 'NONE',  ( 0.000000000000000000, 0.000000000000000000, 1.000000000000000000 ) ) ;
#10870 = AXIS2_PLACEMENT_3D ( 'NONE', #3766, #39697, #6881 ) ;
#10871 = CARTESIAN_POINT ( 'NONE',  ( -0.8759842519685039353, 0.1787899950787401882, 1.528051181048598384 ) ) ;
#10872 = ORIENTED_EDGE ( 'NONE', *, *, #40538, .F. ) ;
#10873 = CARTESIAN_POINT ( 'NONE',  ( -0.3100393700787401619, -2.714815113292586694E-26, -0.7086614173228351632 ) ) ;
#10874 = CARTESIAN_POINT ( 'NONE',  ( 1.054774247047244096, 0.000000000000000000, 1.090059055064346527 ) ) ;
#10875 = AXIS2_PLACEMENT_3D ( 'NONE', #38399, #6027, #5569 ) ;
#10876 = VECTOR ( 'NONE', #14988, 39.37007874015748143 ) ;
#10877 = CARTESIAN_POINT ( 'NONE',  ( 0.9500414927467378812, 0.1787899950787401604, 1.761811023568284007 ) ) ;
#10878 = CARTESIAN_POINT ( 'NONE',  ( -0.7185039370078746268, -0.06523048226347956391, 0.6225393700787401619 ) ) ;
#10879 = CARTESIAN_POINT ( 'NONE',  ( -0.8759842519685039353, 0.1787899950787401882, 1.094980314906866203 ) ) ;
#10880 = DIRECTION ( 'NONE',  ( 0.000000000000000000, 0.000000000000000000, -1.000000000000000000 ) ) ;
#10881 = CARTESIAN_POINT ( 'NONE',  ( -0.06244181591619046151, -0.2594434330345063433, -0.05069326177272678174 ) ) ;
#10882 = CARTESIAN_POINT ( 'NONE',  ( 1.054774247047244540, 0.07405724077823318263, 0.2657480314422993595 ) ) ;
#10883 = CARTESIAN_POINT ( 'NONE',  ( -0.6971942568897637749, 2.189545951927499583E-17, 0.2386811023084413619 ) ) ;
#10884 = CARTESIAN_POINT ( 'NONE',  ( -1.054774247047244540, -0.07405724077823318263, 0.7283464566391493200 ) ) ;
#10885 = CARTESIAN_POINT ( 'NONE',  ( 0.9412147342319837628, -0.1574803149606297803, 1.646161417215307843 ) ) ;
#10886 = EDGE_LOOP ( 'NONE', ( #14465, #46016, #10705, #35219 ) ) ;
#10887 = ( BOUNDED_CURVE ( )  B_SPLINE_CURVE ( 2, ( #20483, #32237, #28895, #2956, #314, #10659, #71, #7509, #10425 ),
 .UNSPECIFIED., .F., .T. ) 
 B_SPLINE_CURVE_WITH_KNOTS ( ( 3, 2, 2, 2, 3 ),
 ( 0.4799999999999999822, 0.4824999999999999845, 0.4849999999999999867, 0.4874999999999999889, 0.4899999999999999911 ),
 .UNSPECIFIED. ) 
 CURVE ( )  GEOMETRIC_REPRESENTATION_ITEM ( )  RATIONAL_B_SPLINE_CURVE ( ( 1.000000000000000000, 0.9238795325112869605, 1.000000000000000000, 0.9238795325112869605, 1.000000000000000000, 0.9238795325112869605, 1.000000000000000000, 0.9238795325112869605, 1.000000000000000000 ) ) 
 REPRESENTATION_ITEM ( '' )  ) ;
#10888 = CARTESIAN_POINT ( 'NONE',  ( -0.1787899950787401604, -0.08169291333206318839, 0.07405724077823318263 ) ) ;
#10889 = CARTESIAN_POINT ( 'NONE',  ( 0.6971942568897626646, 0.07405724077823318263, 0.7923228345919055560 ) ) ;
#10890 = CARTESIAN_POINT ( 'NONE',  ( 0.9500414927467377701, -0.1787899950787401604, 1.003937007820253413 ) ) ;
#10891 = CARTESIAN_POINT ( 'NONE',  ( -0.6971942568897637749, 2.189545951927499583E-17, 1.813484251914740053 ) ) ;
#10892 = CARTESIAN_POINT ( 'NONE',  ( 0.9500414927467378812, -0.1787899950787401604, 1.865157480261195877 ) ) ;
#10893 = LINE ( 'NONE', #25259, #21384 ) ;
#10894 = CARTESIAN_POINT ( 'NONE',  ( -0.1264236179284866091, -1.231915306811915523, 0.1264236179284866091 ) ) ;
#10895 = ORIENTED_EDGE ( 'NONE', *, *, #9370, .F. ) ;
#10896 = CARTESIAN_POINT ( 'NONE',  ( -0.1264236179284866091, -0.3105314960092286913, 0.1264236179284866091 ) ) ;
#10897 = CARTESIAN_POINT ( 'NONE',  ( -0.2927220607601821456, -0.1026043301529240143, 0.7433660568023925386 ) ) ;
#10898 = ORIENTED_EDGE ( 'NONE', *, *, #14082, .T. ) ;
#10899 = CARTESIAN_POINT ( 'NONE',  ( 0.9500414927467378812, 0.1787899950787401604, 1.171259842465921741 ) ) ;
#10900 = AXIS2_PLACEMENT_3D ( 'NONE', #43405, #24507, #10132 ) ;
#10901 = CARTESIAN_POINT ( 'NONE',  ( -0.9873396505805591694, -0.1113553986120547346, 1.215551180994834723 ) ) ;
#10902 = CARTESIAN_POINT ( 'NONE',  ( -0.2471922904502827645, -0.09842519685039372024, 0.01321092903694667461 ) ) ;
#10903 = EDGE_CURVE ( 'NONE', #28143, #6860, #795, .T. ) ;
#10904 = CIRCLE ( 'NONE', #7825, 0.1574803149606300579 ) ;
#10905 = CARTESIAN_POINT ( 'NONE',  ( 0.8759842519685039353, -0.1787899950787401882, 1.508366141678519678 ) ) ;
#10906 = CARTESIAN_POINT ( 'NONE',  ( 0.7495606340400177148, -0.1264236179284866091, 0.08612204719033110523 ) ) ;
#10907 = VECTOR ( 'NONE', #42440, 39.37007874015748143 ) ;
#10908 = CARTESIAN_POINT ( 'NONE',  ( 0.07405724077823318263, -1.671259842465922407, -0.1787899950787401604 ) ) ;
#10909 = EDGE_CURVE ( 'NONE', #38992, #6537, #19020, .T. ) ;
#10910 = CARTESIAN_POINT ( 'NONE',  ( -0.7495606340400177148, -0.1264236179284866091, 0.5241141731745827537 ) ) ;
#10911 = DIRECTION ( 'NONE',  ( 0.000000000000000000, 0.000000000000000000, -1.000000000000000000 ) ) ;
#10912 = CARTESIAN_POINT ( 'NONE',  ( -0.7646288533564489232, 0.1113553986120547346, 1.205708661417322913 ) ) ;
#10913 = CARTESIAN_POINT ( 'NONE',  ( 0.8019270111902717657, -0.1787899950787401604, 1.156496062938362046 ) ) ;
#10914 = CARTESIAN_POINT ( 'NONE',  ( 0.9500414927467377701, -0.1787899950787401604, 1.668307086560410157 ) ) ;
#10915 = CARTESIAN_POINT ( 'NONE',  ( -0.7646288533564489232, 0.1113553986120547346, 0.6446850392625511628 ) ) ;
#10916 = CARTESIAN_POINT ( 'NONE',  ( -0.7185039370078746268, 0.06523048226347956391, 1.011318897637796033 ) ) ;
#10917 = DIRECTION ( 'NONE',  ( 0.000000000000000000, 0.000000000000000000, 1.000000000000000000 ) ) ;
#10918 = CARTESIAN_POINT ( 'NONE',  ( 0.1113553986120547346, -0.7805118109160945616, -0.1113553986120547346 ) ) ;
#10919 = CARTESIAN_POINT ( 'NONE',  ( -0.8759842519685039353, 0.1574803149606299191, 1.781496062884598164 ) ) ;
#10920 = CARTESIAN_POINT ( 'NONE',  ( 0.9500414927467378812, 0.1787899950787401604, 0.1476377952218271561 ) ) ;
#10921 = CARTESIAN_POINT ( 'NONE',  ( 0.7125016681442003508, -0.05105472478026783223, 0.03937008547748529347 ) ) ;
#10922 = DIRECTION ( 'NONE',  ( -3.469446951953614583E-15, -1.000000000000000000, 0.000000000000000000 ) ) ;
#10923 = CARTESIAN_POINT ( 'NONE',  ( 0.8759842519685039353, 0.000000000000000000, 4.498031496062992574 ) ) ;
#10924 = CARTESIAN_POINT ( 'NONE',  ( -1.054774247047244096, 0.000000000000000000, 1.242618110182456714 ) ) ;
#10925 = CARTESIAN_POINT ( 'NONE',  ( 0.7185039370078739607, 1.928577636452523993E-17, 0.4527559054042842868 ) ) ;
#10926 = VERTEX_POINT ( 'NONE', #11626 ) ;
#10927 = CARTESIAN_POINT ( 'NONE',  ( 0.8689611821192279040, 0.1748045417376594690, 0.03936951059370389500 ) ) ;
#10928 = CARTESIAN_POINT ( 'NONE',  ( 0.8107537697050254399, 0.1574803149606300301, 0.8390748030420788206 ) ) ;
#10929 = CARTESIAN_POINT ( 'NONE',  ( -0.8107537697050253289, 0.1574803149606300301, 0.4453740156405042727 ) ) ;
#10930 = CARTESIAN_POINT ( 'NONE',  ( 0.002334186094749960728, 0.03366073001697469924, 0.1377957753753820402 ) ) ;
#10931 = CARTESIAN_POINT ( 'NONE',  ( 1.002407869896990045, 0.1264236179284866091, 1.405019684985606476 ) ) ;
#10932 = CARTESIAN_POINT ( 'NONE',  ( -1.033464566929133799, 0.000000000000000000, 1.151574803149606474 ) ) ;
#10934 = CARTESIAN_POINT ( 'NONE',  ( -0.7646288533564489232, -0.1113553986120547346, 1.373031496062992352 ) ) ;
#10933 = CARTESIAN_POINT ( 'NONE',  ( -0.8759842519685039353, 0.1574803149606299191, 0.09842519685039370636 ) ) ;
#10935 = CARTESIAN_POINT ( 'NONE',  ( -0.1787899950787401604, -0.07677165348954355373, 0.07405724077823318263 ) ) ;
#10936 = ORIENTED_EDGE ( 'NONE', *, *, #27522, .T. ) ;
#10937 = CARTESIAN_POINT ( 'NONE',  ( 0.1605321103696192298, -0.05726506528273173774, -0.1404876550525108458 ) ) ;
#10938 = VECTOR ( 'NONE', #5855, 39.37007874015748143 ) ;
#10939 = ORIENTED_EDGE ( 'NONE', *, *, #26804, .F. ) ;
#10940 = LINE ( 'NONE', #25558, #45112 ) ;
#10941 = CARTESIAN_POINT ( 'NONE',  ( -0.1121631700669266513, 0.09842519685039372024, 0.2206756344348398957 ) ) ;
#10942 = CARTESIAN_POINT ( 'NONE',  ( 0.7495606340400177148, -0.1264236179284866091, 0.5634842519147401640 ) ) ;
#10943 = ORIENTED_EDGE ( 'NONE', *, *, #17127, .T. ) ;
#10944 = CARTESIAN_POINT ( 'NONE',  ( -0.9500414927467377701, 0.1787899950787401604, 1.446850393647023836 ) ) ;
#10945 = CARTESIAN_POINT ( 'NONE',  ( -0.06523048226347956391, 0.06840551191855072377, 0.1574803149606297803 ) ) ;
#10946 = CARTESIAN_POINT ( 'NONE',  ( -0.6971942568897648851, -0.07405724077823297447, 1.151574803095843036 ) ) ;
#10947 = AXIS2_PLACEMENT_3D ( 'NONE', #6172, #28019, #27322 ) ;
#10948 = CARTESIAN_POINT ( 'NONE',  ( -0.9500414927467378812, 0.1787899950787401604, 0.8612204723871809131 ) ) ;
#10949 = CARTESIAN_POINT ( 'NONE',  ( -0.6971942568897626646, 0.07405724077823318263, 0.1624015747493861295 ) ) ;
#10950 = CARTESIAN_POINT ( 'NONE',  ( 1.033464566929134687, 0.06523048226347956391, 0.7898622046168821687 ) ) ;
#10951 = CARTESIAN_POINT ( 'NONE',  ( 0.07405724077823318263, -0.8308326296465612382, 0.1787899950787401604 ) ) ;
#10952 = VECTOR ( 'NONE', #40512, 39.37007874015748143 ) ;
#10953 = VERTEX_POINT ( 'NONE', #1044 ) ;
#10954 = CARTESIAN_POINT ( 'NONE',  ( -0.09235291751817698014, -0.08956172857085197003, 0.1299824129084523605 ) ) ;
#10955 = DIRECTION ( 'NONE',  ( 1.822029033848725028E-16, 0.000000000000000000, 1.000000000000000000 ) ) ;
#10956 = ORIENTED_EDGE ( 'NONE', *, *, #429, .T. ) ;
#10957 = ORIENTED_EDGE ( 'NONE', *, *, #3992, .F. ) ;
#10958 = CARTESIAN_POINT ( 'NONE',  ( 0.000000000000000000, -0.09842519685039370636, 0.000000000000000000 ) ) ;
#10959 = CARTESIAN_POINT ( 'NONE',  ( -0.7495606340400177148, 0.1264236179284866091, 0.7849409448281259305 ) ) ;
#10960 = EDGE_CURVE ( 'NONE', #4077, #14069, #34374, .T. ) ;
#10961 = ORIENTED_EDGE ( 'NONE', *, *, #7573, .F. ) ;
#10962 = CARTESIAN_POINT ( 'NONE',  ( -0.6971942568897637749, 2.189545951927499583E-17, 1.857775590497417362 ) ) ;
#10963 = EDGE_CURVE ( 'NONE', #44204, #47215, #32163, .T. ) ;
#10964 = CIRCLE ( 'NONE', #16232, 0.1574803149606299191 ) ;
#10965 = CARTESIAN_POINT ( 'NONE',  ( -1.054774247047244540, -0.07405724077823318263, 0.06397637789899228433 ) ) ;
#10966 = CARTESIAN_POINT ( 'NONE',  ( 0.9412147342319837628, -0.1574803149606297803, 0.7111220472440957785 ) ) ;
#10967 = CARTESIAN_POINT ( 'NONE',  ( -0.1797182628040039365, -0.8671697938350138024, 0.000000000000000000 ) ) ;
#10968 = CARTESIAN_POINT ( 'NONE',  ( 0.1673228346456693549, -0.4889725119976396361, -0.8550419489141689589 ) ) ;
#10969 = CARTESIAN_POINT ( 'NONE',  ( -0.7185039370078739607, 1.928577636452523993E-17, 1.515748031388535200 ) ) ;
#10970 = CARTESIAN_POINT ( 'NONE',  ( 0.6971942568897626646, 0.07405724077823318263, 0.8316929133320636325 ) ) ;
#10971 = CARTESIAN_POINT ( 'NONE',  ( 1.002407869896990045, 0.1264236179284866091, 1.365649606245448844 ) ) ;
#10972 = AXIS2_PLACEMENT_3D ( 'NONE', #40212, #22244, #44052 ) ;
#10973 = VECTOR ( 'NONE', #14135, 39.37007874015748854 ) ;
#10974 = DIRECTION ( 'NONE',  ( 0.000000000000000000, 0.000000000000000000, -1.000000000000000000 ) ) ;
#10975 = CARTESIAN_POINT ( 'NONE',  ( -0.1279527559055118058, 0.2216206741968047289, -0.3149606299212598381 ) ) ;
#10976 = CARTESIAN_POINT ( 'NONE',  ( 0.9873396505805591694, 0.1113553986120547346, 1.471456692913385877 ) ) ;
#10978 = CARTESIAN_POINT ( 'NONE',  ( -0.1586641775163213364, 0.1169123912647608288, -2.121729632260068055 ) ) ;
#10977 = CARTESIAN_POINT ( 'NONE',  ( 0.8206978720991248144, -0.1637064837517050730, 1.987174065507188780 ) ) ;
#10979 = FACE_OUTER_BOUND ( 'NONE', #18165, .T. ) ;
#10980 = CIRCLE ( 'NONE', #37859, 0.09940944881889761386 ) ;
#10982 = DIRECTION ( 'NONE',  ( 0.000000000000000000, 1.000000000000000000, 0.000000000000000000 ) ) ;
#10981 = CARTESIAN_POINT ( 'NONE',  ( 0.8759842519685039353, 0.1787899950787401882, 0.7406496062454487328 ) ) ;
#10983 = CARTESIAN_POINT ( 'NONE',  ( 0.1787899950787401604, -0.8100393700249772788, 0.07405724077823318263 ) ) ;
#10984 = VERTEX_POINT ( 'NONE', #22869 ) ;
#10985 = LINE ( 'NONE', #43305, #13074 ) ;
#10986 = DIRECTION ( 'NONE',  ( 0.000000000000000000, 0.000000000000000000, -1.000000000000000000 ) ) ;
#10987 = CARTESIAN_POINT ( 'NONE',  ( 0.8759842519685039353, -0.1787899950787401882, 0.9965551180564724554 ) ) ;
#10988 = DIRECTION ( 'NONE',  ( 1.000000000000000000, 0.000000000000000000, -1.822029033848725275E-16 ) ) ;
#10989 = CARTESIAN_POINT ( 'NONE',  ( 0.1113553986120547346, -1.508858267716535417, 0.1113553986120547346 ) ) ;
#10990 = EDGE_CURVE ( 'NONE', #5491, #44801, #14365, .T. ) ;
#10991 = LINE ( 'NONE', #21760, #15302 ) ;
#10992 = ORIENTED_EDGE ( 'NONE', *, *, #33424, .T. ) ;
#10993 = CARTESIAN_POINT ( 'NONE',  ( -0.9500414927467378812, 0.1787899950787401604, 0.1082677164816695514 ) ) ;
#10994 = CARTESIAN_POINT ( 'NONE',  ( 0.1113553986120547346, 0.1053149606299212532, 0.1113553986120547346 ) ) ;
#10995 = ORIENTED_EDGE ( 'NONE', *, *, #5952, .T. ) ;
#10996 = CARTESIAN_POINT ( 'NONE',  ( -0.8019270111902716547, 0.1787899950787401604, 1.968503936954110412 ) ) ;
#10997 = CARTESIAN_POINT ( 'NONE',  ( -0.7495606340400177148, -0.1264236179284866091, 1.739665354276945131 ) ) ;
#10998 = CARTESIAN_POINT ( 'NONE',  ( -0.9500414927467378812, 0.1787899950787401604, 1.092519684985605810 ) ) ;
#10999 = CARTESIAN_POINT ( 'NONE',  ( -1.002407869896990045, 0.1264236179284866091, 0.3469488188438744070 ) ) ;
#11000 = DIRECTION ( 'NONE',  ( 0.000000000000000000, -1.000000000000000000, 0.000000000000000000 ) ) ;
#11001 = CARTESIAN_POINT ( 'NONE',  ( -0.1574803149606299191, 0.5323553679591568333, -0.7566348232351034486 ) ) ;
#11002 = CARTESIAN_POINT ( 'NONE',  ( 1.002407869896990045, 0.1264236179284866091, 0.06643700782025216411 ) ) ;
#11003 = CARTESIAN_POINT ( 'NONE',  ( -1.033464566929133799, 0.000000000000000000, 0.5610236220472440971 ) ) ;
#11004 = CARTESIAN_POINT ( 'NONE',  ( 0.07405724077823318263, -0.4371318422449868013, 0.1787899950787401604 ) ) ;
#11005 = CARTESIAN_POINT ( 'NONE',  ( -0.1516314384195220633, -0.09842519685039370636, -0.09561409171430847176 ) ) ;
#11006 = CARTESIAN_POINT ( 'NONE',  ( 0.8759842519685039353, 0.000000000000000000, 4.498031496062992574 ) ) ;
#11007 = CARTESIAN_POINT ( 'NONE',  ( -1.002407869896990045, -0.1264236179284866091, 0.2534448818360003908 ) ) ;
#11008 = EDGE_CURVE ( 'NONE', #28092, #30092, #26722, .T. ) ;
#11009 = CARTESIAN_POINT ( 'NONE',  ( 0.2471902767489403685, -0.09658829859166323528, 0.02317992046427707481 ) ) ;
#11010 = ORIENTED_EDGE ( 'NONE', *, *, #33199, .F. ) ;
#11011 = CARTESIAN_POINT ( 'NONE',  ( -1.054774247047244096, 0.000000000000000000, 1.405019684985606476 ) ) ;
#11012 = ORIENTED_EDGE ( 'NONE', *, *, #9538, .T. ) ;
#11013 = EDGE_CURVE ( 'NONE', #27525, #45154, #4176, .T. ) ;
#11014 = CARTESIAN_POINT ( 'NONE',  ( 0.1787899950787401604, -1.248031496009228913, 0.07405724077823318263 ) ) ;
#11015 = CARTESIAN_POINT ( 'NONE',  ( 0.07405724077823318263, -1.326771653489542402, 0.1787899950787401604 ) ) ;
#11016 = ( BOUNDED_CURVE ( )  B_SPLINE_CURVE ( 2, ( #1860, #27544, #9301, #12681, #45457, #23922, #2096, #23680, #38530 ),
 .UNSPECIFIED., .F., .F. ) 
 B_SPLINE_CURVE_WITH_KNOTS ( ( 3, 2, 2, 2, 3 ),
 ( 0.4699999999999999734, 0.4724999999999999756, 0.4749999999999999778, 0.4774999999999999800, 0.4799999999999999822 ),
 .UNSPECIFIED. ) 
 CURVE ( )  GEOMETRIC_REPRESENTATION_ITEM ( )  RATIONAL_B_SPLINE_CURVE ( ( 1.000000000000000000, 0.9238795325112879597, 1.000000000000000000, 0.9238795325112869605, 1.000000000000000000, 0.9238795325112869605, 1.000000000000000000, 0.9238795325112869605, 1.000000000000000000 ) ) 
 REPRESENTATION_ITEM ( '' )  ) ;
#11017 = EDGE_CURVE ( 'NONE', #37016, #480, #2744, .T. ) ;
#11018 = DIRECTION ( 'NONE',  ( 0.001045413116529999870, -0.3952598174835958988, 0.9185687692243027502 ) ) ;
#11019 = CARTESIAN_POINT ( 'NONE',  ( -0.1797182628040039087, -0.6334099513153290673, -0.07444174185955065859 ) ) ;
#11020 = DIRECTION ( 'NONE',  ( 8.659560562353054383E-17, 0.7071067811867007835, -0.7071067811863941399 ) ) ;
#11021 = CARTESIAN_POINT ( 'NONE',  ( 1.002407869896990045, 0.1264236179284866091, 0.4256889763241890057 ) ) ;
#11022 = CARTESIAN_POINT ( 'NONE',  ( 0.06523048226347956391, -0.1727362204724408601, 0.1574803149606297803 ) ) ;
#11023 = ORIENTED_EDGE ( 'NONE', *, *, #34924, .F. ) ;
#11024 = CARTESIAN_POINT ( 'NONE',  ( 0.8107537697050253289, 0.1574803149606300301, 1.823326771546016856 ) ) ;
#11025 = EDGE_LOOP ( 'NONE', ( #29013, #14993, #45918, #16432 ) ) ;
#11026 = CARTESIAN_POINT ( 'NONE',  ( -0.1264236179284866091, -0.1973425196312759700, 0.1264236179284866091 ) ) ;
#11027 = CARTESIAN_POINT ( 'NONE',  ( 0.7646288533564489232, -0.1113553986120547346, 0.2214566928058590567 ) ) ;
#11028 = CARTESIAN_POINT ( 'NONE',  ( 0.9873396505805591694, -0.1113553986120547346, 0.7923228346456693272 ) ) ;
#11029 = DIRECTION ( 'NONE',  ( 0.000000000000000000, 0.000000000000000000, 1.000000000000000000 ) ) ;
#11031 = LINE ( 'NONE', #22258, #33863 ) ;
#11030 = CARTESIAN_POINT ( 'NONE',  ( -0.3161444924769509779, 2.559880088878760951, -3.648497683167374550 ) ) ;
#11032 = CARTESIAN_POINT ( 'NONE',  ( 0.9412147342319837628, -0.1574803149606297803, 0.7898622047244097111 ) ) ;
#11033 = CIRCLE ( 'NONE', #34035, 0.4724409448818896462 ) ;
#11034 = CARTESIAN_POINT ( 'NONE',  ( -0.2617458567146320192, 0.1661939583519094210, 0.8983839595853735371 ) ) ;
#11035 = ORIENTED_EDGE ( 'NONE', *, *, #30144, .T. ) ;
#11036 = VERTEX_POINT ( 'NONE', #7322 ) ;
#11037 = CARTESIAN_POINT ( 'NONE',  ( -0.4330708661417337901, 0.1574803149606330277, 0.9891732283464566011 ) ) ;
#11038 = CARTESIAN_POINT ( 'NONE',  ( 0.9873396505805591694, -0.1113553986120547346, 1.382874015748031704 ) ) ;
#11039 = CARTESIAN_POINT ( 'NONE',  ( 0.1787899950787401882, -1.555610236166708571, -2.189545951927503898E-17 ) ) ;
#11040 = CARTESIAN_POINT ( 'NONE',  ( -0.1574803149606297803, -1.550688976270427011, 0.06523048226347956391 ) ) ;
#11041 = CARTESIAN_POINT ( 'NONE',  ( -0.07405724077823318263, -0.7608267715997808489, -0.1787899950787401604 ) ) ;
#11042 = CARTESIAN_POINT ( 'NONE',  ( -0.7646288533564489232, -0.1113553986120547346, 0.06397637784522892945 ) ) ;
#11043 = CARTESIAN_POINT ( 'NONE',  ( -9.642888182262618425E-18, -1.021653543307086576, -0.1574803149606299191 ) ) ;
#11045 = ( BOUNDED_CURVE ( )  B_SPLINE_CURVE ( 2, ( #41426, #23261, #37876, #19651, #27357, #1420, #16079, #3320, #35913 ),
 .UNSPECIFIED., .F., .F. ) 
 B_SPLINE_CURVE_WITH_KNOTS ( ( 3, 2, 2, 2, 3 ),
 ( 0.1400000000000000133, 0.1424999999999999878, 0.1449999999999999900, 0.1474999999999999922, 0.1499999999999999944 ),
 .UNSPECIFIED. ) 
 CURVE ( )  GEOMETRIC_REPRESENTATION_ITEM ( )  RATIONAL_B_SPLINE_CURVE ( ( 1.000000000000000000, 0.9238795325112869605, 1.000000000000000000, 0.9238795325112869605, 1.000000000000000000, 0.9238795325112869605, 1.000000000000000000, 0.9238795325112869605, 1.000000000000000000 ) ) 
 REPRESENTATION_ITEM ( '' )  ) ;
#11044 = CARTESIAN_POINT ( 'NONE',  ( 0.8107537697050253289, 0.1574803149606300301, 0.9178149605223947516 ) ) ;
#11046 = PLANE ( 'NONE',  #47419 ) ;
#11047 = CARTESIAN_POINT ( 'NONE',  ( -1.054774247047244540, -0.07405724077823318263, 0.4133858267178901480 ) ) ;
#11048 = ORIENTED_EDGE ( 'NONE', *, *, #34881, .F. ) ;
#11049 = ORIENTED_EDGE ( 'NONE', *, *, #43540, .F. ) ;
#11050 = ORIENTED_EDGE ( 'NONE', *, *, #3903, .F. ) ;
#11051 = COLOUR_RGB ( '', 0.40784314, 0.44705882, 0.49803922) ;
#11052 = CARTESIAN_POINT ( 'NONE',  ( -0.9500414927467378812, -0.1787899950787401604, 1.555118110182455382 ) ) ;
#11053 = CARTESIAN_POINT ( 'NONE',  ( 0.7495606340400177148, 0.1264236179284866091, 1.734744094434425232 ) ) ;
#11054 = CARTESIAN_POINT ( 'NONE',  ( -1.054774247047244540, 0.07405724077823318263, 0.8562992125446617919 ) ) ;
#11055 = CARTESIAN_POINT ( 'NONE',  ( 0.7495606340400177148, 0.1264236179284866091, 0.3174212597887562382 ) ) ;
#11056 = CARTESIAN_POINT ( 'NONE',  ( -0.7646288533564489232, -0.1113553986120547346, 1.678149606191684962 ) ) ;
#11057 = CARTESIAN_POINT ( 'NONE',  ( 0.8019270111902716547, -0.1787899950787401604, 0.7627952755367883864 ) ) ;
#11058 = CARTESIAN_POINT ( 'NONE',  ( -1.054774247047244540, -0.07405724077823318263, 0.7283464566391492090 ) ) ;
#11059 = CARTESIAN_POINT ( 'NONE',  ( 7.107660667886486858E-05, -0.1159713038039308503, 0.07472206960544050536 ) ) ;
#11060 = CARTESIAN_POINT ( 'NONE',  ( -1.054774247047244540, -0.07405724077823318263, 1.520669291284818758 ) ) ;
#11061 = CARTESIAN_POINT ( 'NONE',  ( -0.9412147342319837628, 0.1574803149606300301, 1.936515747923967856 ) ) ;
#11062 = ORIENTED_EDGE ( 'NONE', *, *, #7709, .F. ) ;
#11063 = CARTESIAN_POINT ( 'NONE',  ( -0.7185039370078746268, -0.06523048226347956391, 1.606791338582677309 ) ) ;
#11064 = CARTESIAN_POINT ( 'NONE',  ( 0.2066929133858268486, -0.3146900525635061840, -1.066148349997451339 ) ) ;
#11065 = ADVANCED_FACE ( 'NONE', ( #576 ), #32506, .T. ) ;
#11066 = CARTESIAN_POINT ( 'NONE',  ( 1.002407869896990045, -0.1264236179284866091, 1.518208661363559031 ) ) ;
#11067 = CYLINDRICAL_SURFACE ( 'NONE', #17946, 0.1574803149606299191 ) ;
#11068 = ORIENTED_EDGE ( 'NONE', *, *, #35855, .F. ) ;
#11069 = ORIENTED_EDGE ( 'NONE', *, *, #17254, .T. ) ;
#11070 = CARTESIAN_POINT ( 'NONE',  ( -0.1264236179284866091, -0.6747047243556849594, -0.1264236179284866091 ) ) ;
#11071 = ORIENTED_EDGE ( 'NONE', *, *, #45879, .F. ) ;
#11072 = TOROIDAL_SURFACE ( 'NONE', #22540, 0.2047244094488188948, 0.01968503937007873988 ) ;
#11073 = AXIS2_PLACEMENT_3D ( 'NONE', #11142, #14261, #43464 ) ;
#11074 = EDGE_CURVE ( 'NONE', #29015, #39837, #11313, .T. ) ;
#11075 = FACE_OUTER_BOUND ( 'NONE', #45725, .T. ) ;
#11076 = CARTESIAN_POINT ( 'NONE',  ( -0.07405724077823318263, -0.8740157479777336258, -0.1787899950787401604 ) ) ;
#11077 = CARTESIAN_POINT ( 'NONE',  ( 0.9412147342319837628, 0.1574803149606300301, 1.040846456692913424 ) ) ;
#11078 = DIRECTION ( 'NONE',  ( 0.000000000000000000, -1.000000000000000000, 0.000000000000000000 ) ) ;
#11079 = CIRCLE ( 'NONE', #27928, 0.1574803149606301966 ) ;
#11080 = CARTESIAN_POINT ( 'NONE',  ( 0.1797182628040039087, -0.1757327859609983112, -0.07444174185955065859 ) ) ;
#11081 = CARTESIAN_POINT ( 'NONE',  ( 0.1787899950787401882, -0.1541594013001049146, -2.189545951927503898E-17 ) ) ;
#11082 = CARTESIAN_POINT ( 'NONE',  ( 0.1787899950787401882, -0.1038385826234017734, -2.189545951927503898E-17 ) ) ;
#11083 = CARTESIAN_POINT ( 'NONE',  ( 0.2471922904502826812, -0.09842519685039370636, -5.914624404477007554E-17 ) ) ;
#11084 = CARTESIAN_POINT ( 'NONE',  ( 1.054774247047244540, -0.07405724077823318263, 0.6889763778989935750 ) ) ;
#11086 = LINE ( 'NONE', #27378, #18535 ) ;
#11085 = CARTESIAN_POINT ( 'NONE',  ( 0.8759842519685039353, 0.000000000000000000, 4.498031496062992574 ) ) ;
#11088 = CARTESIAN_POINT ( 'NONE',  ( -0.8731188658399394731, -0.1744580357768550638, 1.988137801528226278 ) ) ;
#11087 = CARTESIAN_POINT ( 'NONE',  ( 0.8759842519685039353, 0.000000000000000000, 4.498031496062992574 ) ) ;
#11089 = CARTESIAN_POINT ( 'NONE',  ( -1.033464566929133799, 0.000000000000000000, 1.141732283357039357 ) ) ;
#11090 = CARTESIAN_POINT ( 'NONE',  ( 1.054774247047244540, -0.07405724077823318263, 1.796259842465923073 ) ) ;
#11091 = CARTESIAN_POINT ( 'NONE',  ( -0.1888229765468985855, -0.07899262986810677567, 0.1764160547656800637 ) ) ;
#11092 = CARTESIAN_POINT ( 'NONE',  ( 0.1564216623530370331, 8.908831420875236139E-13, 0.1403857474672218497 ) ) ;
#11094 = CARTESIAN_POINT ( 'NONE',  ( -1.094772975963752103E-17, -0.2514763778989925203, -0.1787899950787401882 ) ) ;
#11093 = CARTESIAN_POINT ( 'NONE',  ( -9.642888182262618425E-18, -0.9330708660342048599, -0.1574803149606299191 ) ) ;
#11096 = CARTESIAN_POINT ( 'NONE',  ( -0.4338976377952755703, -2.656856766417909227E-17, 0.000000000000000000 ) ) ;
#11095 = CARTESIAN_POINT ( 'NONE',  ( -0.7495606340400177148, 0.1264236179284866091, 0.4749015747493858242 ) ) ;
#11097 = CARTESIAN_POINT ( 'NONE',  ( -0.07405724077823318263, -1.134842519631275914, 0.1787899950787401604 ) ) ;
#11098 = DIRECTION ( 'NONE',  ( -0.5735764363510518216, -0.8191520442889876907, 0.000000000000000000 ) ) ;
#11099 = CARTESIAN_POINT ( 'NONE',  ( 1.002407869896990045, -0.1264236179284866091, 0.5684055117572598403 ) ) ;
#11100 = CARTESIAN_POINT ( 'NONE',  ( -1.054774247047244540, 0.07405724077823318263, 1.560039370024977057 ) ) ;
#11101 = ORIENTED_EDGE ( 'NONE', *, *, #22672, .F. ) ;
#11102 = CIRCLE ( 'NONE', #43217, 0.09940944881889761386 ) ;
#11103 = CARTESIAN_POINT ( 'NONE',  ( -1.002407869896990045, -0.1264236179284866091, 1.203248031442299304 ) ) ;
#11104 = CARTESIAN_POINT ( 'NONE',  ( -0.7185039370078739607, 1.928577636452523993E-17, 0.8956692913385826404 ) ) ;
#11105 = CARTESIAN_POINT ( 'NONE',  ( 1.054774247047244540, -0.07405724077823318263, 1.126968503883244654 ) ) ;
#11106 = AXIS2_PLACEMENT_3D ( 'NONE', #47428, #38287, #27302 ) ;
#11107 = CARTESIAN_POINT ( 'NONE',  ( 0.8019270111902717657, -0.1787899950787401604, 1.978346456639149320 ) ) ;
#11108 = CARTESIAN_POINT ( 'NONE',  ( -1.033464566929134687, -0.06523048226347956391, 0.5585629921259840369 ) ) ;
#11109 = CARTESIAN_POINT ( 'NONE',  ( -0.6971942568897648851, 0.07405724077823318263, 1.062992125930488418 ) ) ;
#11110 = EDGE_CURVE ( 'NONE', #18657, #23237, #11395, .T. ) ;
#11111 = CARTESIAN_POINT ( 'NONE',  ( 0.1571168540704948324, 0.1082847392564992711, -0.09327620385769608280 ) ) ;
#11112 = CARTESIAN_POINT ( 'NONE',  ( -0.2360031691064421178, -0.1592377390491987732, -0.08759220388363096743 ) ) ;
#11113 = CARTESIAN_POINT ( 'NONE',  ( 1.002407869896990045, -0.1264236179284866091, 0.2583661416785200671 ) ) ;
#11114 = CARTESIAN_POINT ( 'NONE',  ( -0.9500414927467377701, 0.1787899950787401604, 0.2263779527021421711 ) ) ;
#11115 = PRODUCT_DEFINITION_CONTEXT ( 'detailed design', #26947, 'design' ) ;
#11116 = CARTESIAN_POINT ( 'NONE',  ( -0.6971942568897626646, 0.07405724077823318263, 0.7086614172690703928 ) ) ;
#11117 = VERTEX_POINT ( 'NONE', #11638 ) ;
#11118 = EDGE_CURVE ( 'NONE', #32266, #44909, #39890, .T. ) ;
#11119 = CARTESIAN_POINT ( 'NONE',  ( -0.1787899950787401882, 0.07332677170730689253, 0.000000000000000000 ) ) ;
#11120 = ORIENTED_EDGE ( 'NONE', *, *, #13125, .T. ) ;
#11121 = CARTESIAN_POINT ( 'NONE',  ( 0.6971942568897626646, -0.07405724077823297447, 0.7972440944344250102 ) ) ;
#11122 = EDGE_CURVE ( 'NONE', #30632, #27780, #41769, .T. ) ;
#11123 = CARTESIAN_POINT ( 'NONE',  ( 0.7495606340400177148, 0.1264236179284866091, 1.065452755851747924 ) ) ;
#11124 = CARTESIAN_POINT ( 'NONE',  ( -1.002407869896990045, 0.1264236179284866091, 1.877460629867496067 ) ) ;
#11125 = ORIENTED_EDGE ( 'NONE', *, *, #24244, .T. ) ;
#11126 = DIRECTION ( 'NONE',  ( 0.000000000000000000, -0.7880107536067197938, 0.6156614753256609562 ) ) ;
#11127 = CARTESIAN_POINT ( 'NONE',  ( 0.07405724077823318263, -1.263903495788293307, 0.1787899950787401604 ) ) ;
#11128 = VERTEX_POINT ( 'NONE', #5126 ) ;
#11129 = CARTESIAN_POINT ( 'NONE',  ( 0.07405724077823318263, -0.2096456692375751329, -0.1787899950787401604 ) ) ;
#11130 = ORIENTED_EDGE ( 'NONE', *, *, #20351, .F. ) ;
#11131 = CARTESIAN_POINT ( 'NONE',  ( 0.8019270111902717657, 0.1787899950787401604, 1.215551181048599272 ) ) ;
#11132 = FACE_OUTER_BOUND ( 'NONE', #12538, .T. ) ;
#11133 = CARTESIAN_POINT ( 'NONE',  ( -0.2471904733176818747, -0.07069887449061568185, 0.09042980707098648152 ) ) ;
#11134 = CARTESIAN_POINT ( 'NONE',  ( 0.9500414927467378812, -0.1787899950787401604, 0.09350393695411057804 ) ) ;
#11135 = CONICAL_SURFACE ( 'NONE', #2684, 0.09842519685039370636, 0.9599310885968824758 ) ;
#11136 = VECTOR ( 'NONE', #31000, 39.37007874015748854 ) ;
#11137 = AXIS2_PLACEMENT_3D ( 'NONE', #4665, #11189, #18583 ) ;
#11138 = CARTESIAN_POINT ( 'NONE',  ( 0.07405724077823318263, -1.681102362150960650, 0.1787899950787401604 ) ) ;
#11139 = CARTESIAN_POINT ( 'NONE',  ( -0.9500414927467377701, -0.1787899950787401604, 0.5708661416785200116 ) ) ;
#11140 = CARTESIAN_POINT ( 'NONE',  ( 0.3547871005709968273, -0.09842519685039370636, 1.205361022782828805E-17 ) ) ;
#11141 = CARTESIAN_POINT ( 'NONE',  ( -0.07444174185955065859, -1.489709163913754075, 0.1797182628040039087 ) ) ;
#11142 = CARTESIAN_POINT ( 'NONE',  ( 0.000000000000000000, 0.000000000000000000, -0.3001770169643759867 ) ) ;
#11143 = CARTESIAN_POINT ( 'NONE',  ( 1.054774247047244540, -0.07405724077823318263, 1.284448818843874740 ) ) ;
#11144 = CARTESIAN_POINT ( 'NONE',  ( 0.9500414927467377701, 0.1787899950787401604, 1.643700787347811998 ) ) ;
#11145 = FACE_OUTER_BOUND ( 'NONE', #4052, .T. ) ;
#11146 = CARTESIAN_POINT ( 'NONE',  ( 0.7185039370078739607, 1.928577636452523993E-17, 0.8858267715460158565 ) ) ;
#11147 = CARTESIAN_POINT ( 'NONE',  ( 0.5555748031496083872, 0.1864803149606321375, 0.7480314960629921295 ) ) ;
#11148 = CARTESIAN_POINT ( 'NONE',  ( -0.7185039370078739607, 1.928577636452523993E-17, 0.6496062991050708391 ) ) ;
#11149 = LINE ( 'NONE', #11382, #33901 ) ;
#11150 = CARTESIAN_POINT ( 'NONE',  ( 1.002407869896990045, 0.1264236179284866091, 0.2632874015210397434 ) ) ;
#11151 = SHAPE_REPRESENTATION ( 'Hook Bracket', ( #20860 ), #31601 ) ;
#11152 = CARTESIAN_POINT ( 'NONE',  ( 0.7021184280059326044, 0.02911167292124897457, 0.03937009334504424501 ) ) ;
#11154 = DIRECTION ( 'NONE',  ( -0.000000000000000000, 1.000000000000000000, -3.995705278811693553E-31 ) ) ;
#11153 = CARTESIAN_POINT ( 'NONE',  ( 0.6971942568897648851, 0.07405724077823318263, 1.259842519631276359 ) ) ;
#11155 = CARTESIAN_POINT ( 'NONE',  ( 0.5660731898098425585, -3.032960542342102697E-32, 0.09842519685039370636 ) ) ;
#11156 = CARTESIAN_POINT ( 'NONE',  ( -0.7185039370078739607, 1.928577636452523993E-17, 1.053149606299212504 ) ) ;
#11157 = CARTESIAN_POINT ( 'NONE',  ( -0.9500414927467378812, 0.1787899950787401604, 1.249999999946235896 ) ) ;
#11158 = CARTESIAN_POINT ( 'NONE',  ( 0.8759842519685039353, -0.1574803149606299191, 0.6200787400499527813 ) ) ;
#11159 = ORIENTED_EDGE ( 'NONE', *, *, #12423, .F. ) ;
#11160 = DIRECTION ( 'NONE',  ( 7.051687499798870116E-15, 0.000000000000000000, 1.000000000000000000 ) ) ;
#11161 = CARTESIAN_POINT ( 'NONE',  ( 0.9647019635636798762, 0.1432196322012359857, 0.03937007870177667429 ) ) ;
#11162 = CARTESIAN_POINT ( 'NONE',  ( 0.9412147342319837628, 0.1574803149606300301, 0.8341535431995593664 ) ) ;
#11163 = CARTESIAN_POINT ( 'NONE',  ( -0.7646288533564489232, 0.1113553986120547346, 1.117125984144440975 ) ) ;
#11164 = CARTESIAN_POINT ( 'NONE',  ( 0.6971942568897648851, -0.07405724077823297447, 1.500984251914741607 ) ) ;
#11165 = CARTESIAN_POINT ( 'NONE',  ( -0.8759842519685039353, -0.1574803149606299191, 1.141732283464567121 ) ) ;
#11166 = AXIS2_PLACEMENT_3D ( 'NONE', #16288, #27331, #10988 ) ;
#11167 = EDGE_CURVE ( 'NONE', #31032, #13663, #4277, .T. ) ;
#11168 = DIRECTION ( 'NONE',  ( -1.000000000000000000, 0.000000000000000000, 0.000000000000000000 ) ) ;
#11170 = CARTESIAN_POINT ( 'NONE',  ( -0.7185039370078739607, 1.928577636452523993E-17, 0.1082677165354330728 ) ) ;
#11169 = DIRECTION ( 'NONE',  ( -1.000000000000000000, 0.000000000000000000, 0.000000000000000000 ) ) ;
#11171 = CARTESIAN_POINT ( 'NONE',  ( 0.1264236179284866091, -0.2219488188438744347, 0.1264236179284866091 ) ) ;
#11172 = ORIENTED_EDGE ( 'NONE', *, *, #44084, .F. ) ;
#11173 = CARTESIAN_POINT ( 'NONE',  ( 0.7646288533564489232, -0.1113553986120547346, 0.6545275589475906264 ) ) ;
#11174 = EDGE_CURVE ( 'NONE', #37198, #21900, #44042, .T. ) ;
#11175 = CARTESIAN_POINT ( 'NONE',  ( -0.8759842519685039353, 0.000000000000000000, 0.000000000000000000 ) ) ;
#11176 = ORIENTED_EDGE ( 'NONE', *, *, #19700, .F. ) ;
#11177 = CARTESIAN_POINT ( 'NONE',  ( 0.7495606340400177148, -0.1264236179284866091, 0.6028543306548976854 ) ) ;
#11179 = EDGE_CURVE ( 'NONE', #4869, #23841, #37321, .T. ) ;
#11178 = ORIENTED_EDGE ( 'NONE', *, *, #19255, .T. ) ;
#11180 = CARTESIAN_POINT ( 'NONE',  ( -0.8019270111902716547, -0.1787899950787401604, 1.466535433017102763 ) ) ;
#11181 = CARTESIAN_POINT ( 'NONE',  ( -0.07405724077823318263, -1.809055118056471123, 0.1787899950787401604 ) ) ;
#11182 = CARTESIAN_POINT ( 'NONE',  ( -0.6971942568897648851, -0.07405724077823297447, 1.190944881836001112 ) ) ;
#11183 = AXIS2_PLACEMENT_3D ( 'NONE', #42840, #14124, #10051 ) ;
#11184 = EDGE_LOOP ( 'NONE', ( #23702, #19395, #18389, #40318, #47287, #19417, #32843, #3044, #23834, #37581, #10764, #16990 ) ) ;
#11185 = CARTESIAN_POINT ( 'NONE',  ( 0.7185039370078739607, 1.928577636452523993E-17, 1.318897637687747926 ) ) ;
#11186 = ADVANCED_FACE ( 'NONE', ( #26498 ), #45135, .T. ) ;
#11187 = CARTESIAN_POINT ( 'NONE',  ( -1.002407869896990045, 0.1264236179284866091, 0.8193897637257637756 ) ) ;
#11188 = CARTESIAN_POINT ( 'NONE',  ( -0.6971942568897626646, -0.07405724077823297447, 0.2066929133320631329 ) ) ;
#11189 = DIRECTION ( 'NONE',  ( 0.000000000000000000, -1.000000000000000000, -0.000000000000000000 ) ) ;
#11190 = CARTESIAN_POINT ( 'NONE',  ( 0.8107537697050254399, 0.1574803149606300301, 0.7997047243019207441 ) ) ;
#11191 = CARTESIAN_POINT ( 'NONE',  ( -0.07405724077823318263, -0.8111475902764821999, -0.1787899950787401604 ) ) ;
#11192 = VERTEX_POINT ( 'NONE', #37494 ) ;
#11193 = CARTESIAN_POINT ( 'NONE',  ( 0.8759842519685039353, -0.1574803149606299191, 1.062992125984252079 ) ) ;
#11194 = EDGE_LOOP ( 'NONE', ( #31584, #40026, #5957, #2102 ) ) ;
#11195 = ORIENTED_EDGE ( 'NONE', *, *, #10842, .F. ) ;
#11196 = CARTESIAN_POINT ( 'NONE',  ( 0.9873396505805591694, -0.1113553986120547346, 1.215551180994834723 ) ) ;
#11197 = CARTESIAN_POINT ( 'NONE',  ( -1.002407869896990045, 0.1264236179284866091, 0.8144685038832440993 ) ) ;
#11198 = AXIS2_PLACEMENT_3D ( 'NONE', #43488, #21211, #28439 ) ;
#11199 = CARTESIAN_POINT ( 'NONE',  ( -0.1787899950787401882, -0.4778543306548976854, 0.000000000000000000 ) ) ;
#11200 = CARTESIAN_POINT ( 'NONE',  ( -1.054774247047244096, 0.000000000000000000, 0.1058070865604096300 ) ) ;
#11201 = CARTESIAN_POINT ( 'NONE',  ( 0.1270800023317771588, -0.9213036521027303527, -0.1270800023317771588 ) ) ;
#11202 = CARTESIAN_POINT ( 'NONE',  ( 0.06453057165843432974, -0.2582375021999246956, -0.3090319486758518197 ) ) ;
#11203 = CARTESIAN_POINT ( 'NONE',  ( -0.9873396505805591694, 0.1113553986120547346, 1.579724409341291214 ) ) ;
#11204 = CARTESIAN_POINT ( 'NONE',  ( 1.054774247047244540, 0.07405724077823318263, 0.6988188975840318173 ) ) ;
#11205 = CARTESIAN_POINT ( 'NONE',  ( 0.9500414927467377701, 0.1787899950787401604, 1.328740157426552049 ) ) ;
#11206 = CARTESIAN_POINT ( 'NONE',  ( 0.1574803149606299746, 0.08719492171395763769, -0.5641677032617172793 ) ) ;
#11207 = CARTESIAN_POINT ( 'NONE',  ( 0.9873396505805591694, -0.1113553986120547346, 1.382874015748031704 ) ) ;
#11209 = DIRECTION ( 'NONE',  ( -0.000000000000000000, -0.6156614753256575145, -0.7880107536067225693 ) ) ;
#11208 = CARTESIAN_POINT ( 'NONE',  ( 0.8128431167288246995, -0.1605282852710551433, 1.987016390083011785 ) ) ;
#11210 = CARTESIAN_POINT ( 'NONE',  ( 0.7646288533564489232, 0.1113553986120547346, 0.3297244093412917687 ) ) ;
#11211 = CARTESIAN_POINT ( 'NONE',  ( -0.1113553986120547346, -0.6525590550105826448, -0.1113553986120547346 ) ) ;
#11213 = CARTESIAN_POINT ( 'NONE',  ( 0.03171094329963846520, 0.3740157480314960647, 1.099466564236704746 ) ) ;
#11212 = CARTESIAN_POINT ( 'NONE',  ( 0.8019270111902716547, -0.1787899950787401604, 0.8759842519147408302 ) ) ;
#11214 = CARTESIAN_POINT ( 'NONE',  ( -0.07405724077823318263, -0.8346456692375755493, -0.1787899950787401604 ) ) ;
#11215 = DIRECTION ( 'NONE',  ( -1.000000000000000000, 3.469446951953613794E-15, 1.144917494144692682E-16 ) ) ;
#11216 = CARTESIAN_POINT ( 'NONE',  ( 0.003583035186807825324, -0.1402401972141327779, 0.03270545601322783630 ) ) ;
#11217 = CARTESIAN_POINT ( 'NONE',  ( 1.054774247047244540, -0.07405724077823318263, 0.9645669290800953366 ) ) ;
#11218 = CARTESIAN_POINT ( 'NONE',  ( 0.3246033735368759610, 4.766607801171850497E-17, 0.000000000000000000 ) ) ;
#11219 = CARTESIAN_POINT ( 'NONE',  ( -0.1574803149606299191, -1.641732283464567121, 0.000000000000000000 ) ) ;
#11220 = CARTESIAN_POINT ( 'NONE',  ( 0.8070866141732283561, 0.000000000000000000, 0.8559055118110230342 ) ) ;
#11221 = ADVANCED_FACE ( 'NONE', ( #41058 ), #19033, .F. ) ;
#11222 = ORIENTED_EDGE ( 'NONE', *, *, #39112, .T. ) ;
#11223 = DIRECTION ( 'NONE',  ( -1.000000000000000000, 0.000000000000000000, 0.000000000000000000 ) ) ;
#11224 = CARTESIAN_POINT ( 'NONE',  ( -0.8759842519685039353, -0.1787899950787401882, 0.1304133857730082613 ) ) ;
#11225 = ORIENTED_EDGE ( 'NONE', *, *, #35353, .F. ) ;
#11226 = CARTESIAN_POINT ( 'NONE',  ( 1.033464566929134687, 0.06523048226347956391, 0.3272637795275590289 ) ) ;
#11228 = CARTESIAN_POINT ( 'NONE',  ( 0.1787899950787401882, -1.442421259788756016, -2.189545951927503898E-17 ) ) ;
#11227 = CARTESIAN_POINT ( 'NONE',  ( -0.1574803149606299191, -0.2933070865066460531, 0.000000000000000000 ) ) ;
#11229 = CARTESIAN_POINT ( 'NONE',  ( -0.9500414927467378812, -0.1787899950787401604, 1.668307086560410157 ) ) ;
#11230 = CARTESIAN_POINT ( 'NONE',  ( -0.9500414927467377701, 0.1787899950787401604, 0.8956692912848198684 ) ) ;
#11231 = EDGE_CURVE ( 'NONE', #33230, #22586, #27294, .T. ) ;
#11232 = CARTESIAN_POINT ( 'NONE',  ( -1.054774247047244096, 0.000000000000000000, 0.3813976377415121966 ) ) ;
#11233 = CARTESIAN_POINT ( 'NONE',  ( -0.8759842519685039353, -0.1574803149606299191, 0.1574803149606299191 ) ) ;
#11234 = CARTESIAN_POINT ( 'NONE',  ( 0.3302522695077432791, 4.466152701071653354E-17, 0.000000000000000000 ) ) ;
#11235 = CARTESIAN_POINT ( 'NONE',  ( 0.05473164110560585494, 0.07681961335491396814, -0.2538337431406301747 ) ) ;
#11236 = CARTESIAN_POINT ( 'NONE',  ( -0.2645270498714851204, 0.1617305326345083449, -0.8316512675465659310 ) ) ;
#11237 = CARTESIAN_POINT ( 'NONE',  ( -0.1787899950787401604, -0.4076042831898689656, 0.07405724077823318263 ) ) ;
#11238 = CARTESIAN_POINT ( 'NONE',  ( -0.1791659572252606303, -0.08955948998496260360, -0.1686289933158019450 ) ) ;
#11239 = DIRECTION ( 'NONE',  ( 0.000000000000000000, 0.000000000000000000, 1.000000000000000000 ) ) ;
#11240 = LINE ( 'NONE', #29010, #33309 ) ;
#11241 = CARTESIAN_POINT ( 'NONE',  ( -0.8019270111902717657, 0.1787899950787401604, 0.2706692912848194243 ) ) ;
#11242 = ORIENTED_EDGE ( 'NONE', *, *, #33628, .T. ) ;
#11243 = CARTESIAN_POINT ( 'NONE',  ( 0.8759842519685039353, 0.1574803149606299191, 0.8070866141732283561 ) ) ;
#11244 = VERTEX_POINT ( 'NONE', #1293 ) ;
#11245 = CARTESIAN_POINT ( 'NONE',  ( -0.7495606340400177148, 0.1264236179284866091, 1.419783464513165505 ) ) ;
#11246 = VERTEX_POINT ( 'NONE', #15949 ) ;
#11247 = CARTESIAN_POINT ( 'NONE',  ( 0.1787899950787401882, -1.403051181048598384, -2.189545951927503898E-17 ) ) ;
#11248 = EDGE_CURVE ( 'NONE', #30530, #1000, #6106, .T. ) ;
#11249 = CARTESIAN_POINT ( 'NONE',  ( 0.1264236179284866091, -1.442421259788756016, 0.1264236179284866091 ) ) ;
#11250 = LINE ( 'NONE', #29964, #7197 ) ;
#11251 = CARTESIAN_POINT ( 'NONE',  ( 1.033464566929134687, 0.06523048226347956391, 0.4060039370078741272 ) ) ;
#11252 = CARTESIAN_POINT ( 'NONE',  ( 0.1797182628040039365, -0.6112642820239901909, -2.200913952912460540E-17 ) ) ;
#11253 = LINE ( 'NONE', #8107, #4089 ) ;
#11254 = CARTESIAN_POINT ( 'NONE',  ( -0.7185039370078739607, 1.928577636452523993E-17, 1.003937007766488199 ) ) ;
#11255 = DIRECTION ( 'NONE',  ( 0.000000000000000000, 0.000000000000000000, -1.000000000000000000 ) ) ;
#11256 = CARTESIAN_POINT ( 'NONE',  ( -9.642888182262618425E-18, -0.2342519685039370358, -0.1574803149606299191 ) ) ;
#11257 = CARTESIAN_POINT ( 'NONE',  ( 0.8759842519685039353, -0.1574803149606299191, 1.919291338475149544 ) ) ;
#11258 = ORIENTED_EDGE ( 'NONE', *, *, #40650, .T. ) ;
#11259 = CARTESIAN_POINT ( 'NONE',  ( -0.07405724077823318263, -0.1948818897100161873, 0.1787899950787401604 ) ) ;
#11260 = CARTESIAN_POINT ( 'NONE',  ( -0.7185039370078692977, 0.06523048226347515077, 1.434547243986962428 ) ) ;
#11261 = CARTESIAN_POINT ( 'NONE',  ( 0.9412147342319837628, 0.1574803149606300301, 0.9621062992125994917 ) ) ;
#11262 = CARTESIAN_POINT ( 'NONE',  ( -0.1574803149606299191, 1.928577636452524610E-17, -0.3149606299212598381 ) ) ;
#11264 = LINE ( 'NONE', #44761, #28486 ) ;
#11263 = CARTESIAN_POINT ( 'NONE',  ( -0.7185039370078739607, 1.928577636452523993E-17, 0.4625984251968504046 ) ) ;
#11265 = FACE_BOUND ( 'NONE', #46562, .T. ) ;
#11266 = EDGE_LOOP ( 'NONE', ( #34335, #4281, #26980, #17591 ) ) ;
#11267 = ADVANCED_FACE ( 'NONE', ( #37252, #808 ), #16642, .T. ) ;
#11268 = DIRECTION ( 'NONE',  ( 1.000000000000000000, 0.000000000000000000, 0.000000000000000000 ) ) ;
#11269 = CARTESIAN_POINT ( 'NONE',  ( 0.1574803149606299191, 0.000000000000000000, 0.2952755905511810774 ) ) ;
#11270 = CARTESIAN_POINT ( 'NONE',  ( 0.07405724077823318263, -1.602362204670647161, 0.1787899950787401604 ) ) ;
#11271 = CARTESIAN_POINT ( 'NONE',  ( -0.1574803149606300301, -1.516240157372787944, -0.06523048226347956391 ) ) ;
#11272 = CARTESIAN_POINT ( 'NONE',  ( -9.642888182262618425E-18, -1.139763779527559029, -0.1574803149606299191 ) ) ;
#11273 = CARTESIAN_POINT ( 'NONE',  ( 0.9873396505805591694, -0.1113553986120547346, 0.9005905510735748853 ) ) ;
#11274 = FACE_OUTER_BOUND ( 'NONE', #18877, .T. ) ;
#11275 = EDGE_CURVE ( 'NONE', #21453, #25294, #22792, .T. ) ;
#11276 = CARTESIAN_POINT ( 'NONE',  ( -0.8759842519685039353, -0.1787899950787401882, 0.3666338582139531677 ) ) ;
#11277 = ORIENTED_EDGE ( 'NONE', *, *, #22465, .F. ) ;
#11278 = VERTEX_POINT ( 'NONE', #35333 ) ;
#11279 = VERTEX_POINT ( 'NONE', #20461 ) ;
#11280 = CARTESIAN_POINT ( 'NONE',  ( -0.7495606340400177148, 0.1264236179284866091, 1.616633858213952779 ) ) ;
#11281 = CARTESIAN_POINT ( 'NONE',  ( 0.8759842519685039353, 0.1787899950787401882, 1.651082677111590513 ) ) ;
#11282 = VERTEX_POINT ( 'NONE', #20925 ) ;
#11283 = CARTESIAN_POINT ( 'NONE',  ( 0.1113553986120547346, -1.341535432963338437, 0.1113553986120547346 ) ) ;
#11284 = CARTESIAN_POINT ( 'NONE',  ( -0.6971942568897626646, -0.07405724077823297447, 0.8759842519147408302 ) ) ;
#11285 = DIRECTION ( 'NONE',  ( -1.000000000000000000, 0.000000000000000000, 0.000000000000000000 ) ) ;
#11286 = CARTESIAN_POINT ( 'NONE',  ( -0.8759842519685039353, -0.1787899950787401882, 1.272145669237574772 ) ) ;
#11287 = CARTESIAN_POINT ( 'NONE',  ( -1.002407869896990045, 0.1264236179284866091, 0.7750984251430865779 ) ) ;
#11288 = CARTESIAN_POINT ( 'NONE',  ( 1.033464566929134687, 0.06523048226347956391, 0.9079724408373541777 ) ) ;
#11289 = CARTESIAN_POINT ( 'NONE',  ( 0.05769625742918475797, 0.07859832706092276244, 0.2521221211081680624 ) ) ;
#11290 = CARTESIAN_POINT ( 'NONE',  ( -0.9500414927467378812, -0.1787899950787401604, 1.594488188922613237 ) ) ;
#11291 = CARTESIAN_POINT ( 'NONE',  ( -0.7185039370078739607, 1.928577636452523993E-17, 1.830708661309795149 ) ) ;
#11292 = ORIENTED_EDGE ( 'NONE', *, *, #7894, .T. ) ;
#11293 = CARTESIAN_POINT ( 'NONE',  ( -0.9873396505805591694, 0.1113553986120547346, 1.628937007874015963 ) ) ;
#11294 = CARTESIAN_POINT ( 'NONE',  ( 0.1776748150188054431, -0.4231595423373736287, -0.9814026967226106013 ) ) ;
#11295 = CARTESIAN_POINT ( 'NONE',  ( 0.6971942568897648851, -0.07405724077823297447, 1.387795275536786610 ) ) ;
#11296 = DIRECTION ( 'NONE',  ( 2.775557561562890735E-17, -0.6156614753256639538, -0.7880107536067174623 ) ) ;
#11297 = ORIENTED_EDGE ( 'NONE', *, *, #46777, .F. ) ;
#11298 = ( BOUNDED_CURVE ( )  B_SPLINE_CURVE ( 2, ( #23091, #37709, #26943, #34137, #43588, #35941, #17958, #28542, #2850 ),
 .UNSPECIFIED., .F., .T. ) 
 B_SPLINE_CURVE_WITH_KNOTS ( ( 3, 2, 2, 2, 3 ),
 ( 0.7900000000000000355, 0.7924999999999999822, 0.7950000000000000400, 0.7974999999999999867, 0.8000000000000000444 ),
 .UNSPECIFIED. ) 
 CURVE ( )  GEOMETRIC_REPRESENTATION_ITEM ( )  RATIONAL_B_SPLINE_CURVE ( ( 1.000000000000000000, 0.9238795325112899581, 1.000000000000000000, 0.9238795325112869605, 1.000000000000000000, 0.9238795325112869605, 1.000000000000000000, 0.9238795325112869605, 1.000000000000000000 ) ) 
 REPRESENTATION_ITEM ( '' )  ) ;
#11299 = ORIENTED_EDGE ( 'NONE', *, *, #12527, .F. ) ;
#11300 = CARTESIAN_POINT ( 'NONE',  ( -0.1787899950787401604, -0.6722440944344262315, -0.07405724077823318263 ) ) ;
#11301 = VERTEX_POINT ( 'NONE', #2474 ) ;
#11302 = CARTESIAN_POINT ( 'NONE',  ( -0.07405724077823318263, -0.9429133857730090940, 0.1787899950787401604 ) ) ;
#11303 = ADVANCED_FACE ( 'NONE', ( #38442 ), #39365, .F. ) ;
#11304 = CARTESIAN_POINT ( 'NONE',  ( -0.1264236179284866091, -0.4434055117572598959, -0.1264236179284866091 ) ) ;
#11305 = CARTESIAN_POINT ( 'NONE',  ( 0.1787899950787401882, -0.9650590550643465271, -2.189545951927503898E-17 ) ) ;
#11306 = DIRECTION ( 'NONE',  ( 1.822029033848725028E-16, 0.000000000000000000, 1.000000000000000000 ) ) ;
#11307 = LENGTH_MEASURE_WITH_UNIT ( LENGTH_MEASURE( 0.02539999999999999897 ), #25460 ) ;
#11308 = CARTESIAN_POINT ( 'NONE',  ( 0.1270800023317771588, -0.1437445969846202765, 0.1270800023317771588 ) ) ;
#11309 = CARTESIAN_POINT ( 'NONE',  ( -0.1574803149606300301, 0.1668307086614173873, -0.06523048226347956391 ) ) ;
#11310 = CARTESIAN_POINT ( 'NONE',  ( 0.1264236179284866091, -0.1087598424659214497, 0.1264236179284866091 ) ) ;
#11311 = CARTESIAN_POINT ( 'NONE',  ( 0.2471922763370229259, -0.09254788073173002283, -0.04110581524678511012 ) ) ;
#11312 = CARTESIAN_POINT ( 'NONE',  ( 0.9500414927467378812, 0.1787899950787401604, 0.7381889763241898939 ) ) ;
#11313 = CIRCLE ( 'NONE', #6675, 0.09842519685039310962 ) ;
#11314 = ( BOUNDED_CURVE ( )  B_SPLINE_CURVE ( 2, ( #6198, #13634, #28761, #10533, #24902, #25130, #6906, #36166, #13873 ),
 .UNSPECIFIED., .F., .T. ) 
 B_SPLINE_CURVE_WITH_KNOTS ( ( 3, 2, 2, 2, 3 ),
 ( 0.9499999999999999556, 0.9525000000000000133, 0.9549999999999999600, 0.9575000000000000178, 0.9599999999999999645 ),
 .UNSPECIFIED. ) 
 CURVE ( )  GEOMETRIC_REPRESENTATION_ITEM ( )  RATIONAL_B_SPLINE_CURVE ( ( 1.000000000000000000, 0.9238795325112899581, 1.000000000000000000, 0.9238795325112869605, 1.000000000000000000, 0.9238795325112869605, 1.000000000000000000, 0.9238795325112869605, 1.000000000000000000 ) ) 
 REPRESENTATION_ITEM ( '' )  ) ;
#11316 = CARTESIAN_POINT ( 'NONE',  ( 1.033464566929133799, 0.000000000000000000, 1.338582677057826853 ) ) ;
#11315 = FACE_OUTER_BOUND ( 'NONE', #43752, .T. ) ;
#11318 = DIRECTION ( 'NONE',  ( 0.000000000000000000, 0.000000000000000000, -1.000000000000000000 ) ) ;
#11317 = DIRECTION ( 'NONE',  ( 0.000000000000000000, 0.000000000000000000, 1.000000000000000000 ) ) ;
#11319 = CARTESIAN_POINT ( 'NONE',  ( -0.7185039370078739607, 1.928577636452523993E-17, 1.043307086506645831 ) ) ;
#11320 = CARTESIAN_POINT ( 'NONE',  ( 0.7495606340400177148, -0.1264236179284866091, 1.902066929080094448 ) ) ;
#11322 = CARTESIAN_POINT ( 'NONE',  ( 0.9412147342319837628, -0.1574803149606297803, 1.882381889656251639 ) ) ;
#11321 = CYLINDRICAL_SURFACE ( 'NONE', #23775, 0.1574803149606299191 ) ;
#11323 = EDGE_CURVE ( 'NONE', #15970, #40728, #4554, .T. ) ;
#11324 = VERTEX_POINT ( 'NONE', #34867 ) ;
#11325 = CARTESIAN_POINT ( 'NONE',  ( -1.033464566929133799, 1.928577636452524610E-17, 2.869337061179095023E-17 ) ) ;
#11326 = CARTESIAN_POINT ( 'NONE',  ( 0.1264236179284866091, -0.3056102361667090705, 0.1264236179284866091 ) ) ;
#11327 = FACE_OUTER_BOUND ( 'NONE', #35326, .T. ) ;
#11328 = CARTESIAN_POINT ( 'NONE',  ( -0.1264236179284866091, -1.147145669237574772, -0.1264236179284866091 ) ) ;
#11329 = CARTESIAN_POINT ( 'NONE',  ( 0.9500414927467378812, -0.1787899950787401604, 0.2559055117572600624 ) ) ;
#11330 = CARTESIAN_POINT ( 'NONE',  ( 0.1620125769272121319, 0.07969870020048158699, -0.1380420919957745518 ) ) ;
#11331 = CARTESIAN_POINT ( 'NONE',  ( 1.054774247047244096, 0.000000000000000000, 0.5733267715997795166 ) ) ;
#11332 = EDGE_CURVE ( 'NONE', #2870, #35775, #2242, .T. ) ;
#11333 = CARTESIAN_POINT ( 'NONE',  ( -1.054774247047244540, -0.07405724077823318263, 1.555118110182455382 ) ) ;
#11334 = ORIENTED_EDGE ( 'NONE', *, *, #21603, .F. ) ;
#11335 = FACE_OUTER_BOUND ( 'NONE', #21755, .T. ) ;
#11336 = APPLICATION_CONTEXT ( 'automotive_design' ) ;
#11337 = CARTESIAN_POINT ( 'NONE',  ( 0.8759842519685039353, -0.1787899950787401882, 1.277066929080094448 ) ) ;
#11338 = CARTESIAN_POINT ( 'NONE',  ( 0.8759842519685039353, 0.1787899950787401882, 0.03690944876513417572 ) ) ;
#11339 = CARTESIAN_POINT ( 'NONE',  ( -1.054774247047244540, -0.07405724077823318263, 1.043307086560409269 ) ) ;
#11340 = CARTESIAN_POINT ( 'NONE',  ( -0.2170082705494138786, -0.1702044488443286430, -0.06846571731941632211 ) ) ;
#11341 = CARTESIAN_POINT ( 'NONE',  ( 0.7495606340400177148, 0.1264236179284866091, 0.4355314960092284138 ) ) ;
#11342 = CARTESIAN_POINT ( 'NONE',  ( -0.6971942568897626646, -0.07405724077823297447, 0.2411417322297010890 ) ) ;
#11343 = EDGE_CURVE ( 'NONE', #7779, #20929, #43474, .T. ) ;
#11344 = CARTESIAN_POINT ( 'NONE',  ( -0.7495606340400177148, -0.1264236179284866091, 0.7160433070328504623 ) ) ;
#11345 = CARTESIAN_POINT ( 'NONE',  ( 0.8759842519685039353, -0.1574803149606299191, 1.722440944774362270 ) ) ;
#11346 = ORIENTED_EDGE ( 'NONE', *, *, #38952, .T. ) ;
#11347 = ADVANCED_FACE ( 'NONE', ( #35567 ), #13982, .F. ) ;
#11348 = AXIS2_PLACEMENT_3D ( 'NONE', #33797, #7880, #15576 ) ;
#11349 = CARTESIAN_POINT ( 'NONE',  ( -0.7646288533564489232, 0.1113553986120547346, 1.363188976377952999 ) ) ;
#11350 = CARTESIAN_POINT ( 'NONE',  ( 1.054774247047244096, 0.000000000000000000, 1.129429133804503937 ) ) ;
#11351 = CARTESIAN_POINT ( 'NONE',  ( -0.8019270111902716547, 0.1787899950787401604, 1.845472440891119392 ) ) ;
#11352 = ORIENTED_EDGE ( 'NONE', *, *, #43378, .F. ) ;
#11353 = CARTESIAN_POINT ( 'NONE',  ( 1.002407869896990045, 0.1264236179284866091, 1.916830708607653477 ) ) ;
#11354 = CIRCLE ( 'NONE', #5962, 0.1864803149606299448 ) ;
#11355 = DIRECTION ( 'NONE',  ( 1.822029033848725028E-16, 0.000000000000000000, 1.000000000000000000 ) ) ;
#11356 = CARTESIAN_POINT ( 'NONE',  ( 0.07405724077823318263, -1.524730267441837483, -0.1787899950787401604 ) ) ;
#11357 = ORIENTED_EDGE ( 'NONE', *, *, #33834, .T. ) ;
#11358 = CARTESIAN_POINT ( 'NONE',  ( 0.07405724077823318263, -0.3277559054580475584, -0.1787899950787401604 ) ) ;
#11359 = CARTESIAN_POINT ( 'NONE',  ( -0.3094241246319155980, -0.02236840013889274115, 0.7097937670812509703 ) ) ;
#11360 = ORIENTED_EDGE ( 'NONE', *, *, #36047, .T. ) ;
#11361 = CARTESIAN_POINT ( 'NONE',  ( 0.8759842519685039353, 0.1787899950787401882, 1.252460629867496067 ) ) ;
#11362 = FACE_OUTER_BOUND ( 'NONE', #10886, .T. ) ;
#11363 = CARTESIAN_POINT ( 'NONE',  ( 0.001106411046829887477, -0.1060985490479111754, -0.09184399599051619456 ) ) ;
#11364 = CARTESIAN_POINT ( 'NONE',  ( 0.9500414927467378812, 0.1787899950787401604, 1.486220472387181690 ) ) ;
#11365 = CARTESIAN_POINT ( 'NONE',  ( 1.054774247047244096, 0.000000000000000000, 0.1796259841982051075 ) ) ;
#11366 = CARTESIAN_POINT ( 'NONE',  ( -1.094772975963752103E-17, -1.590059055064346305, -0.1787899950787401882 ) ) ;
#11367 = SHAPE_DEFINITION_REPRESENTATION ( #5938, #19102 ) ;
#11368 = ADVANCED_FACE ( 'NONE', ( #24768 ), #5853, .T. ) ;
#11369 = CARTESIAN_POINT ( 'NONE',  ( -1.002407869896990045, -0.1264236179284866091, 0.4552165353793071745 ) ) ;
#11370 = AXIS2_PLACEMENT_3D ( 'NONE', #39169, #38722, #17607 ) ;
#11372 = CARTESIAN_POINT ( 'NONE',  ( -0.7119983469427643152, -0.03169511975089377848, 1.983853482814432745 ) ) ;
#11371 = CARTESIAN_POINT ( 'NONE',  ( 0.1270800023317771588, -1.354374518244462422, -0.1270800023317771588 ) ) ;
#11373 = CARTESIAN_POINT ( 'NONE',  ( 0.7495606340400177148, -0.1264236179284866091, 1.429625984198204858 ) ) ;
#11374 = CARTESIAN_POINT ( 'NONE',  ( 1.002407869896990045, -0.1264236179284866091, 1.749507873961984483 ) ) ;
#11375 = ADVANCED_FACE ( 'NONE', ( #46330 ), #16862, .T. ) ;
#11376 = FACE_OUTER_BOUND ( 'NONE', #16173, .T. ) ;
#11377 = CARTESIAN_POINT ( 'NONE',  ( -0.07810294628632777347, 0.1299212598425197041, 0.1504079689250619467 ) ) ;
#11379 = CARTESIAN_POINT ( 'NONE',  ( -0.8084482433127401224, 0.1455052200007756480, 1.979717192799555825 ) ) ;
#11378 = CARTESIAN_POINT ( 'NONE',  ( -1.033464566929133799, 0.000000000000000000, 1.505905511811023612 ) ) ;
#11380 = CARTESIAN_POINT ( 'NONE',  ( 0.8759842519685039353, -0.1574803149606299191, 0.8169291337507401662 ) ) ;
#11381 = CARTESIAN_POINT ( 'NONE',  ( -0.7185039370078746268, -0.06523048226347956391, 1.921751968503937480 ) ) ;
#11382 = CARTESIAN_POINT ( 'NONE',  ( 0.1574803149606299191, 0.4668427075568346574, -0.7022306805398661478 ) ) ;
#11383 = CARTESIAN_POINT ( 'NONE',  ( 0.9500414927467378812, 0.1787899950787401604, 0.2657480314422993595 ) ) ;
#11384 = CARTESIAN_POINT ( 'NONE',  ( -1.033464566929133799, 0.000000000000000000, 1.702755905511810885 ) ) ;
#11385 = CARTESIAN_POINT ( 'NONE',  ( 1.284448818897637956, -0.3937007874015748254, -1.181102362204724310 ) ) ;
#11386 = CARTESIAN_POINT ( 'NONE',  ( 0.1968503937007874682, -1.308580299410598613, -1.920078980116132872 ) ) ;
#11387 = CARTESIAN_POINT ( 'NONE',  ( 1.033464566929133799, 0.000000000000000000, 0.7086614172153071767 ) ) ;
#11388 = VERTEX_POINT ( 'NONE', #17338 ) ;
#11389 = CARTESIAN_POINT ( 'NONE',  ( 0.9873396505805591694, 0.1113553986120547346, 1.392716535433070835 ) ) ;
#11390 = CARTESIAN_POINT ( 'NONE',  ( -0.2019004115846159131, -0.3515432751093511277, -1.037355456931929210 ) ) ;
#11391 = ORIENTED_EDGE ( 'NONE', *, *, #29238, .T. ) ;
#11392 = CARTESIAN_POINT ( 'NONE',  ( 0.7185039370078746268, -0.06523048226347956391, 0.2682086614173231909 ) ) ;
#11393 = CARTESIAN_POINT ( 'NONE',  ( -0.07444174185955065859, -0.008409951315329022153, -0.1797182628040039087 ) ) ;
#11394 = CARTESIAN_POINT ( 'NONE',  ( 1.054774247047244540, -0.07405724077823318263, 1.555118110182455382 ) ) ;
#11395 = LINE ( 'NONE', #15234, #20472 ) ;
#11396 = CARTESIAN_POINT ( 'NONE',  ( 0.1573602050224713056, -0.1351575695123996834, 0.04671412196467249894 ) ) ;
#11397 = CARTESIAN_POINT ( 'NONE',  ( 0.2759478392031630145, -0.09842519685039370636, 1.870565676741759775 ) ) ;
#11398 = CARTESIAN_POINT ( 'NONE',  ( 0.1264236179284866091, -0.1727362204186775607, -0.1264236179284866091 ) ) ;
#11399 = ORIENTED_EDGE ( 'NONE', *, *, #40917, .T. ) ;
#11400 = ADVANCED_FACE ( 'NONE', ( #9924 ), #24531, .F. ) ;
#11401 = DIRECTION ( 'NONE',  ( 1.822029033848725028E-16, 0.000000000000000000, 1.000000000000000000 ) ) ;
#11402 = CARTESIAN_POINT ( 'NONE',  ( 0.1888229765471286237, -0.07899262986800696662, -0.1764160547655181654 ) ) ;
#11403 = EDGE_LOOP ( 'NONE', ( #35721, #31288, #38159, #34983 ) ) ;
#11404 = CARTESIAN_POINT ( 'NONE',  ( 0.6971942568897637749, 2.189545951927499583E-17, 0.9128937007336377363 ) ) ;
#11405 = CARTESIAN_POINT ( 'NONE',  ( 0.1113553986120547346, 0.03641732294217271682, 0.1113553986120547346 ) ) ;
#11406 = CARTESIAN_POINT ( 'NONE',  ( -1.054774247047244096, 0.000000000000000000, 1.286909448765133801 ) ) ;
#11407 = ORIENTED_EDGE ( 'NONE', *, *, #15210, .F. ) ;
#11408 = CARTESIAN_POINT ( 'NONE',  ( -0.2559055118110236116, -0.08227967500866986694, -0.05504294401599051090 ) ) ;
#11409 = EDGE_CURVE ( 'NONE', #954, #25562, #2933, .T. ) ;
#11410 = DIRECTION ( 'NONE',  ( -1.000000000000000000, 0.000000000000000000, 0.000000000000000000 ) ) ;
#11411 = CARTESIAN_POINT ( 'NONE',  ( -0.1377952755905511861, -1.331775896911328393E-15, 0.8070866141732283561 ) ) ;
#11412 = CARTESIAN_POINT ( 'NONE',  ( 0.5415383587465882886, 4.466152701071653354E-17, 0.000000000000000000 ) ) ;
#11413 = CARTESIAN_POINT ( 'NONE',  ( 0.07405724077823318263, -0.8160688501190034305, -0.1787899950787401604 ) ) ;
#11414 = ORIENTED_EDGE ( 'NONE', *, *, #6259, .T. ) ;
#11415 = CYLINDRICAL_SURFACE ( 'NONE', #42497, 0.1003937007874010356 ) ;
#11416 = VERTEX_POINT ( 'NONE', #36732 ) ;
#11417 = DIRECTION ( 'NONE',  ( 1.822029033848725028E-16, 0.000000000000000000, 1.000000000000000000 ) ) ;
#11418 = CIRCLE ( 'NONE', #15256, 0.009842519685039369942 ) ;
#11419 = CARTESIAN_POINT ( 'NONE',  ( -1.054774247047244540, -0.07405724077823318263, 0.8070866141194653620 ) ) ;
#11420 = DIRECTION ( 'NONE',  ( -1.000000000000000000, -0.000000000000000000, 0.000000000000000000 ) ) ;
#11421 = CIRCLE ( 'NONE', #17526, 0.09842519685039370636 ) ;
#11422 = CARTESIAN_POINT ( 'NONE',  ( -0.9500414927467377701, -0.1787899950787401604, 1.830708661363559253 ) ) ;
#11423 = CARTESIAN_POINT ( 'NONE',  ( -0.1264236179284866091, -0.4827755904974173617, -0.1264236179284866091 ) ) ;
#11424 = EDGE_CURVE ( 'NONE', #25085, #29994, #3184, .T. ) ;
#11425 = ( BOUNDED_SURFACE ( )  B_SPLINE_SURFACE ( 1, 2, ( 
 ( #30718, #11309, #1207, #44571, #37888, #12258, #11542, #25923, #44810, #37166, #4551, #37644, #40505, #7931, #36938, #22549, #4088, #41195, #8401, #18711, #11790, #26407, #23029, #33370, #19184, #4312, #26880, #41441, #19666, #34308, #33606, #719, #8160, #22788, #33843, #23741, #34529, #27607, #1685, #46232, #35251, #9367, #35480, #27844, #42159, #2620, #42629, #9837, #35011, #17022, #2159, #2386, #38347, #41915, #17253, #45290, #16556, #12969, #23991, #41679, #31659, #27129, #13437, #46002, #12506, #5523, #20137, #34783, #5282, #31185, #38590, #16786, #28066, #8884, #1924, #31425, #16332, #24447, #13210, #39046, #6212, #19898, #30954, #5766, #23519, #20607, #38823, #12742, #20371, #9605, #38122, #42406, #9126, #24227, #20841, #45520, #5986, #27373, #45759, #25405, #17950, #32608, #10309, #21071, #14139, #35708, #32840, #21799, #43348, #22022, #14376, #10552, #36648, #29275, #43823, #3344, #18200, #47196, #36424, #24922, #28536, #3808, #31891, #3094, #46947, #25151, #28292, #47436, #13654, #14604, #29023, #46470, #39514, #6688, #21306, #39279, #17719, #39741, #43581, #11022, #42854, #35934, #10795, #17481, #25640, #39983, #40215, #7406, #6453, #32115, #6928, #10063, #7174, #24682, #46702, #43103, #32369, #34022, #438, #4257, #7635, #44986, #663, #1146, #11256, #29970, #15091, #906, #37831, #29738, #44280, #33790, #33315, #11483, #22972, #33547, #22251, #15804, #18892, #26105, #15317, #37338, #40678, #30432, #44517, #23218, #37109, #8346, #7875, #22490, #15569, #26353, #22733, #4488, #36882, #18424, #33073, #37579, #30208, #12196, #4740, #4038, #200, #44752, #11970, #19367, #26823, #14847, #41379, #29511, #8579, #25867, #44059, #40449, #42571, #38294, #35186, #1864, #9780, #23683, #42351, #19843, #34472, #34954, #1622, #5215, #16500, #23458, #24390, #4989, #9546, #5463, #2333, #24167, #38060, #19609, #9303, #45461, #31130, #31365, #34248, #8823, #1378, #16271, #45224, #5701, #2099, #16036, #20078, #34725, #16729, #12446, #12916, #12686, #45944, #38769, #20547, #13155, #27068, #30664, #27788, #38533, #20315, #27311, #41616, #45697, #41861, #5930, #16959, #27546, #9065, #31599, #42098, #23926, #46180, #13378, #28006, #10740, #28726, #43525, #32061, #35656, #11610, #38989, #10254, #6635, #3032, #35422, #25348, #20780, #39931, #39684, #29854, #46649, #13834, #28477, #46415, #24859, #21255, #43295, #7118, #44395, #17424, #25093, #10010, #21742, #10495, #36373, #3529, #13593, #24623, #17663, #2560, #14323, #32551, #6398, #18142, #35879, #32785, #21010, #39459, #28231, #47380, #32311, #14552, #31829, #46890, #2795, #21491, #6159, #43047, #14080, #6870, #39223, #36123, #17193, #3278, #42794, #47138, #28968, #33907, #41259, #45106, #4614, #41741, #8225, #12081, #15441, #5332, #8459, #8945, #19003, #37707, #22851, #8700, #45575, #37466, #19248, #26940, #26469, #41031, #30782, #23089, #30095, #23565, #26705, #1028, #4860, #12324, #15684, #38169, #19486, #31006, #44869, #16151, #30321, #34134, #23336, #1264, #15917, #30544, #44627, #26232, #40798, #45349, #41494, #19952, #12562, #11842, #7991, #37949, #5097, #19721, #34359, #22616, #1496, #37228, #27187, #33666, #34592, #1742, #16387, #4373, #27896, #24506, #5583, #20663, #9428, #9893, #31946, #28350, #20900, #34840, #17544, #6274, #46298, #13489, #38648, #1985, #42458, #16615, #13714, #2679, #24279, #2908, #42680, #9663, #32181, #10131, #24739, #2444, #46532, #17072, #17310, #5823, #24048, #12797, #27431, #31475, #38874, #6039, #9180, #42919, #41972, #39336, #28120, #23796, #20431, #35065, #2216, #20189, #46059, #35307, #31713, #6514, #38412, #16835, #39101, #31242, #21133, #35539, #35768, #45819, #13028, #27665, #42226, #13267, #47452, #18216, #39530, #43842, #6947, #13906, #21322, #6467, #17970, #3825, #14625, #36444, #17497, #29294, #3111, #21085, #14391, #11043, #24693, #32858, #43362, #21568, #10812, #10569, #21816, #43121, #7191, #3596, #35953, #25659, #29041, #40235, #22041, #25171, #32624, #10325, #7423, #47211, #36667, #18446, #33095, #14866, #39755, #17734, #36206, #29525, #24937, #32384, #216, #44076, #6709, #39294, #35725, #2860, #3358, #46965, #32128, #14154, #46720, #28798, #43600, #25424, #39998, #18672, #15338, #11272, #928, #11751, #41162, #34042, #29991, #4057, #26372, #44535, #15108, #40931, #41404, #37854, #29753, #8127, #26610, #44771, #45007, #44301, #12220, #23241, #8366, #4275, #5009, #16059, #18909, #8601, #22750, #30224, #15586, #15826, #22267, #11504, #1167, #22992, #37356, #11987, #33812, #7650, #33332, #36903, #455, #19391, #26126, #26843, #19145, #683, #19628, #30451, #40696, #33565, #25885, #37604, #7892, #34269, #4764, #40467, #30686, #1399, #22510, #37126, #16524, #42373, #27091, #12938, #35213, #17221, #13402, #20572, #28032, #38314, #31153, #9571, #41642, #27571, #2351, #45250, #42591, #34493, #41881, #8846, #38559, #24412, #16984, #24190, #38084, #31623, #23707, #23483, #34978, #46203, #12470, #38792, #45722, #42119, #31393, #9334, #5949, #1648, #27813, #9803, #9087, #39016, #2123, #6180, #20804, #23953, #5724, #30922, #35445, #20340, #2583, #5241, #19868, #16292, #16752, #5488, #45962, #45483, #12711, #20102, #27336, #34748, #1889, #13176, #18162, #7139, #32332, #21034, #13614, #10273, #31856, #29240, #39480, #28988, #36396, #39243, #35899, #46434, #21509, #46912, #14342, #3550, #3052, #24649, #14102, #17681, #35679, #28748, #14571, #10989, #2816, #43312, #47158, #17920, #32802, #17447, #47397, #43791, #43546, #24883, #25606, #36613, #6657, #40180, #10516, #3301, #36147, #7381, #42817, #32081, #21991, #10760, #25114, #32573, #6891, #28254, #6417, #10029, #46670, #3772, #13856, #28503, #39703, #21274, #43069, #25367, #3998, #11449, #33037, #11692, #40410, #4704, #33509, #164, #37795, #25833, #22450, #18395, #8072, #18851, #866, #41110, #37071, #11219, #621, #4224, #22212, #15281, #1109, #44951, #36842, #29931, #33756, #4449, #19334, #18619, #33983, #30401, #15526, #26066, #12161, #23179, #40635, #15770, #44476, #37298, #22694, #22933, #29472, #33279, #8302, #30169, #26317, #19084, #40873, #14811, #7597, #44017, #404, #26551, #15054, #26785, #44709, #7838, #41344, #37543, #44246, #11931, #8545, #45659, #27032, #38735, #20042, #19575, #24357, #27752, #35151, #45429, #23647, #2067, #34220, #34681, #42317, #1347, #20516, #41584, #1583, #16003 ),
 ( #24132, #1827, #2293, #34437, #38258, #8786, #31565, #16462, #16923, #23422, #31099, #16235, #34922, #30625, #30868, #12648, #5667, #5184, #19805, #9509, #12878, #38024, #46146, #5422, #27273, #27511, #23886, #41822, #13343, #42063, #9741, #9267, #5902, #9024, #16698, #27972, #38495, #20274, #31326, #45903, #13119, #42537, #14285, #10214, #31799, #6599, #24818, #42755, #39419, #21703, #18105, #9975, #21213, #6830, #25055, #25304, #24587, #39894, #3489, #21450, #32023, #32747, #43732, #46613, #36337, #2992, #10455, #28686, #43490, #17157, #39184, #28927, #36080, #35843, #43255, #14039, #35387, #13561, #46382, #28197, #47092, #6357, #7078, #43005, #28442, #47345, #10698, #20972, #17626, #6119, #32270, #35617, #14517, #46850, #20744, #10935, #29184, #38955, #39649, #3236, #17866, #2760, #32509, #17384, #41062, #4408, #109, #25787, #40126, #40592, #15476, #26264, #29882, #3722, #40826, #7548, #7325, #37028, #8020, #25555, #22651, #29658, #26016, #15238, #44198, #11642, #43969, #37256, #19037, #36795, #33704, #18805, #812, #44659, #11398, #4179, #40357, #30123, #33462, #44427, #11876, #26503, #21942, #7785, #3948, #22400, #36562, #22158, #33229, #18343, #32985, #18572, #14754, #29425, #11171, #356, #579, #15006, #46762, #20895, #18254, #17538, #35760, #14194, #14, #43640, #32663, #2901, #10851, #43159, #32173, #21613, #25464, #35534, #14431, #39568, #47001, #36247, #6745, #18009, #24973, #3398, #47249, #21364, #29083, #40038, #36479, #32896, #35991, #43398, #3632, #14663, #29337, #43880, #25701, #9897, #13717, #9432, #20193, #42229, #28354, #41977, #45823, #20667, #38878, #12801, #39105, #6279, #20902, #38654, #45579, #38175, #13033, #8949, #35543, #27669, #2448, #2685, #16392, #5827, #23569, #46064, #27900, #17313, #31951, #42463, #1749, #9667, #24283, #9184, #5337, #19958, #34598, #23800, #31013, #38416, #25472, #18490, #46770, #268, #32185, #7240, #36002, #13956, #39576, #17786, #32433, #3406, #21861, #3641, #21, #14205, #18022, #32905, #20330, #41873, #12929, #45713, #19619, #45238, #34259, #30677, #31382, #1390, #24181, #27325, #12700, #16974, #45955, #8837, #16283, #37843, #16515, #12462, #9559, #5478, #5001, #42581, #13167, #5939, #30914, #9078, #34968, #16049, #20093, #27801, #23231, #38783, #27080, #20560, #41630, #35202, #2343, #38549, #45473, #31613, #28021, #23697, #46194, #34739, #42111, #27562, #42365, #23472, #38074, #13392, #2112, #31144, #9320, #23942, #5229, #19857, #34484, #1637, #5713, #16743, #10753, #13845, #43058, #3543, #17911, #42807, #17437, #6173, #32322, #32071, #43536, #24869, #2572, #9793, #32562, #21753, #14091, #28736, #21500, #17208, #10506, #47150, #25104, #18154, #3291, #14334, #28979, #32794, #47390, #19077, #8062, #36606, #33749, #22206, #25600, #33502, #858, #43781, #37292, #15047, #26060, #29925, #29697, #40866, #155, #26310, #22688, #40404, #4443, #615, #15517, #41102, #44238, #4217, #29465, #30160, #18846, #44701, #8296, #11919, #33976, #11443, #7592, #40630, #1102, #14806, #36838, #26542, #22923, #44010, #37536, #4695, #19327, #7829, #33029, #40171, #3990, #10983, #15760, #18612, #7373, #21984, #3765, #396, #18387, #15274, #22444, #11214, #25827, #37065, #33272, #44470, #11685, #34209, #2232, #13728, #10145, #1337, #46077, #46319, #17088, #20914, #42474, #21145, #13503, #27911, #35780, #28366, #42935, #20681, #2697, #35321, #35553, #24062, #27680, #2922, #30393, #16851, #13278, #9679, #26778, #17324, #12154, #31960, #31726, #44942, #38669, #5838, #20446, #37785, #31493, #24294, #2461, #46545, #41337, #9446, #28135, #15993, #24754, #42692, #39350, #6531, #4937, #30616, #38892, #8536, #23168, #24519, #45180, #19563, #6055, #12401, #42243, #39117, #35084, #44130, #47269, #33158, #10388, #29104, #14218, #34, #36953, #28859, #43418, #18272, #17798, #32445, #22093, #32680, #21386, #279, #3417, #25229, #14448, #36495, #10626, #14924, #43659, #22325, #36267, #7474, #47023, #39817, #14683, #7006, #21633, #10867, #36011, #17557, #32195, #36720, #18034, #29589, #3882, #3168, #46782, #21875, #25487, #40053, #43898, #13969, #7253, #28619, #3651, #24993, #32915, #29356, #7710, #11097, #25720, #40289, #39588, #18501, #11328, #25940, #6769, #40520, #43179, #41208, #26661, #503, #26185, #15162, #11561, #12272, #29806, #5059, #37901, #7949, #19676, #16109, #19439, #44585, #30733, #8897, #11803, #1450, #15637, #23042, #8414, #8650, #15397, #34318, #40753, #15870, #22801, #37660, #4816, #44353, #22568, #37183, #4327, #26893, #18960, #45302, #8175, #40990, #12520, #41450, #33620, #26422, #18729, #44826, #735, #41695, #19201, #33389, #23529, #23288, #4110, #37409, #4567, #1219, #30041, #33860, #979, #30274, #12038, #34089, #30498, #45058, #31433, #17268, #13447, #2400, #30964, #28076, #16567, #19912, #27854, #42637, #38132, #31670, #9380, #20380, #24236, #24001, #35266, #41928, #20617, #17033, #34793, #46248, #42413, #9848, #35495, #38600, #46014, #23751, #24458, #13219, #39060, #2634, #6228, #28302, #5774, #1933, #35020, #42869, #9134, #31197, #20852, #31904, #38362, #46485, #13666, #10082, #2169, #27384, #34542, #45770, #5292, #1694, #12980, #16343, #45531, #12754, #42172, #5533, #9617, #16792, #20148, #27619, #38833, #5997, #6560, #10169, #46570, #21168, #6312, #2947, #40230, #36901, #37125, #7890, #40464, #4055, #26123, #37354, #11985, #213, #22508, #7419, #26370, #40694, #22748, #8125, #29290, #22037, #453, #18212, #44533, #15336, #36663, #40929, #18670, #4507, #3821, #7647, #11039, #926, #33330, #19143, #14620, #15106, #18441, #18907, #41160, #33092, #14863, #33563, #29522, #44073, #33809, #29751, #25654, #15584, #22264, #11270, #44299, #681, #25882, #30222, #11502, #26608, #29988, #11749, #44769, #21812, #36440, #3592, #32854, #47448, #43838, #13174, #27811, #45720, #27089, #5722, #27569, #26841, #22990, #12709, #34267, #34491, #34746, #37601, #12218, #4762, #41401, #1165, #9085, #5485, #45960, #41640, #23481, #20100, #15824, #16290, #5007, #19388, #34040, #31391, #1397, #30449, #8364, #1887, #41879, #23705, #16057, #45005, #38082, #8599, #9331, #12936, #19866, #23239, #38312, #5239, #30684, #20338, #34976, #45481, #42117, #27334, #23951, #45247, #12468, #8844, #1645, #30920, #16522, #31151, #38557, #2121, #16750, #14100, #43067, #33223, #35443, #17219, #31854, #2349, #46432 ),
 ( #10271, #39478, #349, #28252, #10027, #6655, #35211, #2814, #39014, #24188, #20570, #18567, #6178, #16982, #14998, #35897, #28501, #24881, #20802, #31621, #24647, #46201, #43310, #32330, #6415, #42371, #21272, #39241, #9569, #39701, #6889, #32079, #28746, #46668, #46910, #2581, #13612, #38790, #5947, #42815, #21032, #35677, #13400, #10514, #28030, #25112, #3050, #42589, #17445, #13854, #17679, #9801, #21507, #36145, #3299, #24410, #15943, #11634, #22877, #18797, #12106, #41053, #8484, #41284, #22394, #33454, #30116, #11393, #30344, #15709, #15227, #26731, #803, #23119, #29874, #4398, #37020, #19510, #15468, #37732, #7777, #44648, #44416, #19272, #45130, #26253, #40815, #37489, #570, #8012, #4887, #33693, #22641, #34159, #19027, #37246, #11866, #8251, #26491, #1288, #4643, #30568, #33928, #29649, #1051, #44190, #26006, #40585, #44893, #4173, #14661, #29567, #18006, #21611, #44337, #24328, #43638, #40035, #36477, #20715, #44114, #6089, #11308, #25699, #15144, #32661, #47247, #14429, #31767, #10848, #7232, #29334, #40504, #29791, #3396, #11080, #42730, #25922, #43878, #7691, #22307, #46350, #9945, #3630, #35355, #258, #18484, #39794, #36937, #21851, #4087, #6987, #25462, #13534, #18709, #18252, #33369, #17125, #32894, #36244, #7457, #38927, #29081, #12, #40271, #24550, #22078, #488, #36703, #28169, #2502, #3864, #33132, #14906, #30482, #37395, #41677, #23028, #16328, #30261, #1433, #26406, #40970, #41440, #8158, #11789, #37642, #30027, #30953, #11541, #16094, #44809, #8882, #30715, #44570, #26166, #15859, #4550, #4796, #37886, #40735, #15378, #7929, #22787, #4311, #12257, #8636, #1682, #12021, #26646, #23270, #18944, #19424, #19183, #22548, #37164, #34526, #33842, #33605, #718, #5044, #45042, #26879, #963, #15621, #41194, #34077, #12504, #45288, #1205, #19664, #34306, #27127, #23517, #38120, #5280, #19895, #23987, #28287, #42401, #2842, #16783, #35476, #12965, #27606, #28063, #42156, #45756, #9602, #31182, #17478, #45518, #2615, #31421, #10060, #17250, #9364, #12740, #2382, #38586, #24223, #24442, #27370, #1921, #41912, #5763, #38344, #46228, #42625, #35704, #13207, #27841, #9834, #5520, #5982, #20368, #9124, #23740, #21067, #35007, #20135, #34781, #39042, #31655, #13432, #2155, #38820, #20602, #35247, #46466, #31887, #17018, #6208, #20837, #13650, #24679, #39275, #6450, #36420, #18421, #3578, #33069, #25146, #6923, #4032, #32112, #3341, #47192, #43577, #28531, #14842, #39510, #11252, #32836, #22246, #10791, #25401, #39978, #6684, #7171, #18196, #11019, #36878, #46698, #21302, #17714, #23679, #9776, #9542, #35419, #38986, #12679, #5458, #31361, #1617, #28003, #42568, #34720, #24387, #34951, #17192, #1859, #38529, #41856, #31824, #2095, #46411, #45456, #16725, #16497, #35183, #5211, #31127, #45693, #2329, #12913, #27543, #13590, #20310, #9060, #28227, #10006, #19839, #5698, #42096, #45941, #34467, #9300, #23921, #16267, #30900, #13151, #27306, #27785, #42346, #24164, #38766, #21007, #17659, #39219, #36594, #46886, #36369, #43765, #46645, #43291, #6395, #28964, #39679, #21737, #14547, #10491, #32057, #6866, #25089, #43043, #21487, #21969, #18374, #10250, #36119, #7114, #25343, #25585, #24856, #40158, #3751, #3524, #32308, #33016, #43999, #14074, #138, #3274, #10735, #43521, #10967, #3028, #7357, #28473, #18136, #17898, #39927, #32781, #35653, #13832, #2791, #39455, #47375, #17420, #14791, #32546, #28722, #29452, #29217, #6631, #47134, #21250, #11201, #35875, #12140, #40853, #40390, #45165, #1086, #8523, #18834, #44459, #22910, #7579, #8048, #15745, #25814, #41321, #15035, #22431, #22192, #19064, #4925, #30379, #37524, #18597, #44925, #4205, #36828, #15503, #26764, #3979, #19310, #11672, #22676, #11904, #26296, #4680, #29684, #8284, #33963, #37051, #23153, #30148, #37768, #19548, #37277, #33733, #11430, #34195, #843, #1323, #15980, #30601, #4432, #33259, #40621, #7815, #383, #33489, #26048, #44687, #44226, #605, #15262, #29909, #26527, #41087, #31539, #30844, #27008, #16673, #38235, #38472, #38713, #41552, #16213, #8760, #45411, #5162, #13093, #9487, #2506, #45637, #27489, #24106, #19781, #20253, #9001, #23397, #38001, #35361, #23625, #34415, #17130, #5883, #45881, #27726, #5393, #1558, #42040, #12624, #13318, #2274, #23860, #31772, #42288, #9242, #12387, #9719, #24333, #2040, #46120, #31301, #16899, #20016, #34655, #27247, #41801, #31073, #5642, #34899, #1805, #27949, #16444, #42516, #20490, #12856, #35128, #38931, #6093, #20718, #32242, #14012, #32486, #14489, #36537, #24795, #43462, #42979, #3464, #25275, #47315, #32723, #20949, #10188, #21425, #42733, #21678, #39863, #21185, #18075, #43225, #29148, #35818, #46824, #35593, #40101, #10430, #43704, #2732, #7053, #2965, #36309, #18318, #7295, #21915, #46354, #13538, #28172, #9948, #24557, #36765, #1030, #18779, #40565, #548, #4375, #11371, #15686, #29856, #25982, #33668, #33202, #324, #37468, #15205, #3924, #30323, #33433, #7755, #44396, #19005, #22373, #44871, #11612, #37708, #4153, #22852, #14974, #29630, #15443, #44169, #36997, #26233, #18546, #4862, #32956, #4616, #40799, #12083, #19250, #7992, #78, #37230, #22618, #781, #11844, #14726, #30097, #29399, #44629, #25761, #26471, #41033, #23090, #8227, #33909, #26707, #40330, #41261, #8461, #43943, #11141, #7517, #22138, #41496, #24281, #13031, #5585, #20191, #45351, #8702, #1744, #23338, #20433, #9430, #31008, #9665, #1987, #16389, #38876, #16837, #31477, #9182, #38650, #23797, #24050, #12564, #16153, #19488, #34136, #38171, #34594, #45577, #15919, #5825, #1266, #35067, #34842, #30546, #27189, #41743, #8947, #26942, #5334, #12799, #38414, #2218, #45108, #23567, #16617, #37951, #46061, #31244, #13269, #27898, #5099, #19723, #27433, #12326, #42228, #27667, #34360, #42460, #41974, #1498, #30784, #19954, #45821, #32668, #35769, #21621, #46300, #17546, #2681, #36001, #25471, #17312, #18018, #43406, #43649, #6516, #31948, #39338, #10858, #24508, #46534, #3159, #17784, #9895, #39806, #6994, #28845, #21135, #42682, #35309, #13716, #6041, #3405, #28351, #32432, #10616, #13491, #10133, #20665, #43169, #2910, #47010, #25215, #24741, #28122, #32183, #46769, #39103, #13955, #36254, #47257, #6276, #28606, #21375, #39575, #14437, #20901, #29090, #2446, #14202, #42921, #17074, #31715, #10374, #35541, #24981, #6753, #29796 ) ),
 .UNSPECIFIED., .F., .F., .T. ) 
 B_SPLINE_SURFACE_WITH_KNOTS ( ( 2, 1, 2 ),
 ( 3, 2, 2, 2, 2, 2, 2, 2, 2, 2, 2, 2, 2, 2, 2, 2, 2, 2, 2, 2, 2, 2, 2, 2, 2, 2, 2, 2, 2, 2, 2, 2, 2, 2, 2, 2, 2, 2, 2, 2, 2, 2, 2, 2, 2, 2, 2, 2, 2, 2, 2, 2, 2, 2, 2, 2, 2, 2, 2, 2, 2, 2, 2, 2, 2, 2, 2, 2, 2, 2, 2, 2, 2, 2, 2, 2, 2, 2, 2, 2, 2, 2, 2, 2, 2, 2, 2, 2, 2, 2, 2, 2, 2, 2, 2, 2, 2, 2, 2, 2, 2, 2, 2, 2, 2, 2, 2, 2, 2, 2, 2, 2, 2, 2, 2, 2, 2, 2, 2, 2, 2, 2, 2, 2, 2, 2, 2, 2, 2, 2, 2, 2, 2, 2, 2, 2, 2, 2, 2, 2, 2, 2, 2, 2, 2, 2, 2, 2, 2, 2, 2, 2, 2, 2, 2, 2, 2, 2, 2, 2, 2, 2, 2, 2, 2, 2, 2, 2, 2, 2, 2, 2, 2, 2, 2, 2, 2, 2, 2, 2, 2, 2, 2, 2, 2, 2, 2, 2, 2, 2, 2, 2, 2, 2, 2, 2, 2, 2, 2, 2, 2, 2, 2, 2, 2, 2, 2, 2, 2, 2, 2, 2, 2, 2, 2, 2, 2, 2, 2, 2, 2, 2, 2, 2, 2, 2, 2, 2, 2, 2, 2, 2, 2, 2, 2, 2, 2, 2, 2, 2, 2, 2, 2, 2, 2, 2, 2, 2, 2, 2, 2, 2, 2, 2, 2, 2, 2, 2, 2, 2, 2, 2, 2, 2, 2, 2, 2, 2, 2, 2, 2, 2, 2, 2, 2, 2, 2, 2, 2, 2, 2, 2, 2, 2, 2, 2, 2, 2, 2, 2, 2, 2, 2, 2, 2, 2, 2, 2, 2, 2, 2, 2, 2, 2, 2, 2, 2, 2, 2, 2, 2, 2, 2, 2, 2, 2, 2, 2, 2, 2, 2, 2, 2, 2, 2, 2, 2, 2, 2, 2, 2, 2, 2, 2, 2, 2, 2, 2, 2, 2, 2, 2, 2, 2, 2, 2, 2, 2, 2, 2, 2, 2, 2, 2, 2, 2, 2, 2, 2, 2, 2, 2, 2, 2, 2, 2, 2, 2, 2, 2, 2, 2, 2, 2, 2, 2, 2, 2, 2, 2, 2, 2, 2, 2, 2, 2, 2, 2, 2, 2, 2, 2, 2, 2, 2, 2, 2, 2, 2, 2, 3 ),
 ( 0.000000000000000000, 1.000000000000000000, 1.043560847470196062 ),
 ( 0.000000000000000000, 0.002500000000000000052, 0.005000000000000000104, 0.007499999999999999722, 0.01000000000000000021, 0.01250000000000000069, 0.01499999999999999944, 0.01750000000000000167, 0.02000000000000000042, 0.02249999999999999917, 0.02500000000000000139, 0.02750000000000000014, 0.02999999999999999889, 0.03250000000000000111, 0.03500000000000000333, 0.03749999999999999861, 0.04000000000000000083, 0.04250000000000000305, 0.04499999999999999833, 0.04750000000000000056, 0.05000000000000000278, 0.05249999999999999806, 0.05500000000000000028, 0.05750000000000000250, 0.05999999999999999778, 0.06250000000000000000, 0.06500000000000000222, 0.06750000000000000444, 0.07000000000000000666, 0.07249999999999999500, 0.07499999999999999722, 0.07749999999999999944, 0.08000000000000000167, 0.08250000000000000389, 0.08500000000000000611, 0.08749999999999999445, 0.08999999999999999667, 0.09249999999999999889, 0.09500000000000000111, 0.09750000000000000333, 0.1000000000000000056, 0.1024999999999999939, 0.1049999999999999961, 0.1074999999999999983, 0.1100000000000000006, 0.1125000000000000028, 0.1150000000000000050, 0.1174999999999999933, 0.1199999999999999956, 0.1224999999999999978, 0.1250000000000000000, 0.1275000000000000022, 0.1300000000000000044, 0.1325000000000000067, 0.1350000000000000089, 0.1375000000000000111, 0.1400000000000000133, 0.1424999999999999878, 0.1449999999999999900, 0.1474999999999999922, 0.1499999999999999944, 0.1524999999999999967, 0.1549999999999999989, 0.1575000000000000011, 0.1600000000000000033, 0.1625000000000000056, 0.1650000000000000078, 0.1675000000000000100, 0.1700000000000000122, 0.1724999999999999867, 0.1749999999999999889, 0.1774999999999999911, 0.1799999999999999933, 0.1824999999999999956, 0.1849999999999999978, 0.1875000000000000000, 0.1900000000000000022, 0.1925000000000000044, 0.1950000000000000067, 0.1975000000000000089, 0.2000000000000000111, 0.2025000000000000133, 0.2049999999999999878, 0.2074999999999999900, 0.2099999999999999922, 0.2124999999999999944, 0.2149999999999999967, 0.2174999999999999989, 0.2200000000000000011, 0.2225000000000000033, 0.2250000000000000056, 0.2275000000000000078, 0.2300000000000000100, 0.2325000000000000122, 0.2349999999999999867, 0.2374999999999999889, 0.2399999999999999911, 0.2424999999999999933, 0.2449999999999999956, 0.2474999999999999978, 0.2500000000000000000, 0.2525000000000000022, 0.2550000000000000044, 0.2575000000000000067, 0.2600000000000000089, 0.2625000000000000111, 0.2650000000000000133, 0.2675000000000000155, 0.2700000000000000178, 0.2725000000000000200, 0.2750000000000000222, 0.2775000000000000244, 0.2800000000000000266, 0.2824999999999999734, 0.2849999999999999756, 0.2874999999999999778, 0.2899999999999999800, 0.2924999999999999822, 0.2949999999999999845, 0.2974999999999999867, 0.2999999999999999889, 0.3024999999999999911, 0.3049999999999999933, 0.3074999999999999956, 0.3099999999999999978, 0.3125000000000000000, 0.3150000000000000022, 0.3175000000000000044, 0.3200000000000000067, 0.3225000000000000089, 0.3250000000000000111, 0.3275000000000000133, 0.3300000000000000155, 0.3325000000000000178, 0.3350000000000000200, 0.3375000000000000222, 0.3400000000000000244, 0.3425000000000000266, 0.3449999999999999734, 0.3474999999999999756, 0.3499999999999999778, 0.3524999999999999800, 0.3549999999999999822, 0.3574999999999999845, 0.3599999999999999867, 0.3624999999999999889, 0.3649999999999999911, 0.3674999999999999933, 0.3699999999999999956, 0.3724999999999999978, 0.3750000000000000000, 0.3775000000000000022, 0.3800000000000000044, 0.3825000000000000067, 0.3850000000000000089, 0.3875000000000000111, 0.3900000000000000133, 0.3925000000000000155, 0.3950000000000000178, 0.3975000000000000200, 0.4000000000000000222, 0.4025000000000000244, 0.4050000000000000266, 0.4074999999999999734, 0.4099999999999999756, 0.4124999999999999778, 0.4149999999999999800, 0.4174999999999999822, 0.4199999999999999845, 0.4224999999999999867, 0.4249999999999999889, 0.4274999999999999911, 0.4299999999999999933, 0.4324999999999999956, 0.4349999999999999978, 0.4375000000000000000, 0.4400000000000000022, 0.4425000000000000044, 0.4450000000000000067, 0.4475000000000000089, 0.4500000000000000111, 0.4525000000000000133, 0.4550000000000000155, 0.4575000000000000178, 0.4600000000000000200, 0.4625000000000000222, 0.4650000000000000244, 0.4675000000000000266, 0.4699999999999999734, 0.4724999999999999756, 0.4749999999999999778, 0.4774999999999999800, 0.4799999999999999822, 0.4824999999999999845, 0.4849999999999999867, 0.4874999999999999889, 0.4899999999999999911, 0.4924999999999999933, 0.4949999999999999956, 0.4974999999999999978, 0.5000000000000000000, 0.5024999999999999467, 0.5050000000000000044, 0.5074999999999999512, 0.5100000000000000089, 0.5124999999999999556, 0.5150000000000000133, 0.5174999999999999600, 0.5200000000000000178, 0.5224999999999999645, 0.5250000000000000222, 0.5274999999999999689, 0.5300000000000000266, 0.5324999999999999734, 0.5350000000000000311, 0.5374999999999999778, 0.5400000000000000355, 0.5424999999999999822, 0.5450000000000000400, 0.5474999999999999867, 0.5500000000000000444, 0.5524999999999999911, 0.5550000000000000488, 0.5574999999999999956, 0.5600000000000000533, 0.5625000000000000000, 0.5649999999999999467, 0.5675000000000000044, 0.5699999999999999512, 0.5725000000000000089, 0.5749999999999999556, 0.5775000000000000133, 0.5799999999999999600, 0.5825000000000000178, 0.5849999999999999645, 0.5875000000000000222, 0.5899999999999999689, 0.5925000000000000266, 0.5949999999999999734, 0.5975000000000000311, 0.5999999999999999778, 0.6025000000000000355, 0.6049999999999999822, 0.6075000000000000400, 0.6099999999999999867, 0.6125000000000000444, 0.6149999999999999911, 0.6175000000000000488, 0.6199999999999999956, 0.6225000000000000533, 0.6250000000000000000, 0.6274999999999999467, 0.6300000000000000044, 0.6324999999999999512, 0.6350000000000000089, 0.6374999999999999556, 0.6400000000000000133, 0.6424999999999999600, 0.6450000000000000178, 0.6474999999999999645, 0.6500000000000000222, 0.6524999999999999689, 0.6550000000000000266, 0.6574999999999999734, 0.6600000000000000311, 0.6624999999999999778, 0.6650000000000000355, 0.6674999999999999822, 0.6700000000000000400, 0.6724999999999999867, 0.6750000000000000444, 0.6774999999999999911, 0.6800000000000000488, 0.6824999999999999956, 0.6850000000000000533, 0.6875000000000000000, 0.6899999999999999467, 0.6925000000000000044, 0.6949999999999999512, 0.6975000000000000089, 0.6999999999999999556, 0.7025000000000000133, 0.7049999999999999600, 0.7075000000000000178, 0.7099999999999999645, 0.7125000000000000222, 0.7149999999999999689, 0.7175000000000000266, 0.7199999999999999734, 0.7225000000000000311, 0.7249999999999999778, 0.7275000000000000355, 0.7299999999999999822, 0.7325000000000000400, 0.7349999999999999867, 0.7375000000000000444, 0.7399999999999999911, 0.7425000000000000488, 0.7449999999999999956, 0.7475000000000000533, 0.7500000000000000000, 0.7524999999999999467, 0.7550000000000000044, 0.7574999999999999512, 0.7600000000000000089, 0.7624999999999999556, 0.7650000000000000133, 0.7674999999999999600, 0.7700000000000000178, 0.7724999999999999645, 0.7750000000000000222, 0.7774999999999999689, 0.7800000000000000266, 0.7824999999999999734, 0.7850000000000000311, 0.7874999999999999778, 0.7900000000000000355, 0.7924999999999999822, 0.7950000000000000400, 0.7974999999999999867, 0.8000000000000000444, 0.8024999999999999911, 0.8050000000000000488, 0.8074999999999999956, 0.8100000000000000533, 0.8125000000000000000, 0.8149999999999999467, 0.8175000000000000044, 0.8199999999999999512, 0.8225000000000000089, 0.8249999999999999556, 0.8275000000000000133, 0.8299999999999999600, 0.8325000000000000178, 0.8349999999999999645, 0.8375000000000000222, 0.8399999999999999689, 0.8425000000000000266, 0.8449999999999999734, 0.8475000000000000311, 0.8499999999999999778, 0.8525000000000000355, 0.8549999999999999822, 0.8575000000000000400, 0.8599999999999999867, 0.8625000000000000444, 0.8649999999999999911, 0.8675000000000000488, 0.8699999999999999956, 0.8725000000000000533, 0.8750000000000000000, 0.8774999999999999467, 0.8800000000000000044, 0.8824999999999999512, 0.8850000000000000089, 0.8874999999999999556, 0.8900000000000000133, 0.8924999999999999600, 0.8950000000000000178, 0.8974999999999999645, 0.9000000000000000222, 0.9024999999999999689, 0.9050000000000000266, 0.9074999999999999734, 0.9100000000000000311, 0.9124999999999999778, 0.9150000000000000355, 0.9174999999999999822, 0.9200000000000000400, 0.9224999999999999867, 0.9250000000000000444, 0.9274999999999999911, 0.9300000000000000488, 0.9324999999999999956, 0.9350000000000000533, 0.9375000000000000000, 0.9399999999999999467, 0.9425000000000000044, 0.9449999999999999512, 0.9475000000000000089, 0.9499999999999999556, 0.9525000000000000133, 0.9549999999999999600, 0.9575000000000000178, 0.9599999999999999645, 0.9625000000000000222, 0.9649999999999999689, 0.9675000000000000266, 0.9699999999999999734, 0.9725000000000000311, 0.9749999999999999778, 0.9775000000000000355, 0.9799999999999999822, 0.9825000000000000400, 0.9849999999999999867, 0.9875000000000000444, 0.9899999999999999911, 0.9925000000000000488, 0.9949999999999999956, 0.9975000000000000533, 1.000000000000000000 ),
 .UNSPECIFIED. ) 
 GEOMETRIC_REPRESENTATION_ITEM ( )  RATIONAL_B_SPLINE_SURFACE ( (
 ( 1.000000000000000000, 0.9238795325112869605, 1.000000000000000000, 0.9238795325112869605, 1.000000000000000000, 0.9238795325112869605, 1.000000000000000000, 0.9238795325112869605, 1.000000000000000000, 0.9238795325112869605, 1.000000000000000000, 0.9238795325112869605, 1.000000000000000000, 0.9238795325112869605, 1.000000000000000000, 0.9238795325112869605, 1.000000000000000000, 0.9238795325112869605, 1.000000000000000000, 0.9238795325112869605, 1.000000000000000000, 0.9238795325112869605, 1.000000000000000000, 0.9238795325112869605, 1.000000000000000000, 0.9238795325112869605, 1.000000000000000000, 0.9238795325112869605, 1.000000000000000000, 0.9238795325112869605, 1.000000000000000000, 0.9238795325112869605, 1.000000000000000000, 0.9238795325112869605, 1.000000000000000000, 0.9238795325112869605, 1.000000000000000000, 0.9238795325112869605, 1.000000000000000000, 0.9238795325112869605, 1.000000000000000000, 0.9238795325112869605, 1.000000000000000000, 0.9238795325112869605, 1.000000000000000000, 0.9238795325112869605, 1.000000000000000000, 0.9238795325112869605, 1.000000000000000000, 0.9238795325112869605, 1.000000000000000000, 0.9238795325112869605, 1.000000000000000000, 0.9238795325112869605, 1.000000000000000000, 0.9238795325112869605, 1.000000000000000000, 0.9238795325112869605, 1.000000000000000000, 0.9238795325112869605, 1.000000000000000000, 0.9238795325112869605, 1.000000000000000000, 0.9238795325112869605, 1.000000000000000000, 0.9238795325112869605, 1.000000000000000000, 0.9238795325112869605, 1.000000000000000000, 0.9238795325112869605, 1.000000000000000000, 0.9238795325112869605, 1.000000000000000000, 0.9238795325112869605, 1.000000000000000000, 0.9238795325112869605, 1.000000000000000000, 0.9238795325112869605, 1.000000000000000000, 0.9238795325112869605, 1.000000000000000000, 0.9238795325112869605, 1.000000000000000000, 0.9238795325112869605, 1.000000000000000000, 0.9238795325112869605, 1.000000000000000000, 0.9238795325112869605, 1.000000000000000000, 0.9238795325112869605, 1.000000000000000000, 0.9238795325112869605, 1.000000000000000000, 0.9238795325112869605, 1.000000000000000000, 0.9238795325112869605, 1.000000000000000000, 0.9238795325112869605, 1.000000000000000000, 0.9238795325112869605, 1.000000000000000000, 0.9238795325112869605, 1.000000000000000000, 0.9238795325112869605, 1.000000000000000000, 0.9238795325112869605, 1.000000000000000000, 0.9238795325112869605, 1.000000000000000000, 0.9238795325112869605, 1.000000000000000000, 0.9238795325112869605, 1.000000000000000000, 0.9238795325112869605, 1.000000000000000000, 0.9238795325112869605, 1.000000000000000000, 0.9238795325112869605, 1.000000000000000000, 0.9238795325112869605, 1.000000000000000000, 0.9238795325112869605, 1.000000000000000000, 0.9238795325112869605, 1.000000000000000000, 0.9238795325112869605, 1.000000000000000000, 0.9238795325112869605, 1.000000000000000000, 0.9238795325112869605, 1.000000000000000000, 0.9238795325112869605, 1.000000000000000000, 0.9238795325112869605, 1.000000000000000000, 0.9238795325112869605, 1.000000000000000000, 0.9238795325112869605, 1.000000000000000000, 0.9238795325112869605, 1.000000000000000000, 0.9238795325112869605, 1.000000000000000000, 0.9238795325112869605, 1.000000000000000000, 0.9238795325112869605, 1.000000000000000000, 0.9238795325112869605, 1.000000000000000000, 0.9238795325112869605, 1.000000000000000000, 0.9238795325112869605, 1.000000000000000000, 0.9238795325112869605, 1.000000000000000000, 0.9238795325112869605, 1.000000000000000000, 0.9238795325112869605, 1.000000000000000000, 0.9238795325112869605, 1.000000000000000000, 0.9238795325112869605, 1.000000000000000000, 0.9238795325112869605, 1.000000000000000000, 0.9238795325112869605, 1.000000000000000000, 0.9238795325112869605, 1.000000000000000000, 0.9238795325112869605, 1.000000000000000000, 0.9238795325112869605, 1.000000000000000000, 0.9238795325112869605, 1.000000000000000000, 0.9238795325112869605, 1.000000000000000000, 0.9238795325112869605, 1.000000000000000000, 0.9238795325112869605, 1.000000000000000000, 0.9238795325112869605, 1.000000000000000000, 0.9238795325112869605, 1.000000000000000000, 0.9238795325112869605, 1.000000000000000000, 0.9238795325112869605, 1.000000000000000000, 0.9238795325112869605, 1.000000000000000000, 0.9238795325112869605, 1.000000000000000000, 0.9238795325112869605, 1.000000000000000000, 0.9238795325112869605, 1.000000000000000000, 0.9238795325112869605, 1.000000000000000000, 0.9238795325112869605, 1.000000000000000000, 0.9238795325112869605, 1.000000000000000000, 0.9238795325112869605, 1.000000000000000000, 0.9238795325112869605, 1.000000000000000000, 0.9238795325112869605, 1.000000000000000000, 0.9238795325112869605, 1.000000000000000000, 0.9238795325112869605, 1.000000000000000000, 0.9238795325112869605, 1.000000000000000000, 0.9238795325112869605, 1.000000000000000000, 0.9238795325112869605, 1.000000000000000000, 0.9238795325112869605, 1.000000000000000000, 0.9238795325112869605, 1.000000000000000000, 0.9238795325112869605, 1.000000000000000000, 0.9238795325112869605, 1.000000000000000000, 0.9238795325112869605, 1.000000000000000000, 0.9238795325112869605, 1.000000000000000000, 0.9238795325112869605, 1.000000000000000000, 0.9238795325112869605, 1.000000000000000000, 0.9238795325112869605, 1.000000000000000000, 0.9238795325112869605, 1.000000000000000000, 0.9238795325112869605, 1.000000000000000000, 0.9238795325112869605, 1.000000000000000000, 0.9238795325112869605, 1.000000000000000000, 0.9238795325112869605, 1.000000000000000000, 0.9238795325112869605, 1.000000000000000000, 0.9238795325112869605, 1.000000000000000000, 0.9238795325112869605, 1.000000000000000000, 0.9238795325112869605, 1.000000000000000000, 0.9238795325112869605, 1.000000000000000000, 0.9238795325112869605, 1.000000000000000000, 0.9238795325112869605, 1.000000000000000000, 0.9238795325112869605, 1.000000000000000000, 0.9238795325112869605, 1.000000000000000000, 0.9238795325112869605, 1.000000000000000000, 0.9238795325112869605, 1.000000000000000000, 0.9238795325112869605, 1.000000000000000000, 0.9238795325112869605, 1.000000000000000000, 0.9238795325112869605, 1.000000000000000000, 0.9238795325112869605, 1.000000000000000000, 0.9238795325112869605, 1.000000000000000000, 0.9238795325112869605, 1.000000000000000000, 0.9238795325112869605, 1.000000000000000000, 0.9238795325112869605, 1.000000000000000000, 0.9238795325112869605, 1.000000000000000000, 0.9238795325112869605, 1.000000000000000000, 0.9238795325112869605, 1.000000000000000000, 0.9238795325112869605, 1.000000000000000000, 0.9238795325112869605, 1.000000000000000000, 0.9238795325112869605, 1.000000000000000000, 0.9238795325112869605, 1.000000000000000000, 0.9238795325112869605, 1.000000000000000000, 0.9238795325112869605, 1.000000000000000000, 0.9238795325112869605, 1.000000000000000000, 0.9238795325112869605, 1.000000000000000000, 0.9238795325112869605, 1.000000000000000000, 0.9238795325112869605, 1.000000000000000000, 0.9238795325112869605, 1.000000000000000000, 0.9238795325112869605, 1.000000000000000000, 0.9238795325112869605, 1.000000000000000000, 0.9238795325112869605, 1.000000000000000000, 0.9238795325112869605, 1.000000000000000000, 0.9238795325112869605, 1.000000000000000000, 0.9238795325112869605, 1.000000000000000000, 0.9238795325112869605, 1.000000000000000000, 0.9238795325112869605, 1.000000000000000000, 0.9238795325112869605, 1.000000000000000000, 0.9238795325112869605, 1.000000000000000000, 0.9238795325112869605, 1.000000000000000000, 0.9238795325112869605, 1.000000000000000000, 0.9238795325112869605, 1.000000000000000000, 0.9238795325112869605, 1.000000000000000000, 0.9238795325112869605, 1.000000000000000000, 0.9238795325112869605, 1.000000000000000000, 0.9238795325112869605, 1.000000000000000000, 0.9238795325112869605, 1.000000000000000000, 0.9238795325112869605, 1.000000000000000000, 0.9238795325112869605, 1.000000000000000000, 0.9238795325112869605, 1.000000000000000000, 0.9238795325112869605, 1.000000000000000000, 0.9238795325112869605, 1.000000000000000000, 0.9238795325112869605, 1.000000000000000000, 0.9238795325112869605, 1.000000000000000000, 0.9238795325112869605, 1.000000000000000000, 0.9238795325112869605, 1.000000000000000000, 0.9238795325112869605, 1.000000000000000000, 0.9238795325112869605, 1.000000000000000000, 0.9238795325112869605, 1.000000000000000000, 0.9238795325112869605, 1.000000000000000000, 0.9238795325112869605, 1.000000000000000000, 0.9238795325112869605, 1.000000000000000000, 0.9238795325112869605, 1.000000000000000000, 0.9238795325112869605, 1.000000000000000000, 0.9238795325112869605, 1.000000000000000000, 0.9238795325112869605, 1.000000000000000000, 0.9238795325112869605, 1.000000000000000000, 0.9238795325112869605, 1.000000000000000000, 0.9238795325112869605, 1.000000000000000000, 0.9238795325112869605, 1.000000000000000000, 0.9238795325112869605, 1.000000000000000000, 0.9238795325112869605, 1.000000000000000000, 0.9238795325112869605, 1.000000000000000000, 0.9238795325112869605, 1.000000000000000000, 0.9238795325112869605, 1.000000000000000000, 0.9238795325112869605, 1.000000000000000000, 0.9238795325112869605, 1.000000000000000000, 0.9238795325112869605, 1.000000000000000000, 0.9238795325112869605, 1.000000000000000000, 0.9238795325112869605, 1.000000000000000000, 0.9238795325112869605, 1.000000000000000000, 0.9238795325112869605, 1.000000000000000000, 0.9238795325112869605, 1.000000000000000000, 0.9238795325112869605, 1.000000000000000000, 0.9238795325112869605, 1.000000000000000000, 0.9238795325112869605, 1.000000000000000000, 0.9238795325112869605, 1.000000000000000000, 0.9238795325112869605, 1.000000000000000000, 0.9238795325112869605, 1.000000000000000000, 0.9238795325112869605, 1.000000000000000000, 0.9238795325112869605, 1.000000000000000000, 0.9238795325112869605, 1.000000000000000000, 0.9238795325112869605, 1.000000000000000000, 0.9238795325112869605, 1.000000000000000000, 0.9238795325112869605, 1.000000000000000000, 0.9238795325112869605, 1.000000000000000000, 0.9238795325112869605, 1.000000000000000000, 0.9238795325112869605, 1.000000000000000000, 0.9238795325112869605, 1.000000000000000000, 0.9238795325112869605, 1.000000000000000000, 0.9238795325112869605, 1.000000000000000000, 0.9238795325112869605, 1.000000000000000000, 0.9238795325112869605, 1.000000000000000000, 0.9238795325112869605, 1.000000000000000000, 0.9238795325112869605, 1.000000000000000000, 0.9238795325112869605, 1.000000000000000000, 0.9238795325112869605, 1.000000000000000000, 0.9238795325112869605, 1.000000000000000000, 0.9238795325112869605, 1.000000000000000000, 0.9238795325112869605, 1.000000000000000000, 0.9238795325112869605, 1.000000000000000000, 0.9238795325112869605, 1.000000000000000000, 0.9238795325112869605, 1.000000000000000000, 0.9238795325112869605, 1.000000000000000000, 0.9238795325112869605, 1.000000000000000000, 0.9238795325112869605, 1.000000000000000000, 0.9238795325112869605, 1.000000000000000000, 0.9238795325112869605, 1.000000000000000000, 0.9238795325112869605, 1.000000000000000000, 0.9238795325112869605, 1.000000000000000000, 0.9238795325112869605, 1.000000000000000000, 0.9238795325112869605, 1.000000000000000000, 0.9238795325112869605, 1.000000000000000000, 0.9238795325112869605, 1.000000000000000000, 0.9238795325112869605, 1.000000000000000000, 0.9238795325112869605, 1.000000000000000000, 0.9238795325112869605, 1.000000000000000000, 0.9238795325112869605, 1.000000000000000000, 0.9238795325112869605, 1.000000000000000000, 0.9238795325112869605, 1.000000000000000000, 0.9238795325112869605, 1.000000000000000000, 0.9238795325112869605, 1.000000000000000000, 0.9238795325112869605, 1.000000000000000000, 0.9238795325112869605, 1.000000000000000000, 0.9238795325112869605, 1.000000000000000000, 0.9238795325112869605, 1.000000000000000000, 0.9238795325112869605, 1.000000000000000000, 0.9238795325112869605, 1.000000000000000000, 0.9238795325112869605, 1.000000000000000000, 0.9238795325112869605, 1.000000000000000000, 0.9238795325112869605, 1.000000000000000000, 0.9238795325112869605, 1.000000000000000000, 0.9238795325112869605, 1.000000000000000000, 0.9238795325112869605, 1.000000000000000000, 0.9238795325112869605, 1.000000000000000000, 0.9238795325112869605, 1.000000000000000000, 0.9238795325112869605, 1.000000000000000000, 0.9238795325112869605, 1.000000000000000000, 0.9238795325112869605, 1.000000000000000000, 0.9238795325112869605, 1.000000000000000000, 0.9238795325112869605, 1.000000000000000000, 0.9238795325112869605, 1.000000000000000000, 0.9238795325112869605, 1.000000000000000000, 0.9238795325112869605, 1.000000000000000000, 0.9238795325112869605, 1.000000000000000000, 0.9238795325112869605, 1.000000000000000000, 0.9238795325112869605, 1.000000000000000000, 0.9238795325112869605, 1.000000000000000000, 0.9238795325112869605, 1.000000000000000000, 0.9238795325112869605, 1.000000000000000000, 0.9238795325112869605, 1.000000000000000000, 0.9238795325112869605, 1.000000000000000000, 0.9238795325112869605, 1.000000000000000000, 0.9238795325112869605, 1.000000000000000000, 0.9238795325112869605, 1.000000000000000000, 0.9238795325112869605, 1.000000000000000000, 0.9238795325112869605, 1.000000000000000000, 0.9238795325112869605, 1.000000000000000000, 0.9238795325112869605, 1.000000000000000000, 0.9238795325112869605, 1.000000000000000000, 0.9238795325112869605, 1.000000000000000000, 0.9238795325112869605, 1.000000000000000000, 0.9238795325112869605, 1.000000000000000000, 0.9238795325112869605, 1.000000000000000000, 0.9238795325112869605, 1.000000000000000000, 0.9238795325112869605, 1.000000000000000000, 0.9238795325112869605, 1.000000000000000000, 0.9238795325112869605, 1.000000000000000000, 0.9238795325112869605, 1.000000000000000000, 0.9238795325112869605, 1.000000000000000000, 0.9238795325112869605, 1.000000000000000000, 0.9238795325112869605, 1.000000000000000000, 0.9238795325112869605, 1.000000000000000000, 0.9238795325112869605, 1.000000000000000000, 0.9238795325112869605, 1.000000000000000000, 0.9238795325112869605, 1.000000000000000000, 0.9238795325112869605, 1.000000000000000000, 0.9238795325112869605, 1.000000000000000000, 0.9238795325112869605, 1.000000000000000000, 0.9238795325112869605, 1.000000000000000000, 0.9238795325112869605, 1.000000000000000000, 0.9238795325112869605, 1.000000000000000000, 0.9238795325112869605, 1.000000000000000000, 0.9238795325112869605, 1.000000000000000000, 0.9238795325112869605, 1.000000000000000000, 0.9238795325112869605, 1.000000000000000000, 0.9238795325112869605, 1.000000000000000000, 0.9238795325112869605, 1.000000000000000000, 0.9238795325112869605, 1.000000000000000000, 0.9238795325112869605, 1.000000000000000000, 0.9238795325112869605, 1.000000000000000000, 0.9238795325112869605, 1.000000000000000000, 0.9238795325112869605, 1.000000000000000000, 0.9238795325112869605, 1.000000000000000000, 0.9238795325112869605, 1.000000000000000000, 0.9238795325112869605, 1.000000000000000000, 0.9238795325112869605, 1.000000000000000000, 0.9238795325112869605, 1.000000000000000000, 0.9238795325112869605, 1.000000000000000000, 0.9238795325112869605, 1.000000000000000000, 0.9238795325112869605, 1.000000000000000000, 0.9238795325112869605, 1.000000000000000000, 0.9238795325112869605, 1.000000000000000000, 0.9238795325112869605, 1.000000000000000000, 0.9238795325112869605, 1.000000000000000000, 0.9238795325112869605, 1.000000000000000000, 0.9238795325112869605, 1.000000000000000000, 0.9238795325112869605, 1.000000000000000000, 0.9238795325112869605, 1.000000000000000000, 0.9238795325112869605, 1.000000000000000000, 0.9238795325112869605, 1.000000000000000000, 0.9238795325112869605, 1.000000000000000000, 0.9238795325112869605, 1.000000000000000000, 0.9238795325112869605, 1.000000000000000000, 0.9238795325112869605, 1.000000000000000000, 0.9238795325112869605, 1.000000000000000000, 0.9238795325112869605, 1.000000000000000000, 0.9238795325112869605, 1.000000000000000000, 0.9238795325112869605, 1.000000000000000000, 0.9238795325112869605, 1.000000000000000000, 0.9238795325112869605, 1.000000000000000000, 0.9238795325112869605, 1.000000000000000000, 0.9238795325112869605, 1.000000000000000000, 0.9238795325112869605, 1.000000000000000000, 0.9238795325112869605, 1.000000000000000000, 0.9238795325112869605, 1.000000000000000000, 0.9238795325112869605, 1.000000000000000000, 0.9238795325112869605, 1.000000000000000000, 0.9238795325112869605, 1.000000000000000000, 0.9238795325112869605, 1.000000000000000000, 0.9238795325112869605, 1.000000000000000000, 0.9238795325112869605, 1.000000000000000000, 0.9238795325112869605, 1.000000000000000000, 0.9238795325112869605, 1.000000000000000000, 0.9238795325112869605, 1.000000000000000000, 0.9238795325112869605, 1.000000000000000000, 0.9238795325112869605, 1.000000000000000000, 0.9238795325112869605, 1.000000000000000000, 0.9238795325112869605, 1.000000000000000000, 0.9238795325112869605, 1.000000000000000000, 0.9238795325112869605, 1.000000000000000000, 0.9238795325112869605, 1.000000000000000000, 0.9238795325112869605, 1.000000000000000000, 0.9238795325112869605, 1.000000000000000000, 0.9238795325112869605, 1.000000000000000000, 0.9238795325112869605, 1.000000000000000000, 0.9238795325112869605, 1.000000000000000000, 0.9238795325112869605, 1.000000000000000000, 0.9238795325112869605, 1.000000000000000000, 0.9238795325112869605, 1.000000000000000000, 0.9238795325112869605, 1.000000000000000000, 0.9238795325112869605, 1.000000000000000000, 0.9238795325112869605, 1.000000000000000000, 0.9238795325112869605, 1.000000000000000000, 0.9238795325112869605, 1.000000000000000000, 0.9238795325112869605, 1.000000000000000000, 0.9238795325112869605, 1.000000000000000000, 0.9238795325112869605, 1.000000000000000000, 0.9238795325112869605, 1.000000000000000000, 0.9238795325112869605, 1.000000000000000000, 0.9238795325112869605, 1.000000000000000000, 0.9238795325112869605, 1.000000000000000000, 0.9238795325112869605, 1.000000000000000000),
 ( 1.000000000000000000, 0.9238795325112869605, 1.000000000000000000, 0.9238795325112869605, 1.000000000000000000, 0.9238795325112869605, 1.000000000000000000, 0.9238795325112869605, 1.000000000000000000, 0.9238795325112869605, 1.000000000000000000, 0.9238795325112869605, 1.000000000000000000, 0.9238795325112869605, 1.000000000000000000, 0.9238795325112869605, 1.000000000000000000, 0.9238795325112869605, 1.000000000000000000, 0.9238795325112869605, 1.000000000000000000, 0.9238795325112869605, 1.000000000000000000, 0.9238795325112869605, 1.000000000000000000, 0.9238795325112869605, 1.000000000000000000, 0.9238795325112869605, 1.000000000000000000, 0.9238795325112869605, 1.000000000000000000, 0.9238795325112869605, 1.000000000000000000, 0.9238795325112869605, 1.000000000000000000, 0.9238795325112869605, 1.000000000000000000, 0.9238795325112869605, 1.000000000000000000, 0.9238795325112869605, 1.000000000000000000, 0.9238795325112869605, 1.000000000000000000, 0.9238795325112869605, 1.000000000000000000, 0.9238795325112869605, 1.000000000000000000, 0.9238795325112869605, 1.000000000000000000, 0.9238795325112869605, 1.000000000000000000, 0.9238795325112869605, 1.000000000000000000, 0.9238795325112869605, 1.000000000000000000, 0.9238795325112869605, 1.000000000000000000, 0.9238795325112869605, 1.000000000000000000, 0.9238795325112869605, 1.000000000000000000, 0.9238795325112869605, 1.000000000000000000, 0.9238795325112869605, 1.000000000000000000, 0.9238795325112869605, 1.000000000000000000, 0.9238795325112869605, 1.000000000000000000, 0.9238795325112869605, 1.000000000000000000, 0.9238795325112869605, 1.000000000000000000, 0.9238795325112869605, 1.000000000000000000, 0.9238795325112869605, 1.000000000000000000, 0.9238795325112869605, 1.000000000000000000, 0.9238795325112869605, 1.000000000000000000, 0.9238795325112869605, 1.000000000000000000, 0.9238795325112869605, 1.000000000000000000, 0.9238795325112869605, 1.000000000000000000, 0.9238795325112869605, 1.000000000000000000, 0.9238795325112869605, 1.000000000000000000, 0.9238795325112869605, 1.000000000000000000, 0.9238795325112869605, 1.000000000000000000, 0.9238795325112869605, 1.000000000000000000, 0.9238795325112869605, 1.000000000000000000, 0.9238795325112869605, 1.000000000000000000, 0.9238795325112869605, 1.000000000000000000, 0.9238795325112869605, 1.000000000000000000, 0.9238795325112869605, 1.000000000000000000, 0.9238795325112869605, 1.000000000000000000, 0.9238795325112869605, 1.000000000000000000, 0.9238795325112869605, 1.000000000000000000, 0.9238795325112869605, 1.000000000000000000, 0.9238795325112869605, 1.000000000000000000, 0.9238795325112869605, 1.000000000000000000, 0.9238795325112869605, 1.000000000000000000, 0.9238795325112869605, 1.000000000000000000, 0.9238795325112869605, 1.000000000000000000, 0.9238795325112869605, 1.000000000000000000, 0.9238795325112869605, 1.000000000000000000, 0.9238795325112869605, 1.000000000000000000, 0.9238795325112869605, 1.000000000000000000, 0.9238795325112869605, 1.000000000000000000, 0.9238795325112869605, 1.000000000000000000, 0.9238795325112869605, 1.000000000000000000, 0.9238795325112869605, 1.000000000000000000, 0.9238795325112869605, 1.000000000000000000, 0.9238795325112869605, 1.000000000000000000, 0.9238795325112869605, 1.000000000000000000, 0.9238795325112869605, 1.000000000000000000, 0.9238795325112869605, 1.000000000000000000, 0.9238795325112869605, 1.000000000000000000, 0.9238795325112869605, 1.000000000000000000, 0.9238795325112869605, 1.000000000000000000, 0.9238795325112869605, 1.000000000000000000, 0.9238795325112869605, 1.000000000000000000, 0.9238795325112869605, 1.000000000000000000, 0.9238795325112869605, 1.000000000000000000, 0.9238795325112869605, 1.000000000000000000, 0.9238795325112869605, 1.000000000000000000, 0.9238795325112869605, 1.000000000000000000, 0.9238795325112869605, 1.000000000000000000, 0.9238795325112869605, 1.000000000000000000, 0.9238795325112869605, 1.000000000000000000, 0.9238795325112869605, 1.000000000000000000, 0.9238795325112869605, 1.000000000000000000, 0.9238795325112869605, 1.000000000000000000, 0.9238795325112869605, 1.000000000000000000, 0.9238795325112869605, 1.000000000000000000, 0.9238795325112869605, 1.000000000000000000, 0.9238795325112869605, 1.000000000000000000, 0.9238795325112869605, 1.000000000000000000, 0.9238795325112869605, 1.000000000000000000, 0.9238795325112869605, 1.000000000000000000, 0.9238795325112869605, 1.000000000000000000, 0.9238795325112869605, 1.000000000000000000, 0.9238795325112869605, 1.000000000000000000, 0.9238795325112869605, 1.000000000000000000, 0.9238795325112869605, 1.000000000000000000, 0.9238795325112869605, 1.000000000000000000, 0.9238795325112869605, 1.000000000000000000, 0.9238795325112869605, 1.000000000000000000, 0.9238795325112869605, 1.000000000000000000, 0.9238795325112869605, 1.000000000000000000, 0.9238795325112869605, 1.000000000000000000, 0.9238795325112869605, 1.000000000000000000, 0.9238795325112869605, 1.000000000000000000, 0.9238795325112869605, 1.000000000000000000, 0.9238795325112869605, 1.000000000000000000, 0.9238795325112869605, 1.000000000000000000, 0.9238795325112869605, 1.000000000000000000, 0.9238795325112869605, 1.000000000000000000, 0.9238795325112869605, 1.000000000000000000, 0.9238795325112869605, 1.000000000000000000, 0.9238795325112869605, 1.000000000000000000, 0.9238795325112869605, 1.000000000000000000, 0.9238795325112869605, 1.000000000000000000, 0.9238795325112869605, 1.000000000000000000, 0.9238795325112869605, 1.000000000000000000, 0.9238795325112869605, 1.000000000000000000, 0.9238795325112869605, 1.000000000000000000, 0.9238795325112869605, 1.000000000000000000, 0.9238795325112869605, 1.000000000000000000, 0.9238795325112869605, 1.000000000000000000, 0.9238795325112869605, 1.000000000000000000, 0.9238795325112869605, 1.000000000000000000, 0.9238795325112869605, 1.000000000000000000, 0.9238795325112869605, 1.000000000000000000, 0.9238795325112869605, 1.000000000000000000, 0.9238795325112869605, 1.000000000000000000, 0.9238795325112869605, 1.000000000000000000, 0.9238795325112869605, 1.000000000000000000, 0.9238795325112869605, 1.000000000000000000, 0.9238795325112869605, 1.000000000000000000, 0.9238795325112869605, 1.000000000000000000, 0.9238795325112869605, 1.000000000000000000, 0.9238795325112869605, 1.000000000000000000, 0.9238795325112869605, 1.000000000000000000, 0.9238795325112869605, 1.000000000000000000, 0.9238795325112869605, 1.000000000000000000, 0.9238795325112869605, 1.000000000000000000, 0.9238795325112869605, 1.000000000000000000, 0.9238795325112869605, 1.000000000000000000, 0.9238795325112869605, 1.000000000000000000, 0.9238795325112869605, 1.000000000000000000, 0.9238795325112869605, 1.000000000000000000, 0.9238795325112869605, 1.000000000000000000, 0.9238795325112869605, 1.000000000000000000, 0.9238795325112869605, 1.000000000000000000, 0.9238795325112869605, 1.000000000000000000, 0.9238795325112869605, 1.000000000000000000, 0.9238795325112869605, 1.000000000000000000, 0.9238795325112869605, 1.000000000000000000, 0.9238795325112869605, 1.000000000000000000, 0.9238795325112869605, 1.000000000000000000, 0.9238795325112869605, 1.000000000000000000, 0.9238795325112869605, 1.000000000000000000, 0.9238795325112869605, 1.000000000000000000, 0.9238795325112869605, 1.000000000000000000, 0.9238795325112869605, 1.000000000000000000, 0.9238795325112869605, 1.000000000000000000, 0.9238795325112869605, 1.000000000000000000, 0.9238795325112869605, 1.000000000000000000, 0.9238795325112869605, 1.000000000000000000, 0.9238795325112869605, 1.000000000000000000, 0.9238795325112869605, 1.000000000000000000, 0.9238795325112869605, 1.000000000000000000, 0.9238795325112869605, 1.000000000000000000, 0.9238795325112869605, 1.000000000000000000, 0.9238795325112869605, 1.000000000000000000, 0.9238795325112869605, 1.000000000000000000, 0.9238795325112869605, 1.000000000000000000, 0.9238795325112869605, 1.000000000000000000, 0.9238795325112869605, 1.000000000000000000, 0.9238795325112869605, 1.000000000000000000, 0.9238795325112869605, 1.000000000000000000, 0.9238795325112869605, 1.000000000000000000, 0.9238795325112869605, 1.000000000000000000, 0.9238795325112869605, 1.000000000000000000, 0.9238795325112869605, 1.000000000000000000, 0.9238795325112869605, 1.000000000000000000, 0.9238795325112869605, 1.000000000000000000, 0.9238795325112869605, 1.000000000000000000, 0.9238795325112869605, 1.000000000000000000, 0.9238795325112869605, 1.000000000000000000, 0.9238795325112869605, 1.000000000000000000, 0.9238795325112869605, 1.000000000000000000, 0.9238795325112869605, 1.000000000000000000, 0.9238795325112869605, 1.000000000000000000, 0.9238795325112869605, 1.000000000000000000, 0.9238795325112869605, 1.000000000000000000, 0.9238795325112869605, 1.000000000000000000, 0.9238795325112869605, 1.000000000000000000, 0.9238795325112869605, 1.000000000000000000, 0.9238795325112869605, 1.000000000000000000, 0.9238795325112869605, 1.000000000000000000, 0.9238795325112869605, 1.000000000000000000, 0.9238795325112869605, 1.000000000000000000, 0.9238795325112869605, 1.000000000000000000, 0.9238795325112869605, 1.000000000000000000, 0.9238795325112869605, 1.000000000000000000, 0.9238795325112869605, 1.000000000000000000, 0.9238795325112869605, 1.000000000000000000, 0.9238795325112869605, 1.000000000000000000, 0.9238795325112869605, 1.000000000000000000, 0.9238795325112869605, 1.000000000000000000, 0.9238795325112869605, 1.000000000000000000, 0.9238795325112869605, 1.000000000000000000, 0.9238795325112869605, 1.000000000000000000, 0.9238795325112869605, 1.000000000000000000, 0.9238795325112869605, 1.000000000000000000, 0.9238795325112869605, 1.000000000000000000, 0.9238795325112869605, 1.000000000000000000, 0.9238795325112869605, 1.000000000000000000, 0.9238795325112869605, 1.000000000000000000, 0.9238795325112869605, 1.000000000000000000, 0.9238795325112869605, 1.000000000000000000, 0.9238795325112869605, 1.000000000000000000, 0.9238795325112869605, 1.000000000000000000, 0.9238795325112869605, 1.000000000000000000, 0.9238795325112869605, 1.000000000000000000, 0.9238795325112869605, 1.000000000000000000, 0.9238795325112869605, 1.000000000000000000, 0.9238795325112869605, 1.000000000000000000, 0.9238795325112869605, 1.000000000000000000, 0.9238795325112869605, 1.000000000000000000, 0.9238795325112869605, 1.000000000000000000, 0.9238795325112869605, 1.000000000000000000, 0.9238795325112869605, 1.000000000000000000, 0.9238795325112869605, 1.000000000000000000, 0.9238795325112869605, 1.000000000000000000, 0.9238795325112869605, 1.000000000000000000, 0.9238795325112869605, 1.000000000000000000, 0.9238795325112869605, 1.000000000000000000, 0.9238795325112869605, 1.000000000000000000, 0.9238795325112869605, 1.000000000000000000, 0.9238795325112869605, 1.000000000000000000, 0.9238795325112869605, 1.000000000000000000, 0.9238795325112869605, 1.000000000000000000, 0.9238795325112869605, 1.000000000000000000, 0.9238795325112869605, 1.000000000000000000, 0.9238795325112869605, 1.000000000000000000, 0.9238795325112869605, 1.000000000000000000, 0.9238795325112869605, 1.000000000000000000, 0.9238795325112869605, 1.000000000000000000, 0.9238795325112869605, 1.000000000000000000, 0.9238795325112869605, 1.000000000000000000, 0.9238795325112869605, 1.000000000000000000, 0.9238795325112869605, 1.000000000000000000, 0.9238795325112869605, 1.000000000000000000, 0.9238795325112869605, 1.000000000000000000, 0.9238795325112869605, 1.000000000000000000, 0.9238795325112869605, 1.000000000000000000, 0.9238795325112869605, 1.000000000000000000, 0.9238795325112869605, 1.000000000000000000, 0.9238795325112869605, 1.000000000000000000, 0.9238795325112869605, 1.000000000000000000, 0.9238795325112869605, 1.000000000000000000, 0.9238795325112869605, 1.000000000000000000, 0.9238795325112869605, 1.000000000000000000, 0.9238795325112869605, 1.000000000000000000, 0.9238795325112869605, 1.000000000000000000, 0.9238795325112869605, 1.000000000000000000, 0.9238795325112869605, 1.000000000000000000, 0.9238795325112869605, 1.000000000000000000, 0.9238795325112869605, 1.000000000000000000, 0.9238795325112869605, 1.000000000000000000, 0.9238795325112869605, 1.000000000000000000, 0.9238795325112869605, 1.000000000000000000, 0.9238795325112869605, 1.000000000000000000, 0.9238795325112869605, 1.000000000000000000, 0.9238795325112869605, 1.000000000000000000, 0.9238795325112869605, 1.000000000000000000, 0.9238795325112869605, 1.000000000000000000, 0.9238795325112869605, 1.000000000000000000, 0.9238795325112869605, 1.000000000000000000, 0.9238795325112869605, 1.000000000000000000, 0.9238795325112869605, 1.000000000000000000, 0.9238795325112869605, 1.000000000000000000, 0.9238795325112869605, 1.000000000000000000, 0.9238795325112869605, 1.000000000000000000, 0.9238795325112869605, 1.000000000000000000, 0.9238795325112869605, 1.000000000000000000, 0.9238795325112869605, 1.000000000000000000, 0.9238795325112869605, 1.000000000000000000, 0.9238795325112869605, 1.000000000000000000, 0.9238795325112869605, 1.000000000000000000, 0.9238795325112869605, 1.000000000000000000, 0.9238795325112869605, 1.000000000000000000, 0.9238795325112869605, 1.000000000000000000, 0.9238795325112869605, 1.000000000000000000, 0.9238795325112869605, 1.000000000000000000, 0.9238795325112869605, 1.000000000000000000, 0.9238795325112869605, 1.000000000000000000, 0.9238795325112869605, 1.000000000000000000, 0.9238795325112869605, 1.000000000000000000, 0.9238795325112869605, 1.000000000000000000, 0.9238795325112869605, 1.000000000000000000, 0.9238795325112869605, 1.000000000000000000, 0.9238795325112869605, 1.000000000000000000, 0.9238795325112869605, 1.000000000000000000, 0.9238795325112869605, 1.000000000000000000, 0.9238795325112869605, 1.000000000000000000, 0.9238795325112869605, 1.000000000000000000, 0.9238795325112869605, 1.000000000000000000, 0.9238795325112869605, 1.000000000000000000, 0.9238795325112869605, 1.000000000000000000, 0.9238795325112869605, 1.000000000000000000, 0.9238795325112869605, 1.000000000000000000, 0.9238795325112869605, 1.000000000000000000, 0.9238795325112869605, 1.000000000000000000, 0.9238795325112869605, 1.000000000000000000, 0.9238795325112869605, 1.000000000000000000, 0.9238795325112869605, 1.000000000000000000, 0.9238795325112869605, 1.000000000000000000, 0.9238795325112869605, 1.000000000000000000, 0.9238795325112869605, 1.000000000000000000, 0.9238795325112869605, 1.000000000000000000, 0.9238795325112869605, 1.000000000000000000, 0.9238795325112869605, 1.000000000000000000, 0.9238795325112869605, 1.000000000000000000, 0.9238795325112869605, 1.000000000000000000, 0.9238795325112869605, 1.000000000000000000, 0.9238795325112869605, 1.000000000000000000, 0.9238795325112869605, 1.000000000000000000, 0.9238795325112869605, 1.000000000000000000, 0.9238795325112869605, 1.000000000000000000, 0.9238795325112869605, 1.000000000000000000, 0.9238795325112869605, 1.000000000000000000, 0.9238795325112869605, 1.000000000000000000, 0.9238795325112869605, 1.000000000000000000, 0.9238795325112869605, 1.000000000000000000, 0.9238795325112869605, 1.000000000000000000, 0.9238795325112869605, 1.000000000000000000, 0.9238795325112869605, 1.000000000000000000, 0.9238795325112869605, 1.000000000000000000, 0.9238795325112869605, 1.000000000000000000, 0.9238795325112869605, 1.000000000000000000, 0.9238795325112869605, 1.000000000000000000, 0.9238795325112869605, 1.000000000000000000, 0.9238795325112869605, 1.000000000000000000, 0.9238795325112869605, 1.000000000000000000, 0.9238795325112869605, 1.000000000000000000, 0.9238795325112869605, 1.000000000000000000, 0.9238795325112869605, 1.000000000000000000, 0.9238795325112869605, 1.000000000000000000, 0.9238795325112869605, 1.000000000000000000, 0.9238795325112869605, 1.000000000000000000, 0.9238795325112869605, 1.000000000000000000, 0.9238795325112869605, 1.000000000000000000, 0.9238795325112869605, 1.000000000000000000, 0.9238795325112869605, 1.000000000000000000, 0.9238795325112869605, 1.000000000000000000, 0.9238795325112869605, 1.000000000000000000, 0.9238795325112869605, 1.000000000000000000, 0.9238795325112869605, 1.000000000000000000, 0.9238795325112869605, 1.000000000000000000, 0.9238795325112869605, 1.000000000000000000, 0.9238795325112869605, 1.000000000000000000, 0.9238795325112869605, 1.000000000000000000, 0.9238795325112869605, 1.000000000000000000, 0.9238795325112869605, 1.000000000000000000, 0.9238795325112869605, 1.000000000000000000, 0.9238795325112869605, 1.000000000000000000, 0.9238795325112869605, 1.000000000000000000, 0.9238795325112869605, 1.000000000000000000, 0.9238795325112869605, 1.000000000000000000, 0.9238795325112869605, 1.000000000000000000, 0.9238795325112869605, 1.000000000000000000, 0.9238795325112869605, 1.000000000000000000, 0.9238795325112869605, 1.000000000000000000, 0.9238795325112869605, 1.000000000000000000, 0.9238795325112869605, 1.000000000000000000, 0.9238795325112869605, 1.000000000000000000, 0.9238795325112869605, 1.000000000000000000, 0.9238795325112869605, 1.000000000000000000, 0.9238795325112869605, 1.000000000000000000, 0.9238795325112869605, 1.000000000000000000, 0.9238795325112869605, 1.000000000000000000, 0.9238795325112869605, 1.000000000000000000, 0.9238795325112869605, 1.000000000000000000, 0.9238795325112869605, 1.000000000000000000, 0.9238795325112869605, 1.000000000000000000, 0.9238795325112869605, 1.000000000000000000, 0.9238795325112869605, 1.000000000000000000, 0.9238795325112869605, 1.000000000000000000, 0.9238795325112869605, 1.000000000000000000, 0.9238795325112869605, 1.000000000000000000, 0.9238795325112869605, 1.000000000000000000, 0.9238795325112869605, 1.000000000000000000, 0.9238795325112869605, 1.000000000000000000, 0.9238795325112869605, 1.000000000000000000, 0.9238795325112869605, 1.000000000000000000, 0.9238795325112869605, 1.000000000000000000, 0.9238795325112869605, 1.000000000000000000, 0.9238795325112869605, 1.000000000000000000),
 ( 1.000000000000000000, 0.9238795325112869605, 1.000000000000000000, 0.9238795325112869605, 1.000000000000000000, 0.9238795325112869605, 1.000000000000000000, 0.9238795325112869605, 1.000000000000000000, 0.9238795325112869605, 1.000000000000000000, 0.9238795325112869605, 1.000000000000000000, 0.9238795325112869605, 1.000000000000000000, 0.9238795325112869605, 1.000000000000000000, 0.9238795325112869605, 1.000000000000000000, 0.9238795325112869605, 1.000000000000000000, 0.9238795325112869605, 1.000000000000000000, 0.9238795325112869605, 1.000000000000000000, 0.9238795325112869605, 1.000000000000000000, 0.9238795325112869605, 1.000000000000000000, 0.9238795325112869605, 1.000000000000000000, 0.9238795325112869605, 1.000000000000000000, 0.9238795325112869605, 1.000000000000000000, 0.9238795325112869605, 1.000000000000000000, 0.9238795325112869605, 1.000000000000000000, 0.9238795325112869605, 1.000000000000000000, 0.9238795325112869605, 1.000000000000000000, 0.9238795325112869605, 1.000000000000000000, 0.9238795325112869605, 1.000000000000000000, 0.9238795325112869605, 1.000000000000000000, 0.9238795325112869605, 1.000000000000000000, 0.9238795325112869605, 1.000000000000000000, 0.9238795325112869605, 1.000000000000000000, 0.9238795325112869605, 1.000000000000000000, 0.9238795325112869605, 1.000000000000000000, 0.9238795325112869605, 1.000000000000000000, 0.9238795325112869605, 1.000000000000000000, 0.9238795325112869605, 1.000000000000000000, 0.9238795325112869605, 1.000000000000000000, 0.9238795325112869605, 1.000000000000000000, 0.9238795325112869605, 1.000000000000000000, 0.9238795325112869605, 1.000000000000000000, 0.9238795325112869605, 1.000000000000000000, 0.9238795325112869605, 1.000000000000000000, 0.9238795325112869605, 1.000000000000000000, 0.9238795325112869605, 1.000000000000000000, 0.9238795325112869605, 1.000000000000000000, 0.9238795325112869605, 1.000000000000000000, 0.9238795325112869605, 1.000000000000000000, 0.9238795325112869605, 1.000000000000000000, 0.9238795325112869605, 1.000000000000000000, 0.9238795325112869605, 1.000000000000000000, 0.9238795325112869605, 1.000000000000000000, 0.9238795325112869605, 1.000000000000000000, 0.9238795325112869605, 1.000000000000000000, 0.9238795325112869605, 1.000000000000000000, 0.9238795325112869605, 1.000000000000000000, 0.9238795325112869605, 1.000000000000000000, 0.9238795325112869605, 1.000000000000000000, 0.9238795325112869605, 1.000000000000000000, 0.9238795325112869605, 1.000000000000000000, 0.9238795325112869605, 1.000000000000000000, 0.9238795325112869605, 1.000000000000000000, 0.9238795325112869605, 1.000000000000000000, 0.9238795325112869605, 1.000000000000000000, 0.9238795325112869605, 1.000000000000000000, 0.9238795325112869605, 1.000000000000000000, 0.9238795325112869605, 1.000000000000000000, 0.9238795325112869605, 1.000000000000000000, 0.9238795325112869605, 1.000000000000000000, 0.9238795325112869605, 1.000000000000000000, 0.9238795325112869605, 1.000000000000000000, 0.9238795325112869605, 1.000000000000000000, 0.9238795325112869605, 1.000000000000000000, 0.9238795325112869605, 1.000000000000000000, 0.9238795325112869605, 1.000000000000000000, 0.9238795325112869605, 1.000000000000000000, 0.9238795325112869605, 1.000000000000000000, 0.9238795325112869605, 1.000000000000000000, 0.9238795325112869605, 1.000000000000000000, 0.9238795325112869605, 1.000000000000000000, 0.9238795325112869605, 1.000000000000000000, 0.9238795325112869605, 1.000000000000000000, 0.9238795325112869605, 1.000000000000000000, 0.9238795325112869605, 1.000000000000000000, 0.9238795325112869605, 1.000000000000000000, 0.9238795325112869605, 1.000000000000000000, 0.9238795325112869605, 1.000000000000000000, 0.9238795325112869605, 1.000000000000000000, 0.9238795325112869605, 1.000000000000000000, 0.9238795325112869605, 1.000000000000000000, 0.9238795325112869605, 1.000000000000000000, 0.9238795325112869605, 1.000000000000000000, 0.9238795325112869605, 1.000000000000000000, 0.9238795325112869605, 1.000000000000000000, 0.9238795325112869605, 1.000000000000000000, 0.9238795325112869605, 1.000000000000000000, 0.9238795325112869605, 1.000000000000000000, 0.9238795325112869605, 1.000000000000000000, 0.9238795325112869605, 1.000000000000000000, 0.9238795325112869605, 1.000000000000000000, 0.9238795325112869605, 1.000000000000000000, 0.9238795325112869605, 1.000000000000000000, 0.9238795325112869605, 1.000000000000000000, 0.9238795325112869605, 1.000000000000000000, 0.9238795325112869605, 1.000000000000000000, 0.9238795325112869605, 1.000000000000000000, 0.9238795325112869605, 1.000000000000000000, 0.9238795325112869605, 1.000000000000000000, 0.9238795325112869605, 1.000000000000000000, 0.9238795325112869605, 1.000000000000000000, 0.9238795325112869605, 1.000000000000000000, 0.9238795325112869605, 1.000000000000000000, 0.9238795325112869605, 1.000000000000000000, 0.9238795325112869605, 1.000000000000000000, 0.9238795325112869605, 1.000000000000000000, 0.9238795325112869605, 1.000000000000000000, 0.9238795325112869605, 1.000000000000000000, 0.9238795325112869605, 1.000000000000000000, 0.9238795325112869605, 1.000000000000000000, 0.9238795325112869605, 1.000000000000000000, 0.9238795325112869605, 1.000000000000000000, 0.9238795325112869605, 1.000000000000000000, 0.9238795325112869605, 1.000000000000000000, 0.9238795325112869605, 1.000000000000000000, 0.9238795325112869605, 1.000000000000000000, 0.9238795325112869605, 1.000000000000000000, 0.9238795325112869605, 1.000000000000000000, 0.9238795325112869605, 1.000000000000000000, 0.9238795325112869605, 1.000000000000000000, 0.9238795325112869605, 1.000000000000000000, 0.9238795325112869605, 1.000000000000000000, 0.9238795325112869605, 1.000000000000000000, 0.9238795325112869605, 1.000000000000000000, 0.9238795325112869605, 1.000000000000000000, 0.9238795325112869605, 1.000000000000000000, 0.9238795325112869605, 1.000000000000000000, 0.9238795325112869605, 1.000000000000000000, 0.9238795325112869605, 1.000000000000000000, 0.9238795325112869605, 1.000000000000000000, 0.9238795325112869605, 1.000000000000000000, 0.9238795325112869605, 1.000000000000000000, 0.9238795325112869605, 1.000000000000000000, 0.9238795325112869605, 1.000000000000000000, 0.9238795325112869605, 1.000000000000000000, 0.9238795325112869605, 1.000000000000000000, 0.9238795325112869605, 1.000000000000000000, 0.9238795325112869605, 1.000000000000000000, 0.9238795325112869605, 1.000000000000000000, 0.9238795325112869605, 1.000000000000000000, 0.9238795325112869605, 1.000000000000000000, 0.9238795325112869605, 1.000000000000000000, 0.9238795325112869605, 1.000000000000000000, 0.9238795325112869605, 1.000000000000000000, 0.9238795325112869605, 1.000000000000000000, 0.9238795325112869605, 1.000000000000000000, 0.9238795325112869605, 1.000000000000000000, 0.9238795325112869605, 1.000000000000000000, 0.9238795325112869605, 1.000000000000000000, 0.9238795325112869605, 1.000000000000000000, 0.9238795325112869605, 1.000000000000000000, 0.9238795325112869605, 1.000000000000000000, 0.9238795325112869605, 1.000000000000000000, 0.9238795325112869605, 1.000000000000000000, 0.9238795325112869605, 1.000000000000000000, 0.9238795325112869605, 1.000000000000000000, 0.9238795325112869605, 1.000000000000000000, 0.9238795325112869605, 1.000000000000000000, 0.9238795325112869605, 1.000000000000000000, 0.9238795325112869605, 1.000000000000000000, 0.9238795325112869605, 1.000000000000000000, 0.9238795325112869605, 1.000000000000000000, 0.9238795325112869605, 1.000000000000000000, 0.9238795325112869605, 1.000000000000000000, 0.9238795325112869605, 1.000000000000000000, 0.9238795325112869605, 1.000000000000000000, 0.9238795325112869605, 1.000000000000000000, 0.9238795325112869605, 1.000000000000000000, 0.9238795325112869605, 1.000000000000000000, 0.9238795325112869605, 1.000000000000000000, 0.9238795325112869605, 1.000000000000000000, 0.9238795325112869605, 1.000000000000000000, 0.9238795325112869605, 1.000000000000000000, 0.9238795325112869605, 1.000000000000000000, 0.9238795325112869605, 1.000000000000000000, 0.9238795325112869605, 1.000000000000000000, 0.9238795325112869605, 1.000000000000000000, 0.9238795325112869605, 1.000000000000000000, 0.9238795325112869605, 1.000000000000000000, 0.9238795325112869605, 1.000000000000000000, 0.9238795325112869605, 1.000000000000000000, 0.9238795325112869605, 1.000000000000000000, 0.9238795325112869605, 1.000000000000000000, 0.9238795325112869605, 1.000000000000000000, 0.9238795325112869605, 1.000000000000000000, 0.9238795325112869605, 1.000000000000000000, 0.9238795325112869605, 1.000000000000000000, 0.9238795325112869605, 1.000000000000000000, 0.9238795325112869605, 1.000000000000000000, 0.9238795325112869605, 1.000000000000000000, 0.9238795325112869605, 1.000000000000000000, 0.9238795325112869605, 1.000000000000000000, 0.9238795325112869605, 1.000000000000000000, 0.9238795325112869605, 1.000000000000000000, 0.9238795325112869605, 1.000000000000000000, 0.9238795325112869605, 1.000000000000000000, 0.9238795325112869605, 1.000000000000000000, 0.9238795325112869605, 1.000000000000000000, 0.9238795325112869605, 1.000000000000000000, 0.9238795325112869605, 1.000000000000000000, 0.9238795325112869605, 1.000000000000000000, 0.9238795325112869605, 1.000000000000000000, 0.9238795325112869605, 1.000000000000000000, 0.9238795325112869605, 1.000000000000000000, 0.9238795325112869605, 1.000000000000000000, 0.9238795325112869605, 1.000000000000000000, 0.9238795325112869605, 1.000000000000000000, 0.9238795325112869605, 1.000000000000000000, 0.9238795325112869605, 1.000000000000000000, 0.9238795325112869605, 1.000000000000000000, 0.9238795325112869605, 1.000000000000000000, 0.9238795325112869605, 1.000000000000000000, 0.9238795325112869605, 1.000000000000000000, 0.9238795325112869605, 1.000000000000000000, 0.9238795325112869605, 1.000000000000000000, 0.9238795325112869605, 1.000000000000000000, 0.9238795325112869605, 1.000000000000000000, 0.9238795325112869605, 1.000000000000000000, 0.9238795325112869605, 1.000000000000000000, 0.9238795325112869605, 1.000000000000000000, 0.9238795325112869605, 1.000000000000000000, 0.9238795325112869605, 1.000000000000000000, 0.9238795325112869605, 1.000000000000000000, 0.9238795325112869605, 1.000000000000000000, 0.9238795325112869605, 1.000000000000000000, 0.9238795325112869605, 1.000000000000000000, 0.9238795325112869605, 1.000000000000000000, 0.9238795325112869605, 1.000000000000000000, 0.9238795325112869605, 1.000000000000000000, 0.9238795325112869605, 1.000000000000000000, 0.9238795325112869605, 1.000000000000000000, 0.9238795325112869605, 1.000000000000000000, 0.9238795325112869605, 1.000000000000000000, 0.9238795325112869605, 1.000000000000000000, 0.9238795325112869605, 1.000000000000000000, 0.9238795325112869605, 1.000000000000000000, 0.9238795325112869605, 1.000000000000000000, 0.9238795325112869605, 1.000000000000000000, 0.9238795325112869605, 1.000000000000000000, 0.9238795325112869605, 1.000000000000000000, 0.9238795325112869605, 1.000000000000000000, 0.9238795325112869605, 1.000000000000000000, 0.9238795325112869605, 1.000000000000000000, 0.9238795325112869605, 1.000000000000000000, 0.9238795325112869605, 1.000000000000000000, 0.9238795325112869605, 1.000000000000000000, 0.9238795325112869605, 1.000000000000000000, 0.9238795325112869605, 1.000000000000000000, 0.9238795325112869605, 1.000000000000000000, 0.9238795325112869605, 1.000000000000000000, 0.9238795325112869605, 1.000000000000000000, 0.9238795325112869605, 1.000000000000000000, 0.9238795325112869605, 1.000000000000000000, 0.9238795325112869605, 1.000000000000000000, 0.9238795325112869605, 1.000000000000000000, 0.9238795325112869605, 1.000000000000000000, 0.9238795325112869605, 1.000000000000000000, 0.9238795325112869605, 1.000000000000000000, 0.9238795325112869605, 1.000000000000000000, 0.9238795325112869605, 1.000000000000000000, 0.9238795325112869605, 1.000000000000000000, 0.9238795325112869605, 1.000000000000000000, 0.9238795325112869605, 1.000000000000000000, 0.9238795325112869605, 1.000000000000000000, 0.9238795325112869605, 1.000000000000000000, 0.9238795325112869605, 1.000000000000000000, 0.9238795325112869605, 1.000000000000000000, 0.9238795325112869605, 1.000000000000000000, 0.9238795325112869605, 1.000000000000000000, 0.9238795325112869605, 1.000000000000000000, 0.9238795325112869605, 1.000000000000000000, 0.9238795325112869605, 1.000000000000000000, 0.9238795325112869605, 1.000000000000000000, 0.9238795325112869605, 1.000000000000000000, 0.9238795325112869605, 1.000000000000000000, 0.9238795325112869605, 1.000000000000000000, 0.9238795325112869605, 1.000000000000000000, 0.9238795325112869605, 1.000000000000000000, 0.9238795325112869605, 1.000000000000000000, 0.9238795325112869605, 1.000000000000000000, 0.9238795325112869605, 1.000000000000000000, 0.9238795325112869605, 1.000000000000000000, 0.9238795325112869605, 1.000000000000000000, 0.9238795325112869605, 1.000000000000000000, 0.9238795325112869605, 1.000000000000000000, 0.9238795325112869605, 1.000000000000000000, 0.9238795325112869605, 1.000000000000000000, 0.9238795325112869605, 1.000000000000000000, 0.9238795325112869605, 1.000000000000000000, 0.9238795325112869605, 1.000000000000000000, 0.9238795325112869605, 1.000000000000000000, 0.9238795325112869605, 1.000000000000000000, 0.9238795325112869605, 1.000000000000000000, 0.9238795325112869605, 1.000000000000000000, 0.9238795325112869605, 1.000000000000000000, 0.9238795325112869605, 1.000000000000000000, 0.9238795325112869605, 1.000000000000000000, 0.9238795325112869605, 1.000000000000000000, 0.9238795325112869605, 1.000000000000000000, 0.9238795325112869605, 1.000000000000000000, 0.9238795325112869605, 1.000000000000000000, 0.9238795325112869605, 1.000000000000000000, 0.9238795325112869605, 1.000000000000000000, 0.9238795325112869605, 1.000000000000000000, 0.9238795325112869605, 1.000000000000000000, 0.9238795325112869605, 1.000000000000000000, 0.9238795325112869605, 1.000000000000000000, 0.9238795325112869605, 1.000000000000000000, 0.9238795325112869605, 1.000000000000000000, 0.9238795325112869605, 1.000000000000000000, 0.9238795325112869605, 1.000000000000000000, 0.9238795325112869605, 1.000000000000000000, 0.9238795325112869605, 1.000000000000000000, 0.9238795325112869605, 1.000000000000000000, 0.9238795325112869605, 1.000000000000000000, 0.9238795325112869605, 1.000000000000000000, 0.9238795325112869605, 1.000000000000000000, 0.9238795325112869605, 1.000000000000000000, 0.9238795325112869605, 1.000000000000000000, 0.9238795325112869605, 1.000000000000000000, 0.9238795325112869605, 1.000000000000000000, 0.9238795325112869605, 1.000000000000000000, 0.9238795325112869605, 1.000000000000000000, 0.9238795325112869605, 1.000000000000000000, 0.9238795325112869605, 1.000000000000000000, 0.9238795325112869605, 1.000000000000000000, 0.9238795325112869605, 1.000000000000000000, 0.9238795325112869605, 1.000000000000000000, 0.9238795325112869605, 1.000000000000000000, 0.9238795325112869605, 1.000000000000000000, 0.9238795325112869605, 1.000000000000000000, 0.9238795325112869605, 1.000000000000000000, 0.9238795325112869605, 1.000000000000000000, 0.9238795325112869605, 1.000000000000000000, 0.9238795325112869605, 1.000000000000000000, 0.9238795325112869605, 1.000000000000000000, 0.9238795325112869605, 1.000000000000000000, 0.9238795325112869605, 1.000000000000000000, 0.9238795325112869605, 1.000000000000000000, 0.9238795325112869605, 1.000000000000000000, 0.9238795325112869605, 1.000000000000000000, 0.9238795325112869605, 1.000000000000000000, 0.9238795325112869605, 1.000000000000000000, 0.9238795325112869605, 1.000000000000000000, 0.9238795325112869605, 1.000000000000000000, 0.9238795325112869605, 1.000000000000000000, 0.9238795325112869605, 1.000000000000000000, 0.9238795325112869605, 1.000000000000000000, 0.9238795325112869605, 1.000000000000000000, 0.9238795325112869605, 1.000000000000000000, 0.9238795325112869605, 1.000000000000000000, 0.9238795325112869605, 1.000000000000000000, 0.9238795325112869605, 1.000000000000000000, 0.9238795325112869605, 1.000000000000000000, 0.9238795325112869605, 1.000000000000000000, 0.9238795325112869605, 1.000000000000000000, 0.9238795325112869605, 1.000000000000000000, 0.9238795325112869605, 1.000000000000000000, 0.9238795325112869605, 1.000000000000000000, 0.9238795325112869605, 1.000000000000000000, 0.9238795325112869605, 1.000000000000000000, 0.9238795325112869605, 1.000000000000000000, 0.9238795325112869605, 1.000000000000000000, 0.9238795325112869605, 1.000000000000000000, 0.9238795325112869605, 1.000000000000000000, 0.9238795325112869605, 1.000000000000000000, 0.9238795325112869605, 1.000000000000000000, 0.9238795325112869605, 1.000000000000000000, 0.9238795325112869605, 1.000000000000000000, 0.9238795325112869605, 1.000000000000000000, 0.9238795325112869605, 1.000000000000000000, 0.9238795325112869605, 1.000000000000000000, 0.9238795325112869605, 1.000000000000000000, 0.9238795325112869605, 1.000000000000000000, 0.9238795325112869605, 1.000000000000000000, 0.9238795325112869605, 1.000000000000000000, 0.9238795325112869605, 1.000000000000000000, 0.9238795325112869605, 1.000000000000000000, 0.9238795325112869605, 1.000000000000000000, 0.9238795325112869605, 1.000000000000000000, 0.9238795325112869605, 1.000000000000000000, 0.9238795325112869605, 1.000000000000000000, 0.9238795325112869605, 1.000000000000000000, 0.9238795325112869605, 1.000000000000000000, 0.9238795325112869605, 1.000000000000000000, 0.9238795325112869605, 1.000000000000000000, 0.9238795325112869605, 1.000000000000000000, 0.9238795325112869605, 1.000000000000000000, 0.9238795325112869605, 1.000000000000000000, 0.9238795325112869605, 1.000000000000000000, 0.9238795325112869605, 1.000000000000000000, 0.9238795325112869605, 1.000000000000000000, 0.9238795325112869605, 1.000000000000000000, 0.9238795325112869605, 1.000000000000000000, 0.9238795325112869605, 1.000000000000000000, 0.9238795325112869605, 1.000000000000000000) ) ) 
 REPRESENTATION_ITEM ( '' )  SURFACE ( )  ) ;
#11426 = EDGE_CURVE ( 'NONE', #6306, #40667, #11354, .T. ) ;
#11427 = DIRECTION ( 'NONE',  ( 0.000000000000000000, 0.000000000000000000, 1.000000000000000000 ) ) ;
#11428 = CARTESIAN_POINT ( 'NONE',  ( -0.7185039370078739607, 1.928577636452523993E-17, 0.9350393700787401619 ) ) ;
#11429 = DIRECTION ( 'NONE',  ( -1.000000000000000000, 0.000000000000000000, 0.000000000000000000 ) ) ;
#11430 = CARTESIAN_POINT ( 'NONE',  ( -1.100456976456230270E-17, -1.034492628480683019, -0.1797182628040039365 ) ) ;
#11431 = DIRECTION ( 'NONE',  ( 1.000000000000000000, 0.000000000000000000, -1.822029033848725275E-16 ) ) ;
#11432 = CARTESIAN_POINT ( 'NONE',  ( 1.002407869896990045, 0.1264236179284866091, 0.8981299212060788184 ) ) ;
#11433 = CARTESIAN_POINT ( 'NONE',  ( 0.8759842519685039353, 0.1787899950787401882, 1.331200787347811110 ) ) ;
#11434 = EDGE_CURVE ( 'NONE', #15222, #11894, #14114, .T. ) ;
#11435 = ADVANCED_FACE ( 'NONE', ( #25500 ), #46520, .F. ) ;
#11436 = CARTESIAN_POINT ( 'NONE',  ( 0.8107537697050254399, 0.1574803149606300301, 0.5241141731208195376 ) ) ;
#11437 = CARTESIAN_POINT ( 'NONE',  ( 0.9412147342319837628, 0.1574803149606300301, 1.395177165354331672 ) ) ;
#11439 = LINE ( 'NONE', #29228, #27771 ) ;
#11438 = CARTESIAN_POINT ( 'NONE',  ( 0.7351878293081982596, 0.08236403197891215000, 1.981599075499917095 ) ) ;
#11440 = CARTESIAN_POINT ( 'NONE',  ( 0.7185039370078739607, 1.928577636452523993E-17, 0.4527559054042842868 ) ) ;
#11442 = CARTESIAN_POINT ( 'NONE',  ( 0.1527640389977631963, 0.1049476924225429125, 0.09381581576814683465 ) ) ;
#11441 = CARTESIAN_POINT ( 'NONE',  ( 0.6971942568897648851, 0.07405724077823318263, 0.7874015747493863238 ) ) ;
#11443 = CARTESIAN_POINT ( 'NONE',  ( 0.1787899950787401604, -0.7706692912848194243, 0.07405724077823318263 ) ) ;
#11444 = ORIENTED_EDGE ( 'NONE', *, *, #251, .T. ) ;
#11445 = CARTESIAN_POINT ( 'NONE',  ( -0.9873396505805591694, 0.1113553986120547346, 0.8415354330708662012 ) ) ;
#11446 = LINE ( 'NONE', #37295, #19059 ) ;
#11447 = CARTESIAN_POINT ( 'NONE',  ( 0.8019270111902717657, -0.1787899950787401604, 1.190944881836001112 ) ) ;
#11448 = CARTESIAN_POINT ( 'NONE',  ( -0.1574803149606299191, 0.7443365962042343131, -3.523993443072799270 ) ) ;
#11450 = AXIS2_PLACEMENT_3D ( 'NONE', #22352, #13997, #7281 ) ;
#11449 = CARTESIAN_POINT ( 'NONE',  ( -0.1574803149606299191, -1.602362204724409489, 0.000000000000000000 ) ) ;
#11451 = CARTESIAN_POINT ( 'NONE',  ( -0.9873396505805591694, -0.1113553986120547346, 0.5167322834645668994 ) ) ;
#11452 = ORIENTED_EDGE ( 'NONE', *, *, #35074, .T. ) ;
#11453 = DIRECTION ( 'NONE',  ( 0.000000000000000000, 0.000000000000000000, -1.000000000000000000 ) ) ;
#11454 = CARTESIAN_POINT ( 'NONE',  ( -1.002407869896990045, -0.1264236179284866091, 0.2928149605761578567 ) ) ;
#11455 = EDGE_LOOP ( 'NONE', ( #10728, #14213, #44849, #19890 ) ) ;
#11456 = CARTESIAN_POINT ( 'NONE',  ( 1.033464566929133799, 0.000000000000000000, 1.742125984251968518 ) ) ;
#11457 = CARTESIAN_POINT ( 'NONE',  ( -0.8019270111902717657, 0.1787899950787401604, 1.609251968450173376 ) ) ;
#11458 = CARTESIAN_POINT ( 'NONE',  ( -0.7495606340400177148, 0.1264236179284866091, 0.3961614172690708924 ) ) ;
#11459 = FACE_OUTER_BOUND ( 'NONE', #32987, .T. ) ;
#11460 = LINE ( 'NONE', #25845, #21062 ) ;
#11461 = DIRECTION ( 'NONE',  ( 3.469446951953620894E-15, 1.000000000000000000, 0.000000000000000000 ) ) ;
#11462 = CARTESIAN_POINT ( 'NONE',  ( -0.1787899950787401604, -0.3288641257095537562, 0.07405724077823318263 ) ) ;
#11463 = B_SPLINE_CURVE_WITH_KNOTS ( 'NONE', 3,
 ( #3280, #36374, #10255, #28727, #6399, #17902, #43296, #32552, #3531, #28969, #43769, #21256, #24860, #35880, #20782, #10011, #17664, #47140, #43526, #42795, #39932, #7121, #32312, #10496, #25094, #6871, #10742, #21743 ),
 .UNSPECIFIED., .F., .F.,
 ( 4, 2, 2, 2, 2, 2, 2, 2, 2, 2, 2, 2, 2, 4 ),
 ( 0.000000000000000000, 0.001273870958249984650, 0.001910806437374976867, 0.002547741916499968867, 0.003184677395624961084, 0.003821612874749952433, 0.004458548353874944650, 0.005095483832999936867, 0.005732419312124930819, 0.006369354791249923903, 0.007006290270374916987, 0.007643225749499910938, 0.008917096707749896239, 0.01019096766599988241 ),
 .UNSPECIFIED. ) ;
#11464 = CARTESIAN_POINT ( 'NONE',  ( -0.02294826503924878025, -0.08955989818537933578, 0.2205244489207712766 ) ) ;
#11465 = FACE_OUTER_BOUND ( 'NONE', #16662, .T. ) ;
#11466 = CARTESIAN_POINT ( 'NONE',  ( -0.9412147342319837628, 0.1574803149606300301, 1.975885826664125711 ) ) ;
#11467 = CARTESIAN_POINT ( 'NONE',  ( -0.9500414927467378812, 0.1787899950787401604, 0.3444881889226146243 ) ) ;
#11468 = ORIENTED_EDGE ( 'NONE', *, *, #15210, .T. ) ;
#11469 = ORIENTED_EDGE ( 'NONE', *, *, #28714, .T. ) ;
#11470 = CARTESIAN_POINT ( 'NONE',  ( -1.002407869896990045, -0.1264236179284866091, 1.360728346402929168 ) ) ;
#11471 = VERTEX_POINT ( 'NONE', #39602 ) ;
#11472 = CARTESIAN_POINT ( 'NONE',  ( 0.07405724077823318263, -1.331692913332063855, 0.1787899950787401604 ) ) ;
#11473 = AXIS2_PLACEMENT_3D ( 'NONE', #20398, #35037, #12537 ) ;
#11474 = CARTESIAN_POINT ( 'NONE',  ( -0.1787899950787401604, -1.538385826717890703, -0.07405724077823318263 ) ) ;
#11475 = EDGE_CURVE ( 'NONE', #46256, #8098, #28872, .T. ) ;
#11476 = FACE_OUTER_BOUND ( 'NONE', #23551, .T. ) ;
#11477 = CARTESIAN_POINT ( 'NONE',  ( -2.859251968503937036, 0.000000000000000000, 0.000000000000000000 ) ) ;
#11478 = CARTESIAN_POINT ( 'NONE',  ( 0.7646288533564489232, -0.1113553986120547346, 0.4281496062992125595 ) ) ;
#11479 = DIRECTION ( 'NONE',  ( 0.000000000000000000, 1.000000000000000000, 0.000000000000000000 ) ) ;
#11480 = CARTESIAN_POINT ( 'NONE',  ( -1.033464566929133799, 0.000000000000000000, 1.102362204616881947 ) ) ;
#11481 = CARTESIAN_POINT ( 'NONE',  ( 0.9500414927467378812, 0.1787899950787401604, 0.4281496062454490659 ) ) ;
#11482 = CARTESIAN_POINT ( 'NONE',  ( 1.033464566929133799, 0.000000000000000000, 1.456692913278299084 ) ) ;
#11483 = CARTESIAN_POINT ( 'NONE',  ( -0.06523048226347956391, -0.2563976377952757457, 0.1574803149606297803 ) ) ;
#11484 = VERTEX_POINT ( 'NONE', #22337 ) ;
#11485 = CARTESIAN_POINT ( 'NONE',  ( 0.8107537697050253289, -0.1574803149606297803, 1.995570866034207080 ) ) ;
#11486 = ORIENTED_EDGE ( 'NONE', *, *, #6811, .T. ) ;
#11487 = EDGE_CURVE ( 'NONE', #16814, #23361, #43909, .T. ) ;
#11488 = CARTESIAN_POINT ( 'NONE',  ( -0.1233909491491453209, -0.09102144875556358872, -0.1293981901162606918 ) ) ;
#11489 = CARTESIAN_POINT ( 'NONE',  ( -1.054774247047244540, 0.07405724077823318263, 1.013779527505291878 ) ) ;
#11490 = CARTESIAN_POINT ( 'NONE',  ( 0.9873396505805591694, -0.1113553986120547346, 0.9891732283464568232 ) ) ;
#11491 = LINE ( 'NONE', #22497, #21277 ) ;
#11492 = CARTESIAN_POINT ( 'NONE',  ( -0.1574803149606299191, -0.5688976376877488139, 0.000000000000000000 ) ) ;
#11494 = CARTESIAN_POINT ( 'NONE',  ( 0.8759842519685039353, -0.1574803149606299191, 0.7480314960629921295 ) ) ;
#11493 = DIRECTION ( 'NONE',  ( -0.000000000000000000, -0.000000000000000000, 1.000000000000000000 ) ) ;
#11495 = CARTESIAN_POINT ( 'NONE',  ( -0.1697971239859669412, -0.08954441352768210960, -0.01236366681777519710 ) ) ;
#11496 = CARTESIAN_POINT ( 'NONE',  ( 0.7185039370078739607, 1.928577636452523993E-17, 1.437007873908220601 ) ) ;
#11497 = ORIENTED_EDGE ( 'NONE', *, *, #33595, .T. ) ;
#11498 = CARTESIAN_POINT ( 'NONE',  ( 0.9500414927467378812, -0.1787899950787401604, 0.6446850393163160442 ) ) ;
#11499 = ORIENTED_EDGE ( 'NONE', *, *, #24906, .T. ) ;
#11500 = DIRECTION ( 'NONE',  ( 0.000000000000000000, 0.000000000000000000, -1.000000000000000000 ) ) ;
#11501 = DIRECTION ( 'NONE',  ( 0.000000000000000000, 0.9945218953682737340, 0.1045284632676499459 ) ) ;
#11502 = CARTESIAN_POINT ( 'NONE',  ( -0.1787899950787401882, -1.614665354276944909, 0.000000000000000000 ) ) ;
#11503 = CARTESIAN_POINT ( 'NONE',  ( -1.094772975963752103E-17, -0.6845472440407243120, -0.1787899950787401882 ) ) ;
#11504 = CARTESIAN_POINT ( 'NONE',  ( -9.642888182262618425E-18, -1.218503937007874072, -0.1574803149606299191 ) ) ;
#11505 = CARTESIAN_POINT ( 'NONE',  ( 0.8107537697050253289, 0.1574803149606300301, 1.075295275483024504 ) ) ;
#11506 = CARTESIAN_POINT ( 'NONE',  ( 0.3100393700787401619, 0.000000000000000000, 1.181102362204724310 ) ) ;
#11507 = VECTOR ( 'NONE', #4450, 39.37007874015748143 ) ;
#11508 = ORIENTED_EDGE ( 'NONE', *, *, #30710, .F. ) ;
#11509 = ORIENTED_EDGE ( 'NONE', *, *, #44983, .F. ) ;
#11510 = ORIENTED_EDGE ( 'NONE', *, *, #25210, .F. ) ;
#11511 = CARTESIAN_POINT ( 'NONE',  ( -0.8019270111902717657, 0.1787899950787401604, 1.732283464513166615 ) ) ;
#11512 = CARTESIAN_POINT ( 'NONE',  ( 0.9500414927467378812, -0.1787899950787401604, 1.712598425143087688 ) ) ;
#11513 = CARTESIAN_POINT ( 'NONE',  ( -1.054774247047244540, -0.07405724077823318263, 0.7332677164816707727 ) ) ;
#11514 = CARTESIAN_POINT ( 'NONE',  ( 1.033464566929133799, 0.000000000000000000, 1.781496062992125928 ) ) ;
#11515 = CARTESIAN_POINT ( 'NONE',  ( 0.8759842519685039353, 0.1787899950787401882, 0.3518700786863940833 ) ) ;
#11516 = AXIS2_PLACEMENT_3D ( 'NONE', #8468, #46071, #20439 ) ;
#11517 = DIRECTION ( 'NONE',  ( 0.000000000000000000, 0.000000000000000000, -1.000000000000000000 ) ) ;
#11518 = CARTESIAN_POINT ( 'NONE',  ( -1.054774247047244096, 0.000000000000000000, 1.242618110182456714 ) ) ;
#11519 = CARTESIAN_POINT ( 'NONE',  ( -1.054774247047244096, 0.000000000000000000, 0.8095472440407244230 ) ) ;
#11520 = AXIS2_PLACEMENT_3D ( 'NONE', #27824, #5025, #42384 ) ;
#11521 = CARTESIAN_POINT ( 'NONE',  ( 0.5415383587465882886, -0.09842519685039370636, 0.000000000000000000 ) ) ;
#11522 = DIRECTION ( 'NONE',  ( 0.000000000000000000, 0.000000000000000000, 1.000000000000000000 ) ) ;
#11523 = CARTESIAN_POINT ( 'NONE',  ( -1.002407869896990045, -0.1264236179284866091, 1.596948818843874074 ) ) ;
#11524 = CARTESIAN_POINT ( 'NONE',  ( -0.7185039370078739607, 1.928577636452523993E-17, 1.909448818790110192 ) ) ;
#11525 = ORIENTED_EDGE ( 'NONE', *, *, #29179, .F. ) ;
#11526 = CARTESIAN_POINT ( 'NONE',  ( -0.8107537697050253289, -0.1574803149606297803, 1.611712598425196319 ) ) ;
#11527 = CARTESIAN_POINT ( 'NONE',  ( 0.1885137525767837108, -0.3997902715136080753, -0.9996607721191614893 ) ) ;
#11528 = CARTESIAN_POINT ( 'NONE',  ( 0.6971942568897648851, 0.07405724077823318263, 1.461614173174583753 ) ) ;
#11529 = CARTESIAN_POINT ( 'NONE',  ( 0.1110659630103943002, -0.09851382545259528001, 0.09590396427280079017 ) ) ;
#11530 = DIRECTION ( 'NONE',  ( -0.7071067811865454633, 0.000000000000000000, 0.7071067811865494601 ) ) ;
#11531 = EDGE_LOOP ( 'NONE', ( #45257, #30073, #25689, #40926 ) ) ;
#11532 = ORIENTED_EDGE ( 'NONE', *, *, #220, .F. ) ;
#11533 = ORIENTED_EDGE ( 'NONE', *, *, #9039, .T. ) ;
#11534 = CARTESIAN_POINT ( 'NONE',  ( -0.07405724077823318263, -0.8395669290800948925, -0.1787899950787401604 ) ) ;
#11535 = CARTESIAN_POINT ( 'NONE',  ( 0.1787899950787401604, -0.4606299212060784853, 0.07405724077823318263 ) ) ;
#11536 = CARTESIAN_POINT ( 'NONE',  ( 0.07405724077823318263, -0.9970472440407247561, -0.1787899950787401604 ) ) ;
#11537 = EDGE_CURVE ( 'NONE', #1651, #19863, #29118, .T. ) ;
#11538 = VECTOR ( 'NONE', #14914, 39.37007874015748143 ) ;
#11539 = DIRECTION ( 'NONE',  ( -1.000000000000000000, 0.000000000000000000, 0.000000000000000000 ) ) ;
#11540 = CARTESIAN_POINT ( 'NONE',  ( 1.002407869896990045, -0.1264236179284866091, 1.710137795221826851 ) ) ;
#11541 = CARTESIAN_POINT ( 'NONE',  ( -0.07444174185955065859, -0.3086068017090296545, 0.1797182628040039087 ) ) ;
#11542 = CARTESIAN_POINT ( 'NONE',  ( 0.1113553986120547346, 0.1545275590551181133, -0.1113553986120547346 ) ) ;
#11543 = PRODUCT_DEFINITION_SHAPE ( 'NONE', 'NONE',  #47473 ) ;
#11544 = VECTOR ( 'NONE', #19730, 39.37007874015748143 ) ;
#11545 = CARTESIAN_POINT ( 'NONE',  ( 3.284318927891251994E-17, -0.03494094482812622193, 0.1787899950787401882 ) ) ;
#11546 = EDGE_CURVE ( 'NONE', #16593, #4842, #15957, .T. ) ;
#11547 = CARTESIAN_POINT ( 'NONE',  ( -0.7185039370078746268, 0.06523048226347956391, 1.080216535325543958 ) ) ;
#11548 = CARTESIAN_POINT ( 'NONE',  ( 0.7495606340400177148, 0.1264236179284866091, 0.7849409448281259305 ) ) ;
#11549 = AXIS2_PLACEMENT_3D ( 'NONE', #3198, #46809, #32472 ) ;
#11550 = PRESENTATION_STYLE_ASSIGNMENT (( #4316 ) ) ;
#11552 = CARTESIAN_POINT ( 'NONE',  ( 0.000000000000000000, 0.09842519685039370636, 0.000000000000000000 ) ) ;
#11551 = DIRECTION ( 'NONE',  ( -1.000000000000000000, 0.000000000000000000, 0.000000000000000000 ) ) ;
#11553 = LINE ( 'NONE', #4319, #42971 ) ;
#11554 = CARTESIAN_POINT ( 'NONE',  ( 1.002407869896990045, -0.1264236179284866091, 1.833169291284818758 ) ) ;
#11555 = AXIS2_PLACEMENT_3D ( 'NONE', #11386, #37013, #15461 ) ;
#11556 = DIRECTION ( 'NONE',  ( 0.000000000000000000, 0.000000000000000000, 1.000000000000000000 ) ) ;
#11557 = ORIENTED_EDGE ( 'NONE', *, *, #38937, .F. ) ;
#11558 = CARTESIAN_POINT ( 'NONE',  ( 0.07405724077823318263, -0.2293307086076536994, 0.1787899950787401604 ) ) ;
#11560 = CARTESIAN_POINT ( 'NONE',  ( -0.7185039370078739607, 1.928577636452523993E-17, 1.683070866141732402 ) ) ;
#11559 = CARTESIAN_POINT ( 'NONE',  ( -0.6971942568897626646, -0.07405724077823297447, 0.4035433070328508509 ) ) ;
#11561 = CARTESIAN_POINT ( 'NONE',  ( 3.284318927891251994E-17, -1.171751968450173154, 0.1787899950787401882 ) ) ;
#11562 = CARTESIAN_POINT ( 'NONE',  ( 0.7495606340400177148, 0.1264236179284866091, 0.2386811023084413619 ) ) ;
#11563 = CYLINDRICAL_SURFACE ( 'NONE', #27765, 0.1574803149606299191 ) ;
#11564 = CARTESIAN_POINT ( 'NONE',  ( -0.9500414927467378812, 0.1787899950787401604, 1.801181102308441861 ) ) ;
#11565 = VERTEX_POINT ( 'NONE', #18742 ) ;
#11566 = CARTESIAN_POINT ( 'NONE',  ( -1.054774247047244540, 0.07405724077823318263, 1.210629921206079818 ) ) ;
#11567 = CARTESIAN_POINT ( 'NONE',  ( -1.033464566929133799, 0.000000000000000000, 0.7086614172153071767 ) ) ;
#11568 = CARTESIAN_POINT ( 'NONE',  ( 0.6971942568897637749, 2.189545951927499583E-17, 1.267224409395055096 ) ) ;
#11569 = CARTESIAN_POINT ( 'NONE',  ( 0.6971942568897648851, -0.07405724077823297447, 1.934055118056471567 ) ) ;
#11570 = CARTESIAN_POINT ( 'NONE',  ( -1.054774247047244540, -0.07405724077823318263, 1.082677165300567346 ) ) ;
#11571 = CARTESIAN_POINT ( 'NONE',  ( -0.1247969209625214848, -0.09842895638388027280, -0.1280391975408537442 ) ) ;
#11572 = FACE_OUTER_BOUND ( 'NONE', #1200, .T. ) ;
#11573 = CARTESIAN_POINT ( 'NONE',  ( 0.8759842519685039353, 0.1787899950787401882, 0.4699803149068661479 ) ) ;
#11574 = CARTESIAN_POINT ( 'NONE',  ( -0.8759842519685039353, -0.1787899950787401882, 0.4060039369541102450 ) ) ;
#11575 = CARTESIAN_POINT ( 'NONE',  ( -0.7495606340400177148, -0.1264236179284866091, 0.7947834645131652831 ) ) ;
#11576 = ORIENTED_EDGE ( 'NONE', *, *, #20913, .T. ) ;
#11577 = EDGE_CURVE ( 'NONE', #19741, #11246, #35342, .T. ) ;
#11578 = CARTESIAN_POINT ( 'NONE',  ( -0.2362204724409469325, 2.422684756221293634E-15, 0.9891732283464568232 ) ) ;
#11579 = EDGE_LOOP ( 'NONE', ( #11807, #7408, #6353, #12227 ) ) ;
#11580 = CARTESIAN_POINT ( 'NONE',  ( -1.033464566929134687, 0.06523048226347956391, 0.2091535433070865757 ) ) ;
#11581 = CARTESIAN_POINT ( 'NONE',  ( 0.6971942568897648851, -0.07405724077823297447, 1.072834645615528659 ) ) ;
#11582 = CARTESIAN_POINT ( 'NONE',  ( 0.8107537697050254399, 0.1574803149606300301, 1.941437007766490863 ) ) ;
#11583 = CONICAL_SURFACE ( 'NONE', #39868, 0.09842519685039370636, 0.9599310885968824758 ) ;
#11584 = ORIENTED_EDGE ( 'NONE', *, *, #38703, .F. ) ;
#11585 = AXIS2_PLACEMENT_3D ( 'NONE', #27024, #36839, #23170 ) ;
#11586 = CARTESIAN_POINT ( 'NONE',  ( 0.8759842519685039353, -0.1787899950787401882, 1.941437007820252081 ) ) ;
#11587 = AXIS2_PLACEMENT_3D ( 'NONE', #34729, #41865, #34475 ) ;
#11588 = DIRECTION ( 'NONE',  ( -1.000000000000000000, -5.377642775528100415E-15, 4.197754538034575138E-15 ) ) ;
#11589 = CARTESIAN_POINT ( 'NONE',  ( 0.1787899950787401604, -1.534572787126878390, 0.07405724077823318263 ) ) ;
#11590 = ORIENTED_EDGE ( 'NONE', *, *, #34224, .T. ) ;
#11591 = CARTESIAN_POINT ( 'NONE',  ( -0.07405724077823318263, -0.5049212597887556830, 0.1787899950787401604 ) ) ;
#11592 = EDGE_CURVE ( 'NONE', #43256, #1072, #45563, .T. ) ;
#11593 = CARTESIAN_POINT ( 'NONE',  ( -0.3053278657842537491, -0.05482723079889069429, 0.7175196379025509108 ) ) ;
#11594 = EDGE_CURVE ( 'NONE', #9411, #37983, #24009, .T. ) ;
#11595 = ORIENTED_EDGE ( 'NONE', *, *, #4400, .T. ) ;
#11596 = CARTESIAN_POINT ( 'NONE',  ( 1.002407869896990045, 0.1264236179284866091, 1.129429133804503937 ) ) ;
#11597 = DIRECTION ( 'NONE',  ( 0.000000000000000000, 0.7071067811862592478, 0.7071067811868357866 ) ) ;
#11598 = CARTESIAN_POINT ( 'NONE',  ( 1.229559056033039366E-16, 0.000000000000000000, 0.4931102362204718426 ) ) ;
#11599 = ( BOUNDED_CURVE ( )  B_SPLINE_CURVE ( 2, ( #47418, #16062, #28441, #43254, #18104, #26015, #44426, #26263, #29183, #40825, #28926, #25303, #21941, #36561, #7547, #29424, #39134, #46560, #13295, #34871, #20694, #42487, #6549, #21161, #13062, #5615, #46332, #20464, #31509, #9462, #35336, #17573, #20222, #27699, #24080, #42709, #35099, #42007, #38688, #2477, #5857, #32213, #13516, #2246, #17103, #28149, #9927, #18745, #520, #28636, #47284, #43672, #40071, #25007, #33172, #10405, #294, #29372, #33403, #21650, #18520, #39605, #25246, #32930, #44143, #21401, #36735, #14461, #7723, #43193, #3187, #28875, #3434, #14940, #17815, #25734, #32462, #11114, #40305, #39833, #7488, #29602, #10883, #11342, #10641, #29121, #47041, #22340, #25503, #25955, #36026, #36283, #40534, #7271, #36968, #43912, #32693, #4121, #51, #43433, #6782, #14233, #21889, #7025, #14698, #18048, #36510, #22107, #3665, #3893, #18288, #12287, #19688, #22582, #19217, #15178, #4828, #15652, #45072, #37917, #33876, #19923, #5072, #995, #12535, #34332, #33635, #29821, #19451, #41002, #37428, #15410, #12052, #8910, #44367, #749, #7963, #15887, #26906, #5306, #30290, #26674, #34106, #1233, #1462, #26201, #30057, #16122, #41466, #40767, #11574, #4582, #44599, #37196, #4340, #18973, #23300, #11815, #30744, #44842, #41224, #27155, #8428, #23056, #26439, #8664, #37676, #45317, #41710, #23541, #34555, #30511, #8190, #38142, #22814, #24011, #45543, #46264, #31684, #5549, #35507, #12766, #6479, #21100, #17280, #20159, #42422, #20630, #39069, #1707, #20395, #6239, #16584, #31212, #13459, #45785, #1953, #46025, #34809, #16354, #30977, #2182, #46497, #20864, #12993, #27397, #6010, #27635, #38612, #42188, #13237, #42882, #41941, #9393, #9148, #2412, #28089, #39305, #16804, #31444, #42650, #38843, #2647, #23766, #5790, #31916, #9862, #38375, #27865, #9630, #24247, #35275, #17043, #24474, #13676, #28314, #10092, #24704, #25183, #14168, #40481, #39547, #7206, #33110, #234, #25435, #7436, #17984, #39770, #43375, #25899, #7666, #35738, #6961, #3375, #47224, #32144, #40248, #17510, #22055, #36455, #46735, #21581, #36223, #13920, #32399, #40011, #3838, #28567, #43855, #32637, #14880, #43135, #10339, #35966, #10587, #36679, #24949, #32870, #6720, #18228, #11058, #29307, #3123, #18461, #14407, #23205, #29540, #21335, #29057, #17751, #21828, #43613, #14638, #25673, #10822, #46976, #3609, #44091, #28813, #11287, #7908, #33345, #1181, #941, #30464, #22524, #12234, #45263, #15122, #37140, #44315, #1413, #22282, #11519, #43325, #10526, #29252, #43080, #14351, #3064, #17693, #46923, #26563, #40423, #29484, #4231, #26074, #4007, #25841, #36854, #37553, #7607, #30409, #33518, #18860, #7847, #34227, #18628, #11701, #44027, #26794, #19099, #15780, #40887, #631, #15289, #19583, #1355, #11230, #29940, #44485, #8081, #412, #33993, #15063, #44958, #44724, #29710, #22460, #19342, #44256, #40647, #33766, #12170, #22703, #4716, #37309, #8555, #4458, #877, #15538, #11941, #41351, #41121, #8315, #22945, #23189, #37802, #4955, #42326, #13354, #42076, #42551, #23658, #1836, #34445, #9754, #20286, #38966, #8795, #34693, #6131, #20528, #35401, #30637, #45199, #38034, #16247, #2774, #21718, #36350, #21228, #40138, #36094, #39905, #35633, #47109, #3504, #28942, #46626, #24834, #7338, #39437, #46395, #14299, #32522, #6372, #18117, #35853, #21951, #2542, #32761, #20984, #43270, #21464, #47357, #17170, #3004, #29196, #17397, #32036, #43502, #13811, #28452, #14051, #43021, #13572, #28207, #43743, #17639, #32285, #25566, #42771, #10227, #28699, #9987, #24597, #10713, #25318, #39196, #6614, #17878, #10471, #25068, #39660, #6842, #3253, #30002, #37368, #8139, #15121, #15600, #37617, #34055, #26620, #44787, #26384, #41175, #4289, #4523, #44314, #7665, #694, #22281, #19404, #8375, #44546, #33109, #30463, #36918, #233, #11764, #40480, #4776, #12000, #14879, #1180, #15841, #45021, #11518, #37139, #30236, #29539, #33579, #23005, #37869, #12233, #4072, #29767, #44090, #18920, #11286, #26139, #22762, #26858, #25898, #41417, #15350, #8614, #18685, #33344, #468, #40707, #23253, #7907, #18460, #22523, #940, #40943, #19161, #33822, #24827, #35393, #21222, #35158, #38961, #9516, #32280, #2538, #3001, #45262, #27977, #39430, #6125, #17393, #17635, #20750, #13567, #38743, #32031, #17166, #28694, #27108, #42545, #6608, #31805, #10466, #6365, #9748, #19642, #39190, #20523, #34287, #46389, #24140, #16073, #1412, #2301, #16929, #28203, #42765, #46622, #9982, #2769, #13806, #28448, #43014, #39655, #29433, #36570, #22164, #15013, #10944, #47103, #116, #25563, #10708, #14763, #22408, #587, #11180, #40365, #3956, #7088, #44205, #15243, #21459, #25313, #14293, #7791, #37034, #44433, #36090, #28937, #36345, #3499, #1305, #22889, #23376, #45390, #19763, #4413, #26271, #1064, #4660, #819, #19043, #33710, #34396, #15481, #27226, #44906, #15722, #19287, #31052, #44665, #8500, #40834, #19523, #26506, #12605, #23130, #12119, #33941, #16424, #41066, #4902, #30580, #45144, #12364, #26982, #30820, #41533, #41779, #8740, #1536, #8980, #23601, #38213, #5373, #19994, #34633, #1783, #20934, #31517, #39373, #27467, #34879, #13071, #35107, #17348, #2024, #9933, #16654, #42717, #24539, #9469, #39142, #2484, #27708, #17110, #13300, #6311, #35574, #46100, #5622, #27929, #42492, #31281, #9699, #42960, #6557, #45858, #24313, #46568, #24776, #2717, #31980, #13751, #21167, #20230, #13520, #28392, #2946, #38913, #6074, #10168, #42268, #20699, #24086, #35801, #17581, #32224, #12835, #42015, #35341, #9221, #31752, #46335, #38694, #23839, #38451, #5866, #16873, #2253, #20471, #28154, #25014, #29128, #13993, #40081, #21407, #33180, #40314, #28643, #18525, #29610, #44151, #39843, #18055, #14472, #10891, #43201, #3900, #10412, #301, #58, #36974, #7032, #36742, #25511, #14947, #7497, #14704, #11351, #3196, #22348, #39612, #32702, #6789, #47049, #21659, #25960, #36034, #43919, #17823, #29379, #11124, #43444, #25741, #36518, #22117, #40541, #47292, #7278, #32470, #7731, #21896, #4129, #18753, #36291, #46808, #43682, #14242, #28883, #3443, #10649, #18296, #25254, #3673, #32937, #37204, #44374, #38148, #5313, #1470, #4347, #26682, #4836, #23306, #30518, #37923, #40774, #45081, #19697, #12292, #41009, #26915, #5077, #7970, #37440, #33411, #23065, #33882 ),
 .UNSPECIFIED., .F., .T. ) 
 B_SPLINE_CURVE_WITH_KNOTS ( ( 3, 2, 2, 2, 2, 2, 2, 2, 2, 2, 2, 2, 2, 2, 2, 2, 2, 2, 2, 2, 2, 2, 2, 2, 2, 2, 2, 2, 2, 2, 2, 2, 2, 2, 2, 2, 2, 2, 2, 2, 2, 2, 2, 2, 2, 2, 2, 2, 2, 2, 2, 2, 2, 2, 2, 2, 2, 2, 2, 2, 2, 2, 2, 2, 2, 2, 2, 2, 2, 2, 2, 2, 2, 2, 2, 2, 2, 2, 2, 2, 2, 2, 2, 2, 2, 2, 2, 2, 2, 2, 2, 2, 2, 2, 2, 2, 2, 2, 2, 2, 2, 2, 2, 2, 2, 2, 2, 2, 2, 2, 2, 2, 2, 2, 2, 2, 2, 2, 2, 2, 2, 2, 2, 2, 2, 2, 2, 2, 2, 2, 2, 2, 2, 2, 2, 2, 2, 2, 2, 2, 2, 2, 2, 2, 2, 2, 2, 2, 2, 2, 2, 2, 2, 2, 2, 2, 2, 2, 2, 2, 2, 2, 2, 2, 2, 2, 2, 2, 2, 2, 2, 2, 2, 2, 2, 2, 2, 2, 2, 2, 2, 2, 2, 2, 2, 2, 2, 2, 2, 2, 2, 2, 2, 2, 2, 2, 2, 2, 2, 2, 2, 2, 2, 2, 2, 2, 2, 2, 2, 2, 2, 2, 2, 2, 2, 2, 2, 2, 2, 2, 2, 2, 2, 2, 2, 2, 2, 2, 2, 2, 2, 2, 2, 2, 2, 2, 2, 2, 2, 2, 2, 2, 2, 2, 2, 2, 2, 2, 2, 2, 2, 2, 2, 2, 2, 2, 2, 2, 2, 2, 2, 2, 2, 2, 2, 2, 2, 2, 2, 2, 2, 2, 2, 2, 2, 2, 2, 2, 2, 2, 2, 2, 2, 2, 2, 2, 2, 2, 2, 2, 2, 2, 2, 2, 2, 2, 2, 2, 2, 2, 2, 2, 2, 2, 2, 2, 2, 2, 2, 2, 2, 2, 2, 2, 2, 2, 2, 2, 2, 2, 2, 2, 2, 2, 2, 2, 2, 2, 2, 2, 2, 2, 2, 2, 2, 2, 2, 2, 2, 2, 2, 2, 2, 2, 2, 2, 2, 2, 2, 2, 2, 2, 2, 2, 2, 2, 2, 2, 2, 2, 2, 2, 2, 2, 2, 2, 2, 2, 2, 2, 2, 2, 2, 2, 2, 2, 2, 2, 2, 2, 2, 2, 2, 2, 2, 2, 2, 2, 2, 2, 2, 2, 2, 2, 2, 2, 2, 3 ),
 ( 0.008750000026272800741, 0.01000000000000000021, 0.01250000000000000069, 0.01499999999999999944, 0.01750000000000000167, 0.02000000000000000042, 0.02249999999999999917, 0.02500000000000000139, 0.02750000000000000014, 0.02999999999999999889, 0.03250000000000000111, 0.03500000000000000333, 0.03749999999999999861, 0.04000000000000000083, 0.04249999999999999611, 0.04499999999999999833, 0.04750000000000000056, 0.05000000000000000278, 0.05249999999999999112, 0.05499999999999999334, 0.05749999999999999556, 0.05999999999999999778, 0.06250000000000000000, 0.06500000000000000222, 0.06750000000000000444, 0.07000000000000000666, 0.07249999999999999500, 0.07499999999999999722, 0.07749999999999999944, 0.08000000000000000167, 0.08250000000000000389, 0.08500000000000000611, 0.08749999999999999445, 0.08999999999999999667, 0.09249999999999999889, 0.09500000000000000111, 0.09750000000000000333, 0.1000000000000000056, 0.1024999999999999939, 0.1049999999999999961, 0.1074999999999999983, 0.1100000000000000006, 0.1125000000000000028, 0.1150000000000000050, 0.1174999999999999933, 0.1199999999999999956, 0.1224999999999999978, 0.1250000000000000000, 0.1275000000000000300, 0.1300000000000000044, 0.1325000000000000067, 0.1350000000000000089, 0.1375000000000000111, 0.1400000000000000133, 0.1424999999999999878, 0.1449999999999999900, 0.1474999999999999922, 0.1499999999999999944, 0.1524999999999999967, 0.1549999999999999989, 0.1575000000000000011, 0.1600000000000000033, 0.1625000000000000056, 0.1650000000000000078, 0.1675000000000000100, 0.1700000000000000122, 0.1724999999999999867, 0.1749999999999999889, 0.1774999999999999911, 0.1799999999999999933, 0.1824999999999999956, 0.1849999999999999978, 0.1875000000000000000, 0.1900000000000000022, 0.1925000000000000044, 0.1950000000000000067, 0.1975000000000000089, 0.2000000000000000111, 0.2025000000000000133, 0.2049999999999999878, 0.2074999999999999900, 0.2099999999999999922, 0.2124999999999999944, 0.2149999999999999967, 0.2174999999999999989, 0.2200000000000000011, 0.2225000000000000033, 0.2250000000000000056, 0.2275000000000000078, 0.2300000000000000100, 0.2325000000000000122, 0.2349999999999999867, 0.2374999999999999889, 0.2399999999999999911, 0.2424999999999999933, 0.2449999999999999956, 0.2474999999999999978, 0.2500000000000000000, 0.2525000000000000022, 0.2550000000000000044, 0.2575000000000000067, 0.2600000000000000089, 0.2625000000000000111, 0.2650000000000000133, 0.2675000000000000155, 0.2700000000000000178, 0.2725000000000000755, 0.2750000000000000222, 0.2775000000000000244, 0.2800000000000000266, 0.2824999999999999734, 0.2849999999999999756, 0.2874999999999999778, 0.2899999999999999800, 0.2924999999999999822, 0.2949999999999999845, 0.2974999999999999867, 0.2999999999999999889, 0.3024999999999999911, 0.3049999999999999933, 0.3074999999999999956, 0.3099999999999999978, 0.3125000000000000000, 0.3150000000000000022, 0.3175000000000000044, 0.3200000000000000067, 0.3225000000000000089, 0.3250000000000000111, 0.3275000000000000133, 0.3300000000000000155, 0.3325000000000000178, 0.3350000000000000200, 0.3375000000000000222, 0.3400000000000000244, 0.3425000000000000266, 0.3449999999999999734, 0.3474999999999999756, 0.3499999999999999778, 0.3524999999999999800, 0.3549999999999999822, 0.3574999999999999845, 0.3599999999999999867, 0.3624999999999999889, 0.3649999999999999911, 0.3674999999999999933, 0.3699999999999999956, 0.3724999999999999978, 0.3750000000000000000, 0.3775000000000000022, 0.3800000000000000044, 0.3825000000000000067, 0.3850000000000000089, 0.3875000000000000111, 0.3900000000000000133, 0.3925000000000000155, 0.3950000000000000178, 0.3975000000000000755, 0.4000000000000000222, 0.4025000000000000244, 0.4050000000000000266, 0.4074999999999999734, 0.4099999999999999756, 0.4124999999999999778, 0.4149999999999999800, 0.4174999999999999822, 0.4199999999999999845, 0.4224999999999999867, 0.4249999999999999889, 0.4274999999999999911, 0.4299999999999999933, 0.4324999999999999956, 0.4349999999999999978, 0.4375000000000000000, 0.4400000000000000022, 0.4425000000000000044, 0.4450000000000000067, 0.4475000000000000089, 0.4500000000000000111, 0.4525000000000000133, 0.4550000000000000155, 0.4575000000000000178, 0.4600000000000000200, 0.4625000000000000222, 0.4650000000000000244, 0.4675000000000000266, 0.4699999999999999734, 0.4724999999999999756, 0.4749999999999999778, 0.4774999999999999800, 0.4799999999999999822, 0.4824999999999999845, 0.4849999999999999867, 0.4874999999999999889, 0.4899999999999999911, 0.4924999999999999933, 0.4949999999999999956, 0.4974999999999999978, 0.5000000000000000000, 0.5024999999999999467, 0.5050000000000000044, 0.5074999999999999512, 0.5100000000000000089, 0.5124999999999999556, 0.5150000000000000133, 0.5174999999999999600, 0.5200000000000000178, 0.5224999999999999645, 0.5250000000000000222, 0.5274999999999999689, 0.5300000000000000266, 0.5324999999999999734, 0.5350000000000000311, 0.5374999999999999778, 0.5400000000000000355, 0.5424999999999999822, 0.5450000000000000400, 0.5474999999999999867, 0.5500000000000000444, 0.5524999999999999911, 0.5550000000000000488, 0.5574999999999999956, 0.5600000000000000533, 0.5625000000000000000, 0.5649999999999999467, 0.5675000000000000044, 0.5699999999999999512, 0.5725000000000000089, 0.5749999999999999556, 0.5775000000000000133, 0.5799999999999999600, 0.5825000000000000178, 0.5849999999999999645, 0.5875000000000000222, 0.5899999999999999689, 0.5925000000000000266, 0.5949999999999999734, 0.5975000000000000311, 0.5999999999999999778, 0.6025000000000000355, 0.6049999999999999822, 0.6075000000000000400, 0.6099999999999999867, 0.6125000000000000444, 0.6149999999999999911, 0.6175000000000000488, 0.6199999999999999956, 0.6225000000000000533, 0.6250000000000000000, 0.6274999999999999467, 0.6300000000000000044, 0.6324999999999999512, 0.6350000000000000089, 0.6374999999999999556, 0.6400000000000000133, 0.6424999999999999600, 0.6450000000000000178, 0.6474999999999999645, 0.6500000000000000222, 0.6524999999999999689, 0.6550000000000000266, 0.6574999999999999734, 0.6600000000000000311, 0.6624999999999999778, 0.6650000000000000355, 0.6674999999999999822, 0.6700000000000000400, 0.6724999999999999867, 0.6750000000000000444, 0.6774999999999999911, 0.6800000000000000488, 0.6824999999999999956, 0.6850000000000000533, 0.6875000000000000000, 0.6899999999999999467, 0.6925000000000000044, 0.6949999999999999512, 0.6975000000000000089, 0.6999999999999999556, 0.7025000000000000133, 0.7049999999999999600, 0.7075000000000000178, 0.7099999999999999645, 0.7125000000000000222, 0.7149999999999999689, 0.7175000000000000266, 0.7199999999999999734, 0.7225000000000000311, 0.7249999999999999778, 0.7275000000000000355, 0.7299999999999999822, 0.7325000000000000400, 0.7349999999999999867, 0.7375000000000000444, 0.7399999999999999911, 0.7425000000000000488, 0.7449999999999999956, 0.7475000000000000533, 0.7500000000000000000, 0.7524999999999999467, 0.7550000000000000044, 0.7574999999999999512, 0.7600000000000000089, 0.7624999999999999556, 0.7650000000000000133, 0.7674999999999999600, 0.7700000000000000178, 0.7724999999999999645, 0.7750000000000000222, 0.7774999999999999689, 0.7800000000000000266, 0.7824999999999999734, 0.7850000000000000311, 0.7874999999999999778, 0.7900000000000000355, 0.7924999999999999822, 0.7950000000000000400, 0.7974999999999999867, 0.8000000000000000444, 0.8024999999999999911, 0.8050000000000000488, 0.8074999999999999956, 0.8100000000000000533, 0.8125000000000000000, 0.8149999999999999467, 0.8175000000000000044, 0.8199999999999999512, 0.8225000000000000089, 0.8249999999999999556, 0.8275000000000000133, 0.8299999999999999600, 0.8325000000000000178, 0.8349999999999999645, 0.8375000000000000222, 0.8399999999999999689, 0.8425000000000000266, 0.8449999999999999734, 0.8475000000000000311, 0.8499999999999999778, 0.8525000000000000355, 0.8549999999999999822, 0.8575000000000000400, 0.8599999999999999867, 0.8625000000000000444, 0.8649999999999999911, 0.8675000000000000488, 0.8699999999999999956, 0.8725000000000000533, 0.8750000000000000000, 0.8774999999999999467, 0.8800000000000000044, 0.8824999999999999512, 0.8850000000000000089, 0.8874999999999999556, 0.8900000000000000133, 0.8924999999999999600, 0.8950000000000000178, 0.8974999999999999645, 0.9000000000000000222, 0.9024999999999999689, 0.9050000000000000266, 0.9074999999999999734, 0.9100000000000000311, 0.9124999999999999778, 0.9150000000000000355, 0.9174999999999999822, 0.9200000000000000400, 0.9224999999999999867, 0.9250000000000000444, 0.9274999999999999911, 0.9300000000000000488, 0.9324999999999999956, 0.9350000000000000533, 0.9375000000000000000, 0.9399999999999999467, 0.9425000000000000044, 0.9449999999999999512, 0.9475000000000000089, 0.9499999999999999556, 0.9525000000000000133, 0.9549999999999999600, 0.9575000000000000178, 0.9599999999999999645, 0.9625000000000000222, 0.9649999999999999689, 0.9675000000000000266, 0.9699999999999999734, 0.9725000000000000311, 0.9749999999999999778, 0.9775000000000000355, 0.9799999999999999822, 0.9825000000000000400, 0.9849999999999999867, 0.9875000000000000444, 0.9899999999999999911, 0.9925000000000000488, 0.9949999999999999956, 0.9975000000000000533, 1.000000000000000000 ),
 .UNSPECIFIED. ) 
 CURVE ( )  GEOMETRIC_REPRESENTATION_ITEM ( )  RATIONAL_B_SPLINE_CURVE ( ( 0.9619397662556429252, 0.9619397670556029123, 1.000000000000000000, 0.9238795325112869605, 1.000000000000000000, 0.9238795325112869605, 1.000000000000000000, 0.9238795325112869605, 1.000000000000000000, 0.9238795325112869605, 1.000000000000000000, 0.9238795325112869605, 1.000000000000000000, 0.9238795325112869605, 1.000000000000000000, 0.9238795325112869605, 1.000000000000000000, 0.9238795325112869605, 1.000000000000000000, 0.9238795325112869605, 1.000000000000000000, 0.9238795325112869605, 1.000000000000000000, 0.9238795325112869605, 1.000000000000000000, 0.9238795325112869605, 1.000000000000000000, 0.9238795325112869605, 1.000000000000000000, 0.9238795325112869605, 1.000000000000000000, 0.9238795325112869605, 1.000000000000000000, 0.9238795325112869605, 1.000000000000000000, 0.9238795325112869605, 1.000000000000000000, 0.9238795325112869605, 1.000000000000000000, 0.9238795325112869605, 1.000000000000000000, 0.9238795325112869605, 1.000000000000000000, 0.9238795325112869605, 1.000000000000000000, 0.9238795325112869605, 1.000000000000000000, 0.9238795325112869605, 1.000000000000000000, 0.9238795325112869605, 1.000000000000000000, 0.9238795325112869605, 1.000000000000000000, 0.9238795325112869605, 1.000000000000000000, 0.9238795325112869605, 1.000000000000000000, 0.9238795325112869605, 1.000000000000000000, 0.9238795325112869605, 1.000000000000000000, 0.9238795325112869605, 1.000000000000000000, 0.9238795325112869605, 1.000000000000000000, 0.9238795325112869605, 1.000000000000000000, 0.9238795325112869605, 1.000000000000000000, 0.9238795325112869605, 1.000000000000000000, 0.9238795325112869605, 1.000000000000000000, 0.9238795325112869605, 1.000000000000000000, 0.9238795325112869605, 1.000000000000000000, 0.9238795325112869605, 1.000000000000000000, 0.9238795325112869605, 1.000000000000000000, 0.9238795325112869605, 1.000000000000000000, 0.9238795325112869605, 1.000000000000000000, 0.9238795325112869605, 1.000000000000000000, 0.9238795325112869605, 1.000000000000000000, 0.9238795325112869605, 1.000000000000000000, 0.9238795325112869605, 1.000000000000000000, 0.9238795325112869605, 1.000000000000000000, 0.9238795325112869605, 1.000000000000000000, 0.9238795325112869605, 1.000000000000000000, 0.9238795325112869605, 1.000000000000000000, 0.9238795325112869605, 1.000000000000000000, 0.9238795325112869605, 1.000000000000000000, 0.9238795325112869605, 1.000000000000000000, 0.9238795325112869605, 1.000000000000000000, 0.9238795325112869605, 1.000000000000000000, 0.9238795325112869605, 1.000000000000000000, 0.9238795325112869605, 1.000000000000000000, 0.9238795325112869605, 1.000000000000000000, 0.9238795325112869605, 1.000000000000000000, 0.9238795325112869605, 1.000000000000000000, 0.9238795325112869605, 1.000000000000000000, 0.9238795325112869605, 1.000000000000000000, 0.9238795325112869605, 1.000000000000000000, 0.9238795325112869605, 1.000000000000000000, 0.9238795325112869605, 1.000000000000000000, 0.9238795325112869605, 1.000000000000000000, 0.9238795325112869605, 1.000000000000000000, 0.9238795325112869605, 1.000000000000000000, 0.9238795325112869605, 1.000000000000000000, 0.9238795325112869605, 1.000000000000000000, 0.9238795325112869605, 1.000000000000000000, 0.9238795325112869605, 1.000000000000000000, 0.9238795325112869605, 1.000000000000000000, 0.9238795325112869605, 1.000000000000000000, 0.9238795325112869605, 1.000000000000000000, 0.9238795325112869605, 1.000000000000000000, 0.9238795325112869605, 1.000000000000000000, 0.9238795325112869605, 1.000000000000000000, 0.9238795325112869605, 1.000000000000000000, 0.9238795325112869605, 1.000000000000000000, 0.9238795325112869605, 1.000000000000000000, 0.9238795325112869605, 1.000000000000000000, 0.9238795325112869605, 1.000000000000000000, 0.9238795325112869605, 1.000000000000000000, 0.9238795325112869605, 1.000000000000000000, 0.9238795325112869605, 1.000000000000000000, 0.9238795325112869605, 1.000000000000000000, 0.9238795325112869605, 1.000000000000000000, 0.9238795325112869605, 1.000000000000000000, 0.9238795325112869605, 1.000000000000000000, 0.9238795325112869605, 1.000000000000000000, 0.9238795325112869605, 1.000000000000000000, 0.9238795325112869605, 1.000000000000000000, 0.9238795325112869605, 1.000000000000000000, 0.9238795325112869605, 1.000000000000000000, 0.9238795325112869605, 1.000000000000000000, 0.9238795325112869605, 1.000000000000000000, 0.9238795325112869605, 1.000000000000000000, 0.9238795325112869605, 1.000000000000000000, 0.9238795325112869605, 1.000000000000000000, 0.9238795325112869605, 1.000000000000000000, 0.9238795325112869605, 1.000000000000000000, 0.9238795325112869605, 1.000000000000000000, 0.9238795325112869605, 1.000000000000000000, 0.9238795325112869605, 1.000000000000000000, 0.9238795325112869605, 1.000000000000000000, 0.9238795325112869605, 1.000000000000000000, 0.9238795325112869605, 1.000000000000000000, 0.9238795325112869605, 1.000000000000000000, 0.9238795325112869605, 1.000000000000000000, 0.9238795325112869605, 1.000000000000000000, 0.9238795325112869605, 1.000000000000000000, 0.9238795325112869605, 1.000000000000000000, 0.9238795325112869605, 1.000000000000000000, 0.9238795325112869605, 1.000000000000000000, 0.9238795325112869605, 1.000000000000000000, 0.9238795325112869605, 1.000000000000000000, 0.9238795325112869605, 1.000000000000000000, 0.9238795325112869605, 1.000000000000000000, 0.9238795325112869605, 1.000000000000000000, 0.9238795325112869605, 1.000000000000000000, 0.9238795325112869605, 1.000000000000000000, 0.9238795325112869605, 1.000000000000000000, 0.9238795325112869605, 1.000000000000000000, 0.9238795325112869605, 1.000000000000000000, 0.9238795325112869605, 1.000000000000000000, 0.9238795325112869605, 1.000000000000000000, 0.9238795325112869605, 1.000000000000000000, 0.9238795325112869605, 1.000000000000000000, 0.9238795325112869605, 1.000000000000000000, 0.9238795325112869605, 1.000000000000000000, 0.9238795325112869605, 1.000000000000000000, 0.9238795325112869605, 1.000000000000000000, 0.9238795325112869605, 1.000000000000000000, 0.9238795325112869605, 1.000000000000000000, 0.9238795325112869605, 1.000000000000000000, 0.9238795325112869605, 1.000000000000000000, 0.9238795325112869605, 1.000000000000000000, 0.9238795325112869605, 1.000000000000000000, 0.9238795325112869605, 1.000000000000000000, 0.9238795325112869605, 1.000000000000000000, 0.9238795325112869605, 1.000000000000000000, 0.9238795325112869605, 1.000000000000000000, 0.9238795325112869605, 1.000000000000000000, 0.9238795325112869605, 1.000000000000000000, 0.9238795325112869605, 1.000000000000000000, 0.9238795325112869605, 1.000000000000000000, 0.9238795325112869605, 1.000000000000000000, 0.9238795325112869605, 1.000000000000000000, 0.9238795325112869605, 1.000000000000000000, 0.9238795325112869605, 1.000000000000000000, 0.9238795325112869605, 1.000000000000000000, 0.9238795325112869605, 1.000000000000000000, 0.9238795325112869605, 1.000000000000000000, 0.9238795325112869605, 1.000000000000000000, 0.9238795325112869605, 1.000000000000000000, 0.9238795325112869605, 1.000000000000000000, 0.9238795325112869605, 1.000000000000000000, 0.9238795325112869605, 1.000000000000000000, 0.9238795325112869605, 1.000000000000000000, 0.9238795325112869605, 1.000000000000000000, 0.9238795325112869605, 1.000000000000000000, 0.9238795325112869605, 1.000000000000000000, 0.9238795325112869605, 1.000000000000000000, 0.9238795325112869605, 1.000000000000000000, 0.9238795325112869605, 1.000000000000000000, 0.9238795325112869605, 1.000000000000000000, 0.9238795325112869605, 1.000000000000000000, 0.9238795325112869605, 1.000000000000000000, 0.9238795325112869605, 1.000000000000000000, 0.9238795325112869605, 1.000000000000000000, 0.9238795325112869605, 1.000000000000000000, 0.9238795325112869605, 1.000000000000000000, 0.9238795325112869605, 1.000000000000000000, 0.9238795325112869605, 1.000000000000000000, 0.9238795325112869605, 1.000000000000000000, 0.9238795325112869605, 1.000000000000000000, 0.9238795325112869605, 1.000000000000000000, 0.9238795325112869605, 1.000000000000000000, 0.9238795325112869605, 1.000000000000000000, 0.9238795325112869605, 1.000000000000000000, 0.9238795325112869605, 1.000000000000000000, 0.9238795325112869605, 1.000000000000000000, 0.9238795325112869605, 1.000000000000000000, 0.9238795325112869605, 1.000000000000000000, 0.9238795325112869605, 1.000000000000000000, 0.9238795325112869605, 1.000000000000000000, 0.9238795325112869605, 1.000000000000000000, 0.9238795325112869605, 1.000000000000000000, 0.9238795325112869605, 1.000000000000000000, 0.9238795325112869605, 1.000000000000000000, 0.9238795325112869605, 1.000000000000000000, 0.9238795325112869605, 1.000000000000000000, 0.9238795325112869605, 1.000000000000000000, 0.9238795325112869605, 1.000000000000000000, 0.9238795325112869605, 1.000000000000000000, 0.9238795325112869605, 1.000000000000000000, 0.9238795325112869605, 1.000000000000000000, 0.9238795325112869605, 1.000000000000000000, 0.9238795325112869605, 1.000000000000000000, 0.9238795325112869605, 1.000000000000000000, 0.9238795325112869605, 1.000000000000000000, 0.9238795325112869605, 1.000000000000000000, 0.9238795325112869605, 1.000000000000000000, 0.9238795325112869605, 1.000000000000000000, 0.9238795325112869605, 1.000000000000000000, 0.9238795325112869605, 1.000000000000000000, 0.9238795325112869605, 1.000000000000000000, 0.9238795325112869605, 1.000000000000000000, 0.9238795325112869605, 1.000000000000000000, 0.9238795325112869605, 1.000000000000000000, 0.9238795325112869605, 1.000000000000000000, 0.9238795325112869605, 1.000000000000000000, 0.9238795325112869605, 1.000000000000000000, 0.9238795325112869605, 1.000000000000000000, 0.9238795325112869605, 1.000000000000000000, 0.9238795325112869605, 1.000000000000000000, 0.9238795325112869605, 1.000000000000000000, 0.9238795325112869605, 1.000000000000000000, 0.9238795325112869605, 1.000000000000000000, 0.9238795325112869605, 1.000000000000000000, 0.9238795325112869605, 1.000000000000000000, 0.9238795325112869605, 1.000000000000000000, 0.9238795325112869605, 1.000000000000000000, 0.9238795325112869605, 1.000000000000000000, 0.9238795325112869605, 1.000000000000000000, 0.9238795325112869605, 1.000000000000000000, 0.9238795325112869605, 1.000000000000000000, 0.9238795325112869605, 1.000000000000000000, 0.9238795325112869605, 1.000000000000000000, 0.9238795325112869605, 1.000000000000000000, 0.9238795325112869605, 1.000000000000000000, 0.9238795325112869605, 1.000000000000000000, 0.9238795325112869605, 1.000000000000000000, 0.9238795325112869605, 1.000000000000000000, 0.9238795325112869605, 1.000000000000000000, 0.9238795325112869605, 1.000000000000000000, 0.9238795325112869605, 1.000000000000000000, 0.9238795325112869605, 1.000000000000000000, 0.9238795325112869605, 1.000000000000000000, 0.9238795325112869605, 1.000000000000000000, 0.9238795325112869605, 1.000000000000000000, 0.9238795325112869605, 1.000000000000000000, 0.9238795325112869605, 1.000000000000000000, 0.9238795325112869605, 1.000000000000000000, 0.9238795325112869605, 1.000000000000000000, 0.9238795325112869605, 1.000000000000000000, 0.9238795325112869605, 1.000000000000000000, 0.9238795325112869605, 1.000000000000000000, 0.9238795325112869605, 1.000000000000000000, 0.9238795325112869605, 1.000000000000000000, 0.9238795325112869605, 1.000000000000000000, 0.9238795325112869605, 1.000000000000000000, 0.9238795325112869605, 1.000000000000000000, 0.9238795325112869605, 1.000000000000000000, 0.9238795325112869605, 1.000000000000000000, 0.9238795325112869605, 1.000000000000000000, 0.9238795325112869605, 1.000000000000000000, 0.9238795325112869605, 1.000000000000000000, 0.9238795325112869605, 1.000000000000000000, 0.9238795325112869605, 1.000000000000000000, 0.9238795325112869605, 1.000000000000000000, 0.9238795325112869605, 1.000000000000000000, 0.9238795325112869605, 1.000000000000000000, 0.9238795325112869605, 1.000000000000000000, 0.9238795325112869605, 1.000000000000000000, 0.9238795325112869605, 1.000000000000000000, 0.9238795325112869605, 1.000000000000000000, 0.9238795325112869605, 1.000000000000000000, 0.9238795325112869605, 1.000000000000000000, 0.9238795325112869605, 1.000000000000000000, 0.9238795325112869605, 1.000000000000000000, 0.9238795325112869605, 1.000000000000000000, 0.9238795325112869605, 1.000000000000000000, 0.9238795325112869605, 1.000000000000000000, 0.9238795325112869605, 1.000000000000000000, 0.9238795325112869605, 1.000000000000000000, 0.9238795325112869605, 1.000000000000000000, 0.9238795325112869605, 1.000000000000000000, 0.9238795325112869605, 1.000000000000000000, 0.9238795325112869605, 1.000000000000000000, 0.9238795325112869605, 1.000000000000000000, 0.9238795325112869605, 1.000000000000000000, 0.9238795325112869605, 1.000000000000000000, 0.9238795325112869605, 1.000000000000000000, 0.9238795325112869605, 1.000000000000000000, 0.9238795325112869605, 1.000000000000000000, 0.9238795325112869605, 1.000000000000000000, 0.9238795325112869605, 1.000000000000000000, 0.9238795325112869605, 1.000000000000000000, 0.9238795325112869605, 1.000000000000000000, 0.9238795325112869605, 1.000000000000000000, 0.9238795325112869605, 1.000000000000000000, 0.9238795325112869605, 1.000000000000000000, 0.9238795325112869605, 1.000000000000000000, 0.9238795325112869605, 1.000000000000000000, 0.9238795325112869605, 1.000000000000000000, 0.9238795325112869605, 1.000000000000000000, 0.9238795325112869605, 1.000000000000000000, 0.9238795325112869605, 1.000000000000000000, 0.9238795325112869605, 1.000000000000000000, 0.9238795325112869605, 1.000000000000000000, 0.9238795325112869605, 1.000000000000000000, 0.9238795325112869605, 1.000000000000000000, 0.9238795325112869605, 1.000000000000000000, 0.9238795325112869605, 1.000000000000000000, 0.9238795325112869605, 1.000000000000000000, 0.9238795325112869605, 1.000000000000000000, 0.9238795325112869605, 1.000000000000000000, 0.9238795325112869605, 1.000000000000000000, 0.9238795325112869605, 1.000000000000000000, 0.9238795325112869605, 1.000000000000000000, 0.9238795325112869605, 1.000000000000000000, 0.9238795325112869605, 1.000000000000000000, 0.9238795325112869605, 1.000000000000000000, 0.9238795325112869605, 1.000000000000000000, 0.9238795325112869605, 1.000000000000000000, 0.9238795325112869605, 1.000000000000000000, 0.9238795325112869605, 1.000000000000000000, 0.9238795325112869605, 1.000000000000000000, 0.9238795325112869605, 1.000000000000000000, 0.9238795325112869605, 1.000000000000000000, 0.9238795325112869605, 1.000000000000000000, 0.9238795325112869605, 1.000000000000000000, 0.9238795325112869605, 1.000000000000000000, 0.9238795325112869605, 1.000000000000000000, 0.9238795325112869605, 1.000000000000000000, 0.9238795325112869605, 1.000000000000000000, 0.9238795325112869605, 1.000000000000000000, 0.9238795325112869605, 1.000000000000000000, 0.9238795325112869605, 1.000000000000000000, 0.9238795325112869605, 1.000000000000000000, 0.9238795325112869605, 1.000000000000000000, 0.9238795325112869605, 1.000000000000000000, 0.9238795325112869605, 1.000000000000000000, 0.9238795325112869605, 1.000000000000000000, 0.9238795325112869605, 1.000000000000000000, 0.9238795325112869605, 1.000000000000000000, 0.9238795325112869605, 1.000000000000000000, 0.9238795325112869605, 1.000000000000000000, 0.9238795325112869605, 1.000000000000000000, 0.9238795325112869605, 1.000000000000000000, 0.9238795325112869605, 1.000000000000000000, 0.9238795325112869605, 1.000000000000000000, 0.9238795325112869605, 1.000000000000000000, 0.9238795325112869605, 1.000000000000000000, 0.9238795325112869605, 1.000000000000000000, 0.9238795325112869605, 1.000000000000000000, 0.9238795325112869605, 1.000000000000000000, 0.9238795325112869605, 1.000000000000000000, 0.9238795325112869605, 1.000000000000000000, 0.9238795325112869605, 1.000000000000000000, 0.9238795325112869605, 1.000000000000000000, 0.9238795325112869605, 1.000000000000000000, 0.9238795325112869605, 1.000000000000000000, 0.9238795325112869605, 1.000000000000000000, 0.9238795325112869605, 1.000000000000000000, 0.9238795325112869605, 1.000000000000000000, 0.9238795325112869605, 1.000000000000000000, 0.9238795325112869605, 1.000000000000000000, 0.9238795325112869605, 1.000000000000000000, 0.9238795325112869605, 1.000000000000000000, 0.9238795325112869605, 1.000000000000000000, 0.9238795325112869605, 1.000000000000000000, 0.9238795325112869605, 1.000000000000000000, 0.9238795325112869605, 1.000000000000000000, 0.9238795325112869605, 1.000000000000000000, 0.9238795325112869605, 1.000000000000000000, 0.9238795325112869605, 1.000000000000000000, 0.9238795325112869605, 1.000000000000000000, 0.9238795325112869605, 1.000000000000000000, 0.9238795325112869605, 1.000000000000000000, 0.9238795325112869605, 1.000000000000000000, 0.9238795325112869605, 1.000000000000000000, 0.9238795325112869605, 1.000000000000000000, 0.9238795325112869605, 1.000000000000000000, 0.9238795325112869605, 1.000000000000000000, 0.9238795325112869605, 1.000000000000000000, 0.9238795325112869605, 1.000000000000000000, 0.9238795325112869605, 1.000000000000000000, 0.9238795325112869605, 1.000000000000000000, 0.9238795325112869605, 1.000000000000000000, 0.9238795325112869605, 1.000000000000000000, 0.9238795325112869605, 1.000000000000000000, 0.9238795325112869605, 1.000000000000000000, 0.9238795325112869605, 1.000000000000000000, 0.9238795325112869605, 1.000000000000000000, 0.9238795325112869605, 1.000000000000000000, 0.9238795325112869605, 1.000000000000000000, 0.9238795325112869605, 1.000000000000000000, 0.9238795325112869605, 1.000000000000000000, 0.9238795325112869605, 1.000000000000000000, 0.9238795325112869605, 1.000000000000000000, 0.9238795325112869605, 1.000000000000000000, 0.9238795325112869605, 1.000000000000000000, 0.9238795325112869605, 1.000000000000000000, 0.9238795325112869605, 1.000000000000000000 ) ) 
 REPRESENTATION_ITEM ( '' )  ) ;
#11600 = EDGE_CURVE ( 'NONE', #28962, #18481, #46022, .T. ) ;
#11601 = CARTESIAN_POINT ( 'NONE',  ( 0.01230737760510134012, -0.07955613945526751607, -0.1377952755905511861 ) ) ;
#11602 = CARTESIAN_POINT ( 'NONE',  ( 0.9500414927467378812, -0.1787899950787401604, 1.510826771599780294 ) ) ;
#11603 = CARTESIAN_POINT ( 'NONE',  ( 1.054774247047244540, 0.07405724077823318263, 0.1427165353793072855 ) ) ;
#11604 = CARTESIAN_POINT ( 'NONE',  ( -0.1787899950787401882, 0.1017461105109186970, 0.000000000000000000 ) ) ;
#11605 = CARTESIAN_POINT ( 'NONE',  ( 0.1264236179284866091, -1.678641732229700922, 0.1264236179284866091 ) ) ;
#11606 = PRODUCT_CONTEXT ( 'NONE', #15971, 'mechanical' ) ;
#11607 = EDGE_CURVE ( 'NONE', #26601, #31651, #21245, .T. ) ;
#11608 = TOROIDAL_SURFACE ( 'NONE', #25369, 0.3912448816427699927, 0.04921259842519685318 ) ;
#11609 = CARTESIAN_POINT ( 'NONE',  ( -0.8019270111902716547, -0.1787899950787401604, 0.6446850393163160442 ) ) ;
#11611 = ( NAMED_UNIT ( * ) PLANE_ANGLE_UNIT ( ) SI_UNIT ( $, .RADIAN. ) ) ;
#11610 = CARTESIAN_POINT ( 'NONE',  ( 0.1113553986120547346, -0.5246062992125984925, 0.1113553986120547346 ) ) ;
#11612 = CARTESIAN_POINT ( 'NONE',  ( 0.1797182628040039087, -1.396205226905880226, -0.07444174185955065859 ) ) ;
#11613 = DIRECTION ( 'NONE',  ( 0.000000000000000000, 0.000000000000000000, 1.000000000000000000 ) ) ;
#11614 = CARTESIAN_POINT ( 'NONE',  ( 0.8019270111902717657, -0.1787899950787401604, 1.432086614119464141 ) ) ;
#11615 = CARTESIAN_POINT ( 'NONE',  ( 1.002407869896990045, -0.1264236179284866091, 1.710137795221826851 ) ) ;
#11616 = AXIS2_PLACEMENT_3D ( 'NONE', #16375, #20181, #17531 ) ;
#11617 = VECTOR ( 'NONE', #17985, 39.37007874015748143 ) ;
#11618 = CARTESIAN_POINT ( 'NONE',  ( 0.8107537697050254399, 0.1574803149606300301, 0.1402559055118110520 ) ) ;
#11619 = CARTESIAN_POINT ( 'NONE',  ( -0.9412147342319837628, -0.1574803149606297803, 1.449311023514519681 ) ) ;
#11620 = CARTESIAN_POINT ( 'NONE',  ( -1.181162989532618060E-16, 0.000000000000000000, -0.2952755905511816326 ) ) ;
#11622 = CARTESIAN_POINT ( 'NONE',  ( 0.1787899950787401604, 0.1299212598962831977, 0.07405724077823318263 ) ) ;
#11621 = CARTESIAN_POINT ( 'NONE',  ( 0.1574803149606299191, -0.8248031494987716483, -1.928577636452523993E-17 ) ) ;
#11623 = CARTESIAN_POINT ( 'NONE',  ( -1.033464566929133799, 0.000000000000000000, 1.230314960629921295 ) ) ;
#11624 = CARTESIAN_POINT ( 'NONE',  ( 0.7495606340400177148, 0.1264236179284866091, 0.3124999999462365619 ) ) ;
#11625 = CARTESIAN_POINT ( 'NONE',  ( -0.9873396505805591694, -0.1113553986120547346, 1.727362204616881947 ) ) ;
#11626 = CARTESIAN_POINT ( 'NONE',  ( 0.7185039370078739607, 1.928577636452523993E-17, 0.5413385826771653919 ) ) ;
#11627 = CARTESIAN_POINT ( 'NONE',  ( 0.3980944881889770248, 0.1864803149606327204, 0.7480314960629921295 ) ) ;
#11628 = CARTESIAN_POINT ( 'NONE',  ( -0.7495606340400177148, 0.1264236179284866091, 1.257381889710015743 ) ) ;
#11629 = CARTESIAN_POINT ( 'NONE',  ( 0.7185039370078739607, 1.928577636452523993E-17, 0.6496062991050708391 ) ) ;
#11630 = ORIENTED_EDGE ( 'NONE', *, *, #6428, .T. ) ;
#11631 = LINE ( 'NONE', #29646, #23030 ) ;
#11632 = FACE_OUTER_BOUND ( 'NONE', #28011, .T. ) ;
#11633 = ORIENTED_EDGE ( 'NONE', *, *, #9113, .F. ) ;
#11634 = CARTESIAN_POINT ( 'NONE',  ( 0.1797182628040039087, 0.01619634789726941138, 0.07444174185955046430 ) ) ;
#11635 = CARTESIAN_POINT ( 'NONE',  ( 0.07405724077823318263, -1.252952755851747924, 0.1787899950787401604 ) ) ;
#11636 = CARTESIAN_POINT ( 'NONE',  ( -0.8759842519685039353, -0.1574803149606299191, 0.03937007874015843040 ) ) ;
#11637 = CARTESIAN_POINT ( 'NONE',  ( 0.6971942568897637749, 2.189545951927499583E-17, 1.656003936954110412 ) ) ;
#11638 = CARTESIAN_POINT ( 'NONE',  ( 1.033464566929133799, 0.000000000000000000, 0.5905511809948347235 ) ) ;
#11640 = CARTESIAN_POINT ( 'NONE',  ( 0.9412147342319837628, 0.1574803149606300301, 1.906988188976377563 ) ) ;
#11639 = DIRECTION ( 'NONE',  ( 1.000000000000000000, -3.469446951953626022E-15, -0.000000000000000000 ) ) ;
#11641 = CARTESIAN_POINT ( 'NONE',  ( 0.7185039370078739607, 1.928577636452523993E-17, 1.909448818790110192 ) ) ;
#11642 = CARTESIAN_POINT ( 'NONE',  ( -0.07405724077823318263, -0.1505905511273389341, 0.1787899950787401604 ) ) ;
#11643 = CARTESIAN_POINT ( 'NONE',  ( 0.9873396505805591694, 0.1113553986120547346, 1.304133858160188897 ) ) ;
#11644 = ORIENTED_EDGE ( 'NONE', *, *, #31492, .T. ) ;
#11645 = CARTESIAN_POINT ( 'NONE',  ( -0.8759842519685039353, 0.000000000000000000, 0.000000000000000000 ) ) ;
#11646 = CARTESIAN_POINT ( 'NONE',  ( -0.04509681258129859954, -0.07057211410339614410, 0.2593943580756443712 ) ) ;
#11647 = CARTESIAN_POINT ( 'NONE',  ( 0.8019270111902717657, 0.1787899950787401604, 0.6692913385289144257 ) ) ;
#11648 = CARTESIAN_POINT ( 'NONE',  ( 0.8759842519685039353, -0.1787899950787401882, 0.8833661416785196785 ) ) ;
#11649 = CARTESIAN_POINT ( 'NONE',  ( -0.1574803149606300301, -0.09891732272711858953, -0.06523048226347956391 ) ) ;
#11650 = CARTESIAN_POINT ( 'NONE',  ( -0.6971942568897637749, 2.189545951927499583E-17, 1.345964566875370139 ) ) ;
#11651 = VERTEX_POINT ( 'NONE', #41938 ) ;
#11652 = ADVANCED_FACE ( 'NONE', ( #20392 ), #42420, .T. ) ;
#11653 = VECTOR ( 'NONE', #18017, 39.37007874015748854 ) ;
#11654 = CONICAL_SURFACE ( 'NONE', #13924, 0.08090551181102362266, 0.9599310885968742602 ) ;
#11655 = EDGE_CURVE ( 'NONE', #24265, #6860, #2873, .T. ) ;
#11656 = CARTESIAN_POINT ( 'NONE',  ( -1.054774247047244540, 0.07405724077823318263, 0.3051181101824569919 ) ) ;
#11657 = DIRECTION ( 'NONE',  ( 0.000000000000000000, 0.000000000000000000, 1.000000000000000000 ) ) ;
#11658 = CARTESIAN_POINT ( 'NONE',  ( -7.957671378281915615E-17, 0.1574803149606340824, -0.3937007874015748254 ) ) ;
#11659 = CARTESIAN_POINT ( 'NONE',  ( -0.07405724077823318263, -0.9144940469693966234, 0.1787899950787401604 ) ) ;
#11660 = ORIENTED_EDGE ( 'NONE', *, *, #31147, .T. ) ;
#11661 = FACE_OUTER_BOUND ( 'NONE', #28548, .T. ) ;
#11662 = EDGE_CURVE ( 'NONE', #46614, #42394, #23558, .T. ) ;
#11663 = EDGE_LOOP ( 'NONE', ( #41281, #15030, #23544, #30924, #14040 ) ) ;
#11664 = AXIS2_PLACEMENT_3D ( 'NONE', #9169, #23557, #2203 ) ;
#11665 = AXIS2_PLACEMENT_3D ( 'NONE', #10444, #32497, #29162 ) ;
#11666 = CARTESIAN_POINT ( 'NONE',  ( -0.8107537697050234415, -0.1574803149606297803, 0.2632874014672759722 ) ) ;
#11667 = LINE ( 'NONE', #1800, #10064 ) ;
#11668 = CARTESIAN_POINT ( 'NONE',  ( 0.7185039370078739607, 1.928577636452523993E-17, 1.830708661309795149 ) ) ;
#11669 = CARTESIAN_POINT ( 'NONE',  ( -0.8759842519685039353, 0.1787899950787401882, 0.1943897637257641919 ) ) ;
#11670 = CARTESIAN_POINT ( 'NONE',  ( -0.8107537697050253289, 0.1574803149606300301, 0.8489173228346468258 ) ) ;
#11671 = CARTESIAN_POINT ( 'NONE',  ( -0.5555748031496060557, 0.1864803149606359678, 0.7480314960629921295 ) ) ;
#11672 = CARTESIAN_POINT ( 'NONE',  ( 0.07444174185955046430, -0.9975831796617853353, -0.1797182628040039087 ) ) ;
#11673 = CARTESIAN_POINT ( 'NONE',  ( 1.033464566929133799, 0.000000000000000000, 1.545275590551181244 ) ) ;
#11674 = CARTESIAN_POINT ( 'NONE',  ( -0.7185039370078746268, -0.06523048226347956391, 1.596948818790111080 ) ) ;
#11675 = CARTESIAN_POINT ( 'NONE',  ( 1.054774247047244096, 0.000000000000000000, 0.9719488188438739629 ) ) ;
#11676 = CARTESIAN_POINT ( 'NONE',  ( 0.7495606340400177148, 0.1264236179284866091, 0.1156496062454492185 ) ) ;
#11677 = CARTESIAN_POINT ( 'NONE',  ( 0.9412147342319837628, 0.1574803149606300301, 1.473917322834645605 ) ) ;
#11679 = DIRECTION ( 'NONE',  ( -1.000000000000000000, 0.000000000000000000, 0.000000000000000000 ) ) ;
#11678 = CARTESIAN_POINT ( 'NONE',  ( 0.7126071576447854383, -0.03525399196628299647, 1.983921887778285376 ) ) ;
#11680 = CARTESIAN_POINT ( 'NONE',  ( 0.9873396505805591694, 0.1113553986120547346, 0.3198818896562523606 ) ) ;
#11681 = CARTESIAN_POINT ( 'NONE',  ( -0.1574803149606299191, -0.6870078739082204899, 0.000000000000000000 ) ) ;
#11682 = VECTOR ( 'NONE', #22981, 39.37007874015748143 ) ;
#11684 = CARTESIAN_POINT ( 'NONE',  ( 0.1574803149606299191, 1.928577636452524610E-17, -0.1183602362204724257 ) ) ;
#11683 = CARTESIAN_POINT ( 'NONE',  ( 0.7495606340400177148, 0.1264236179284866091, 0.8636811023084409733 ) ) ;
#11685 = CARTESIAN_POINT ( 'NONE',  ( 0.1787899950787401882, -0.8469488188438739629, -2.189545951927503898E-17 ) ) ;
#11686 = ORIENTED_EDGE ( 'NONE', *, *, #33675, .T. ) ;
#11687 = AXIS2_PLACEMENT_3D ( 'NONE', #15905, #44856, #34574 ) ;
#11689 = DIRECTION ( 'NONE',  ( 1.000000000000000000, -0.000000000000000000, -1.144917494144692682E-16 ) ) ;
#11688 = VECTOR ( 'NONE', #15164, 39.37007874015748854 ) ;
#11690 = CARTESIAN_POINT ( 'NONE',  ( 0.9500414927467378812, 0.1787899950787401604, 1.210629921206079818 ) ) ;
#11691 = DIRECTION ( 'NONE',  ( 0.000000000000000000, 0.000000000000000000, 1.000000000000000000 ) ) ;
#11692 = CARTESIAN_POINT ( 'NONE',  ( -0.1113553986120547346, -1.607283464566929165, -0.1113553986120547346 ) ) ;
#11693 = LINE ( 'NONE', #22213, #10732 ) ;
#11694 = ORIENTED_EDGE ( 'NONE', *, *, #16527, .T. ) ;
#11695 = CARTESIAN_POINT ( 'NONE',  ( -1.054774247047244096, 0.000000000000000000, 0.1796259841982051075 ) ) ;
#11697 = VERTEX_POINT ( 'NONE', #9145 ) ;
#11696 = AXIS2_PLACEMENT_3D ( 'NONE', #30608, #30156, #23867 ) ;
#11698 = CARTESIAN_POINT ( 'NONE',  ( -1.033464566929134687, 0.06523048226347956391, 0.6028543307086614567 ) ) ;
#11699 = CARTESIAN_POINT ( 'NONE',  ( -1.054774247047244540, 0.07405724077823318263, 1.796259842465923073 ) ) ;
#11700 = EDGE_CURVE ( 'NONE', #8495, #5435, #6236, .T. ) ;
#11701 = CARTESIAN_POINT ( 'NONE',  ( -0.6971942568897648851, -0.07405724077823297447, 0.8710629920722218200 ) ) ;
#11702 = CARTESIAN_POINT ( 'NONE',  ( -0.7495606340400177148, -0.1264236179284866091, 0.5241141731745827537 ) ) ;
#11703 = EDGE_CURVE ( 'NONE', #7899, #36581, #2409, .T. ) ;
#11704 = DIRECTION ( 'NONE',  ( 0.000000000000000000, -0.6156614753256598460, -0.7880107536067206819 ) ) ;
#11705 = CARTESIAN_POINT ( 'NONE',  ( 1.033464566929133799, 0.000000000000000000, 0.3937007872940480047 ) ) ;
#11706 = FACE_BOUND ( 'NONE', #31447, .T. ) ;
#11707 = CARTESIAN_POINT ( 'NONE',  ( 1.054774247047244096, 0.000000000000000000, 0.02214566923757503927 ) ) ;
#11708 = CARTESIAN_POINT ( 'NONE',  ( -0.3009843105729483326, 0.07510662309419861848, -0.7260587119189039207 ) ) ;
#11709 = CARTESIAN_POINT ( 'NONE',  ( 0.07405724077823318263, -0.5946121572056172200, 0.1787899950787401604 ) ) ;
#11710 = CARTESIAN_POINT ( 'NONE',  ( -0.1256064272821220407, -0.08955963219184016888, -0.2158613615193716861 ) ) ;
#11711 = CARTESIAN_POINT ( 'NONE',  ( 0.1574803149606300301, 0.04379921270595223126, -0.06523048226347956391 ) ) ;
#11712 = DIRECTION ( 'NONE',  ( 1.000000000000000000, 0.000000000000000000, 0.000000000000000000 ) ) ;
#11713 = EDGE_CURVE ( 'NONE', #13468, #3727, #37048, .T. ) ;
#11714 = EDGE_CURVE ( 'NONE', #32806, #13348, #3675, .T. ) ;
#11715 = CARTESIAN_POINT ( 'NONE',  ( 0.2559055130920101506, -0.08227836217959635934, -0.05504206144341895063 ) ) ;
#11716 = CARTESIAN_POINT ( 'NONE',  ( -1.002407869896990045, -0.1264236179284866091, 0.2928149605761578567 ) ) ;
#11717 = ( BOUNDED_CURVE ( )  B_SPLINE_CURVE ( 2, ( #17429, #46187, #31372, #9311, #16965, #23934, #38995, #35429, #6402 ),
 .UNSPECIFIED., .F., .T. ) 
 B_SPLINE_CURVE_WITH_KNOTS ( ( 3, 2, 2, 2, 3 ),
 ( 0.02500000000000000139, 0.02750000000000000014, 0.02999999999999999889, 0.03250000000000000111, 0.03500000000000000333 ),
 .UNSPECIFIED. ) 
 CURVE ( )  GEOMETRIC_REPRESENTATION_ITEM ( )  RATIONAL_B_SPLINE_CURVE ( ( 1.000000000000000000, 0.9238795325112869605, 1.000000000000000000, 0.9238795325112869605, 1.000000000000000000, 0.9238795325112869605, 1.000000000000000000, 0.9238795325112869605, 1.000000000000000000 ) ) 
 REPRESENTATION_ITEM ( '' )  ) ;
#11718 = CARTESIAN_POINT ( 'NONE',  ( 0.1787899950787401882, -1.768332629646561127, -2.189545951927503898E-17 ) ) ;
#11719 = COLOUR_RGB ( '', 0.40784314, 0.44705882, 0.49803922) ;
#11720 = ORIENTED_EDGE ( 'NONE', *, *, #43269, .F. ) ;
#11721 = CARTESIAN_POINT ( 'NONE',  ( 0.2471922436403682921, -0.09120620265198671472, 0.04599440333040333284 ) ) ;
#11722 = VERTEX_POINT ( 'NONE', #43133 ) ;
#11723 = VERTEX_POINT ( 'NONE', #25897 ) ;
#11724 = CONICAL_SURFACE ( 'NONE', #7864, 0.08090551181102362266, 0.7853981633974511656 ) ;
#11725 = CARTESIAN_POINT ( 'NONE',  ( 3.284318927891251994E-17, -1.334153543253322916, 0.1787899950787401882 ) ) ;
#11726 = CARTESIAN_POINT ( 'NONE',  ( 0.1264236179284866091, -1.521161417269070837, 0.1264236179284866091 ) ) ;
#11727 = FACE_OUTER_BOUND ( 'NONE', #44189, .T. ) ;
#11728 = DIRECTION ( 'NONE',  ( -0.5587636178032998613, -0.8293269677391227335, 2.999999999999999050E-15 ) ) ;
#11729 = CARTESIAN_POINT ( 'NONE',  ( 1.033464566929133799, 0.000000000000000000, 0.5216535433070865757 ) ) ;
#11730 = CARTESIAN_POINT ( 'NONE',  ( -6.728203135043436585E-17, 0.1574803149606340824, -0.4940944881889759444 ) ) ;
#11731 = CARTESIAN_POINT ( 'NONE',  ( -0.8107537697050253289, 0.1574803149606300301, 1.114665354223180804 ) ) ;
#11732 = CARTESIAN_POINT ( 'NONE',  ( 0.8759842519685039353, 0.1787899950787401882, 0.5093503936470236138 ) ) ;
#11733 = CARTESIAN_POINT ( 'NONE',  ( -0.4620708661417322616, 0.9842519685039375910, -0.7135826771653542844 ) ) ;
#11734 = B_SPLINE_CURVE_WITH_KNOTS ( 'NONE', 3,
 ( #45805, #13013, #37695, #27656, #42210, #4848, #9414, #24033, #38637, #30774, #16374, #5809, #1253, #30999, #34126, #30531, #45092 ),
 .UNSPECIFIED., .F., .F.,
 ( 4, 2, 2, 2, 2, 1, 2, 2, 4 ),
 ( 0.000000000000000000, 0.1250000000000007216, 0.1875000000000010825, 0.2500000000000014433, 0.3750000000000018319, 0.4375000000000019984, 0.4687500000000020539, 0.5000000000000019984, 1.000000000000000000 ),
 .UNSPECIFIED. ) ;
#11735 = CARTESIAN_POINT ( 'NONE',  ( 0.7185039370078739607, 1.928577636452523993E-17, 1.909448818790110192 ) ) ;
#11736 = VERTEX_POINT ( 'NONE', #32142 ) ;
#11737 = DIRECTION ( 'NONE',  ( -1.000000000000000000, 0.000000000000000000, 0.000000000000000000 ) ) ;
#11738 = CARTESIAN_POINT ( 'NONE',  ( -0.9500414927467377701, -0.1787899950787401604, 0.9251968503399373711 ) ) ;
#11739 = CARTESIAN_POINT ( 'NONE',  ( 0.9873396505805591694, 0.1113553986120547346, 0.8809055118110236116 ) ) ;
#11740 = DIRECTION ( 'NONE',  ( 0.000000000000000000, -1.000000000000000000, 0.000000000000000000 ) ) ;
#11741 = CARTESIAN_POINT ( 'NONE',  ( 0.9873396505805591694, -0.1113553986120547346, 0.7529527559055118058 ) ) ;
#11742 = CARTESIAN_POINT ( 'NONE',  ( -0.1066054788070368298, -0.08956136665047831347, 0.1197104361589552413 ) ) ;
#11743 = ORIENTED_EDGE ( 'NONE', *, *, #20979, .F. ) ;
#11744 = CARTESIAN_POINT ( 'NONE',  ( 0.1596648500867438869, 0.05551101047364393609, -0.1404739575301623966 ) ) ;
#11745 = CARTESIAN_POINT ( 'NONE',  ( -0.2741699206993517546, 0.1449164722121958904, 0.9603235990907990072 ) ) ;
#11746 = ORIENTED_EDGE ( 'NONE', *, *, #44785, .F. ) ;
#11747 = CARTESIAN_POINT ( 'NONE',  ( -0.9412147342319837628, 0.1574803149606300301, 1.779035432963339769 ) ) ;
#11748 = CARTESIAN_POINT ( 'NONE',  ( 0.7185039370078739607, 1.928577636452523993E-17, 1.161417322727118284 ) ) ;
#11749 = CARTESIAN_POINT ( 'NONE',  ( -0.07405724077823318263, -1.622047244040725866, -0.1787899950787401604 ) ) ;
#11750 = CARTESIAN_POINT ( 'NONE',  ( -0.1787899950787401604, -0.7165354330171036512, -0.07405724077823318263 ) ) ;
#11751 = CARTESIAN_POINT ( 'NONE',  ( 0.1113553986120547346, -1.144685039370078705, -0.1113553986120547346 ) ) ;
#11752 = CARTESIAN_POINT ( 'NONE',  ( 1.033464566929134687, -0.06523048226347956391, 1.060531495955465031 ) ) ;
#11753 = DIRECTION ( 'NONE',  ( -1.000000000000000000, 0.000000000000000000, 0.000000000000000000 ) ) ;
#11754 = CONICAL_SURFACE ( 'NONE', #37744, 0.2114570894355444486, 1.221730476396037490 ) ;
#11755 = ORIENTED_EDGE ( 'NONE', *, *, #18650, .T. ) ;
#11756 = CARTESIAN_POINT ( 'NONE',  ( -0.6971942568897648851, 0.07405724077823318263, 1.697834645615527771 ) ) ;
#11757 = CARTESIAN_POINT ( 'NONE',  ( 0.9500414927467378812, -0.1787899950787401604, 1.633858267662771313 ) ) ;
#11758 = CARTESIAN_POINT ( 'NONE',  ( 0.1614206436753637397, -0.4404907083123212330, -0.9678621058557815848 ) ) ;
#11760 = FACE_OUTER_BOUND ( 'NONE', #20047, .T. ) ;
#11759 = VECTOR ( 'NONE', #4719, 39.37007874015747433 ) ;
#11761 = CARTESIAN_POINT ( 'NONE',  ( -0.8759842519685039353, 0.000000000000000000, 0.000000000000000000 ) ) ;
#11762 = CARTESIAN_POINT ( 'NONE',  ( 0.6971942568897637749, 2.189545951927499583E-17, 0.2436023621509610382 ) ) ;
#11763 = CARTESIAN_POINT ( 'NONE',  ( 0.1574803149606300023, 0.07627223685636330686, -0.1475485644998806023 ) ) ;
#11764 = CARTESIAN_POINT ( 'NONE',  ( -0.6971942568897637749, 2.189545951927499583E-17, 1.222933070812378009 ) ) ;
#11765 = CARTESIAN_POINT ( 'NONE',  ( -0.7495606340400177148, 0.1264236179284866091, 0.9424212597887559051 ) ) ;
#11766 = CARTESIAN_POINT ( 'NONE',  ( -1.054774247047244540, -0.07405724077823318263, 0.06397637789899228433 ) ) ;
#11767 = ADVANCED_FACE ( 'NONE', ( #24948 ), #28811, .T. ) ;
#11768 = CARTESIAN_POINT ( 'NONE',  ( -0.8759842519685039353, 0.000000000000000000, 0.000000000000000000 ) ) ;
#11769 = CARTESIAN_POINT ( 'NONE',  ( -0.7495606340400177148, 0.1264236179284866091, 1.577263779473795369 ) ) ;
#11770 = CARTESIAN_POINT ( 'NONE',  ( -1.033464566929133799, 0.000000000000000000, 1.811023621939716444 ) ) ;
#11771 = ORIENTED_EDGE ( 'NONE', *, *, #16427, .T. ) ;
#11772 = FACE_OUTER_BOUND ( 'NONE', #29279, .T. ) ;
#11773 = CARTESIAN_POINT ( 'NONE',  ( -1.033464566929134687, 0.06523048226347956391, 1.665846456692914312 ) ) ;
#11774 = CYLINDRICAL_SURFACE ( 'NONE', #42713, 0.1574803149606299191 ) ;
#11775 = CARTESIAN_POINT ( 'NONE',  ( 0.8019270111902716547, -0.1787899950787401604, 1.628937007820252303 ) ) ;
#11776 = CARTESIAN_POINT ( 'NONE',  ( 0.02596600997328759458, -0.09851382729582973397, 0.1524084879473496246 ) ) ;
#11777 = CARTESIAN_POINT ( 'NONE',  ( 0.1476377952755906220, 0.3648440108500937140, -3.619166627704267558 ) ) ;
#11778 = EDGE_CURVE ( 'NONE', #8150, #22180, #32635, .T. ) ;
#11779 = CARTESIAN_POINT ( 'NONE',  ( -0.2559086337351289542, 0.02188737959670186695, -0.3144303560290073740 ) ) ;
#11780 = ORIENTED_EDGE ( 'NONE', *, *, #40396, .F. ) ;
#11781 = EDGE_CURVE ( 'NONE', #13902, #20455, #19283, .T. ) ;
#11782 = ORIENTED_EDGE ( 'NONE', *, *, #16203, .F. ) ;
#11783 = ORIENTED_EDGE ( 'NONE', *, *, #1494, .T. ) ;
#11784 = CARTESIAN_POINT ( 'NONE',  ( 0.1787899950787401882, -0.8518700786863936392, -2.189545951927503898E-17 ) ) ;
#11785 = CARTESIAN_POINT ( 'NONE',  ( -0.1264236179284866091, -1.019192913332062966, 0.1264236179284866091 ) ) ;
#11786 = ORIENTED_EDGE ( 'NONE', *, *, #44329, .F. ) ;
#11787 = ( NAMED_UNIT ( * ) SI_UNIT ( $, .STERADIAN. ) SOLID_ANGLE_UNIT ( ) ) ;
#11788 = CARTESIAN_POINT ( 'NONE',  ( 0.6971942568897637749, 2.189545951927499583E-17, 1.774114173174582643 ) ) ;
#11789 = CARTESIAN_POINT ( 'NONE',  ( 0.1797182628040039087, -0.2987642820239903574, 0.07444174185955046430 ) ) ;
#11790 = CARTESIAN_POINT ( 'NONE',  ( -9.642888182262618425E-18, 0.1200787401574803237, -0.1574803149606299191 ) ) ;
#11791 = CARTESIAN_POINT ( 'NONE',  ( -1.033464566929133799, 0.000000000000000000, 0.9055118109160944506 ) ) ;
#11792 = EDGE_CURVE ( 'NONE', #24385, #32150, #29722, .T. ) ;
#11793 = CARTESIAN_POINT ( 'NONE',  ( 0.8019270111902717657, -0.1787899950787401604, 0.8366141731745828647 ) ) ;
#11795 = DIRECTION ( 'NONE',  ( 0.000000000000000000, -1.000000000000000000, 0.000000000000000000 ) ) ;
#11794 = ( NAMED_UNIT ( * ) PLANE_ANGLE_UNIT ( ) SI_UNIT ( $, .RADIAN. ) ) ;
#11796 = CYLINDRICAL_SURFACE ( 'NONE', #8885, 0.1574803149606299191 ) ;
#11797 = DIRECTION ( 'NONE',  ( -0.000000000000000000, 1.000000000000000000, -0.000000000000000000 ) ) ;
#11798 = CARTESIAN_POINT ( 'NONE',  ( 0.8759842519685039353, -0.1787899950787401882, 1.867618110182456714 ) ) ;
#11799 = CARTESIAN_POINT ( 'NONE',  ( 0.9873396505805591694, 0.1113553986120547346, 0.09350393700787401619 ) ) ;
#11800 = DIRECTION ( 'NONE',  ( 0.000000000000000000, -1.000000000000000000, 0.000000000000000000 ) ) ;
#11801 = CARTESIAN_POINT ( 'NONE',  ( -0.1787899950787401882, -0.2810039369541106336, 0.000000000000000000 ) ) ;
#11802 = CARTESIAN_POINT ( 'NONE',  ( 0.1377952755905511861, 0.000000000000000000, -0.2495040853978291451 ) ) ;
#11803 = CARTESIAN_POINT ( 'NONE',  ( 0.1787899950787401882, -1.201279527505291433, -2.189545951927503898E-17 ) ) ;
#11804 = CARTESIAN_POINT ( 'NONE',  ( 1.054774247047244540, 0.07405724077823318263, 0.2657480314422993595 ) ) ;
#11805 = DIRECTION ( 'NONE',  ( -1.000000000000000000, 0.000000000000000000, 0.000000000000000000 ) ) ;
#11806 = CARTESIAN_POINT ( 'NONE',  ( -0.8759842519685039353, 0.1787899950787401882, 1.803641732229700700 ) ) ;
#11807 = ORIENTED_EDGE ( 'NONE', *, *, #20325, .F. ) ;
#11808 = CARTESIAN_POINT ( 'NONE',  ( -0.9500414927467378812, -0.1787899950787401604, 1.358267716481669662 ) ) ;
#11809 = CARTESIAN_POINT ( 'NONE',  ( -0.8107537697050254399, 0.1574803149606300301, 0.8882874015748026819 ) ) ;
#11810 = CARTESIAN_POINT ( 'NONE',  ( 0.7495606340400177148, 0.1264236179284866091, 0.04183070860765386589 ) ) ;
#11811 = CARTESIAN_POINT ( 'NONE',  ( -0.6971942568897648851, -0.07405724077823297447, 1.067913385773007651 ) ) ;
#11812 = CARTESIAN_POINT ( 'NONE',  ( -0.1198507064121036164, -0.09842530151305696473, -0.1326724740186921714 ) ) ;
#11813 = DIRECTION ( 'NONE',  ( 1.000000000000000000, 0.000000000000000000, 0.000000000000000000 ) ) ;
#11814 = CARTESIAN_POINT ( 'NONE',  ( 0.6971942568897637749, 2.189545951927499583E-17, 0.5191929133320630774 ) ) ;
#11815 = CARTESIAN_POINT ( 'NONE',  ( -0.9500414927467377701, 0.1787899950787401604, 0.4232283464029293896 ) ) ;
#11816 = ORIENTED_EDGE ( 'NONE', *, *, #16723, .T. ) ;
#11817 = EDGE_CURVE ( 'NONE', #18659, #6785, #32471, .T. ) ;
#11818 = CARTESIAN_POINT ( 'NONE',  ( -0.9412147342319837628, 0.1574803149606300301, 0.8735236219397174429 ) ) ;
#11819 = CARTESIAN_POINT ( 'NONE',  ( -0.8759842519685039353, 0.1574803149606299191, 0.1377952755905511861 ) ) ;
#11820 = CARTESIAN_POINT ( 'NONE',  ( -0.2183449438721881963, -0.09851385166753484635, -0.1145859995850722346 ) ) ;
#11821 = VERTEX_POINT ( 'NONE', #46734 ) ;
#11822 = ADVANCED_FACE ( 'NONE', ( #6718 ), #9011, .F. ) ;
#11823 = CARTESIAN_POINT ( 'NONE',  ( -0.7185039370078746268, -0.06523048226347956391, 1.291830708661417360 ) ) ;
#11824 = CARTESIAN_POINT ( 'NONE',  ( 0.1586955767088446545, -0.1469626601063630800, -0.02104375706137109892 ) ) ;
#11825 = CARTESIAN_POINT ( 'NONE',  ( -0.8759842519685039353, -0.1787899950787401882, 0.05167322829269314910 ) ) ;
#11826 = CARTESIAN_POINT ( 'NONE',  ( 0.1787899950787401604, -1.450911369804040785, -0.07405724077823318263 ) ) ;
#11827 = EDGE_LOOP ( 'NONE', ( #32231, #43129, #27996, #7922 ) ) ;
#11828 = CARTESIAN_POINT ( 'NONE',  ( 0.000000000000000000, -0.3937007874015748254, 0.000000000000000000 ) ) ;
#11829 = CARTESIAN_POINT ( 'NONE',  ( -0.07405724077823318263, -0.4015748030958427028, -0.1787899950787401604 ) ) ;
#11830 = ORIENTED_EDGE ( 'NONE', *, *, #9491, .F. ) ;
#11831 = CARTESIAN_POINT ( 'NONE',  ( 0.7495606340400177148, -0.1264236179284866091, 1.188484251914740275 ) ) ;
#11832 = CARTESIAN_POINT ( 'NONE',  ( 0.9873396505805591694, 0.1113553986120547346, 1.589566929133858331 ) ) ;
#11833 = DIRECTION ( 'NONE',  ( -0.8191520442889996811, 0.000000000000000000, -0.5735764363510347241 ) ) ;
#11834 = CARTESIAN_POINT ( 'NONE',  ( 0.1787899950787401604, -0.2244094487651340231, 0.07405724077823318263 ) ) ;
#11835 = CARTESIAN_POINT ( 'NONE',  ( 0.6971942568897648851, -0.07405724077823297447, 1.500984251914741607 ) ) ;
#11836 = CARTESIAN_POINT ( 'NONE',  ( -0.1787899950787401882, 0.1411161892510761906, 0.000000000000000000 ) ) ;
#11837 = CARTESIAN_POINT ( 'NONE',  ( 0.1264236179284866091, -1.708169291284818980, -0.1264236179284866091 ) ) ;
#11838 = LINE ( 'NONE', #34587, #6566 ) ;
#11839 = ORIENTED_EDGE ( 'NONE', *, *, #34177, .T. ) ;
#11840 = EDGE_CURVE ( 'NONE', #32303, #47141, #17982, .T. ) ;
#11841 = CARTESIAN_POINT ( 'NONE',  ( -0.8759842519685039353, -0.1787899950787401882, 0.6471456692375747721 ) ) ;
#11843 = CARTESIAN_POINT ( 'NONE',  ( 0.8107537697050234415, -0.1574803149606297803, 0.3026574802074336046 ) ) ;
#11842 = CARTESIAN_POINT ( 'NONE',  ( -9.642888182262618425E-18, -0.7854330708661416693, -0.1574803149606299191 ) ) ;
#11844 = CARTESIAN_POINT ( 'NONE',  ( -0.07444174185955065859, -1.450339085173596443, 0.1797182628040039087 ) ) ;
#11845 = CARTESIAN_POINT ( 'NONE',  ( 0.000000000000000000, 0.000000000000000000, -0.2103840066576717072 ) ) ;
#11846 = CARTESIAN_POINT ( 'NONE',  ( 0.2471922904502826812, 0.08571147543118957934, -0.06121067491484653150 ) ) ;
#11847 = CARTESIAN_POINT ( 'NONE',  ( 0.7495606340400177148, 0.1264236179284866091, 1.769192913332062966 ) ) ;
#11848 = AXIS2_PLACEMENT_3D ( 'NONE', #5161, #22430, #24556 ) ;
#11849 = VECTOR ( 'NONE', #29685, 39.37007874015748854 ) ;
#11850 = CARTESIAN_POINT ( 'NONE',  ( -1.033464566929133799, 0.000000000000000000, 0.6791338582677166613 ) ) ;
#11851 = B_SPLINE_CURVE_WITH_KNOTS ( 'NONE', 3,
 ( #19856, #10019, #34738, #2342, #34483 ),
 .UNSPECIFIED., .F., .F.,
 ( 4, 1, 4 ),
 ( 0.000000000000000000, 0.002020725942163684868, 0.004041451884327374941 ),
 .UNSPECIFIED. ) ;
#11852 = CARTESIAN_POINT ( 'NONE',  ( 0.9873396505805591694, -0.1113553986120547346, 0.9005905510735748853 ) ) ;
#11853 = DIRECTION ( 'NONE',  ( -1.000000000000000000, -0.000000000000000000, 0.000000000000000000 ) ) ;
#11854 = CARTESIAN_POINT ( 'NONE',  ( -0.1113553986120547346, -0.8395669290263306772, 0.1113553986120547346 ) ) ;
#11855 = CARTESIAN_POINT ( 'NONE',  ( 1.054774247047244096, 0.000000000000000000, 0.2977362204186775885 ) ) ;
#11857 = DIRECTION ( 'NONE',  ( 1.000000000000000000, 0.000000000000000000, 0.000000000000000000 ) ) ;
#11856 = CARTESIAN_POINT ( 'NONE',  ( 0.9500414927467377701, -0.1787899950787401604, 1.235236220418678199 ) ) ;
#11858 = DIRECTION ( 'NONE',  ( -1.000000000000000000, 3.469446951953613794E-15, 0.000000000000000000 ) ) ;
#11859 = CARTESIAN_POINT ( 'NONE',  ( -0.6195511811023656223, 0.6102362204724408601, 0.5854071585544579071 ) ) ;
#11860 = CARTESIAN_POINT ( 'NONE',  ( -0.7495606340400177148, 0.1264236179284866091, 1.375492125930488196 ) ) ;
#11861 = CARTESIAN_POINT ( 'NONE',  ( 0.7185039370078746268, -0.06523048226347956391, 0.6520669290263312323 ) ) ;
#11862 = ORIENTED_EDGE ( 'NONE', *, *, #8528, .T. ) ;
#11863 = CARTESIAN_POINT ( 'NONE',  ( -1.033464566929133799, 0.000000000000000000, 1.742125984251968518 ) ) ;
#11864 = CARTESIAN_POINT ( 'NONE',  ( 0.8107537697050254399, 0.1574803149606300301, 0.6914370078740148529 ) ) ;
#11865 = ORIENTED_EDGE ( 'NONE', *, *, #9224, .F. ) ;
#11866 = CARTESIAN_POINT ( 'NONE',  ( -0.1797182628040039365, -0.07976821903186437357, 0.000000000000000000 ) ) ;
#11867 = CARTESIAN_POINT ( 'NONE',  ( 0.1787899950787401604, -1.208661417269070393, 0.07405724077823318263 ) ) ;
#11868 = CARTESIAN_POINT ( 'NONE',  ( 0.008412300615072984891, 0.06606319696301089783, 0.1377952755905512139 ) ) ;
#11869 = CARTESIAN_POINT ( 'NONE',  ( 0.8019270111902717657, 0.1787899950787401604, 1.569881889710015299 ) ) ;
#11870 = CARTESIAN_POINT ( 'NONE',  ( -0.7185039370078746268, -0.06523048226347956391, 1.291830708661417360 ) ) ;
#11871 = CARTESIAN_POINT ( 'NONE',  ( 0.7646288533564489232, 0.1113553986120547346, 0.2509842518609771700 ) ) ;
#11873 = LINE ( 'NONE', #34869, #32355 ) ;
#11872 = CARTESIAN_POINT ( 'NONE',  ( 0.1577586585109163331, -0.1377137394883627131, 0.04231661445894344120 ) ) ;
#11874 = CARTESIAN_POINT ( 'NONE',  ( 0.6971942568897626646, 0.07405724077823318263, 0.04429133852891373180 ) ) ;
#11875 = EDGE_CURVE ( 'NONE', #8777, #8725, #43611, .T. ) ;
#11876 = CARTESIAN_POINT ( 'NONE',  ( 3.284318927891251994E-17, -0.1874999999462366451, 0.1787899950787401882 ) ) ;
#11877 = ORIENTED_EDGE ( 'NONE', *, *, #17908, .F. ) ;
#11878 = EDGE_CURVE ( 'NONE', #26517, #17121, #7204, .T. ) ;
#11879 = CARTESIAN_POINT ( 'NONE',  ( -0.1574803149606299191, 0.09055118110236221041, 0.000000000000000000 ) ) ;
#11880 = EDGE_LOOP ( 'NONE', ( #27529, #10084, #19052, #35979 ) ) ;
#11881 = CARTESIAN_POINT ( 'NONE',  ( 1.002407869896990045, 0.1264236179284866091, 0.9768700786863937502 ) ) ;
#11882 = CARTESIAN_POINT ( 'NONE',  ( -0.1113553986120547346, -0.06200787390822106587, -0.1113553986120547346 ) ) ;
#11883 = CARTESIAN_POINT ( 'NONE',  ( -0.7495606340400177148, 0.1264236179284866091, 1.262303149552535420 ) ) ;
#11884 = ORIENTED_EDGE ( 'NONE', *, *, #1730, .T. ) ;
#11885 = EDGE_CURVE ( 'NONE', #4491, #9701, #47296, .T. ) ;
#11886 = ( BOUNDED_CURVE ( )  B_SPLINE_CURVE ( 2, ( #24918, #2380, #24678, #42623, #39508, #28776, #43344, #10545, #25143 ),
 .UNSPECIFIED., .F., .F. ) 
 B_SPLINE_CURVE_WITH_KNOTS ( ( 3, 2, 2, 2, 3 ),
 ( 0.7600000000000000089, 0.7624999999999999556, 0.7650000000000000133, 0.7674999999999999600, 0.7700000000000000178 ),
 .UNSPECIFIED. ) 
 CURVE ( )  GEOMETRIC_REPRESENTATION_ITEM ( )  RATIONAL_B_SPLINE_CURVE ( ( 1.000000000000000000, 0.9238795325112869605, 1.000000000000000000, 0.9238795325112869605, 1.000000000000000000, 0.9238795325112869605, 1.000000000000000000, 0.9238795325112829637, 1.000000000000000000 ) ) 
 REPRESENTATION_ITEM ( '' )  ) ;
#11887 = CARTESIAN_POINT ( 'NONE',  ( -0.9500414927467378812, 0.1787899950787401604, 0.3100393700249766682 ) ) ;
#11888 = DIRECTION ( 'NONE',  ( 0.000000000000000000, 0.000000000000000000, 1.000000000000000000 ) ) ;
#11889 = VECTOR ( 'NONE', #14058, 39.37007874015748143 ) ;
#11890 = CIRCLE ( 'NONE', #9560, 0.1574803149606299191 ) ;
#11891 = CYLINDRICAL_SURFACE ( 'NONE', #20598, 0.1574803149606299191 ) ;
#11892 = CARTESIAN_POINT ( 'NONE',  ( 0.1787899950787401882, -0.9809310548434114763, -2.189545951927503898E-17 ) ) ;
#11893 = EDGE_LOOP ( 'NONE', ( #11720, #31674, #22413, #1819 ) ) ;
#11894 = VERTEX_POINT ( 'NONE', #8861 ) ;
#11895 = CIRCLE ( 'NONE', #27197, 0.3912448816427701037 ) ;
#11896 = AXIS2_PLACEMENT_3D ( 'NONE', #42095, #12191, #31125 ) ;
#11897 = ORIENTED_EDGE ( 'NONE', *, *, #13562, .T. ) ;
#11898 = CARTESIAN_POINT ( 'NONE',  ( 0.006360881761561069936, -0.05628132561868937761, 0.1377921049841277779 ) ) ;
#11899 = DIRECTION ( 'NONE',  ( 0.000000000000000000, 0.000000000000000000, 1.000000000000000000 ) ) ;
#11900 = CARTESIAN_POINT ( 'NONE',  ( 0.7185039370078692977, 0.06523048226347515077, 1.434547243986962428 ) ) ;
#11901 = CARTESIAN_POINT ( 'NONE',  ( -0.7495606340400177148, -0.1264236179284866091, 0.2485236219934806867 ) ) ;
#11902 = CARTESIAN_POINT ( 'NONE',  ( -0.9412147342319837628, 0.1574803149606300301, 0.9621062992125994917 ) ) ;
#11903 = DIRECTION ( 'NONE',  ( 0.000000000000000000, -1.000000000000000000, 0.000000000000000000 ) ) ;
#11904 = CARTESIAN_POINT ( 'NONE',  ( 0.1797182628040039087, -1.002504439504306344, -0.07444174185955065859 ) ) ;
#11905 = CARTESIAN_POINT ( 'NONE',  ( 0.7185039370078739607, 1.928577636452523993E-17, 1.092519685039370136 ) ) ;
#11906 = CARTESIAN_POINT ( 'NONE',  ( -0.8759842519685039353, -0.1574803149606299191, 1.525590551073574774 ) ) ;
#11907 = CARTESIAN_POINT ( 'NONE',  ( 0.8019270111902717657, -0.1787899950787401604, 0.9202755904974182499 ) ) ;
#11908 = CARTESIAN_POINT ( 'NONE',  ( 0.8019270111902716547, -0.1787899950787401604, 1.348425196796630976 ) ) ;
#11909 = CIRCLE ( 'NONE', #17241, 0.8366141732283465249 ) ;
#11910 = CARTESIAN_POINT ( 'NONE',  ( 0.7646288533564489232, 0.1113553986120547346, 0.5265748030420794867 ) ) ;
#11911 = CARTESIAN_POINT ( 'NONE',  ( 0.8107537697050253289, 0.1574803149606300301, 1.360728346456693050 ) ) ;
#11913 = DIRECTION ( 'NONE',  ( -1.000000000000000000, -6.679788269418529283E-17, 0.000000000000000000 ) ) ;
#11912 = CARTESIAN_POINT ( 'NONE',  ( 0.7171850904892348444, -0.05464115389802457617, 1.984299705265581304 ) ) ;
#11914 = CARTESIAN_POINT ( 'NONE',  ( 0.7185039370078739607, 1.928577636452523993E-17, 1.476377952648377789 ) ) ;
#11915 = CARTESIAN_POINT ( 'NONE',  ( 0.1574803149606300301, -0.7091535431995588112, 0.06523048226347956391 ) ) ;
#11916 = CARTESIAN_POINT ( 'NONE',  ( -0.3980944881889759146, 0.2597269656108969760, 0.7480314960629921295 ) ) ;
#11917 = CARTESIAN_POINT ( 'NONE',  ( 0.9500414927467377701, -0.1787899950787401604, 0.8021653542769462408 ) ) ;
#11918 = CARTESIAN_POINT ( 'NONE',  ( 0.6971942568897648851, 0.07405724077823318263, 1.776574803095843702 ) ) ;
#11920 = AXIS2_PLACEMENT_3D ( 'NONE', #29616, #22355, #7741 ) ;
#11919 = CARTESIAN_POINT ( 'NONE',  ( 0.1787899950787401604, -0.7657480314423001921, -0.07405724077823318263 ) ) ;
#11921 = CARTESIAN_POINT ( 'NONE',  ( 0.1574803149606299191, 0.000000000000000000, -0.1966003937007873570 ) ) ;
#11922 = EDGE_LOOP ( 'NONE', ( #18416, #10479, #15708, #9700, #46879, #16747 ) ) ;
#11923 = EDGE_CURVE ( 'NONE', #26504, #47218, #15149, .T. ) ;
#11924 = CARTESIAN_POINT ( 'NONE',  ( 1.033464566929133355, -0.06523048226348075740, 0.4306102361129452438 ) ) ;
#11925 = CONICAL_SURFACE ( 'NONE', #44800, 0.1574803149606299191, 0.9599310885968735940 ) ;
#11926 = AXIS2_PLACEMENT_3D ( 'NONE', #27470, #42021, #20235 ) ;
#11927 = CARTESIAN_POINT ( 'NONE',  ( 9.037241287634464769E-18, -0.1260561954211091296, 0.05725481610291012491 ) ) ;
#11928 = CARTESIAN_POINT ( 'NONE',  ( -0.8759842519685039353, -0.1574803149606299191, 0.06889763768774861963 ) ) ;
#11929 = CARTESIAN_POINT ( 'NONE',  ( 1.054774247047244540, 0.07405724077823318263, 1.126968503883244654 ) ) ;
#11930 = DIRECTION ( 'NONE',  ( 5.159318851433039196E-16, 0.6156614753256609562, 0.7880107536067197938 ) ) ;
#11931 = CARTESIAN_POINT ( 'NONE',  ( 2.892866454678787531E-17, -1.750000000000000222, 0.1574803149606299191 ) ) ;
#11932 = CARTESIAN_POINT ( 'NONE',  ( -0.3690944881889761109, 0.1864803149606354127, -0.7480314960629921295 ) ) ;
#11933 = ADVANCED_FACE ( 'NONE', ( #22761 ), #1411, .T. ) ;
#11934 = ORIENTED_EDGE ( 'NONE', *, *, #29473, .T. ) ;
#11935 = CARTESIAN_POINT ( 'NONE',  ( 0.2395294000716133853, 0.1968503937007874127, 0.4921259842519685179 ) ) ;
#11936 = CARTESIAN_POINT ( 'NONE',  ( -0.9500414927467378812, -0.1787899950787401604, 0.2903543306548980185 ) ) ;
#11937 = ORIENTED_EDGE ( 'NONE', *, *, #32102, .F. ) ;
#11938 = CARTESIAN_POINT ( 'NONE',  ( 0.8107537697050254399, 0.1574803149606300301, 1.754429133858266932 ) ) ;
#11939 = CARTESIAN_POINT ( 'NONE',  ( -0.1787899950787401604, -1.503937007820251637, -0.07405724077823318263 ) ) ;
#11940 = CARTESIAN_POINT ( 'NONE',  ( -0.6971942568897648851, 0.07405724077823318263, 1.771653543253322249 ) ) ;
#11941 = CARTESIAN_POINT ( 'NONE',  ( -0.7495606340400177148, -0.1264236179284866091, 0.9522637794737952577 ) ) ;
#11942 = CARTESIAN_POINT ( 'NONE',  ( -1.002407869896990045, -0.1264236179284866091, 0.4552165353793071745 ) ) ;
#11943 = FACE_OUTER_BOUND ( 'NONE', #3490, .T. ) ;
#11944 = PRODUCT_DEFINITION ( 'UNKNOWN', '', #26300, #18289 ) ;
#11945 = CARTESIAN_POINT ( 'NONE',  ( 0.3551574803149606385, -0.2362204724409449064, 0.000000000000000000 ) ) ;
#11946 = CARTESIAN_POINT ( 'NONE',  ( -1.033464566929133799, 0.000000000000000000, 0.3149606298137326843 ) ) ;
#11947 = CARTESIAN_POINT ( 'NONE',  ( -0.3070313825494068727, 0.04447134000132169085, -1.037676521114162531 ) ) ;
#11948 = CARTESIAN_POINT ( 'NONE',  ( -0.1264236179284866091, -0.5724664879142778995, -0.1264236179284866091 ) ) ;
#11949 = CARTESIAN_POINT ( 'NONE',  ( -0.09248453076245886917, -0.08955999818690787984, 0.2055509654934188912 ) ) ;
#11950 = DIRECTION ( 'NONE',  ( -1.000000000000000000, 0.000000000000000000, 0.000000000000000000 ) ) ;
#11951 = CARTESIAN_POINT ( 'NONE',  ( 0.8759842519685039353, -0.1574803149606299191, 1.929133858267716661 ) ) ;
#11952 = PRODUCT_DEFINITION_SHAPE ( 'NONE', 'NONE',  #6332 ) ;
#11953 = AXIS2_PLACEMENT_3D ( 'NONE', #19333, #11930, #33982 ) ;
#11954 = CARTESIAN_POINT ( 'NONE',  ( -0.8759842491179902213, 0.1574803149606299191, 1.978346456692913646 ) ) ;
#11955 = CARTESIAN_POINT ( 'NONE',  ( -1.002407869896990045, 0.1264236179284866091, 0.3026574802611972648 ) ) ;
#11956 = CARTESIAN_POINT ( 'NONE',  ( -1.033464566929133799, 1.928577636452524610E-17, 2.869337061179095023E-17 ) ) ;
#11957 = VERTEX_POINT ( 'NONE', #23252 ) ;
#11958 = CARTESIAN_POINT ( 'NONE',  ( -0.1574803149606299191, 0.07021257666614952320, -0.1553045758542780375 ) ) ;
#11959 = ORIENTED_EDGE ( 'NONE', *, *, #33254, .F. ) ;
#11960 = CARTESIAN_POINT ( 'NONE',  ( -1.002407869896990045, 0.1264236179284866091, 1.488681102308440751 ) ) ;
#11961 = EDGE_LOOP ( 'NONE', ( #12897, #26559, #41039, #33100, #35426, #8503, #41723, #31883, #46859, #7428, #25835, #98 ) ) ;
#11962 = CARTESIAN_POINT ( 'NONE',  ( -0.07405724077823318263, -1.390748031442299082, -0.1787899950787401604 ) ) ;
#11963 = CARTESIAN_POINT ( 'NONE',  ( -0.07405724077823318263, -1.528543307032852239, 0.1787899950787401604 ) ) ;
#11964 = CARTESIAN_POINT ( 'NONE',  ( -0.3551574803149606385, -2.130889186148732174E-17, 0.000000000000000000 ) ) ;
#11965 = CARTESIAN_POINT ( 'NONE',  ( 0.1602931993194442739, -0.07955613945526318620, 0.1377952755905511861 ) ) ;
#11966 = CARTESIAN_POINT ( 'NONE',  ( 1.033464566929134687, 0.06523048226347956391, 0.5241141732283461918 ) ) ;
#11967 = CARTESIAN_POINT ( 'NONE',  ( 0.3727034120734909473, 4.616380251121755931E-17, 0.000000000000000000 ) ) ;
#11968 = CARTESIAN_POINT ( 'NONE',  ( -0.8107537697050253289, 0.1574803149606300301, 1.154035432963338659 ) ) ;
#11969 = CARTESIAN_POINT ( 'NONE',  ( 1.054774247047244096, 0.000000000000000000, 0.06151574797773248782 ) ) ;
#11971 = CARTESIAN_POINT ( 'NONE',  ( 0.4736248074375614681, 1.025704337919490117, -1.138861239548320858 ) ) ;
#11970 = CARTESIAN_POINT ( 'NONE',  ( 2.892866454678787531E-17, -0.3326771653543306728, 0.1574803149606299191 ) ) ;
#11972 = CARTESIAN_POINT ( 'NONE',  ( 0.9412147342319837628, 0.1574803149606300301, 1.936515747923967856 ) ) ;
#11973 = ORIENTED_EDGE ( 'NONE', *, *, #33362, .T. ) ;
#11974 = EDGE_CURVE ( 'NONE', #461, #33076, #30936, .T. ) ;
#11975 = LINE ( 'NONE', #1383, #16910 ) ;
#11976 = LINE ( 'NONE', #4044, #25875 ) ;
#11978 = CARTESIAN_POINT ( 'NONE',  ( 0.9412147342319837628, -0.1574803149606297803, 1.537893700787401841 ) ) ;
#11977 = DIRECTION ( 'NONE',  ( 1.822029033848725028E-16, 0.000000000000000000, 1.000000000000000000 ) ) ;
#11979 = CARTESIAN_POINT ( 'NONE',  ( -0.1376518243080670778, -0.08956097154447616171, 0.08777079064950775444 ) ) ;
#11980 = ORIENTED_EDGE ( 'NONE', *, *, #43584, .F. ) ;
#11981 = EDGE_CURVE ( 'NONE', #30394, #25443, #45738, .T. ) ;
#11982 = ORIENTED_EDGE ( 'NONE', *, *, #33305, .T. ) ;
#11983 = CYLINDRICAL_SURFACE ( 'NONE', #26456, 0.5905511811023623769 ) ;
#11984 = CARTESIAN_POINT ( 'NONE',  ( 0.4934383202099732468, 4.616380251121755931E-17, 0.000000000000000000 ) ) ;
#11985 = CARTESIAN_POINT ( 'NONE',  ( -1.094772975963752103E-17, -1.506397637741511586, -0.1787899950787401882 ) ) ;
#11986 = CARTESIAN_POINT ( 'NONE',  ( -0.1264236179284866091, -0.8272637794737952577, 0.1264236179284866091 ) ) ;
#11987 = CARTESIAN_POINT ( 'NONE',  ( 0.1574803149606299191, -1.228346456692913424, -1.928577636452523993E-17 ) ) ;
#11988 = CARTESIAN_POINT ( 'NONE',  ( 0.9412147342319837628, 0.1574803149606300301, 1.149114173120819427 ) ) ;
#11989 = CARTESIAN_POINT ( 'NONE',  ( 0.8759842519685039353, 0.000000000000000000, 4.498031496062992574 ) ) ;
#11990 = UNCERTAINTY_MEASURE_WITH_UNIT (LENGTH_MEASURE( 1.000000000000000082E-05 ), #45107, 'distance_accuracy_value', 'NONE') ;
#11991 = ORIENTED_EDGE ( 'NONE', *, *, #16294, .T. ) ;
#11992 = ORIENTED_EDGE ( 'NONE', *, *, #12023, .F. ) ;
#11993 = CARTESIAN_POINT ( 'NONE',  ( -0.9500414927467378812, 0.1787899950787401604, 1.766732283410803461 ) ) ;
#11994 = CARTESIAN_POINT ( 'NONE',  ( -0.9873396505805591694, -0.1113553986120547346, 0.5954724409448819422 ) ) ;
#11995 = CARTESIAN_POINT ( 'NONE',  ( 0.6971942568897648851, -0.07405724077823297447, 1.702755905458047003 ) ) ;
#11996 = CARTESIAN_POINT ( 'NONE',  ( 0.7185039370078739607, 1.928577636452523993E-17, 1.791338582569637738 ) ) ;
#11997 = CARTESIAN_POINT ( 'NONE',  ( 0.6971942568897626646, 0.07405724077823318263, 0.3198818897100162983 ) ) ;
#11998 = CARTESIAN_POINT ( 'NONE',  ( -1.002407869896990045, 0.1264236179284866091, 1.444389763725763665 ) ) ;
#11999 = DIRECTION ( 'NONE',  ( 0.000000000000000000, 0.000000000000000000, -1.000000000000000000 ) ) ;
#12000 = CARTESIAN_POINT ( 'NONE',  ( -0.8019270111902716547, -0.1787899950787401604, 1.230314960576158967 ) ) ;
#12001 = CARTESIAN_POINT ( 'NONE',  ( -0.8019270111902717657, 0.1787899950787401604, 0.9005905511273389896 ) ) ;
#12002 = CARTESIAN_POINT ( 'NONE',  ( -0.6971942568897637749, 2.189545951927499583E-17, 0.04675196845017354913 ) ) ;
#12003 = ( BOUNDED_CURVE ( )  B_SPLINE_CURVE ( 2, ( #12828, #23125, #12597, #19986, #22883, #34166, #15474, #5128, #15951 ),
 .UNSPECIFIED., .F., .T. ) 
 B_SPLINE_CURVE_WITH_KNOTS ( ( 3, 2, 2, 2, 3 ),
 ( 0.3599999999999999867, 0.3624999999999999889, 0.3649999999999999911, 0.3674999999999999933, 0.3699999999999999956 ),
 .UNSPECIFIED. ) 
 CURVE ( )  GEOMETRIC_REPRESENTATION_ITEM ( )  RATIONAL_B_SPLINE_CURVE ( ( 1.000000000000000000, 0.9238795325112869605, 1.000000000000000000, 0.9238795325112869605, 1.000000000000000000, 0.9238795325112869605, 1.000000000000000000, 0.9238795325112869605, 1.000000000000000000 ) ) 
 REPRESENTATION_ITEM ( '' )  ) ;
#12004 = CARTESIAN_POINT ( 'NONE',  ( 0.1093692153654458876, 0.09774221684002680488, 0.2222887249338434679 ) ) ;
#12005 = CARTESIAN_POINT ( 'NONE',  ( -1.054774247047244540, -0.07405724077823318263, 1.599409448765135133 ) ) ;
#12006 = CARTESIAN_POINT ( 'NONE',  ( -1.054774247047244096, 0.000000000000000000, 0.02706692908009476414 ) ) ;
#12007 = CYLINDRICAL_SURFACE ( 'NONE', #5755, 0.1864803149606298893 ) ;
#12008 = CARTESIAN_POINT ( 'NONE',  ( -0.8759842519685039353, 0.000000000000000000, 2.007874015640504162 ) ) ;
#12009 = CARTESIAN_POINT ( 'NONE',  ( 0.7495606340400177148, -0.1264236179284866091, 1.547736220418677089 ) ) ;
#12010 = CARTESIAN_POINT ( 'NONE',  ( -0.1598411944706594756, -0.09842519685039370636, 0.1688112090790881981 ) ) ;
#12011 = LINE ( 'NONE', #4787, #14204 ) ;
#12012 = ORIENTED_EDGE ( 'NONE', *, *, #17959, .T. ) ;
#12013 = EDGE_LOOP ( 'NONE', ( #5149, #43314, #19935, #17708 ) ) ;
#12014 = CARTESIAN_POINT ( 'NONE',  ( -0.9500414927467377701, 0.1787899950787401604, 1.176181102308441195 ) ) ;
#12015 = ORIENTED_EDGE ( 'NONE', *, *, #22719, .F. ) ;
#12016 = CARTESIAN_POINT ( 'NONE',  ( 0.1264236179284866091, -0.9355314960092283583, 0.1264236179284866091 ) ) ;
#12017 = ( BOUNDED_CURVE ( )  B_SPLINE_CURVE ( 2, ( #26430, #25726, #12044, #14689, #7716, #36502, #26666, #15644, #18279 ),
 .UNSPECIFIED., .F., .T. ) 
 B_SPLINE_CURVE_WITH_KNOTS ( ( 3, 2, 2, 2, 3 ),
 ( 0.5100000000000000089, 0.5124999999999999556, 0.5150000000000000133, 0.5174999999999999600, 0.5200000000000000178 ),
 .UNSPECIFIED. ) 
 CURVE ( )  GEOMETRIC_REPRESENTATION_ITEM ( )  RATIONAL_B_SPLINE_CURVE ( ( 1.000000000000000000, 0.9238795325112869605, 1.000000000000000000, 0.9238795325112869605, 1.000000000000000000, 0.9238795325112869605, 1.000000000000000000, 0.9238795325112869605, 1.000000000000000000 ) ) 
 REPRESENTATION_ITEM ( '' )  ) ;
#12018 = CARTESIAN_POINT ( 'NONE',  ( -0.1787899950787401882, -1.024114173174582643, 0.000000000000000000 ) ) ;
#12019 = DIRECTION ( 'NONE',  ( 0.000000000000000000, 0.000000000000000000, -1.000000000000000000 ) ) ;
#12020 = CARTESIAN_POINT ( 'NONE',  ( 0.8107537697050234415, -0.1574803149606297803, 0.3125000000000000000 ) ) ;
#12021 = CARTESIAN_POINT ( 'NONE',  ( -0.1797182628040039365, -0.3553587702129669124, 0.000000000000000000 ) ) ;
#12022 = CARTESIAN_POINT ( 'NONE',  ( -0.1184675242425147629, -0.5708661417322835607, 1.224299699984019885 ) ) ;
#12023 = EDGE_CURVE ( 'NONE', #5626, #27121, #18684, .T. ) ;
#12024 = CARTESIAN_POINT ( 'NONE',  ( -1.033464566929134687, 0.06523048226347956391, 0.1304133858267717272 ) ) ;
#12025 = CARTESIAN_POINT ( 'NONE',  ( 0.6971942568897626646, -0.07405724077823297447, 0.7529527558517473684 ) ) ;
#12026 = EDGE_CURVE ( 'NONE', #16941, #8098, #36591, .T. ) ;
#12028 = CARTESIAN_POINT ( 'NONE',  ( -8.354793841626791791E-17, -0.09842519685039370636, -0.2854330708661417804 ) ) ;
#12027 = CARTESIAN_POINT ( 'NONE',  ( 0.05642593091638736097, 0.2629167058585549221, -0.05524818609632992789 ) ) ;
#12029 = FACE_OUTER_BOUND ( 'NONE', #18418, .T. ) ;
#12030 = DIRECTION ( 'NONE',  ( -1.000000000000000000, 0.000000000000000000, 0.000000000000000000 ) ) ;
#12031 = CARTESIAN_POINT ( 'NONE',  ( 1.054774247047244540, 0.07405724077823318263, 1.761811023568284007 ) ) ;
#12032 = ADVANCED_FACE ( 'NONE', ( #44545 ), #40942, .T. ) ;
#12033 = ADVANCED_FACE ( 'NONE', ( #5023 ), #45762, .T. ) ;
#12034 = CARTESIAN_POINT ( 'NONE',  ( 0.9412147342319837628, 0.1574803149606300301, 0.09596456692913378494 ) ) ;
#12035 = DIRECTION ( 'NONE',  ( 1.224646799147351482E-16, 0.000000000000000000, -1.000000000000000000 ) ) ;
#12036 = CARTESIAN_POINT ( 'NONE',  ( -0.1264236179284866091, -0.4040354330171023745, -0.1264236179284866091 ) ) ;
#12037 = CARTESIAN_POINT ( 'NONE',  ( -0.1586641775163213364, 0.8918838478058892516, -1.034309214090478823 ) ) ;
#12039 = CONICAL_SURFACE ( 'NONE', #40325, 0.1003937007874011050, 0.7853981633973787790 ) ;
#12038 = CARTESIAN_POINT ( 'NONE',  ( -0.1264236179284866091, -1.304625984198204636, -0.1264236179284866091 ) ) ;
#12040 = CARTESIAN_POINT ( 'NONE',  ( 0.6971942568897626646, 0.07405724077823318263, 0.2805118109698587214 ) ) ;
#12041 = CARTESIAN_POINT ( 'NONE',  ( -0.6971942568897648851, -0.07405724077823297447, 1.776574803095843924 ) ) ;
#12042 = VERTEX_POINT ( 'NONE', #16072 ) ;
#12043 = CARTESIAN_POINT ( 'NONE',  ( -1.002407869896990045, 0.1264236179284866091, 1.331200787347811110 ) ) ;
#12044 = CARTESIAN_POINT ( 'NONE',  ( 0.7646288533564489232, -0.1113553986120547346, 1.018700787401574770 ) ) ;
#12045 = CARTESIAN_POINT ( 'NONE',  ( -0.1113553986120547346, -1.193897637687748148, 0.1113553986120547346 ) ) ;
#12046 = CARTESIAN_POINT ( 'NONE',  ( 1.002407869896990045, 0.1264236179284866091, 0.03198818892261445085 ) ) ;
#12047 = CARTESIAN_POINT ( 'NONE',  ( -0.9500414927467378812, 0.1787899950787401604, 1.171259842465921741 ) ) ;
#12048 = CARTESIAN_POINT ( 'NONE',  ( 1.033464566929134687, 0.06523048226347956391, 1.537893700679874076 ) ) ;
#12049 = CARTESIAN_POINT ( 'NONE',  ( 0.03943478969741477658, -0.09842516626972255822, -0.1743868110616672018 ) ) ;
#12050 = CARTESIAN_POINT ( 'NONE',  ( 0.1476377952755906220, 0.06415291647593752977, -0.1630605872086748620 ) ) ;
#12051 = CARTESIAN_POINT ( 'NONE',  ( 1.002407869896990045, -0.1264236179284866091, 0.4552165353793071745 ) ) ;
#12052 = CARTESIAN_POINT ( 'NONE',  ( -0.7495606340400177148, -0.1264236179284866091, 0.3617125983714334359 ) ) ;
#12053 = VERTEX_POINT ( 'NONE', #15599 ) ;
#12054 = VERTEX_POINT ( 'NONE', #30697 ) ;
#12055 = CARTESIAN_POINT ( 'NONE',  ( 0.9500414927467378812, -0.1787899950787401604, 0.9251968503399374821 ) ) ;
#12056 = CARTESIAN_POINT ( 'NONE',  ( -0.7185039370078746268, 0.06523048226347956391, 0.1451771653543309226 ) ) ;
#12057 = CARTESIAN_POINT ( 'NONE',  ( 0.9500414927467377701, 0.1787899950787401604, 1.176181102308441195 ) ) ;
#12058 = CARTESIAN_POINT ( 'NONE',  ( 1.033464566929134687, 0.06523048226347956391, 1.931594488081448180 ) ) ;
#12059 = ORIENTED_EDGE ( 'NONE', *, *, #23070, .T. ) ;
#12060 = FACE_OUTER_BOUND ( 'NONE', #40547, .T. ) ;
#12061 = CARTESIAN_POINT ( 'NONE',  ( -1.033464566929133799, 0.000000000000000000, 0.3248031496062992463 ) ) ;
#12062 = CARTESIAN_POINT ( 'NONE',  ( 0.8759842519685039353, -0.1574803149606299191, 0.3149606299212598381 ) ) ;
#12063 = CARTESIAN_POINT ( 'NONE',  ( -0.1787899950787401604, -1.391856251693805779, 0.07405724077823318263 ) ) ;
#12064 = ORIENTED_EDGE ( 'NONE', *, *, #29800, .T. ) ;
#12065 = CARTESIAN_POINT ( 'NONE',  ( -0.07405724077823318263, -0.4409448818359998357, -0.1787899950787401604 ) ) ;
#12066 = DIRECTION ( 'NONE',  ( -5.724375810226267502E-16, -0.6156614753256588468, -0.7880107536067216811 ) ) ;
#12067 = VERTEX_POINT ( 'NONE', #19641 ) ;
#12068 = CARTESIAN_POINT ( 'NONE',  ( 1.054774247047244540, -0.07405724077823318263, 1.279527559001355286 ) ) ;
#12069 = LINE ( 'NONE', #14715, #4190 ) ;
#12070 = LINE ( 'NONE', #26693, #2423 ) ;
#12071 = VECTOR ( 'NONE', #1296, 39.37007874015748854 ) ;
#12072 = CARTESIAN_POINT ( 'NONE',  ( 0.8759842519685039353, 0.1787899950787401882, 0.1894685038832444879 ) ) ;
#12073 = CARTESIAN_POINT ( 'NONE',  ( -0.07405724077823318263, -1.769685039316315267, 0.1787899950787401604 ) ) ;
#12074 = CARTESIAN_POINT ( 'NONE',  ( -0.1787899950787401604, 0.1102362205262043815, -0.07405724077823318263 ) ) ;
#12075 = SHAPE_DEFINITION_REPRESENTATION ( #42283, #1042 ) ;
#12076 = CARTESIAN_POINT ( 'NONE',  ( 0.005379252439919633005, -0.05299006067052474539, -0.1377950963417848562 ) ) ;
#12077 = ORIENTED_EDGE ( 'NONE', *, *, #31779, .T. ) ;
#12078 = EDGE_CURVE ( 'NONE', #3940, #3727, #4775, .T. ) ;
#12079 = CARTESIAN_POINT ( 'NONE',  ( -0.7495606340400177148, 0.1264236179284866091, 0.7111220471903307860 ) ) ;
#12080 = DIRECTION ( 'NONE',  ( -1.000000000000000000, 0.000000000000000000, 0.000000000000000000 ) ) ;
#12082 = CARTESIAN_POINT ( 'NONE',  ( 0.9873396505805591694, -0.1113553986120547346, 0.3100393699712130080 ) ) ;
#12081 = CARTESIAN_POINT ( 'NONE',  ( 0.1113553986120547346, -0.6820866141732283561, 0.1113553986120547346 ) ) ;
#12083 = CARTESIAN_POINT ( 'NONE',  ( 0.1270800023317771588, -1.433114675724777465, -0.1270800023317771588 ) ) ;
#12084 = CARTESIAN_POINT ( 'NONE',  ( -0.06523048226347956391, -0.06446850382948084157, -0.1574803149606300301 ) ) ;
#12085 = DIRECTION ( 'NONE',  ( 0.000000000000000000, 0.7880107536067203489, -0.6156614753256604011 ) ) ;
#12086 = CARTESIAN_POINT ( 'NONE',  ( 0.8759842519685039353, 0.1787899950787401882, 1.375492125930488196 ) ) ;
#12087 = CARTESIAN_POINT ( 'NONE',  ( 1.054774247047244540, 0.07405724077823318263, 1.914370078686394860 ) ) ;
#12089 = ORIENTED_EDGE ( 'NONE', *, *, #8059, .F. ) ;
#12088 = CARTESIAN_POINT ( 'NONE',  ( 1.033464566929134687, 0.06523048226347956391, 1.498523621939716444 ) ) ;
#12090 = EDGE_CURVE ( 'NONE', #28525, #43008, #42147, .T. ) ;
#12092 = CARTESIAN_POINT ( 'NONE',  ( -0.7533556175591157311, 0.1062596105467954882, 1.981019962422237990 ) ) ;
#12091 = CARTESIAN_POINT ( 'NONE',  ( 0.1644020957507537628, -0.08115590401245532937, 0.1405661490837558925 ) ) ;
#12093 = CARTESIAN_POINT ( 'NONE',  ( -0.1574803149606299191, 0.7443365962042343131, -3.523993443072799270 ) ) ;
#12094 = CARTESIAN_POINT ( 'NONE',  ( -0.1264236179284866091, 0.07824803154982658271, 0.1264236179284866091 ) ) ;
#12095 = CARTESIAN_POINT ( 'NONE',  ( 0.7185039370078732945, -0.06523048226347899492, 0.5339566928058584461 ) ) ;
#12096 = CARTESIAN_POINT ( 'NONE',  ( 0.9500414927467378812, 0.1787899950787401604, 0.3051181101824569919 ) ) ;
#12097 = CARTESIAN_POINT ( 'NONE',  ( 1.181102362204724310, -0.3937007874015748254, -0.9842519685039370358 ) ) ;
#12098 = CIRCLE ( 'NONE', #24332, 0.1003937007874010356 ) ;
#12099 = CARTESIAN_POINT ( 'NONE',  ( -0.7185039370078739607, 1.928577636452523993E-17, 0.9645669290263307882 ) ) ;
#12100 = CARTESIAN_POINT ( 'NONE',  ( -1.002407869896990045, -0.1264236179284866091, 1.277066929080094448 ) ) ;
#12101 = CARTESIAN_POINT ( 'NONE',  ( 1.033464566929134687, -0.06523048226347956391, 0.7062007872940467834 ) ) ;
#12102 = VERTEX_POINT ( 'NONE', #42602 ) ;
#12103 = CARTESIAN_POINT ( 'NONE',  ( 0.7646288533564489232, 0.1113553986120547346, 1.402559055118110187 ) ) ;
#12104 = DIRECTION ( 'NONE',  ( 0.000000000000000000, -0.7880107536067206819, 0.6156614753256597350 ) ) ;
#12105 = ORIENTED_EDGE ( 'NONE', *, *, #476, .T. ) ;
#12106 = CARTESIAN_POINT ( 'NONE',  ( 3.301370929368692659E-17, 0.008814458133489902134, 0.1797182628040039365 ) ) ;
#12108 = ORIENTED_EDGE ( 'NONE', *, *, #8398, .F. ) ;
#12107 = CARTESIAN_POINT ( 'NONE',  ( -0.1787899950787401604, -1.228346456639149542, -0.07405724077823318263 ) ) ;
#12109 = CARTESIAN_POINT ( 'NONE',  ( 0.6971942568897648851, 0.07405724077823318263, 1.614173228292692386 ) ) ;
#12110 = CARTESIAN_POINT ( 'NONE',  ( -1.033464566929134687, -0.06523048226347956391, 1.267224409448818978 ) ) ;
#12111 = CARTESIAN_POINT ( 'NONE',  ( -0.7185039370078739607, 1.928577636452523993E-17, 1.161417322727118284 ) ) ;
#12113 = DIRECTION ( 'NONE',  ( 1.000000000000000000, 0.000000000000000000, 0.000000000000000000 ) ) ;
#12112 = CARTESIAN_POINT ( 'NONE',  ( -1.033464566929133799, 0.000000000000000000, 1.820866141732283561 ) ) ;
#12114 = CARTESIAN_POINT ( 'NONE',  ( -0.7185039370078746268, -0.06523048226347956391, 0.4945866140657015353 ) ) ;
#12115 = CARTESIAN_POINT ( 'NONE',  ( 0.7185039370078746268, 0.06523048226347956391, 1.316437007766489975 ) ) ;
#12116 = VERTEX_POINT ( 'NONE', #34989 ) ;
#12117 = ORIENTED_EDGE ( 'NONE', *, *, #3081, .T. ) ;
#12118 = CARTESIAN_POINT ( 'NONE',  ( 1.054774247047244540, -0.07405724077823318263, 0.9301181101824563813 ) ) ;
#12119 = CARTESIAN_POINT ( 'NONE',  ( -0.8019270111902716547, 0.1787899950787401604, 1.569881889710015299 ) ) ;
#12120 = CARTESIAN_POINT ( 'NONE',  ( -9.642888182262618425E-18, -0.02755905501058318954, -0.1574803149606299191 ) ) ;
#12121 = CARTESIAN_POINT ( 'NONE',  ( -0.7495606340400177148, -0.1264236179284866091, 1.350885826717889815 ) ) ;
#12122 = ORIENTED_EDGE ( 'NONE', *, *, #17641, .T. ) ;
#12123 = ADVANCED_FACE ( 'NONE', ( #2596 ), #28264, .T. ) ;
#12124 = CARTESIAN_POINT ( 'NONE',  ( -1.002407869896990045, 0.1264236179284866091, 0.3863188975840318173 ) ) ;
#12125 = DIRECTION ( 'NONE',  ( 1.000000000000000000, 0.000000000000000000, 0.000000000000000000 ) ) ;
#12126 = CARTESIAN_POINT ( 'NONE',  ( -1.033464566929133799, 0.000000000000000000, 1.889763779420031486 ) ) ;
#12127 = CARTESIAN_POINT ( 'NONE',  ( -0.1264236179284866091, -0.9661672753158523363, -0.1264236179284866091 ) ) ;
#12128 = ORIENTED_EDGE ( 'NONE', *, *, #24040, .T. ) ;
#12129 = CARTESIAN_POINT ( 'NONE',  ( -0.1787899950787401882, 0.03887795280966901967, 0.000000000000000000 ) ) ;
#12130 = ORIENTED_EDGE ( 'NONE', *, *, #30668, .T. ) ;
#12131 = ORIENTED_EDGE ( 'NONE', *, *, #26787, .T. ) ;
#12132 = CARTESIAN_POINT ( 'NONE',  ( 1.033464566929133799, 0.000000000000000000, 1.141732283357039357 ) ) ;
#12133 = DIRECTION ( 'NONE',  ( 0.8191520442889861364, 0.000000000000000000, 0.5735764363510541530 ) ) ;
#12134 = CARTESIAN_POINT ( 'NONE',  ( 0.8107537697050254399, 0.1574803149606300301, 1.429625984144440531 ) ) ;
#12135 = VECTOR ( 'NONE', #27592, 39.37007874015748143 ) ;
#12136 = ADVANCED_FACE ( 'NONE', ( #34506 ), #39023, .T. ) ;
#12137 = CARTESIAN_POINT ( 'NONE',  ( -0.9500414927467377701, 0.1787899950787401604, 0.2312992125446618197 ) ) ;
#12138 = CARTESIAN_POINT ( 'NONE',  ( -0.7646288533564489232, 0.1113553986120547346, 0.8120078740157481434 ) ) ;
#12139 = DIRECTION ( 'NONE',  ( 0.000000000000000000, 0.000000000000000000, 1.000000000000000000 ) ) ;
#12140 = CARTESIAN_POINT ( 'NONE',  ( 0.1797182628040039365, -0.9262249119452500290, -2.200913952912460540E-17 ) ) ;
#12141 = CARTESIAN_POINT ( 'NONE',  ( -1.033464566929133799, 0.000000000000000000, 1.663385826771653697 ) ) ;
#12142 = CARTESIAN_POINT ( 'NONE',  ( 0.6971942568897626646, 0.07405724077823318263, 0.9891732282926934960 ) ) ;
#12143 = CARTESIAN_POINT ( 'NONE',  ( 1.054774247047244096, 0.000000000000000000, 1.439468503883244210 ) ) ;
#12144 = CARTESIAN_POINT ( 'NONE',  ( 0.6971942568897637749, 2.189545951927499583E-17, 0.1205708660879689087 ) ) ;
#12145 = CARTESIAN_POINT ( 'NONE',  ( -1.033464566929134687, 0.06523048226347956391, 0.4453740157480309270 ) ) ;
#12146 = CARTESIAN_POINT ( 'NONE',  ( 0.9412147342319837628, 0.1574803149606300301, 1.552657480314961536 ) ) ;
#12148 = CARTESIAN_POINT ( 'NONE',  ( 0.2642359194686346169, 4.766607801171850497E-17, 0.000000000000000000 ) ) ;
#12147 = CARTESIAN_POINT ( 'NONE',  ( 0.7101756151665713501, 0.004432158464400415970, 1.983187800286568381 ) ) ;
#12149 = CARTESIAN_POINT ( 'NONE',  ( -0.1264236179284866091, 0.07332677170730689253, -0.1264236179284866091 ) ) ;
#12150 = DIRECTION ( 'NONE',  ( -1.000000000000000000, 0.000000000000000000, 0.000000000000000000 ) ) ;
#12152 = CARTESIAN_POINT ( 'NONE',  ( -0.8107537697050254399, -0.1574803149606297803, 1.414862204724410377 ) ) ;
#12151 = CARTESIAN_POINT ( 'NONE',  ( 0.8019270111902716547, 0.1787899950787401604, 0.7824803149068668695 ) ) ;
#12153 = CARTESIAN_POINT ( 'NONE',  ( 0.8019270111902716547, -0.1787899950787401604, 1.865157480261198097 ) ) ;
#12154 = CARTESIAN_POINT ( 'NONE',  ( 0.1264236179284866091, -0.9207677164816693294, -0.1264236179284866091 ) ) ;
#12155 = VERTEX_POINT ( 'NONE', #16762 ) ;
#12156 = CARTESIAN_POINT ( 'NONE',  ( 1.033464566929133799, 0.000000000000000000, 0.9153543307086614567 ) ) ;
#12157 = CARTESIAN_POINT ( 'NONE',  ( -0.1574803149606300301, -1.752460629813732185, -0.06523048226347956391 ) ) ;
#12158 = CARTESIAN_POINT ( 'NONE',  ( -1.033464566929134687, 0.06523048226347956391, 0.04183070855389029591 ) ) ;
#12159 = CARTESIAN_POINT ( 'NONE',  ( 0.8019270111902717657, -0.1787899950787401604, 1.072834645615528659 ) ) ;
#12160 = DIRECTION ( 'NONE',  ( 0.000000000000000000, 0.000000000000000000, 1.000000000000000000 ) ) ;
#12161 = CARTESIAN_POINT ( 'NONE',  ( -0.1574803149606300301, -1.683562992125984259, -0.06523048226347956391 ) ) ;
#12162 = DIRECTION ( 'NONE',  ( 3.124924761047742408E-15, 0.9006982393225889671, 0.4344452574044149751 ) ) ;
#12163 = VECTOR ( 'NONE', #23406, 39.37007874015748854 ) ;
#12164 = CARTESIAN_POINT ( 'NONE',  ( 0.2204724409448818867, -0.07955613945526357478, -0.1377952755905511861 ) ) ;
#12165 = CARTESIAN_POINT ( 'NONE',  ( -0.8019270111902717657, -0.1787899950787401604, 0.3248031495525355306 ) ) ;
#12166 = ORIENTED_EDGE ( 'NONE', *, *, #28263, .F. ) ;
#12168 = CARTESIAN_POINT ( 'NONE',  ( -0.1787899950787401882, -1.462106299158834721, 0.000000000000000000 ) ) ;
#12167 = CARTESIAN_POINT ( 'NONE',  ( -9.642888182262618425E-18, -0.3425196849318429826, -0.1574803149606299191 ) ) ;
#12169 = CARTESIAN_POINT ( 'NONE',  ( -0.7495606340400177148, -0.1264236179284866091, 1.779035433017102319 ) ) ;
#12170 = CARTESIAN_POINT ( 'NONE',  ( -1.002407869896990045, 0.1264236179284866091, 0.9325787401037164415 ) ) ;
#12171 = CIRCLE ( 'NONE', #13691, 0.01968503937007870172 ) ;
#12172 = CARTESIAN_POINT ( 'NONE',  ( -0.8759842519685039353, 0.1787899950787401882, 0.5880905511273386566 ) ) ;
#12173 = LINE ( 'NONE', #26797, #11759 ) ;
#12174 = DIRECTION ( 'NONE',  ( -0.000000000000000000, 1.000000000000000000, 0.000000000000000000 ) ) ;
#12175 = DIRECTION ( 'NONE',  ( 1.000000000000000000, 0.000000000000000000, -7.044195017643630340E-15 ) ) ;
#12176 = CARTESIAN_POINT ( 'NONE',  ( -0.1787899950787401604, -0.5650845981504987181, 0.07405724077823318263 ) ) ;
#12177 = CARTESIAN_POINT ( 'NONE',  ( -0.1574815732576543281, -0.08955969983079922758, 0.1660848416297525665 ) ) ;
#12178 = CARTESIAN_POINT ( 'NONE',  ( 0.06523048226347956391, 0.03395669302091284397, 0.1574803149606297803 ) ) ;
#12179 = CARTESIAN_POINT ( 'NONE',  ( -1.033464566929133799, 0.000000000000000000, 1.574803149498771537 ) ) ;
#12180 = DIRECTION ( 'NONE',  ( 0.000000000000000000, -1.000000000000000000, 0.000000000000000000 ) ) ;
#12181 = FACE_OUTER_BOUND ( 'NONE', #24547, .T. ) ;
#12182 = CARTESIAN_POINT ( 'NONE',  ( -0.8759842519685039353, 0.1787899950787401882, 0.4256889763241890057 ) ) ;
#12183 = CARTESIAN_POINT ( 'NONE',  ( -1.033464566929134687, -0.06523048226347956391, 0.4010826771653545619 ) ) ;
#12184 = VERTEX_POINT ( 'NONE', #1659 ) ;
#12185 = EDGE_CURVE ( 'NONE', #17885, #20293, #38094, .T. ) ;
#12186 = CARTESIAN_POINT ( 'NONE',  ( -0.8759842519685039353, 0.1787899950787401882, 1.493602362150960650 ) ) ;
#12187 = CARTESIAN_POINT ( 'NONE',  ( -0.07405724077823318263, -1.297244094434425010, 0.1787899950787401604 ) ) ;
#12188 = CARTESIAN_POINT ( 'NONE',  ( 0.1787899950787401604, -1.513779527505292322, -0.07405724077823318263 ) ) ;
#12189 = EDGE_CURVE ( 'NONE', #17392, #8358, #18245, .T. ) ;
#12190 = CIRCLE ( 'NONE', #39696, 0.1968503937007874405 ) ;
#12191 = DIRECTION ( 'NONE',  ( -1.000000000000000000, -0.000000000000000000, 0.000000000000000000 ) ) ;
#12192 = CARTESIAN_POINT ( 'NONE',  ( -0.8070866141732283561, -0.0009842519685049383633, 0.8559055118110230342 ) ) ;
#12193 = FACE_OUTER_BOUND ( 'NONE', #22167, .T. ) ;
#12194 = CARTESIAN_POINT ( 'NONE',  ( -0.8759842519685039353, 0.1574803149606299191, 1.151574803042078710 ) ) ;
#12195 = CARTESIAN_POINT ( 'NONE',  ( 1.054774247047244540, -0.07405724077823318263, 0.5364173227808821665 ) ) ;
#12197 = CYLINDRICAL_SURFACE ( 'NONE', #24627, 0.09842519685039310962 ) ;
#12196 = CARTESIAN_POINT ( 'NONE',  ( 0.1574803149606300301, -0.3203740157480316486, -0.06523048226347956391 ) ) ;
#12198 = CARTESIAN_POINT ( 'NONE',  ( 0.7185039370078739607, 1.928577636452523993E-17, 1.988188976270425234 ) ) ;
#12199 = ORIENTED_EDGE ( 'NONE', *, *, #45641, .F. ) ;
#12200 = CYLINDRICAL_SURFACE ( 'NONE', #33811, 0.1864803149606299171 ) ;
#12201 = EDGE_CURVE ( 'NONE', #36286, #31518, #7530, .T. ) ;
#12202 = CARTESIAN_POINT ( 'NONE',  ( -0.6971942568897648851, 0.07405724077823318263, 1.107283464513165727 ) ) ;
#12203 = CARTESIAN_POINT ( 'NONE',  ( 0.9412147342319837628, 0.1574803149606300301, 1.040846456692913424 ) ) ;
#12204 = AXIS2_PLACEMENT_3D ( 'NONE', #35577, #31522, #5627 ) ;
#12205 = DIRECTION ( 'NONE',  ( 1.822029033848725028E-16, 0.000000000000000000, 1.000000000000000000 ) ) ;
#12206 = CARTESIAN_POINT ( 'NONE',  ( -0.1113553986120547346, -0.5344488187901101917, -0.1113553986120547346 ) ) ;
#12207 = ADVANCED_FACE ( 'NONE', ( #30933 ), #35103, .T. ) ;
#12208 = DIRECTION ( 'NONE',  ( -1.000000000000000000, 0.000000000000000000, 0.000000000000000000 ) ) ;
#12209 = CARTESIAN_POINT ( 'NONE',  ( 1.033464566929133799, 0.000000000000000000, 1.259842519577511810 ) ) ;
#12210 = CARTESIAN_POINT ( 'NONE',  ( -0.1353283724619816497, -0.08956113309537444556, 0.09080182561100422212 ) ) ;
#12211 = VERTEX_POINT ( 'NONE', #2360 ) ;
#12212 = VECTOR ( 'NONE', #20033, 39.37007874015748143 ) ;
#12213 = CARTESIAN_POINT ( 'NONE',  ( -1.033464566929133799, 1.928577636452524610E-17, 2.869337061179095023E-17 ) ) ;
#12214 = CARTESIAN_POINT ( 'NONE',  ( 0.6971942568897626646, -0.07405724077823297447, 0.7135826771115916234 ) ) ;
#12215 = ORIENTED_EDGE ( 'NONE', *, *, #16423, .T. ) ;
#12216 = CARTESIAN_POINT ( 'NONE',  ( 0.9873396505805591694, -0.1113553986120547346, 0.8316929133858268486 ) ) ;
#12217 = FACE_OUTER_BOUND ( 'NONE', #40358, .T. ) ;
#12218 = CARTESIAN_POINT ( 'NONE',  ( 0.1787899950787401882, -1.673720472387181024, -2.189545951927503898E-17 ) ) ;
#12219 = CARTESIAN_POINT ( 'NONE',  ( 0.1787899950787401882, -0.8518700786863936392, -2.189545951927503898E-17 ) ) ;
#12220 = CARTESIAN_POINT ( 'NONE',  ( 0.1574803149606300301, -1.186515748031495843, -0.06523048226347956391 ) ) ;
#12221 = CARTESIAN_POINT ( 'NONE',  ( 1.033464566929134687, 0.06523048226347956391, 1.183562992018456272 ) ) ;
#12222 = CARTESIAN_POINT ( 'NONE',  ( 0.7185039370078739607, 1.928577636452523993E-17, 1.840551181102362266 ) ) ;
#12223 = CARTESIAN_POINT ( 'NONE',  ( -1.054774247047244540, 0.07405724077823318263, 0.4576771653005669016 ) ) ;
#12224 = EDGE_LOOP ( 'NONE', ( #15611, #33162 ) ) ;
#12225 = CARTESIAN_POINT ( 'NONE',  ( -0.6971942568897637749, 2.189545951927499583E-17, 1.818405511757259729 ) ) ;
#12226 = CARTESIAN_POINT ( 'NONE',  ( 0.7495606340400177148, 0.1264236179284866091, 1.892224409395055096 ) ) ;
#12227 = ORIENTED_EDGE ( 'NONE', *, *, #16063, .F. ) ;
#12228 = CARTESIAN_POINT ( 'NONE',  ( 0.1574803149606300301, -1.373523621939715555, -0.06523048226347956391 ) ) ;
#12229 = CARTESIAN_POINT ( 'NONE',  ( -0.8019270111902717657, -0.1787899950787401604, 0.9202755904974182499 ) ) ;
#12230 = CARTESIAN_POINT ( 'NONE',  ( -0.05036568513382595758, -0.2664124483477782190, -0.3061783854718737596 ) ) ;
#12231 = CARTESIAN_POINT ( 'NONE',  ( 0.6971942568897637749, 2.189545951927499583E-17, 0.4010826771115905687 ) ) ;
#12232 = CARTESIAN_POINT ( 'NONE',  ( -0.6971942568897648851, -0.07405724077823297447, 1.422244094434426120 ) ) ;
#12233 = CARTESIAN_POINT ( 'NONE',  ( -0.6971942568897648851, 0.07405724077823318263, 1.259842519631276359 ) ) ;
#12234 = CARTESIAN_POINT ( 'NONE',  ( -0.6971942568897648851, -0.07405724077823297447, 0.7923228345919055560 ) ) ;
#12235 = CARTESIAN_POINT ( 'NONE',  ( -0.6971942568897637749, 2.189545951927499583E-17, 0.1254921259304885850 ) ) ;
#12236 = VECTOR ( 'NONE', #33617, 39.37007874015748854 ) ;
#12237 = CARTESIAN_POINT ( 'NONE',  ( -0.8107537697050254399, 0.1574803149606300301, 1.665846456585386548 ) ) ;
#12238 = CARTESIAN_POINT ( 'NONE',  ( -0.8759842519685039353, 0.1787899950787401882, 1.690452755851748146 ) ) ;
#12239 = CARTESIAN_POINT ( 'NONE',  ( -0.8107537697050253289, -0.1574803149606297803, 1.995570866034207080 ) ) ;
#12240 = FACE_OUTER_BOUND ( 'NONE', #21625, .T. ) ;
#12241 = CARTESIAN_POINT ( 'NONE',  ( -1.033464566929133799, 0.000000000000000000, 1.742125984251968518 ) ) ;
#12242 = FACE_OUTER_BOUND ( 'NONE', #35117, .T. ) ;
#12243 = CARTESIAN_POINT ( 'NONE',  ( 0.6971942568897637749, 2.189545951927499583E-17, 1.660925196796630088 ) ) ;
#12244 = CARTESIAN_POINT ( 'NONE',  ( -0.2423422045102378020, -0.09842519685039370636, -0.009343655355443130847 ) ) ;
#12245 = CARTESIAN_POINT ( 'NONE',  ( 0.1602931993194442739, -0.07955613945526318620, 0.1377952755905511861 ) ) ;
#12246 = VERTEX_POINT ( 'NONE', #13626 ) ;
#12247 = EDGE_CURVE ( 'NONE', #28970, #23848, #9580, .T. ) ;
#12248 = AXIS2_PLACEMENT_3D ( 'NONE', #11578, #4586, #40771 ) ;
#12249 = EDGE_LOOP ( 'NONE', ( #28262, #46662, #17289, #13117, #41411 ) ) ;
#12250 = AXIS2_PLACEMENT_3D ( 'NONE', #30871, #41587, #15772 ) ;
#12251 = ADVANCED_FACE ( 'NONE', ( #24199 ), #41891, .T. ) ;
#12252 = APPLICATION_CONTEXT ( 'automotive_design' ) ;
#12253 = VERTEX_POINT ( 'NONE', #38327 ) ;
#12254 = CARTESIAN_POINT ( 'NONE',  ( 0.07405724077823318263, -0.8198818897100156322, 0.1787899950787401604 ) ) ;
#12255 = CARTESIAN_POINT ( 'NONE',  ( -1.094772975963752103E-17, -1.112696850339937038, -0.1787899950787401882 ) ) ;
#12256 = CARTESIAN_POINT ( 'NONE',  ( -0.1476377952755905387, -0.2142072668875215635, -1.269802121763611291 ) ) ;
#12257 = CARTESIAN_POINT ( 'NONE',  ( -0.07444174185955065859, -0.3479768804491872314, 0.1797182628040039087 ) ) ;
#12258 = CARTESIAN_POINT ( 'NONE',  ( 0.06523048226347956391, 0.1569881889763779237, -0.1574803149606300301 ) ) ;
#12259 = DIRECTION ( 'NONE',  ( -1.000000000000000000, 0.000000000000000000, 0.000000000000000000 ) ) ;
#12260 = CARTESIAN_POINT ( 'NONE',  ( 1.002407869896990045, -0.1264236179284866091, 0.8439960629383622681 ) ) ;
#12262 = CARTESIAN_POINT ( 'NONE',  ( -1.033464566929133799, 0.000000000000000000, 1.535433070758614127 ) ) ;
#12261 = CARTESIAN_POINT ( 'NONE',  ( 0.05473415491935430810, 0.2638934531858505017, -0.05654496252297439018 ) ) ;
#12263 = CARTESIAN_POINT ( 'NONE',  ( -0.9873396505805591694, -0.1113553986120547346, 0.07381889753026830980 ) ) ;
#12264 = CARTESIAN_POINT ( 'NONE',  ( 0.8107537697050234415, -0.1574803149606297803, 0.06643700776648873985 ) ) ;
#12265 = CARTESIAN_POINT ( 'NONE',  ( 1.033464566929134687, 0.06523048226347956391, 0.1697834645669291653 ) ) ;
#12266 = DIRECTION ( 'NONE',  ( 6.938893903907227392E-16, -0.6156614753256598460, -0.7880107536067207930 ) ) ;
#12269 = EDGE_CURVE ( 'NONE', #41828, #39972, #22070, .T. ) ;
#12268 = CARTESIAN_POINT ( 'NONE',  ( -0.1787899950787401604, -0.3572834645131658382, 0.07405724077823318263 ) ) ;
#12267 = CARTESIAN_POINT ( 'NONE',  ( 0.1113553986120547346, -0.9872047243019212992, 0.1113553986120547346 ) ) ;
#12270 = CARTESIAN_POINT ( 'NONE',  ( 0.1574803149606299191, 0.000000000000000000, 2.731847993664263218E-16 ) ) ;
#12271 = CIRCLE ( 'NONE', #10747, 0.1968503937007874127 ) ;
#12272 = CARTESIAN_POINT ( 'NONE',  ( -0.07405724077823318263, -1.174212598371433769, 0.1787899950787401604 ) ) ;
#12273 = CARTESIAN_POINT ( 'NONE',  ( 1.054774247047244096, 0.000000000000000000, 0.3026574802611972648 ) ) ;
#12274 = ( BOUNDED_CURVE ( )  B_SPLINE_CURVE ( 2, ( #38417, #27670, #20194, #1988, #42230, #24052, #38655, #5828, #11319 ),
 .UNSPECIFIED., .F., .T. ) 
 B_SPLINE_CURVE_WITH_KNOTS ( ( 3, 2, 2, 2, 3 ),
 ( 0.5000000000000000000, 0.5024999999999999467, 0.5050000000000000044, 0.5074999999999999512, 0.5100000000000000089 ),
 .UNSPECIFIED. ) 
 CURVE ( )  GEOMETRIC_REPRESENTATION_ITEM ( )  RATIONAL_B_SPLINE_CURVE ( ( 1.000000000000000000, 0.9238795325112869605, 1.000000000000000000, 0.9238795325112869605, 1.000000000000000000, 0.9238795325112869605, 1.000000000000000000, 0.9238795325112869605, 1.000000000000000000 ) ) 
 REPRESENTATION_ITEM ( '' )  ) ;
#12275 = DIRECTION ( 'NONE',  ( -1.000000000000000000, 0.000000000000000000, 0.000000000000000000 ) ) ;
#12276 = CARTESIAN_POINT ( 'NONE',  ( -1.054774247047244096, 0.000000000000000000, 1.675688976324189117 ) ) ;
#12277 = ORIENTED_EDGE ( 'NONE', *, *, #40328, .T. ) ;
#12278 = CARTESIAN_POINT ( 'NONE',  ( -1.054774247047244540, -0.07405724077823318263, 1.363188976324188895 ) ) ;
#12280 = AXIS2_PLACEMENT_3D ( 'NONE', #13897, #43109, #24926 ) ;
#12279 = DIRECTION ( 'NONE',  ( 0.000000000000000000, -1.000000000000000000, 0.000000000000000000 ) ) ;
#12281 = CARTESIAN_POINT ( 'NONE',  ( 0.8019270111902717657, -0.1787899950787401604, 1.274606299158834277 ) ) ;
#12282 = CARTESIAN_POINT ( 'NONE',  ( -0.9500414927467378812, 0.1787899950787401604, 1.249999999946235896 ) ) ;
#12283 = DIRECTION ( 'NONE',  ( 0.000000000000000000, 0.000000000000000000, 1.000000000000000000 ) ) ;
#12284 = CARTESIAN_POINT ( 'NONE',  ( 0.06167052456099836322, -0.09842519458604685745, -0.1678199136211908638 ) ) ;
#12285 = CARTESIAN_POINT ( 'NONE',  ( -0.7185039370078739607, 1.928577636452523993E-17, 1.358267716427907779 ) ) ;
#12286 = CARTESIAN_POINT ( 'NONE',  ( 0.7495606340400177148, 0.1264236179284866091, 0.3961614172690708924 ) ) ;
#12287 = CARTESIAN_POINT ( 'NONE',  ( -0.8019270111902716547, 0.1787899950787401604, 0.3100393700249766682 ) ) ;
#12288 = ORIENTED_EDGE ( 'NONE', *, *, #16824, .T. ) ;
#12289 = CARTESIAN_POINT ( 'NONE',  ( -0.9412147342319837628, 0.1574803149606300301, 1.355807086614173596 ) ) ;
#12290 = CARTESIAN_POINT ( 'NONE',  ( -1.033464566929134687, -0.06523048226347956391, 0.3617125984251968740 ) ) ;
#12291 = CARTESIAN_POINT ( 'NONE',  ( 1.054774247047244096, 0.000000000000000000, 1.208169291284818980 ) ) ;
#12292 = CARTESIAN_POINT ( 'NONE',  ( -0.6971942568897637749, 2.189545951927499583E-17, 1.970964566875370139 ) ) ;
#12293 = CARTESIAN_POINT ( 'NONE',  ( -0.8759842519685039353, -0.1574803149606299191, 1.968503937007874072 ) ) ;
#12294 = ORIENTED_EDGE ( 'NONE', *, *, #46313, .F. ) ;
#12295 = EDGE_CURVE ( 'NONE', #19153, #2867, #19779, .T. ) ;
#12296 = CARTESIAN_POINT ( 'NONE',  ( 0.9500414927467378812, -0.1787899950787401604, 1.983267716481667886 ) ) ;
#12297 = ( BOUNDED_CURVE ( )  B_SPLINE_CURVE ( 2, ( #20332, #24183, #24638, #5942, #20563, #17212, #31848, #13606, #28246 ),
 .UNSPECIFIED., .F., .T. ) 
 B_SPLINE_CURVE_WITH_KNOTS ( ( 3, 2, 2, 2, 3 ),
 ( 0.5300000000000000266, 0.5324999999999999734, 0.5350000000000000311, 0.5374999999999999778, 0.5400000000000000355 ),
 .UNSPECIFIED. ) 
 CURVE ( )  GEOMETRIC_REPRESENTATION_ITEM ( )  RATIONAL_B_SPLINE_CURVE ( ( 1.000000000000000000, 0.9238795325112869605, 1.000000000000000000, 0.9238795325112869605, 1.000000000000000000, 0.9238795325112869605, 1.000000000000000000, 0.9238795325112869605, 1.000000000000000000 ) ) 
 REPRESENTATION_ITEM ( '' )  ) ;
#12298 = EDGE_CURVE ( 'NONE', #17885, #38458, #47130, .T. ) ;
#12299 = AXIS2_PLACEMENT_3D ( 'NONE', #22088, #37590, #25475 ) ;
#12300 = CARTESIAN_POINT ( 'NONE',  ( -0.9412147342319837628, 0.1574803149606300301, 1.464074803042079376 ) ) ;
#12301 = FACE_OUTER_BOUND ( 'NONE', #16874, .T. ) ;
#12302 = CARTESIAN_POINT ( 'NONE',  ( 0.1264236179284866091, -1.418923180827663444, 0.1264236179284866091 ) ) ;
#12303 = ORIENTED_EDGE ( 'NONE', *, *, #21297, .T. ) ;
#12304 = DIRECTION ( 'NONE',  ( 0.000000000000000000, 0.000000000000000000, -1.000000000000000000 ) ) ;
#12305 = CARTESIAN_POINT ( 'NONE',  ( -0.1264236179284866091, -0.4286417322297008115, 0.1264236179284866091 ) ) ;
#12306 = ADVANCED_FACE ( 'NONE', ( #29775 ), #11774, .T. ) ;
#12307 = CARTESIAN_POINT ( 'NONE',  ( -0.2559070959273828105, 0.05936816977299741449, -0.3110460671459447379 ) ) ;
#12308 = DIRECTION ( 'NONE',  ( 1.822029033848725028E-16, 0.000000000000000000, 1.000000000000000000 ) ) ;
#12309 = ORIENTED_EDGE ( 'NONE', *, *, #34408, .F. ) ;
#12310 = CARTESIAN_POINT ( 'NONE',  ( 0.6971942568897648851, -0.07405724077823297447, 1.304133858213953667 ) ) ;
#12311 = AXIS2_PLACEMENT_3D ( 'NONE', #40869, #12404, #41105 ) ;
#12312 = ADVANCED_FACE ( 'NONE', ( #36687 ), #40019, .T. ) ;
#12313 = CARTESIAN_POINT ( 'NONE',  ( 1.033464566929134687, 0.06523048226347956391, 1.459153543199560144 ) ) ;
#12314 = VECTOR ( 'NONE', #4333, 39.37007874015748143 ) ;
#12315 = DIRECTION ( 'NONE',  ( 1.000000000000000000, 0.000000000000000000, 0.000000000000000000 ) ) ;
#12316 = CARTESIAN_POINT ( 'NONE',  ( 0.004734662961589819648, -0.09521559318209203704, -0.1106847963722246697 ) ) ;
#12317 = CARTESIAN_POINT ( 'NONE',  ( 1.002407869896990045, 0.1264236179284866091, 1.562499999946236118 ) ) ;
#12318 = CARTESIAN_POINT ( 'NONE',  ( 0.1787899950787401604, 0.1238917798022573097, -0.07405724077823318263 ) ) ;
#12319 = CARTESIAN_POINT ( 'NONE',  ( -0.1264236179284866091, 0.1077755906049446960, -0.1264236179284866091 ) ) ;
#12320 = APPLICATION_PROTOCOL_DEFINITION ( 'draft international standard', 'automotive_design', 1998, #44058 ) ;
#12321 = CARTESIAN_POINT ( 'NONE',  ( 0.003028377451660003734, -0.03839001012990030104, -0.1377950774391751565 ) ) ;
#12322 = VERTEX_POINT ( 'NONE', #22769 ) ;
#12323 = CARTESIAN_POINT ( 'NONE',  ( -0.9500414927467377701, 0.1787899950787401604, 0.5856299212060785964 ) ) ;
#12325 = DIRECTION ( 'NONE',  ( 0.000000000000000000, 0.000000000000000000, 1.000000000000000000 ) ) ;
#12324 = CARTESIAN_POINT ( 'NONE',  ( -0.1574803149606299191, -0.7362204724409449064, 0.000000000000000000 ) ) ;
#12326 = CARTESIAN_POINT ( 'NONE',  ( 0.1270800023317771588, -1.629965069425564961, -0.1270800023317771588 ) ) ;
#12327 = DIRECTION ( 'NONE',  ( 0.000000000000000000, 0.000000000000000000, -1.000000000000000000 ) ) ;
#12328 = CARTESIAN_POINT ( 'NONE',  ( 0.1574803149606300301, -0.4680118109160952278, -0.06523048226347956391 ) ) ;
#12329 = CARTESIAN_POINT ( 'NONE',  ( 1.033464566929133799, 0.000000000000000000, 1.653543306979086580 ) ) ;
#12330 = CARTESIAN_POINT ( 'NONE',  ( 1.054774247047244096, 0.000000000000000000, 1.405019684985606476 ) ) ;
#12331 = CARTESIAN_POINT ( 'NONE',  ( 1.054774247047244096, 0.000000000000000000, 1.872539370024976391 ) ) ;
#12332 = CARTESIAN_POINT ( 'NONE',  ( 0.8759842519685039353, 0.1787899950787401882, 0.3075787401037169411 ) ) ;
#12334 = ORIENTED_EDGE ( 'NONE', *, *, #4094, .F. ) ;
#12333 = DIRECTION ( 'NONE',  ( -1.000000000000000000, 0.000000000000000000, 0.000000000000000000 ) ) ;
#12335 = DIRECTION ( 'NONE',  ( -1.000000000000000000, 0.000000000000000000, 0.000000000000000000 ) ) ;
#12336 = DIRECTION ( 'NONE',  ( 0.000000000000000000, -1.000000000000000000, 0.000000000000000000 ) ) ;
#12337 = CARTESIAN_POINT ( 'NONE',  ( 0.1264236179284866091, 0.08809055123486594918, 0.1264236179284866091 ) ) ;
#12338 = CARTESIAN_POINT ( 'NONE',  ( 0.6971942568897637749, 2.189545951927499583E-17, 0.5142716534895434011 ) ) ;
#12339 = DIRECTION ( 'NONE',  ( -1.000000000000000000, 0.000000000000000000, 0.000000000000000000 ) ) ;
#12340 = AXIS2_PLACEMENT_3D ( 'NONE', #27019, #12635, #14858 ) ;
#12341 = CARTESIAN_POINT ( 'NONE',  ( 0.2395294000716133853, 0.1968503937007874127, 1.181102362204724310 ) ) ;
#12342 = CARTESIAN_POINT ( 'NONE',  ( 0.8107537697050253289, 0.1574803149606300301, 0.8390748030420787096 ) ) ;
#12343 = ORIENTED_EDGE ( 'NONE', *, *, #2059, .F. ) ;
#12344 = CARTESIAN_POINT ( 'NONE',  ( -0.8759842519685039353, 0.000000000000000000, 0.000000000000000000 ) ) ;
#12345 = CARTESIAN_POINT ( 'NONE',  ( -1.033464566929133799, 0.000000000000000000, 0.1673228346456692994 ) ) ;
#12346 = VERTEX_POINT ( 'NONE', #4297 ) ;
#12347 = CARTESIAN_POINT ( 'NONE',  ( -0.8759842519685039353, -0.1574803149606299191, 0.5413385825696385156 ) ) ;
#12348 = AXIS2_PLACEMENT_3D ( 'NONE', #19797, #38251, #5412 ) ;
#12349 = CARTESIAN_POINT ( 'NONE',  ( -0.5555748031496036132, 0.9100161909011723615, 0.01858545845903165558 ) ) ;
#12350 = CARTESIAN_POINT ( 'NONE',  ( 0.8759842519685039353, -0.1787899950787401882, 1.587106299158834721 ) ) ;
#12351 = CARTESIAN_POINT ( 'NONE',  ( -0.9412147342319837628, -0.1574803149606297803, 1.301673228346455602 ) ) ;
#12352 = DIRECTION ( 'NONE',  ( 0.000000000000000000, 0.000000000000000000, 1.000000000000000000 ) ) ;
#12354 = DIRECTION ( 'NONE',  ( 1.000000000000000000, 0.000000000000000000, 0.000000000000000000 ) ) ;
#12353 = CARTESIAN_POINT ( 'NONE',  ( -0.7646288533564489232, 0.1113553986120547346, 0.7332677165354331006 ) ) ;
#12355 = CARTESIAN_POINT ( 'NONE',  ( 0.7185039370078778465, -0.06523048226348396317, 1.911909448711369697 ) ) ;
#12356 = AXIS2_PLACEMENT_3D ( 'NONE', #14379, #32844, #47439 ) ;
#12357 = CARTESIAN_POINT ( 'NONE',  ( 1.033464566929134687, 0.06523048226347956391, 1.380413385719244213 ) ) ;
#12358 = ORIENTED_EDGE ( 'NONE', *, *, #25512, .F. ) ;
#12359 = VERTEX_POINT ( 'NONE', #33589 ) ;
#12360 = CARTESIAN_POINT ( 'NONE',  ( -0.05730322896416230327, -0.07836638817768154519, -0.2523490388730016964 ) ) ;
#12361 = ORIENTED_EDGE ( 'NONE', *, *, #24040, .F. ) ;
#12362 = CARTESIAN_POINT ( 'NONE',  ( 0.6971942568897637749, 2.189545951927499583E-17, 0.6766732282926929409 ) ) ;
#12363 = VECTOR ( 'NONE', #16978, 39.37007874015748143 ) ;
#12364 = CARTESIAN_POINT ( 'NONE',  ( -0.8759842519685039353, -0.1787899950787401882, 1.587106299158834721 ) ) ;
#12365 = CARTESIAN_POINT ( 'NONE',  ( 0.06523048226347956391, -0.04478346445940203924, 0.1574803149606297803 ) ) ;
#12366 = CARTESIAN_POINT ( 'NONE',  ( -0.8019270111902717657, -0.1787899950787401604, 1.313976377898992132 ) ) ;
#12367 = EDGE_CURVE ( 'NONE', #21819, #8144, #41163, .T. ) ;
#12368 = DIRECTION ( 'NONE',  ( -1.000000000000000000, 5.472378587457090550E-15, -4.275490733183370330E-15 ) ) ;
#12369 = DIRECTION ( 'NONE',  ( 0.000000000000000000, -1.000000000000000000, 0.000000000000000000 ) ) ;
#12370 = CARTESIAN_POINT ( 'NONE',  ( 0.1264236179284866091, -1.025222393426088452, 0.1264236179284866091 ) ) ;
#12371 = ORIENTED_EDGE ( 'NONE', *, *, #6974, .F. ) ;
#12372 = CARTESIAN_POINT ( 'NONE',  ( 0.1787899950787401882, -0.02017716530056720692, -2.189545951927503898E-17 ) ) ;
#12373 = ORIENTED_EDGE ( 'NONE', *, *, #22828, .F. ) ;
#12374 = ORIENTED_EDGE ( 'NONE', *, *, #14798, .T. ) ;
#12375 = EDGE_CURVE ( 'NONE', #47218, #37257, #18468, .T. ) ;
#12376 = CARTESIAN_POINT ( 'NONE',  ( -0.2559082480989984254, -0.02481004614261094615, -0.3144388117053942833 ) ) ;
#12377 = CARTESIAN_POINT ( 'NONE',  ( -0.1574803149606299191, 0.2876548164643190630, -0.2627373885913885099 ) ) ;
#12378 = CIRCLE ( 'NONE', #8516, 0.1574803149606299191 ) ;
#12379 = AXIS2_PLACEMENT_3D ( 'NONE', #32536, #33483, #25809 ) ;
#12380 = VECTOR ( 'NONE', #32639, 39.37007874015748143 ) ;
#12381 = CARTESIAN_POINT ( 'NONE',  ( -0.1264236179284866091, -0.5910433070328504623, 0.1264236179284866091 ) ) ;
#12382 = VECTOR ( 'NONE', #14265, 39.37007874015748143 ) ;
#12383 = CARTESIAN_POINT ( 'NONE',  ( -0.6971942568897626646, 0.07405724077823318263, 0.2017716534895435399 ) ) ;
#12384 = CARTESIAN_POINT ( 'NONE',  ( -1.033464566929134687, -0.06523048226347956391, 1.070374015748031038 ) ) ;
#12385 = CARTESIAN_POINT ( 'NONE',  ( 0.7185039370078739607, 1.928577636452523993E-17, 0.6594488188976378451 ) ) ;
#12386 = CARTESIAN_POINT ( 'NONE',  ( -0.8759842519685039353, 0.000000000000000000, 0.000000000000000000 ) ) ;
#12387 = CARTESIAN_POINT ( 'NONE',  ( -0.1797182628040039365, -1.182130423756273752, 0.000000000000000000 ) ) ;
#12388 = FACE_OUTER_BOUND ( 'NONE', #25118, .T. ) ;
#12389 = CARTESIAN_POINT ( 'NONE',  ( 1.002407869896990045, 0.1264236179284866091, 0.9374999999462362288 ) ) ;
#12390 = CARTESIAN_POINT ( 'NONE',  ( 0.7495606340400177148, 0.1264236179284866091, 1.414862204670645829 ) ) ;
#12391 = CARTESIAN_POINT ( 'NONE',  ( 0.8019270111902716547, 0.1787899950787401604, 0.1131889763241894220 ) ) ;
#12392 = LINE ( 'NONE', #8766, #39135 ) ;
#12393 = CARTESIAN_POINT ( 'NONE',  ( 0.7185039370078746268, -0.06523048226347956391, 1.567421259842519676 ) ) ;
#12394 = CARTESIAN_POINT ( 'NONE',  ( 0.7290331858934718801, -0.08312163584841733566, 1.984889472013028566 ) ) ;
#12395 = CARTESIAN_POINT ( 'NONE',  ( 1.033464566929133799, 0.000000000000000000, 0.6397637795275591399 ) ) ;
#12396 = CARTESIAN_POINT ( 'NONE',  ( -0.7185039370078739607, 1.928577636452523993E-17, 1.633858267609007875 ) ) ;
#12397 = CARTESIAN_POINT ( 'NONE',  ( 0.1264236179284866091, 0.05364173233722803469, 0.1264236179284866091 ) ) ;
#12398 = CARTESIAN_POINT ( 'NONE',  ( 0.8759842519685039353, -0.1574803149606299191, 0.7874015748031496509 ) ) ;
#12399 = CARTESIAN_POINT ( 'NONE',  ( 0.9500414927467377701, -0.1787899950787401604, 1.038385826717890259 ) ) ;
#12400 = CARTESIAN_POINT ( 'NONE',  ( 0.9500414927467377701, -0.1787899950787401604, 1.751968503883245987 ) ) ;
#12401 = CARTESIAN_POINT ( 'NONE',  ( -0.07405724077823318263, -0.9921259841982054128, -0.1787899950787401604 ) ) ;
#12402 = CARTESIAN_POINT ( 'NONE',  ( 0.7185039370078739607, 1.928577636452523993E-17, 0.4133858266641267654 ) ) ;
#12403 = VERTEX_POINT ( 'NONE', #26392 ) ;
#12404 = DIRECTION ( 'NONE',  ( -0.000000000000000000, 1.000000000000000000, 0.000000000000000000 ) ) ;
#12405 = CARTESIAN_POINT ( 'NONE',  ( -0.7185039370078739607, 1.928577636452523993E-17, 0.1771653542231816925 ) ) ;
#12406 = CARTESIAN_POINT ( 'NONE',  ( 2.892866454678787531E-17, -1.661417322727118062, 0.1574803149606299191 ) ) ;
#12407 = EDGE_LOOP ( 'NONE', ( #20343, #11360, #31214, #36046 ) ) ;
#12408 = CARTESIAN_POINT ( 'NONE',  ( -0.9412147342319837628, 0.1574803149606300301, 0.1254921258767249526 ) ) ;
#12409 = CARTESIAN_POINT ( 'NONE',  ( -1.094772975963752103E-17, -0.08907480309584270284, -0.1787899950787401882 ) ) ;
#12410 = CARTESIAN_POINT ( 'NONE',  ( 0.9500414927467378812, -0.1787899950787401604, 1.156496062938362046 ) ) ;
#12411 = ORIENTED_EDGE ( 'NONE', *, *, #14434, .F. ) ;
#12412 = CARTESIAN_POINT ( 'NONE',  ( 0.2395294000716133853, 0.1968503937007874127, 0.4921259842519685179 ) ) ;
#12413 = VECTOR ( 'NONE', #27563, 39.37007874015748143 ) ;
#12414 = CARTESIAN_POINT ( 'NONE',  ( -0.8759842519685039353, 0.1787899950787401882, 0.5437992125446614589 ) ) ;
#12415 = CARTESIAN_POINT ( 'NONE',  ( -0.8107537697050234415, -0.1574803149606297803, 0.2731299212598424231 ) ) ;
#12416 = CARTESIAN_POINT ( 'NONE',  ( -0.6971942568897626646, -0.07405724077823297447, 0.3198818897100162983 ) ) ;
#12417 = ORIENTED_EDGE ( 'NONE', *, *, #27367, .F. ) ;
#12419 = CARTESIAN_POINT ( 'NONE',  ( -0.07405724077823318263, -1.533464566875370805, 0.1787899950787401604 ) ) ;
#12418 = CARTESIAN_POINT ( 'NONE',  ( 2.892866454678787531E-17, -0.3622047243019216878, 0.1574803149606299191 ) ) ;
#12420 = AXIS2_PLACEMENT_3D ( 'NONE', #32416, #39325, #14656 ) ;
#12421 = AXIS2_PLACEMENT_3D ( 'NONE', #19972, #5840, #30561 ) ;
#12422 = CARTESIAN_POINT ( 'NONE',  ( -0.8019270111902717657, 0.1787899950787401604, 0.5511811023084406402 ) ) ;
#12423 = EDGE_CURVE ( 'NONE', #8964, #8992, #34168, .T. ) ;
#12424 = CARTESIAN_POINT ( 'NONE',  ( -0.2559055118110236116, 0.1477471161312047254, -0.2921040715117803055 ) ) ;
#12425 = CARTESIAN_POINT ( 'NONE',  ( -0.7185039370078739607, 1.928577636452523993E-17, 1.683070866141732402 ) ) ;
#12426 = CARTESIAN_POINT ( 'NONE',  ( -0.1264236179284866091, -0.5232538894890811365, 0.1264236179284866091 ) ) ;
#12427 = CARTESIAN_POINT ( 'NONE',  ( -0.1681363471019937106, -0.08956127397141554203, -0.03619664881022559288 ) ) ;
#12428 = CARTESIAN_POINT ( 'NONE',  ( 1.033464566929134687, -0.06523048226347956391, 0.4798228346456689386 ) ) ;
#12429 = DIRECTION ( 'NONE',  ( 0.000000000000000000, 0.000000000000000000, 1.000000000000000000 ) ) ;
#12430 = EDGE_CURVE ( 'NONE', #45189, #36896, #40255, .T. ) ;
#12431 = CARTESIAN_POINT ( 'NONE',  ( -0.8107537697050254399, -0.1574803149606297803, 1.168799212490898576 ) ) ;
#12432 = CARTESIAN_POINT ( 'NONE',  ( -0.6971942568897626646, -0.07405724077823297447, 0.4379921259304882519 ) ) ;
#12433 = CARTESIAN_POINT ( 'NONE',  ( 3.284318927891251994E-17, -1.817545228071759889, 0.1787899950787401882 ) ) ;
#12434 = DIRECTION ( 'NONE',  ( 0.000000000000000000, -0.7880107536067207930, 0.6156614753256598460 ) ) ;
#12435 = CARTESIAN_POINT ( 'NONE',  ( 0.1787899950787401604, -1.562992125930488196, 0.07405724077823318263 ) ) ;
#12436 = CARTESIAN_POINT ( 'NONE',  ( -0.1264236179284866091, -1.609744094434425232, 0.1264236179284866091 ) ) ;
#12437 = CONICAL_SURFACE ( 'NONE', #43778, 0.1377952755905509641, 0.9599310885968941331 ) ;
#12438 = CARTESIAN_POINT ( 'NONE',  ( 0.5057057357416000487, -0.09842519685039370636, 1.205361022782828805E-17 ) ) ;
#12439 = CYLINDRICAL_SURFACE ( 'NONE', #29320, 0.7874015748031496509 ) ;
#12440 = ADVANCED_BREP_SHAPE_REPRESENTATION ( 'ISO 10513 M8 Lock Nut', ( #4462, #20860 ), #17833 ) ;
#12441 = CARTESIAN_POINT ( 'NONE',  ( 0.9412147342319837628, 0.1574803149606300301, 0.5290354330708663122 ) ) ;
#12442 = FACE_OUTER_BOUND ( 'NONE', #38742, .T. ) ;
#12443 = CARTESIAN_POINT ( 'NONE',  ( -0.9873396505805591694, 0.1113553986120547346, 1.186023621939716666 ) ) ;
#12444 = CARTESIAN_POINT ( 'NONE',  ( 1.002407869896990045, 0.1264236179284866091, 0.5437992125446614589 ) ) ;
#12445 = CYLINDRICAL_SURFACE ( 'NONE', #19300, 0.1377952755905510751 ) ;
#12447 = CARTESIAN_POINT ( 'NONE',  ( -0.7185039370078739607, 1.928577636452523993E-17, 1.633858267609007875 ) ) ;
#12446 = CARTESIAN_POINT ( 'NONE',  ( 0.06523048226347956391, -0.4483267716535432879, 0.1574803149606297803 ) ) ;
#12448 = CIRCLE ( 'NONE', #32360, 0.1864803149606299448 ) ;
#12449 = VECTOR ( 'NONE', #39580, 39.37007874015748143 ) ;
#12450 = FACE_OUTER_BOUND ( 'NONE', #8035, .T. ) ;
#12451 = EDGE_LOOP ( 'NONE', ( #7601, #11068, #28752, #2715 ) ) ;
#12452 = DIRECTION ( 'NONE',  ( -0.5735764363510331698, 0.6455006197386586875, -0.5043203561029997450 ) ) ;
#12453 = CARTESIAN_POINT ( 'NONE',  ( -0.8019270111902716547, -0.1787899950787401604, 1.077755905458048113 ) ) ;
#12454 = CARTESIAN_POINT ( 'NONE',  ( 1.033464566929134687, -0.06523048226347956391, 1.149114173228346969 ) ) ;
#12455 = CARTESIAN_POINT ( 'NONE',  ( -0.9287573551135129835, -0.1680815725407091843, 1.989135227375367743 ) ) ;
#12456 = FACE_OUTER_BOUND ( 'NONE', #25051, .T. ) ;
#12457 = EDGE_CURVE ( 'NONE', #6796, #39036, #41918, .T. ) ;
#12459 = CARTESIAN_POINT ( 'NONE',  ( -0.3161444924769509779, 1.690605217543008632, -0.5092277576975117181 ) ) ;
#12458 = CARTESIAN_POINT ( 'NONE',  ( 0.9412147342319837628, 0.1574803149606300301, 0.1747047244094490082 ) ) ;
#12460 = CARTESIAN_POINT ( 'NONE',  ( -0.7185039370078746268, -0.06523048226347956391, 1.252460629921259061 ) ) ;
#12461 = CARTESIAN_POINT ( 'NONE',  ( -0.1065407853927636261, -0.08956136429197258941, 0.1197608106671575745 ) ) ;
#12462 = CARTESIAN_POINT ( 'NONE',  ( -0.1787899950787401604, -0.5147637794737950356, -0.07405724077823318263 ) ) ;
#12463 = EDGE_LOOP ( 'NONE', ( #9289, #39728 ) ) ;
#12464 = CARTESIAN_POINT ( 'NONE',  ( 0.9412147342319837628, -0.1574803149606297803, 0.8686023622047237547 ) ) ;
#12465 = ORIENTED_EDGE ( 'NONE', *, *, #31141, .T. ) ;
#12466 = CARTESIAN_POINT ( 'NONE',  ( 1.033464566929134687, 0.06523048226347956391, 1.272145669291338432 ) ) ;
#12467 = LINE ( 'NONE', #8843, #14331 ) ;
#12468 = CARTESIAN_POINT ( 'NONE',  ( -0.1787899950787401882, -1.772145669237574994, 0.000000000000000000 ) ) ;
#12469 = CARTESIAN_POINT ( 'NONE',  ( -1.094772975963752103E-17, -0.9601377952218268508, -0.1787899950787401882 ) ) ;
#12470 = CARTESIAN_POINT ( 'NONE',  ( -0.1574803149606297803, -1.363681102362204856, 0.06523048226347956391 ) ) ;
#12471 = CARTESIAN_POINT ( 'NONE',  ( 0.7185039370078746268, -0.06523048226347956391, 1.124507873908221489 ) ) ;
#12472 = DIRECTION ( 'NONE',  ( 1.000000000000000000, 0.000000000000000000, 0.000000000000000000 ) ) ;
#12473 = ORIENTED_EDGE ( 'NONE', *, *, #24133, .F. ) ;
#12474 = VERTEX_POINT ( 'NONE', #947 ) ;
#12475 = CARTESIAN_POINT ( 'NONE',  ( -1.054774247047244540, 0.07405724077823318263, 1.801181102308441861 ) ) ;
#12476 = CARTESIAN_POINT ( 'NONE',  ( 0.7495606340400177148, 0.1264236179284866091, 1.852854330654897685 ) ) ;
#12477 = VERTEX_POINT ( 'NONE', #30244 ) ;
#12478 = CARTESIAN_POINT ( 'NONE',  ( -0.1113553986120547346, -1.351377952648377789, 0.1113553986120547346 ) ) ;
#12479 = CARTESIAN_POINT ( 'NONE',  ( 0.1574803149606299191, -0.5708661417322835607, -6.991093932140394160E-17 ) ) ;
#12480 = CARTESIAN_POINT ( 'NONE',  ( 0.8019270111902717657, 0.1787899950787401604, 0.4724409448281262636 ) ) ;
#12481 = CARTESIAN_POINT ( 'NONE',  ( -0.7495606340400177148, 0.1264236179284866091, 1.454232283410803017 ) ) ;
#12482 = CARTESIAN_POINT ( 'NONE',  ( 0.04256392708710985545, 0.2709142457700762230, -0.3044102143378303871 ) ) ;
#12483 = CARTESIAN_POINT ( 'NONE',  ( -0.9500414927467378812, -0.1787899950787401604, 0.09842519679663024046 ) ) ;
#12484 = TOROIDAL_SURFACE ( 'NONE', #34667, 0.7972440944881888925, 0.009842519685039369942 ) ;
#12485 = EDGE_CURVE ( 'NONE', #44026, #2780, #32878, .T. ) ;
#12486 = CARTESIAN_POINT ( 'NONE',  ( -1.033464566929134687, 0.06523048226347956391, 0.5634842519685042683 ) ) ;
#12487 = CARTESIAN_POINT ( 'NONE',  ( -0.7495606340400177148, -0.1264236179284866091, 1.783956692859621995 ) ) ;
#12488 = CARTESIAN_POINT ( 'NONE',  ( -0.6971942568897637749, 2.189545951927499583E-17, 0.1254921259304885850 ) ) ;
#12489 = CARTESIAN_POINT ( 'NONE',  ( -0.7646288533564489232, -0.1113553986120547346, 1.687992125984252079 ) ) ;
#12490 = DIRECTION ( 'NONE',  ( 1.000000000000000000, 0.000000000000000000, 0.000000000000000000 ) ) ;
#12491 = CARTESIAN_POINT ( 'NONE',  ( 0.9500414927467377701, 0.1787899950787401604, 1.648622047190331230 ) ) ;
#12492 = CARTESIAN_POINT ( 'NONE',  ( -0.1189708289958600340, -0.09851383554566003897, 0.1141074950210181072 ) ) ;
#12493 = CARTESIAN_POINT ( 'NONE',  ( 0.9412147342319837628, 0.1574803149606300301, 0.2042322833570397733 ) ) ;
#12494 = VECTOR ( 'NONE', #36258, 39.37007874015748854 ) ;
#12495 = ADVANCED_FACE ( 'NONE', ( #43863 ), #27116, .T. ) ;
#12496 = ORIENTED_EDGE ( 'NONE', *, *, #6873, .T. ) ;
#12497 = CIRCLE ( 'NONE', #46116, 0.09842519685039370636 ) ;
#12498 = EDGE_LOOP ( 'NONE', ( #14816, #12601, #30015, #22010 ) ) ;
#12499 = CARTESIAN_POINT ( 'NONE',  ( 0.1264236179284866091, -0.9749015747493857686, 0.1264236179284866091 ) ) ;
#12500 = CARTESIAN_POINT ( 'NONE',  ( 0.07405724077823318263, -1.075787401521038689, -0.1787899950787401604 ) ) ;
#12501 = FACE_OUTER_BOUND ( 'NONE', #9869, .T. ) ;
#12502 = ( NAMED_UNIT ( * ) SI_UNIT ( $, .STERADIAN. ) SOLID_ANGLE_UNIT ( ) ) ;
#12503 = CARTESIAN_POINT ( 'NONE',  ( 0.7495606340400177148, 0.1264236179284866091, 0.3912401574265515491 ) ) ;
#12504 = CARTESIAN_POINT ( 'NONE',  ( -0.07444174185955065859, -0.4021107387169037817, -0.1797182628040039087 ) ) ;
#12505 = CARTESIAN_POINT ( 'NONE',  ( -0.7185039370078746268, -0.06523048226347956391, 0.7701771652468031304 ) ) ;
#12506 = CARTESIAN_POINT ( 'NONE',  ( -0.1574803149606299191, 0.01181102362204724393, 0.000000000000000000 ) ) ;
#12507 = DIRECTION ( 'NONE',  ( 0.000000000000000000, 0.7071067811867007835, 0.7071067811863941399 ) ) ;
#12508 = CARTESIAN_POINT ( 'NONE',  ( 0.6971942568897626646, 0.07405724077823318263, 0.8661417322297003674 ) ) ;
#12509 = CIRCLE ( 'NONE', #46925, 0.2471922904502826812 ) ;
#12511 = DIRECTION ( 'NONE',  ( 0.000000000000000000, 0.000000000000000000, 1.000000000000000000 ) ) ;
#12510 = SURFACE_SIDE_STYLE ('',( #34082 ) ) ;
#12512 = CARTESIAN_POINT ( 'NONE',  ( -1.033464566929134687, -0.06523048226347956391, 0.07627952745152805081 ) ) ;
#12513 = CARTESIAN_POINT ( 'NONE',  ( 1.054774247047244096, 0.000000000000000000, 1.916830708607653477 ) ) ;
#12514 = PRODUCT_DEFINITION_FORMATION_WITH_SPECIFIED_SOURCE ( 'ANY', '', #5156, .NOT_KNOWN. ) ;
#12515 = CONICAL_SURFACE ( 'NONE', #7120, 0.1377952755905511861, 1.047197551196598297 ) ;
#12516 = CARTESIAN_POINT ( 'NONE',  ( 1.033464566929134687, 0.06523048226347956391, 0.2091535433070865757 ) ) ;
#12517 = FACE_OUTER_BOUND ( 'NONE', #27166, .T. ) ;
#12518 = CARTESIAN_POINT ( 'NONE',  ( -1.094772975963752103E-17, -0.4483267715997795166, -0.1787899950787401882 ) ) ;
#12519 = CARTESIAN_POINT ( 'NONE',  ( 0.5785143135414534399, 0.6588822455111159604, 0.2968425708877995284 ) ) ;
#12520 = CARTESIAN_POINT ( 'NONE',  ( -0.1264236179284866091, -1.255413385773007873, 0.1264236179284866091 ) ) ;
#12521 = CIRCLE ( 'NONE', #1089, 0.09842519685039317900 ) ;
#12522 = CARTESIAN_POINT ( 'NONE',  ( 0.4620708661417338714, 0.4133858267716533641, 1.186023622047243986 ) ) ;
#12523 = CARTESIAN_POINT ( 'NONE',  ( -1.054774247047244540, 0.07405724077823318263, 1.756889763725764553 ) ) ;
#12524 = VERTEX_POINT ( 'NONE', #8383 ) ;
#12525 = CARTESIAN_POINT ( 'NONE',  ( -0.7495606340400177148, -0.1264236179284866091, 1.272145669237574772 ) ) ;
#12526 = CYLINDRICAL_SURFACE ( 'NONE', #61, 0.1574803149606299191 ) ;
#12527 = EDGE_CURVE ( 'NONE', #35936, #27975, #5506, .T. ) ;
#12528 = CARTESIAN_POINT ( 'NONE',  ( 0.9500414927467378812, 0.1787899950787401604, 1.373031496009229135 ) ) ;
#12529 = CARTESIAN_POINT ( 'NONE',  ( -0.8759842519685039353, -0.1787899950787401882, 0.5684055117572598403 ) ) ;
#12530 = CARTESIAN_POINT ( 'NONE',  ( -0.8759842519685039353, -0.1787899950787401882, 1.154035433017102319 ) ) ;
#12531 = FACE_OUTER_BOUND ( 'NONE', #27623, .T. ) ;
#12532 = CARTESIAN_POINT ( 'NONE',  ( -0.1480151140659365927, -0.09843327264853890535, -0.1007363786963137303 ) ) ;
#12533 = CARTESIAN_POINT ( 'NONE',  ( -0.2066929133858267931, -0.5175744617845221551, -0.9076376772307637175 ) ) ;
#12534 = CARTESIAN_POINT ( 'NONE',  ( 1.002407869896990045, 0.1264236179284866091, 0.5437992125446614589 ) ) ;
#12535 = CARTESIAN_POINT ( 'NONE',  ( -1.002407869896990045, 0.1264236179284866091, 0.3420275590013546751 ) ) ;
#12536 = CARTESIAN_POINT ( 'NONE',  ( -0.6971942568897626646, 0.07405724077823318263, 0.8267716534895444003 ) ) ;
#12537 = DIRECTION ( 'NONE',  ( 1.000000000000000000, 0.000000000000000000, 0.000000000000000000 ) ) ;
#12538 = EDGE_LOOP ( 'NONE', ( #42275, #17973, #13010, #43115 ) ) ;
#12539 = CARTESIAN_POINT ( 'NONE',  ( -0.9412147342319837628, -0.1574803149606297803, 0.3567913385826772532 ) ) ;
#12540 = CARTESIAN_POINT ( 'NONE',  ( 0.8759842519685039353, 0.1787899950787401882, 1.139271653489543290 ) ) ;
#12541 = CARTESIAN_POINT ( 'NONE',  ( -0.1476377952755905387, 0.2512968553230415791, -0.3092734567177705673 ) ) ;
#12542 = CARTESIAN_POINT ( 'NONE',  ( -1.033464566929133799, 1.928577636452524610E-17, 2.869337061179095023E-17 ) ) ;
#12543 = ORIENTED_EDGE ( 'NONE', *, *, #43810, .T. ) ;
#12544 = CARTESIAN_POINT ( 'NONE',  ( -1.054774247047244540, -0.07405724077823318263, 0.9694881889226144578 ) ) ;
#12545 = DIRECTION ( 'NONE',  ( 1.000000000000000000, 0.000000000000000000, 0.000000000000000000 ) ) ;
#12546 = DIRECTION ( 'NONE',  ( 1.000000000000000000, 6.679788269418529283E-17, 0.000000000000000000 ) ) ;
#12547 = CARTESIAN_POINT ( 'NONE',  ( 0.1264236179284866091, -1.645301133583568998, -0.1264236179284866091 ) ) ;
#12548 = ORIENTED_EDGE ( 'NONE', *, *, #7709, .T. ) ;
#12549 = DIRECTION ( 'NONE',  ( -1.000000000000000000, 0.000000000000000000, 0.000000000000000000 ) ) ;
#12550 = CARTESIAN_POINT ( 'NONE',  ( 0.1787899950787401604, -0.4507874015210400209, -0.07405724077823318263 ) ) ;
#12551 = DIRECTION ( 'NONE',  ( -1.000000000000000000, 0.000000000000000000, 0.000000000000000000 ) ) ;
#12552 = B_SPLINE_CURVE_WITH_KNOTS ( 'NONE', 3,
 ( #6604, #27973, #28932, #43495, #6361, #46855, #6834, #9745, #20975, #2297, #39426, #2764, #35623, #42761, #13800, #2997, #32028, #43009, #20747, #10218 ),
 .UNSPECIFIED., .F., .F.,
 ( 4, 1, 1, 1, 1, 1, 2, 2, 1, 1, 1, 2, 2, 4 ),
 ( 0.000000000000000000, 0.2499999999999903411, 0.3749999999999857891, 0.4374999999999835132, 0.4687499999999825695, 0.4843749999999820699, 0.4921874999999819034, 0.4999999999999817923, 0.6249999999999863443, 0.6874999999999884537, 0.7187499999999895639, 0.7343749999999904521, 0.7499999999999914513, 1.000000000000000000 ),
 .UNSPECIFIED. ) ;
#12553 = DIRECTION ( 'NONE',  ( 0.000000000000000000, 1.000000000000000000, 0.000000000000000000 ) ) ;
#12554 = DIRECTION ( 'NONE',  ( 1.000000000000000000, 0.000000000000000000, -1.822029033848725275E-16 ) ) ;
#12555 = CARTESIAN_POINT ( 'NONE',  ( 0.5538057742782149795, -0.08090551181102362266, 0.000000000000000000 ) ) ;
#12556 = CARTESIAN_POINT ( 'NONE',  ( -0.1787899950787401882, -1.737696850339937038, 0.000000000000000000 ) ) ;
#12557 = SHAPE_DEFINITION_REPRESENTATION ( #40586, #9335 ) ;
#12558 = CARTESIAN_POINT ( 'NONE',  ( 0.1377952755905512139, 0.1574803149606299191, -0.9084645669291339098 ) ) ;
#12559 = CARTESIAN_POINT ( 'NONE',  ( 1.054774247047244540, 0.07405724077823318263, 0.5364173227808821665 ) ) ;
#12560 = ( BOUNDED_SURFACE ( )  B_SPLINE_SURFACE ( 3, 2, ( 
 ( #15159, #21628, #36262 ),
 ( #18497, #32675, #21382 ),
 ( #29, #40285, #29353 ),
 ( #43895, #25716, #29803 ),
 ( #7470, #22090, #44350 ),
 ( #33154, #14919, #38129 ) ),
 .UNSPECIFIED., .F., .F., .F. ) 
 B_SPLINE_SURFACE_WITH_KNOTS ( ( 4, 2, 4 ),
 ( 3, 3 ),
 ( 0.01651999345535504898, 0.01858032176739835006, 0.02064065007944164767 ),
 ( 0.000000000000000000, 1.000000000000000000 ),
 .UNSPECIFIED. ) 
 GEOMETRIC_REPRESENTATION_ITEM ( )  RATIONAL_B_SPLINE_SURFACE ( (
 ( 1.000000000000000000, 0.8047781103519390244, 1.000000000000000000),
 ( 1.000000000000000000, 0.8123785825609630695, 1.000000000000000000),
 ( 1.000000000000000000, 0.8190671539781260169, 1.000000000000000000),
 ( 1.000000000000000000, 0.8192352254841890336, 1.000000000000000000),
 ( 1.000000000000000000, 0.8126129677206329616, 1.000000000000000000),
 ( 1.000000000000000000, 0.8047712537969730073, 1.000000000000000000) ) ) 
 REPRESENTATION_ITEM ( '' )  SURFACE ( )  ) ;
#12561 = CARTESIAN_POINT ( 'NONE',  ( -1.054774247047244540, -0.07405724077823318263, 0.6545275590013546196 ) ) ;
#12563 = DIRECTION ( 'NONE',  ( -1.000000000000000000, 0.000000000000000000, 0.000000000000000000 ) ) ;
#12562 = CARTESIAN_POINT ( 'NONE',  ( -0.06523048226347956391, -0.7829724409448810540, -0.1574803149606300301 ) ) ;
#12564 = CARTESIAN_POINT ( 'NONE',  ( 0.1270800023317771588, -1.551224911945249918, -0.1270800023317771588 ) ) ;
#12565 = DIRECTION ( 'NONE',  ( 0.000000000000000000, 1.000000000000000000, 2.891205793294680298E-16 ) ) ;
#12566 = LINE ( 'NONE', #15445, #23059 ) ;
#12567 = CARTESIAN_POINT ( 'NONE',  ( 1.054774247047244540, -0.07405724077823318263, 1.560039370024977057 ) ) ;
#12568 = CARTESIAN_POINT ( 'NONE',  ( 1.002407869896990045, -0.1264236179284866091, 1.788877952702141672 ) ) ;
#12569 = ORIENTED_EDGE ( 'NONE', *, *, #3461, .T. ) ;
#12572 = ORIENTED_EDGE ( 'NONE', *, *, #16561, .T. ) ;
#12571 = EDGE_CURVE ( 'NONE', #13201, #35449, #6392, .T. ) ;
#12570 = DIRECTION ( 'NONE',  ( 0.000000000000000000, 1.000000000000000000, 0.000000000000000000 ) ) ;
#12573 = LINE ( 'NONE', #9441, #6697 ) ;
#12574 = DIRECTION ( 'NONE',  ( -1.000000000000000000, 0.000000000000000000, 0.000000000000000000 ) ) ;
#12575 = CARTESIAN_POINT ( 'NONE',  ( -0.1787899950787401604, 0.03149606304588949135, -0.07405724077823318263 ) ) ;
#12576 = CARTESIAN_POINT ( 'NONE',  ( -0.8759842519685039353, 0.1574803149606299191, 0.1771653543307086520 ) ) ;
#12577 = CARTESIAN_POINT ( 'NONE',  ( 0.6971942568897626646, 0.07405724077823318263, 0.4330708660879683536 ) ) ;
#12578 = ADVANCED_FACE ( 'NONE', ( #38333 ), #32812, .T. ) ;
#12579 = CARTESIAN_POINT ( 'NONE',  ( 0.7654444006328559036, -0.1232301103881700693, 0.03937007855823598801 ) ) ;
#12580 = CARTESIAN_POINT ( 'NONE',  ( 0.8107537697050254399, -0.1574803149606297803, 1.956200787294048338 ) ) ;
#12581 = CARTESIAN_POINT ( 'NONE',  ( -0.7185039370078739607, 1.928577636452523993E-17, 1.318897637687747926 ) ) ;
#12582 = DIRECTION ( 'NONE',  ( 0.000000000000000000, 0.000000000000000000, -1.000000000000000000 ) ) ;
#12583 = CARTESIAN_POINT ( 'NONE',  ( -1.054774247047244096, 0.000000000000000000, 1.360728346402929168 ) ) ;
#12584 = CARTESIAN_POINT ( 'NONE',  ( 0.9412147342319837628, -0.1574803149606297803, 0.8193897636719996713 ) ) ;
#12585 = VERTEX_POINT ( 'NONE', #23013 ) ;
#12586 = EDGE_CURVE ( 'NONE', #38550, #9701, #23971, .T. ) ;
#12587 = CARTESIAN_POINT ( 'NONE',  ( 0.8759842519685039353, 0.1787899950787401882, 1.060531496009228247 ) ) ;
#12588 = ORIENTED_EDGE ( 'NONE', *, *, #3411, .F. ) ;
#12589 = AXIS2_PLACEMENT_3D ( 'NONE', #5459, #16498, #15801 ) ;
#12591 = CARTESIAN_POINT ( 'NONE',  ( -0.1264236179284866091, -1.388287401521039355, -0.1264236179284866091 ) ) ;
#12590 = CARTESIAN_POINT ( 'NONE',  ( 0.1574803149606300301, -1.097933070758615903, -0.06523048226347956391 ) ) ;
#12592 = CARTESIAN_POINT ( 'NONE',  ( -0.9873396505805591694, 0.1113553986120547346, 0.5561023620971968784 ) ) ;
#12593 = DIRECTION ( 'NONE',  ( -3.469446951953608272E-15, -1.000000000000000000, 0.000000000000000000 ) ) ;
#12594 = CARTESIAN_POINT ( 'NONE',  ( -0.9873396505805591694, -0.1113553986120547346, 1.225393700787401619 ) ) ;
#12595 = CARTESIAN_POINT ( 'NONE',  ( 0.7185039370078739607, 1.928577636452523993E-17, 0.2559055117034968463 ) ) ;
#12597 = CARTESIAN_POINT ( 'NONE',  ( -0.9873396505805591694, 0.1113553986120547346, 0.7529527557979842634 ) ) ;
#12596 = CARTESIAN_POINT ( 'NONE',  ( -9.642888182262618425E-18, 0.04133858267716535029, -0.1574803149606299191 ) ) ;
#12598 = CARTESIAN_POINT ( 'NONE',  ( -0.3161444924769509779, 1.209494567139727250, -1.479906699140296045 ) ) ;
#12599 = CARTESIAN_POINT ( 'NONE',  ( 0.8759842519685039353, -0.1574803149606299191, 1.407480314853102321 ) ) ;
#12600 = EDGE_LOOP ( 'NONE', ( #35339, #13655, #8417, #36103 ) ) ;
#12601 = ORIENTED_EDGE ( 'NONE', *, *, #21771, .T. ) ;
#12602 = ( BOUNDED_CURVE ( )  B_SPLINE_CURVE ( 2, ( #47344, #3235, #355, #3947, #29182, #46849, #29657, #39893, #14753 ),
 .UNSPECIFIED., .F., .F. ) 
 B_SPLINE_CURVE_WITH_KNOTS ( ( 3, 2, 2, 2, 3 ),
 ( 0.5899999999999999689, 0.5925000000000000266, 0.5949999999999999734, 0.5975000000000000311, 0.5999999999999999778 ),
 .UNSPECIFIED. ) 
 CURVE ( )  GEOMETRIC_REPRESENTATION_ITEM ( )  RATIONAL_B_SPLINE_CURVE ( ( 1.000000000000000000, 0.9238795325112869605, 1.000000000000000000, 0.9238795325112869605, 1.000000000000000000, 0.9238795325112869605, 1.000000000000000000, 0.9238795325112869605, 1.000000000000000000 ) ) 
 REPRESENTATION_ITEM ( '' )  ) ;
#12603 = CARTESIAN_POINT ( 'NONE',  ( -0.1036066153428575193, -0.09660391682274853398, -0.2256134787374337036 ) ) ;
#12604 = STYLED_ITEM ( 'NONE', ( #18193 ), #4880 ) ;
#12605 = CARTESIAN_POINT ( 'NONE',  ( -0.9500414927467377701, 0.1787899950787401604, 1.564960629867495845 ) ) ;
#12606 = CARTESIAN_POINT ( 'NONE',  ( -0.1574803149606299191, -0.01771653532554381960, 0.000000000000000000 ) ) ;
#12607 = CARTESIAN_POINT ( 'NONE',  ( -1.054774247047244096, 0.000000000000000000, 1.405019684985606476 ) ) ;
#12608 = DIRECTION ( 'NONE',  ( -1.000000000000000000, 0.000000000000000000, 0.000000000000000000 ) ) ;
#12609 = DIRECTION ( 'NONE',  ( -1.000000000000000000, 0.000000000000000000, 0.000000000000000000 ) ) ;
#12610 = CARTESIAN_POINT ( 'NONE',  ( 0.07405724077823318263, -1.052289322559947449, -0.1787899950787401604 ) ) ;
#12611 = EDGE_LOOP ( 'NONE', ( #10076, #34340, #17706, #21844, #24523 ) ) ;
#12612 = CARTESIAN_POINT ( 'NONE',  ( 0.1787899950787401604, 0.05610236225848785896, 0.07405724077823318263 ) ) ;
#12613 = ORIENTED_EDGE ( 'NONE', *, *, #6260, .T. ) ;
#12614 = ORIENTED_EDGE ( 'NONE', *, *, #31630, .F. ) ;
#12615 = CARTESIAN_POINT ( 'NONE',  ( 0.7185039370078739607, 0.000000000000000000, 4.498031496062992574 ) ) ;
#12616 = DIRECTION ( 'NONE',  ( 0.000000000000000000, 1.000000000000000000, 0.000000000000000000 ) ) ;
#12617 = CARTESIAN_POINT ( 'NONE',  ( 0.9873396505805591694, 0.1113553986120547346, 1.786417322834645605 ) ) ;
#12618 = AXIS2_PLACEMENT_3D ( 'NONE', #21962, #14780, #32299 ) ;
#12619 = AXIS2_PLACEMENT_3D ( 'NONE', #19547, #37276, #26047 ) ;
#12620 = AXIS2_PLACEMENT_3D ( 'NONE', #45352, #23568, #41497 ) ;
#12621 = CARTESIAN_POINT ( 'NONE',  ( 0.07405724077823318263, -0.6624015747493856576, 0.1787899950787401604 ) ) ;
#12622 = CARTESIAN_POINT ( 'NONE',  ( -0.8019270111902716547, 0.1787899950787401604, 0.2362204723871814682 ) ) ;
#12623 = CARTESIAN_POINT ( 'NONE',  ( -0.8107537697050253289, 0.1574803149606300301, 1.045767716535432879 ) ) ;
#12624 = CARTESIAN_POINT ( 'NONE',  ( 0.1797182628040039087, -1.164906014307455884, 0.07444174185955046430 ) ) ;
#12625 = CARTESIAN_POINT ( 'NONE',  ( 0.1690594283350484173, 0.1299212598425197318, -0.03640762741699016952 ) ) ;
#12626 = CARTESIAN_POINT ( 'NONE',  ( 0.8019270111902717657, 0.1787899950787401604, 1.141732283410804349 ) ) ;
#12628 = ADVANCED_FACE ( 'NONE', ( #1189 ), #45269, .T. ) ;
#12627 = DIRECTION ( 'NONE',  ( 0.000000000000000000, -1.000000000000000000, 0.000000000000000000 ) ) ;
#12629 = CARTESIAN_POINT ( 'NONE',  ( 0.9412147342319837628, 0.1574803149606300301, 1.592027559055119390 ) ) ;
#12631 = CARTESIAN_POINT ( 'NONE',  ( -0.1496320939564846353, -0.2091027599427721095, -0.3142669362052405435 ) ) ;
#12630 = CARTESIAN_POINT ( 'NONE',  ( 0.7609548656500562114, 0.1137474223536875800, 1.980823507184093391 ) ) ;
#12632 = DIRECTION ( 'NONE',  ( 0.000000000000000000, 0.000000000000000000, -1.000000000000000000 ) ) ;
#12633 = CARTESIAN_POINT ( 'NONE',  ( -0.9873396505805591694, -0.1113553986120547346, 1.609251968396409493 ) ) ;
#12634 = EDGE_CURVE ( 'NONE', #15333, #43692, #15848, .T. ) ;
#12635 = DIRECTION ( 'NONE',  ( 0.000000000000000000, -0.2432573283306646017, 0.9699617890481188054 ) ) ;
#12636 = CARTESIAN_POINT ( 'NONE',  ( 0.7495606340400177148, -0.1264236179284866091, 0.9522637794737952577 ) ) ;
#12637 = CARTESIAN_POINT ( 'NONE',  ( 1.054774247047244540, 0.07405724077823318263, 1.840551181048599938 ) ) ;
#12638 = CARTESIAN_POINT ( 'NONE',  ( 1.033464566929134687, -0.06523048226347956391, 0.2731299211523157133 ) ) ;
#12639 = ORIENTED_EDGE ( 'NONE', *, *, #17859, .F. ) ;
#12640 = CARTESIAN_POINT ( 'NONE',  ( 0.9873396505805591694, -0.1113553986120547346, 1.254921259734991912 ) ) ;
#12641 = EDGE_CURVE ( 'NONE', #6061, #12053, #23501, .T. ) ;
#12642 = CARTESIAN_POINT ( 'NONE',  ( 0.1574803149606300301, -1.732775590443652591, 0.06523048226347956391 ) ) ;
#12643 = CARTESIAN_POINT ( 'NONE',  ( -0.7185039370078739607, 1.928577636452523993E-17, 0.2559055117034968463 ) ) ;
#12644 = CARTESIAN_POINT ( 'NONE',  ( 0.01230737760510409486, -0.1591122789105269553, -1.990515434288500257E-18 ) ) ;
#12645 = CARTESIAN_POINT ( 'NONE',  ( 1.054774247047244096, 0.000000000000000000, 1.281988188922614125 ) ) ;
#12646 = EDGE_CURVE ( 'NONE', #29582, #15059, #17486, .T. ) ;
#12647 = FACE_OUTER_BOUND ( 'NONE', #20908, .T. ) ;
#12648 = CARTESIAN_POINT ( 'NONE',  ( -0.1787899950787401604, 0.1200787402112438867, 0.07405724077823318263 ) ) ;
#12649 = DIRECTION ( 'NONE',  ( 1.000000000000000000, 0.000000000000000000, -1.822029033848725275E-16 ) ) ;
#12650 = CIRCLE ( 'NONE', #41782, 0.09842519685039370636 ) ;
#12651 = VECTOR ( 'NONE', #16760, 39.37007874015748143 ) ;
#12652 = CARTESIAN_POINT ( 'NONE',  ( -0.009906661468957165401, 0.04209688371799823886, 0.2797134572002688002 ) ) ;
#12653 = ORIENTED_EDGE ( 'NONE', *, *, #35124, .F. ) ;
#12654 = EDGE_LOOP ( 'NONE', ( #7337, #32767, #13334, #30925 ) ) ;
#12655 = CARTESIAN_POINT ( 'NONE',  ( -0.1787899950787401882, -1.540846456639149542, 0.000000000000000000 ) ) ;
#12656 = CARTESIAN_POINT ( 'NONE',  ( -0.6971942568897637749, 2.189545951927499583E-17, 0.9916338582139527791 ) ) ;
#12657 = VECTOR ( 'NONE', #5200, 39.37007874015748143 ) ;
#12658 = VECTOR ( 'NONE', #45025, 39.37007874015748143 ) ;
#12659 = CARTESIAN_POINT ( 'NONE',  ( -0.9500414927467378812, 0.1787899950787401604, 1.840551181048599938 ) ) ;
#12660 = ORIENTED_EDGE ( 'NONE', *, *, #33754, .T. ) ;
#12661 = CARTESIAN_POINT ( 'NONE',  ( -0.8759842519685039353, 0.1787899950787401882, 0.7062007873478109987 ) ) ;
#12662 = ORIENTED_EDGE ( 'NONE', *, *, #47026, .T. ) ;
#12663 = LINE ( 'NONE', #16249, #6912 ) ;
#12664 = DIRECTION ( 'NONE',  ( -1.000000000000000000, 3.469446951953613794E-15, 1.144917494144692682E-16 ) ) ;
#12665 = CARTESIAN_POINT ( 'NONE',  ( 0.1264236179284866091, -0.5527814485441993053, 0.1264236179284866091 ) ) ;
#12666 = CARTESIAN_POINT ( 'NONE',  ( -0.03915270915796512097, -0.08956085038011968313, -0.1800528347341008029 ) ) ;
#12667 = CARTESIAN_POINT ( 'NONE',  ( 0.9873396505805591694, -0.1113553986120547346, 0.4773622047244094890 ) ) ;
#12668 = CARTESIAN_POINT ( 'NONE',  ( -0.7495606340400177148, 0.1264236179284866091, 0.4306102361667086820 ) ) ;
#12669 = DIRECTION ( 'NONE',  ( 0.000000000000000000, 0.000000000000000000, -1.000000000000000000 ) ) ;
#12670 = ORIENTED_EDGE ( 'NONE', *, *, #36261, .F. ) ;
#12671 = DIRECTION ( 'NONE',  ( -0.000000000000000000, -0.000000000000000000, -1.000000000000000000 ) ) ;
#12672 = CARTESIAN_POINT ( 'NONE',  ( -0.7495606340400177148, -0.1264236179284866091, 1.508366141678519678 ) ) ;
#12673 = CIRCLE ( 'NONE', #2676, 0.1003937007874011050 ) ;
#12674 = CARTESIAN_POINT ( 'NONE',  ( 0.07405724077823318263, -1.449803149552535642, 0.1787899950787401604 ) ) ;
#12675 = CARTESIAN_POINT ( 'NONE',  ( -0.2066929133858267931, 0.7443365962042343131, -3.523993443072799270 ) ) ;
#12676 = CARTESIAN_POINT ( 'NONE',  ( 0.8759842519685039353, 0.1574803149606299191, 1.033464566821606478 ) ) ;
#12677 = CARTESIAN_POINT ( 'NONE',  ( 0.1642909303726545756, -0.08091908006343519200, 0.1401559281493469367 ) ) ;
#12679 = CARTESIAN_POINT ( 'NONE',  ( 0.07444174185955065859, -0.6580162505279267826, 0.1797182628040039087 ) ) ;
#12678 = CIRCLE ( 'NONE', #395, 0.1864803149606299171 ) ;
#12680 = AXIS2_PLACEMENT_3D ( 'NONE', #15297, #34001, #22954 ) ;
#12681 = CARTESIAN_POINT ( 'NONE',  ( 0.8107537697050254399, -0.1574803149606297803, 0.9424212598425207865 ) ) ;
#12682 = CARTESIAN_POINT ( 'NONE',  ( -0.9412147342319837628, 0.1574803149606300301, 1.188484251860977503 ) ) ;
#12683 = EDGE_CURVE ( 'NONE', #44801, #26576, #20119, .T. ) ;
#12684 = CARTESIAN_POINT ( 'NONE',  ( 0.8759842519685039353, -0.1787899950787401882, 0.6077755904974173617 ) ) ;
#12685 = CARTESIAN_POINT ( 'NONE',  ( 1.054774247047244540, -0.07405724077823318263, 0.05905511805647267048 ) ) ;
#12687 = CARTESIAN_POINT ( 'NONE',  ( -0.7646288533564489232, 0.1113553986120547346, 1.628937007766488199 ) ) ;
#12686 = CARTESIAN_POINT ( 'NONE',  ( -0.06523048226347956391, -0.4532480314960634082, 0.1574803149606297803 ) ) ;
#12688 = VECTOR ( 'NONE', #16262, 39.37007874015748143 ) ;
#12689 = AXIS2_PLACEMENT_3D ( 'NONE', #31521, #9227, #12608 ) ;
#12690 = DIRECTION ( 'NONE',  ( -1.000000000000000000, 0.000000000000000000, 0.000000000000000000 ) ) ;
#12691 = ORIENTED_EDGE ( 'NONE', *, *, #7315, .F. ) ;
#12692 = CARTESIAN_POINT ( 'NONE',  ( 1.033464566929133799, 0.000000000000000000, 1.574803149498771537 ) ) ;
#12693 = CARTESIAN_POINT ( 'NONE',  ( 0.9873396505805591694, 0.1113553986120547346, 1.077755905511811108 ) ) ;
#12694 = DIRECTION ( 'NONE',  ( 1.000000000000000000, -3.368395098984144529E-15, 0.000000000000000000 ) ) ;
#12695 = CARTESIAN_POINT ( 'NONE',  ( 0.6195511811023624027, 0.9842519685039370358, -0.5511811023622036343 ) ) ;
#12696 = ADVANCED_FACE ( 'NONE', ( #12242 ), #16767, .T. ) ;
#12698 = CARTESIAN_POINT ( 'NONE',  ( 0.7185039370078739607, 1.928577636452523993E-17, 1.673228346349165285 ) ) ;
#12697 = DIRECTION ( 'NONE',  ( -1.000000000000000000, 3.469446951953614189E-15, 1.144917494144692682E-16 ) ) ;
#12699 = CARTESIAN_POINT ( 'NONE',  ( 0.7185039370078746268, 0.06523048226347956391, 0.6077755904436539236 ) ) ;
#12700 = CARTESIAN_POINT ( 'NONE',  ( 0.1264236179284866091, -0.4975393700249764461, 0.1264236179284866091 ) ) ;
#12701 = CYLINDRICAL_SURFACE ( 'NONE', #39155, 0.4724409448818896462 ) ;
#12702 = VERTEX_POINT ( 'NONE', #31408 ) ;
#12703 = CARTESIAN_POINT ( 'NONE',  ( 0.7185039370078746268, 0.06523048226347956391, 1.168799212598425896 ) ) ;
#12704 = CARTESIAN_POINT ( 'NONE',  ( 0.8019270111902717657, 0.1787899950787401604, 0.7037401574265510495 ) ) ;
#12705 = ADVANCED_FACE ( 'NONE', ( #20358 ), #34996, .F. ) ;
#12706 = VERTEX_POINT ( 'NONE', #34295 ) ;
#12707 = DIRECTION ( 'NONE',  ( 0.000000000000000000, 0.000000000000000000, -1.000000000000000000 ) ) ;
#12708 = LINE ( 'NONE', #9084, #9742 ) ;
#12709 = CARTESIAN_POINT ( 'NONE',  ( -0.07405724077823318263, -1.661417322780881500, -0.1787899950787401604 ) ) ;
#12710 = CARTESIAN_POINT ( 'NONE',  ( -1.094772975963752103E-17, -0.9207677164816693294, -0.1787899950787401882 ) ) ;
#12711 = CARTESIAN_POINT ( 'NONE',  ( 0.06523048226347956391, -1.432578740157480324, 0.1574803149606297803 ) ) ;
#12712 = CARTESIAN_POINT ( 'NONE',  ( -0.8759842519685039353, 0.1574803149606299191, 1.397637795275590511 ) ) ;
#12713 = EDGE_LOOP ( 'NONE', ( #11959, #32452, #16975, #25153 ) ) ;
#12714 = ORIENTED_EDGE ( 'NONE', *, *, #10960, .T. ) ;
#12715 = CARTESIAN_POINT ( 'NONE',  ( -0.7495606340400177148, 0.1264236179284866091, 1.970964566875370139 ) ) ;
#12716 = CARTESIAN_POINT ( 'NONE',  ( 0.8759842519685039353, -0.1787899950787401882, 1.906988188922614125 ) ) ;
#12717 = ORIENTED_EDGE ( 'NONE', *, *, #1611, .T. ) ;
#12718 = FACE_OUTER_BOUND ( 'NONE', #1394, .T. ) ;
#12719 = CARTESIAN_POINT ( 'NONE',  ( 0.7495606340400177148, -0.1264236179284866091, 0.4847440944344252323 ) ) ;
#12720 = CARTESIAN_POINT ( 'NONE',  ( -0.8759842519685039353, 0.1787899950787401882, 1.370570866087968520 ) ) ;
#12721 = DIRECTION ( 'NONE',  ( -1.000000000000000000, 0.000000000000000000, 0.000000000000000000 ) ) ;
#12722 = CARTESIAN_POINT ( 'NONE',  ( -0.8759842519685039353, -0.1787899950787401882, 0.05659448813521291560 ) ) ;
#12723 = CARTESIAN_POINT ( 'NONE',  ( -0.5314960629921260393, 0.000000000000000000, 4.498031496062992574 ) ) ;
#12724 = CARTESIAN_POINT ( 'NONE',  ( -0.9500414927467378812, -0.1787899950787401604, 1.751968503883245765 ) ) ;
#12725 = CARTESIAN_POINT ( 'NONE',  ( -0.6971942568897626646, -0.07405724077823297447, 0.04921259837143338034 ) ) ;
#12726 = CARTESIAN_POINT ( 'NONE',  ( -0.8759842519685039353, -0.1574803149606299191, 1.692913385826771533 ) ) ;
#12727 = DIRECTION ( 'NONE',  ( 0.000000000000000000, 0.000000000000000000, 1.000000000000000000 ) ) ;
#12728 = CARTESIAN_POINT ( 'NONE',  ( 1.054774247047244096, 0.000000000000000000, 1.680610236166708793 ) ) ;
#12729 = CARTESIAN_POINT ( 'NONE',  ( 0.1352415222742598400, -0.09842519685039370636, -0.1450469393348480240 ) ) ;
#12730 = CARTESIAN_POINT ( 'NONE',  ( -0.8107537697050254399, -0.1574803149606297803, 0.7357283463491665065 ) ) ;
#12731 = AXIS2_PLACEMENT_3D ( 'NONE', #28600, #24275, #39097 ) ;
#12732 = CIRCLE ( 'NONE', #30981, 0.09842519685039370636 ) ;
#12733 = EDGE_CURVE ( 'NONE', #47141, #5874, #11045, .T. ) ;
#12734 = ORIENTED_EDGE ( 'NONE', *, *, #19039, .T. ) ;
#12735 = CARTESIAN_POINT ( 'NONE',  ( 0.1264236179284866091, -1.053641732229700700, 0.1264236179284866091 ) ) ;
#12736 = CARTESIAN_POINT ( 'NONE',  ( -0.07405724077823318263, -1.252952755851747924, 0.1787899950787401604 ) ) ;
#12737 = DIRECTION ( 'NONE',  ( 0.000000000000000000, -1.000000000000000000, 0.000000000000000000 ) ) ;
#12738 = SHAPE_REPRESENTATION_RELATIONSHIP ( 'NONE' , 'NONE' ,  #9335, #5536 ) ;
#12739 = CARTESIAN_POINT ( 'NONE',  ( 1.002407869896990045, 0.1264236179284866091, 0.3813976377415121966 ) ) ;
#12740 = CARTESIAN_POINT ( 'NONE',  ( -0.1797182628040039087, -0.4759296363546985376, -0.07444174185955065859 ) ) ;
#12741 = CARTESIAN_POINT ( 'NONE',  ( -0.7185039370078746268, 0.06523048226347956391, 0.8439960628845977197 ) ) ;
#12742 = CARTESIAN_POINT ( 'NONE',  ( 0.1574803149606300301, -0.04478346456692917921, -0.06523048226347956391 ) ) ;
#12743 = CARTESIAN_POINT ( 'NONE',  ( 0.07405724077823318263, -0.1358267715997797664, -0.1787899950787401604 ) ) ;
#12744 = AXIS2_PLACEMENT_3D ( 'NONE', #47090, #18341, #32983 ) ;
#12745 = CARTESIAN_POINT ( 'NONE',  ( 0.7495606340400177148, -0.1264236179284866091, 0.9522637794737952577 ) ) ;
#12746 = EDGE_CURVE ( 'NONE', #758, #43833, #9049, .T. ) ;
#12748 = CARTESIAN_POINT ( 'NONE',  ( 0.01035225325190847548, 0.08294251417010607697, 0.1319299025309686735 ) ) ;
#12747 = CARTESIAN_POINT ( 'NONE',  ( 0.1987795079023654821, 0.1807288298655941872, -0.05471869868084587585 ) ) ;
#12749 = CARTESIAN_POINT ( 'NONE',  ( 1.002407869896990045, -0.1264236179284866091, 1.911909448765133801 ) ) ;
#12750 = EDGE_CURVE ( 'NONE', #42394, #827, #2366, .T. ) ;
#12751 = CARTESIAN_POINT ( 'NONE',  ( 0.7646288533564489232, -0.1113553986120547346, 0.1919291338582677087 ) ) ;
#12752 = CARTESIAN_POINT ( 'NONE',  ( -1.033464566929133799, 0.000000000000000000, 0.7578740157480314821 ) ) ;
#12753 = CARTESIAN_POINT ( 'NONE',  ( 0.1787899950787401604, -0.3769685038832444324, -0.07405724077823318263 ) ) ;
#12754 = CARTESIAN_POINT ( 'NONE',  ( -0.07405724077823318263, -1.449803149552535642, 0.1787899950787401604 ) ) ;
#12755 = CARTESIAN_POINT ( 'NONE',  ( 1.054774247047244540, 0.07405724077823318263, 0.3444881889226146243 ) ) ;
#12756 = CARTESIAN_POINT ( 'NONE',  ( -1.054774247047244540, -0.07405724077823318263, 1.870078740103715331 ) ) ;
#12757 = ORIENTED_EDGE ( 'NONE', *, *, #19453, .T. ) ;
#12758 = CARTESIAN_POINT ( 'NONE',  ( -1.002407869896990045, -0.1264236179284866091, 1.242618110182456714 ) ) ;
#12759 = FACE_OUTER_BOUND ( 'NONE', #28139, .T. ) ;
#12760 = CARTESIAN_POINT ( 'NONE',  ( 0.7495606340400177148, -0.1264236179284866091, 1.350885826717889815 ) ) ;
#12761 = CARTESIAN_POINT ( 'NONE',  ( -1.054774247047244096, 0.000000000000000000, 0.4995078739619842612 ) ) ;
#12762 = CARTESIAN_POINT ( 'NONE',  ( -0.6971942568897648851, -0.07405724077823297447, 1.264763779473795813 ) ) ;
#12763 = CARTESIAN_POINT ( 'NONE',  ( -1.033464566929133799, 0.000000000000000000, 0.2460629921259842590 ) ) ;
#12764 = CARTESIAN_POINT ( 'NONE',  ( 0.8107537697050254399, 0.1574803149606300301, 0.05167322823892971789 ) ) ;
#12765 = CARTESIAN_POINT ( 'NONE',  ( 0.8019270111902716547, -0.1787899950787401604, 0.6446850393163160442 ) ) ;
#12766 = CARTESIAN_POINT ( 'NONE',  ( -0.8019270111902716547, -0.1787899950787401604, 0.4822834645131655606 ) ) ;
#12767 = DIRECTION ( 'NONE',  ( 0.000000000000000000, 1.000000000000000000, 0.000000000000000000 ) ) ;
#12768 = ORIENTED_EDGE ( 'NONE', *, *, #30555, .T. ) ;
#12769 = CARTESIAN_POINT ( 'NONE',  ( -0.8759842519685039353, 0.1574803149606299191, 0.3346456692913385988 ) ) ;
#12770 = CARTESIAN_POINT ( 'NONE',  ( 1.002407869896990045, 0.1264236179284866091, 1.173720472387181246 ) ) ;
#12771 = CARTESIAN_POINT ( 'NONE',  ( -0.1920024521149243935, -0.09851385062432203854, 0.1351331792528293330 ) ) ;
#12772 = CARTESIAN_POINT ( 'NONE',  ( -0.2559055118110236116, -0.02858058760286992517, -0.02996975140571705304 ) ) ;
#12773 = CARTESIAN_POINT ( 'NONE',  ( -1.033464566929134687, -0.06523048226347956391, 1.306594488188977055 ) ) ;
#12774 = CARTESIAN_POINT ( 'NONE',  ( -0.6971942568897637749, 2.189545951927499583E-17, 0.1205708660879689087 ) ) ;
#12775 = CARTESIAN_POINT ( 'NONE',  ( 0.07405724077823318263, -1.657604283189869632, 0.1787899950787401604 ) ) ;
#12776 = ORIENTED_EDGE ( 'NONE', *, *, #11118, .F. ) ;
#12777 = CARTESIAN_POINT ( 'NONE',  ( -0.1377952755905511861, 0.1564960629921283985, 0.9074803149606294195 ) ) ;
#12778 = CARTESIAN_POINT ( 'NONE',  ( -0.1787899950787401604, -0.6328740156942683770, -0.07405724077823318263 ) ) ;
#12779 = CARTESIAN_POINT ( 'NONE',  ( -0.2624241468390500209, -0.1651049555683128389, 0.9036955682336973439 ) ) ;
#12780 = ORIENTED_EDGE ( 'NONE', *, *, #15074, .F. ) ;
#12781 = CARTESIAN_POINT ( 'NONE',  ( 0.9500414927467378812, -0.1787899950787401604, 1.274606299158834277 ) ) ;
#12782 = CARTESIAN_POINT ( 'NONE',  ( 1.033464566929133799, 0.000000000000000000, 1.456692913278299084 ) ) ;
#12783 = CARTESIAN_POINT ( 'NONE',  ( -0.3161444924769509779, 2.177585298233989164, -3.731703755406937439 ) ) ;
#12784 = CARTESIAN_POINT ( 'NONE',  ( -0.1264236179284866091, -0.2367125983714334636, 0.1264236179284866091 ) ) ;
#12785 = CARTESIAN_POINT ( 'NONE',  ( 0.9873396505805591694, -0.1113553986120547346, 0.1919291337507405548 ) ) ;
#12786 = CARTESIAN_POINT ( 'NONE',  ( 0.8019270111902717657, -0.1787899950787401604, 1.545275590497416696 ) ) ;
#12787 = CARTESIAN_POINT ( 'NONE',  ( 0.6971942568897637749, 2.189545951927499583E-17, 0.2386811023084413619 ) ) ;
#12788 = EDGE_CURVE ( 'NONE', #25178, #16859, #42725, .T. ) ;
#12789 = CARTESIAN_POINT ( 'NONE',  ( -0.1264236179284866091, 0.01808469318808409235, -0.1264236179284866091 ) ) ;
#12790 = CARTESIAN_POINT ( 'NONE',  ( -0.1787899950787401604, -1.809055118056471123, 0.07405724077823318263 ) ) ;
#12791 = APPLICATION_PROTOCOL_DEFINITION ( 'draft international standard', 'automotive_design', 1998, #29442 ) ;
#12792 = DIRECTION ( 'NONE',  ( 0.000000000000000000, 1.000000000000000000, 0.000000000000000000 ) ) ;
#12793 = VECTOR ( 'NONE', #15903, 39.37007874015748854 ) ;
#12794 = CARTESIAN_POINT ( 'NONE',  ( -0.8019270111902716547, -0.1787899950787401604, 0.7627952755367883864 ) ) ;
#12795 = EDGE_CURVE ( 'NONE', #10222, #35496, #9587, .T. ) ;
#12796 = CARTESIAN_POINT ( 'NONE',  ( -1.033464566929134687, -0.06523048226347956391, 1.296751968396409049 ) ) ;
#12798 = CARTESIAN_POINT ( 'NONE',  ( 0.000000000000000000, -0.1637340966949556997, -0.2095700869694007984 ) ) ;
#12797 = CARTESIAN_POINT ( 'NONE',  ( -9.642888182262618425E-18, -0.9035433070866142335, -0.1574803149606299191 ) ) ;
#12799 = CARTESIAN_POINT ( 'NONE',  ( 0.1797182628040039365, -1.595516250527927005, -2.200913952912460540E-17 ) ) ;
#12800 = CARTESIAN_POINT ( 'NONE',  ( 0.1574803149606300023, 0.7443365962042343131, -3.523993443072799270 ) ) ;
#12801 = CARTESIAN_POINT ( 'NONE',  ( -0.07405724077823318263, -0.3474409448281265411, 0.1787899950787401604 ) ) ;
#12802 = PLANE ( 'NONE',  #26908 ) ;
#12803 = CARTESIAN_POINT ( 'NONE',  ( 0.8019270111902717657, 0.1787899950787401604, 1.496062992072220821 ) ) ;
#12804 = CARTESIAN_POINT ( 'NONE',  ( 1.002407869896990045, 0.1264236179284866091, 1.838090551127338657 ) ) ;
#12805 = CARTESIAN_POINT ( 'NONE',  ( 0.7495606340400177148, 0.1264236179284866091, 0.4699803149068661479 ) ) ;
#12806 = ORIENTED_EDGE ( 'NONE', *, *, #9100, .F. ) ;
#12808 = ORIENTED_EDGE ( 'NONE', *, *, #6701, .F. ) ;
#12807 = DIRECTION ( 'NONE',  ( 0.000000000000000000, 0.000000000000000000, 1.000000000000000000 ) ) ;
#12809 = EDGE_CURVE ( 'NONE', #44905, #15659, #24377, .T. ) ;
#12810 = CARTESIAN_POINT ( 'NONE',  ( -0.1574803149606299191, 1.928577636452524610E-17, -0.04012007874015743186 ) ) ;
#12811 = CARTESIAN_POINT ( 'NONE',  ( 1.614954907737318939E-16, 0.1574803149606340824, 0.4940944881889759444 ) ) ;
#12813 = CARTESIAN_POINT ( 'NONE',  ( -0.1264236179284866091, 0.03887795280966901967, 0.1264236179284866091 ) ) ;
#12812 = CARTESIAN_POINT ( 'NONE',  ( -0.1574803149606299191, -0.8444881888688503535, 0.000000000000000000 ) ) ;
#12814 = CARTESIAN_POINT ( 'NONE',  ( 1.054774247047244540, 0.07405724077823318263, 0.4970472440407249226 ) ) ;
#12815 = CARTESIAN_POINT ( 'NONE',  ( 0.1377952755905511861, 0.1564960629921262614, 0.8070866141732283561 ) ) ;
#12816 = CARTESIAN_POINT ( 'NONE',  ( 0.7495606340400177148, -0.1264236179284866091, 0.5585629920722204877 ) ) ;
#12817 = CARTESIAN_POINT ( 'NONE',  ( 0.8107537697050254399, 0.1574803149606300301, 0.2189960629921262614 ) ) ;
#12818 = CARTESIAN_POINT ( 'NONE',  ( 0.7185039370078739607, 1.928577636452523993E-17, 0.8070866140657008136 ) ) ;
#12819 = ORIENTED_EDGE ( 'NONE', *, *, #34372, .T. ) ;
#12820 = CARTESIAN_POINT ( 'NONE',  ( 1.002407869896990045, -0.1264236179284866091, 0.9670275590013542866 ) ) ;
#12822 = CARTESIAN_POINT ( 'NONE',  ( -0.07405724077823318263, -1.375984251914741163, 0.1787899950787401604 ) ) ;
#12821 = CARTESIAN_POINT ( 'NONE',  ( 0.06523048226347956391, -1.107775590443654146, 0.1574803149606297803 ) ) ;
#12823 = CARTESIAN_POINT ( 'NONE',  ( -0.7185039370078739607, 1.928577636452523993E-17, 0.5314960628845992741 ) ) ;
#12824 = CARTESIAN_POINT ( 'NONE',  ( -0.9873396505805591694, 0.1113553986120547346, 0.8021653543307086798 ) ) ;
#12825 = CARTESIAN_POINT ( 'NONE',  ( -0.8759842519685039353, -0.1574803149606299191, 1.299212598425196985 ) ) ;
#12826 = CARTESIAN_POINT ( 'NONE',  ( -1.033464566929134687, -0.06523048226347956391, 1.060531495955465031 ) ) ;
#12828 = CARTESIAN_POINT ( 'NONE',  ( -1.033464566929133799, 0.000000000000000000, 0.7480314959554645871 ) ) ;
#12827 = CARTESIAN_POINT ( 'NONE',  ( 0.1387979473508932082, 0.2153574986359478305, -0.3148284977848753163 ) ) ;
#12829 = CARTESIAN_POINT ( 'NONE',  ( 0.9500414927467377701, -0.1787899950787401604, 0.1377952755367876370 ) ) ;
#12830 = CARTESIAN_POINT ( 'NONE',  ( 1.033464566929134687, 0.06523048226347956391, 1.341043306979086136 ) ) ;
#12831 = ORIENTED_EDGE ( 'NONE', *, *, #45094, .T. ) ;
#12832 = ORIENTED_EDGE ( 'NONE', *, *, #42819, .T. ) ;
#12833 = CARTESIAN_POINT ( 'NONE',  ( 0.1651804164989525703, 0.1299212598425197318, 0.06841997037041518126 ) ) ;
#12834 = FACE_OUTER_BOUND ( 'NONE', #23947, .T. ) ;
#12835 = CARTESIAN_POINT ( 'NONE',  ( -0.8759842519685039353, -0.1787899950787401882, 1.744586614119464807 ) ) ;
#12836 = CARTESIAN_POINT ( 'NONE',  ( 0.06523048226347956391, -0.1874999998924729294, -0.1574803149606300301 ) ) ;
#12837 = ORIENTED_EDGE ( 'NONE', *, *, #25392, .T. ) ;
#12838 = CARTESIAN_POINT ( 'NONE',  ( 0.000000000000000000, 0.000000000000000000, 0.09842519685039370636 ) ) ;
#12839 = CARTESIAN_POINT ( 'NONE',  ( 0.7185039370078739607, 1.928577636452523993E-17, 1.870078740049952559 ) ) ;
#12840 = DIRECTION ( 'NONE',  ( 0.000000000000000000, 0.2126700594527823618, -0.9771240687918550938 ) ) ;
#12841 = CARTESIAN_POINT ( 'NONE',  ( -0.07405724077823318263, -1.071974361930026598, 0.1787899950787401604 ) ) ;
#12842 = ORIENTED_EDGE ( 'NONE', *, *, #20127, .T. ) ;
#12843 = CARTESIAN_POINT ( 'NONE',  ( 3.284318927891251994E-17, -0.1087598424659214497, 0.1787899950787401882 ) ) ;
#12844 = ORIENTED_EDGE ( 'NONE', *, *, #30294, .T. ) ;
#12845 = EDGE_CURVE ( 'NONE', #17121, #25548, #33566, .T. ) ;
#12846 = CARTESIAN_POINT ( 'NONE',  ( 1.033464566929133799, 0.000000000000000000, 1.732283464459401623 ) ) ;
#12847 = CARTESIAN_POINT ( 'NONE',  ( -0.9412147342319837628, -0.1574803149606297803, 0.4256889762704256230 ) ) ;
#12848 = ( BOUNDED_CURVE ( )  B_SPLINE_CURVE ( 2, ( #24398, #20555, #10261, #31839, #28239, #6168, #2800, #47146, #35197 ),
 .UNSPECIFIED., .F., .F. ) 
 B_SPLINE_CURVE_WITH_KNOTS ( ( 3, 2, 2, 2, 3 ),
 ( 0.9899999999999999911, 0.9925000000000000488, 0.9949999999999999956, 0.9975000000000000533, 1.000000000000000000 ),
 .UNSPECIFIED. ) 
 CURVE ( )  GEOMETRIC_REPRESENTATION_ITEM ( )  RATIONAL_B_SPLINE_CURVE ( ( 1.000000000000000000, 0.9238795325112869605, 1.000000000000000000, 0.9238795325112869605, 1.000000000000000000, 0.9238795325112869605, 1.000000000000000000, 0.9238795325112869605, 1.000000000000000000 ) ) 
 REPRESENTATION_ITEM ( '' )  ) ;
#12849 = PRODUCT_DEFINITION_SHAPE ( 'NONE', 'NONE',  #16326 ) ;
#12850 = CARTESIAN_POINT ( 'NONE',  ( 1.033464566929134687, 0.06523048226347956391, 1.783956692913386766 ) ) ;
#12851 = ADVANCED_FACE ( 'NONE', ( #35234 ), #35460, .T. ) ;
#12852 = CARTESIAN_POINT ( 'NONE',  ( 0.1264236179284866091, -0.5812007873478111097, 0.1264236179284866091 ) ) ;
#12853 = ORIENTED_EDGE ( 'NONE', *, *, #22552, .F. ) ;
#12854 = CARTESIAN_POINT ( 'NONE',  ( -0.7646288533564489232, -0.1113553986120547346, 1.018700787401574770 ) ) ;
#12855 = AXIS2_PLACEMENT_3D ( 'NONE', #1037, #18551, #15695 ) ;
#12856 = CARTESIAN_POINT ( 'NONE',  ( -0.07444174185955065859, -1.228882392260211898, -0.1797182628040039087 ) ) ;
#12857 = CARTESIAN_POINT ( 'NONE',  ( 1.054774247047244540, 0.07405724077823318263, 1.131889763725763665 ) ) ;
#12858 = CARTESIAN_POINT ( 'NONE',  ( 0.8019270111902716547, 0.1787899950787401604, 0.1525590550643468324 ) ) ;
#12859 = LINE ( 'NONE', #2278, #42202 ) ;
#12860 = CARTESIAN_POINT ( 'NONE',  ( 0.7185039370078739607, 1.928577636452523993E-17, 1.525590551181102317 ) ) ;
#12862 = CARTESIAN_POINT ( 'NONE',  ( 0.4330708661417295158, 0.1864803149606300281, -1.186023622047243986 ) ) ;
#12861 = CARTESIAN_POINT ( 'NONE',  ( 0.7801209693189999905, 0.1293481257666107553, 1.980357471351750442 ) ) ;
#12863 = CARTESIAN_POINT ( 'NONE',  ( 0.8759842519685039353, -0.1574803149606299191, 0.4625984250893235838 ) ) ;
#12864 = CARTESIAN_POINT ( 'NONE',  ( -0.7185039370078746268, -0.06523048226347956391, 1.636318897530269156 ) ) ;
#12865 = VECTOR ( 'NONE', #10880, 39.37007874015748143 ) ;
#12866 = CARTESIAN_POINT ( 'NONE',  ( 0.1264236179284866091, 0.06348425202226751218, -0.1264236179284866091 ) ) ;
#12867 = ( BOUNDED_CURVE ( )  B_SPLINE_CURVE ( 2, ( #42597, #9809, #13862, #24418, #28507, #20809, #2590, #28751, #17226 ),
 .UNSPECIFIED., .F., .T. ) 
 B_SPLINE_CURVE_WITH_KNOTS ( ( 3, 2, 2, 2, 3 ),
 ( 0.3900000000000000133, 0.3925000000000000155, 0.3950000000000000178, 0.3975000000000000200, 0.4000000000000000222 ),
 .UNSPECIFIED. ) 
 CURVE ( )  GEOMETRIC_REPRESENTATION_ITEM ( )  RATIONAL_B_SPLINE_CURVE ( ( 1.000000000000000000, 0.9238795325112869605, 1.000000000000000000, 0.9238795325112869605, 1.000000000000000000, 0.9238795325112869605, 1.000000000000000000, 0.9238795325112869605, 1.000000000000000000 ) ) 
 REPRESENTATION_ITEM ( '' )  ) ;
#12868 = CARTESIAN_POINT ( 'NONE',  ( 0.8019270111902716547, -0.1787899950787401604, 0.9547244093950545407 ) ) ;
#12869 = CARTESIAN_POINT ( 'NONE',  ( 0.8759842519685039353, 0.1787899950787401882, 1.769192913332062966 ) ) ;
#12870 = CARTESIAN_POINT ( 'NONE',  ( 0.7185039370078739607, 1.928577636452523993E-17, 0.2952755904436539236 ) ) ;
#12871 = ORIENTED_EDGE ( 'NONE', *, *, #12571, .T. ) ;
#12872 = CARTESIAN_POINT ( 'NONE',  ( -0.7185039370078739607, 0.000000000000000000, -2.869337061179095023E-17 ) ) ;
#12873 = CARTESIAN_POINT ( 'NONE',  ( 2.892866454678787531E-17, -1.622047243986960430, 0.1574803149606299191 ) ) ;
#12874 = CARTESIAN_POINT ( 'NONE',  ( -0.7185039370078739607, 1.928577636452523993E-17, 0.2165354329633393804 ) ) ;
#12875 = CARTESIAN_POINT ( 'NONE',  ( 0.6971942568897637749, 2.189545951927499583E-17, 1.262303149552535420 ) ) ;
#12876 = CARTESIAN_POINT ( 'NONE',  ( 0.07857503534296064740, -0.08918665060160307911, 0.2400663896719301416 ) ) ;
#12877 = EDGE_CURVE ( 'NONE', #32389, #16635, #11314, .T. ) ;
#12878 = CARTESIAN_POINT ( 'NONE',  ( -1.094772975963752103E-17, 0.1077755906049446960, -0.1787899950787401882 ) ) ;
#12879 = DIRECTION ( 'NONE',  ( 0.000000000000000000, 0.000000000000000000, -1.000000000000000000 ) ) ;
#12880 = CARTESIAN_POINT ( 'NONE',  ( -1.002407869896990045, -0.1264236179284866091, 0.5290354330171024300 ) ) ;
#12881 = CARTESIAN_POINT ( 'NONE',  ( 0.7185039370078739607, 1.928577636452523993E-17, 0.8956692913385826404 ) ) ;
#12882 = CARTESIAN_POINT ( 'NONE',  ( 0.7185039370078739607, 0.000000000000000000, 4.498031496062992574 ) ) ;
#12883 = VERTEX_POINT ( 'NONE', #46685 ) ;
#12884 = APPLICATION_CONTEXT ( 'automotive_design' ) ;
#12885 = CARTESIAN_POINT ( 'NONE',  ( 0.07405724077823318263, -1.553149606245448178, -0.1787899950787401604 ) ) ;
#12886 = CARTESIAN_POINT ( 'NONE',  ( -1.054774247047244540, -0.07405724077823318263, 0.9694881889226144578 ) ) ;
#12887 = CARTESIAN_POINT ( 'NONE',  ( -0.8107537697050253289, 0.1574803149606300301, 0.02214566929133862661 ) ) ;
#12888 = ORIENTED_EDGE ( 'NONE', *, *, #15774, .T. ) ;
#12889 = CARTESIAN_POINT ( 'NONE',  ( -1.002407869896990045, 0.1264236179284866091, 0.7406496062454487328 ) ) ;
#12890 = ORIENTED_EDGE ( 'NONE', *, *, #44920, .F. ) ;
#12891 = DIRECTION ( 'NONE',  ( 3.469446951953614189E-15, 1.000000000000000000, 0.000000000000000000 ) ) ;
#12892 = VECTOR ( 'NONE', #38777, 39.37007874015748143 ) ;
#12893 = LINE ( 'NONE', #27527, #25957 ) ;
#12894 = ORIENTED_EDGE ( 'NONE', *, *, #24208, .F. ) ;
#12895 = CARTESIAN_POINT ( 'NONE',  ( -0.1459235064575962748, -0.08956109133572084935, -0.09835919643184390382 ) ) ;
#12896 = DIRECTION ( 'NONE',  ( 1.822029033848725028E-16, 0.000000000000000000, 1.000000000000000000 ) ) ;
#12897 = ORIENTED_EDGE ( 'NONE', *, *, #13858, .T. ) ;
#12898 = LINE ( 'NONE', #45927, #18739 ) ;
#12899 = EDGE_CURVE ( 'NONE', #9878, #11697, #37357, .T. ) ;
#12900 = AXIS2_PLACEMENT_3D ( 'NONE', #24429, #32096, #43331 ) ;
#12901 = CARTESIAN_POINT ( 'NONE',  ( -0.7495606340400177148, -0.1264236179284866091, 0.4404527558517480901 ) ) ;
#12902 = CARTESIAN_POINT ( 'NONE',  ( -0.1787899950787401882, -1.788017669016641831, 0.000000000000000000 ) ) ;
#12903 = EDGE_CURVE ( 'NONE', #33336, #19054, #39260, .T. ) ;
#12904 = ORIENTED_EDGE ( 'NONE', *, *, #37158, .T. ) ;
#12905 = EDGE_CURVE ( 'NONE', #5683, #24890, #9839, .T. ) ;
#12906 = CARTESIAN_POINT ( 'NONE',  ( -1.054774247047244096, 0.000000000000000000, 1.680610236166708793 ) ) ;
#12907 = ADVANCED_FACE ( 'NONE', ( #15069 ), #177, .F. ) ;
#12908 = CARTESIAN_POINT ( 'NONE',  ( -0.1787899950787401604, -1.425196850339937482, -0.07405724077823318263 ) ) ;
#12909 = LINE ( 'NONE', #20774, #18771 ) ;
#12910 = CARTESIAN_POINT ( 'NONE',  ( 1.033464566929133799, 0.000000000000000000, 1.535433070758614127 ) ) ;
#12911 = DIRECTION ( 'NONE',  ( 0.000000000000000000, 1.000000000000000000, 0.000000000000000000 ) ) ;
#12912 = CARTESIAN_POINT ( 'NONE',  ( 0.7185039370078746268, -0.06523048226347956391, 0.5437992125984247860 ) ) ;
#12913 = CARTESIAN_POINT ( 'NONE',  ( -0.07444174185955065859, -0.7170713686381637864, -0.1797182628040039087 ) ) ;
#12914 = CARTESIAN_POINT ( 'NONE',  ( 0.7185039370078739607, 0.000000000000000000, 4.498031496062992574 ) ) ;
#12915 = CARTESIAN_POINT ( 'NONE',  ( -0.8759842519685039353, 0.1574803149606299191, 1.190944881782236342 ) ) ;
#12917 = CARTESIAN_POINT ( 'NONE',  ( -0.7185039370078739607, 1.928577636452523993E-17, 0.05905511800270921846 ) ) ;
#12916 = CARTESIAN_POINT ( 'NONE',  ( 2.892866454678787531E-17, -0.4507874015748031815, 0.1574803149606299191 ) ) ;
#12918 = LINE ( 'NONE', #27313, #16937 ) ;
#12919 = ORIENTED_EDGE ( 'NONE', *, *, #29391, .T. ) ;
#12920 = CARTESIAN_POINT ( 'NONE',  ( -0.3100393700787401619, 0.000000000000000000, 1.181102362204724310 ) ) ;
#12921 = CARTESIAN_POINT ( 'NONE',  ( -1.002407869896990045, -0.1264236179284866091, 1.045767716481669440 ) ) ;
#12922 = CARTESIAN_POINT ( 'NONE',  ( 0.8759842519685039353, -0.1574803149606299191, 1.141732283464567121 ) ) ;
#12924 = CYLINDRICAL_SURFACE ( 'NONE', #28574, 0.7381889763779526659 ) ;
#12923 = FACE_OUTER_BOUND ( 'NONE', #3972, .T. ) ;
#12925 = DIRECTION ( 'NONE',  ( 0.000000000000000000, -1.000000000000000000, 0.000000000000000000 ) ) ;
#12927 = CARTESIAN_POINT ( 'NONE',  ( -0.9412147342319837628, -0.1574803149606297803, 1.961122047136568014 ) ) ;
#12926 = CARTESIAN_POINT ( 'NONE',  ( 0.8107537697050254399, -0.1574803149606297803, 0.5782480313885360879 ) ) ;
#12928 = CARTESIAN_POINT ( 'NONE',  ( 1.033464566929133799, 0.000000000000000000, 0.1279527559055118058 ) ) ;
#12929 = CARTESIAN_POINT ( 'NONE',  ( -0.1787899950787401882, -0.4729330708123779536, 0.000000000000000000 ) ) ;
#12930 = ORIENTED_EDGE ( 'NONE', *, *, #12430, .F. ) ;
#12931 = TOROIDAL_SURFACE ( 'NONE', #2188, 0.1870078740157480324, 0.04921259842519685318 ) ;
#12932 = CARTESIAN_POINT ( 'NONE',  ( 0.7495606340400177148, -0.1264236179284866091, 0.7947834645131652831 ) ) ;
#12933 = EDGE_LOOP ( 'NONE', ( #6001, #6838, #8112, #29479 ) ) ;
#12934 = CARTESIAN_POINT ( 'NONE',  ( 0.9412147342319837628, -0.1574803149606297803, 1.301673228346455602 ) ) ;
#12935 = CYLINDRICAL_SURFACE ( 'NONE', #18151, 0.1574803149606299191 ) ;
#12936 = CARTESIAN_POINT ( 'NONE',  ( -0.07405724077823318263, -1.740157480261197875, -0.1787899950787401604 ) ) ;
#12937 = CARTESIAN_POINT ( 'NONE',  ( -0.07405724077823318263, -1.075787401521038689, -0.1787899950787401604 ) ) ;
#12939 = CIRCLE ( 'NONE', #3744, 0.1377952755905509086 ) ;
#12938 = CARTESIAN_POINT ( 'NONE',  ( -9.642888182262618425E-18, -1.297244094488189115, -0.1574803149606299191 ) ) ;
#12940 = CARTESIAN_POINT ( 'NONE',  ( -0.8759842519685039353, 0.1574803149606299191, 1.860236220364913207 ) ) ;
#12941 = ORIENTED_EDGE ( 'NONE', *, *, #29609, .F. ) ;
#12942 = ORIENTED_EDGE ( 'NONE', *, *, #10903, .T. ) ;
#12943 = CARTESIAN_POINT ( 'NONE',  ( -1.054774247047244096, 0.000000000000000000, 1.956200787347811110 ) ) ;
#12944 = CARTESIAN_POINT ( 'NONE',  ( 0.7495606340400177148, 0.1264236179284866091, 1.813484251914740053 ) ) ;
#12945 = ORIENTED_EDGE ( 'NONE', *, *, #2957, .T. ) ;
#12946 = CARTESIAN_POINT ( 'NONE',  ( 1.054774247047244096, 0.000000000000000000, 0.4601377952218267953 ) ) ;
#12947 = CARTESIAN_POINT ( 'NONE',  ( -0.6971942568897648851, 0.07405724077823318263, 1.417322834591906222 ) ) ;
#12948 = CARTESIAN_POINT ( 'NONE',  ( -0.8759842519685039353, 0.1787899950787401882, 0.2731299212060791515 ) ) ;
#12949 = LINE ( 'NONE', #31167, #35239 ) ;
#12950 = CARTESIAN_POINT ( 'NONE',  ( -1.054774247047244540, 0.07405724077823318263, 1.683070866087970074 ) ) ;
#12951 = CARTESIAN_POINT ( 'NONE',  ( -0.9412147342319837628, -0.1574803149606297803, 2.000492125876725424 ) ) ;
#12952 = CARTESIAN_POINT ( 'NONE',  ( -0.2082510178749903962, 0.06746187776213008469, 0.1651992896370024499 ) ) ;
#12953 = CARTESIAN_POINT ( 'NONE',  ( -1.033464566929134687, 0.06523048226347956391, 1.783956692913386766 ) ) ;
#12954 = DIRECTION ( 'NONE',  ( 0.6018150231520413840, -0.000000000000000000, -0.7986355100472980473 ) ) ;
#12955 = CARTESIAN_POINT ( 'NONE',  ( -0.03350623722892267370, -0.09842519685039370636, 0.2233118325431988072 ) ) ;
#12956 = CARTESIAN_POINT ( 'NONE',  ( -1.181162989532618060E-16, 0.000000000000000000, -0.3937007874015748254 ) ) ;
#12957 = EDGE_CURVE ( 'NONE', #34176, #43833, #47174, .T. ) ;
#12958 = ORIENTED_EDGE ( 'NONE', *, *, #40129, .T. ) ;
#12959 = VECTOR ( 'NONE', #13099, 39.37007874015748854 ) ;
#12960 = EDGE_CURVE ( 'NONE', #21109, #22330, #12939, .T. ) ;
#12961 = CARTESIAN_POINT ( 'NONE',  ( -0.1787899950787401604, -1.031496062938363822, -0.07405724077823318263 ) ) ;
#12962 = CIRCLE ( 'NONE', #44328, 0.5905511811023623769 ) ;
#12963 = CARTESIAN_POINT ( 'NONE',  ( -0.1264236179284866091, -1.176673228292692830, 0.1264236179284866091 ) ) ;
#12964 = DIRECTION ( 'NONE',  ( 1.000000000000000000, 0.000000000000000000, -1.822029033848725275E-16 ) ) ;
#12965 = CARTESIAN_POINT ( 'NONE',  ( -0.07444174185955065859, -0.4414808174570614696, -0.1797182628040039087 ) ) ;
#12966 = DIRECTION ( 'NONE',  ( 1.000000000000000000, 0.000000000000000000, 0.000000000000000000 ) ) ;
#12967 = CARTESIAN_POINT ( 'NONE',  ( -0.9873396505805591694, -0.1113553986120547346, 0.7431102361129447997 ) ) ;
#12968 = AXIS2_PLACEMENT_3D ( 'NONE', #14509, #29171, #32977 ) ;
#12969 = CARTESIAN_POINT ( 'NONE',  ( 0.1574803149606300301, 0.02903543307086614220, 0.06523048226347956391 ) ) ;
#12970 = CARTESIAN_POINT ( 'NONE',  ( -0.1787899950787401604, -0.1653543306548978520, -0.07405724077823318263 ) ) ;
#12971 = CARTESIAN_POINT ( 'NONE',  ( 0.1733357866104492107, 0.3740157480314960647, 1.025733466389925352 ) ) ;
#12972 = CARTESIAN_POINT ( 'NONE',  ( 0.9500414927467378812, 0.1787899950787401604, 0.9744094487651340231 ) ) ;
#12973 = ( BOUNDED_CURVE ( )  B_SPLINE_CURVE ( 2, ( #6101, #24113, #38938, #42045, #9248, #34420, #45416, #5648, #31309 ),
 .UNSPECIFIED., .F., .T. ) 
 B_SPLINE_CURVE_WITH_KNOTS ( ( 3, 2, 2, 2, 3 ),
 ( 0.7099999999999999645, 0.7125000000000000222, 0.7149999999999999689, 0.7175000000000000266, 0.7199999999999999734 ),
 .UNSPECIFIED. ) 
 CURVE ( )  GEOMETRIC_REPRESENTATION_ITEM ( )  RATIONAL_B_SPLINE_CURVE ( ( 1.000000000000000000, 0.9238795325112869605, 1.000000000000000000, 0.9238795325112869605, 1.000000000000000000, 0.9238795325112869605, 1.000000000000000000, 0.9238795325112869605, 1.000000000000000000 ) ) 
 REPRESENTATION_ITEM ( '' )  ) ;
#12975 = CARTESIAN_POINT ( 'NONE',  ( 0.1564216623530370331, 8.908831420875236139E-13, 0.1403857474672218497 ) ) ;
#12974 = CARTESIAN_POINT ( 'NONE',  ( 0.1789895911305919018, 0.1921545436410181107, -0.04147023971056211511 ) ) ;
#12976 = CARTESIAN_POINT ( 'NONE',  ( 0.6971942568897648851, -0.07405724077823297447, 1.938976377898990799 ) ) ;
#12977 = CARTESIAN_POINT ( 'NONE',  ( 0.9873396505805591694, 0.1113553986120547346, 0.7135826770578268530 ) ) ;
#12978 = CARTESIAN_POINT ( 'NONE',  ( 0.1787899950787401604, -0.4999999999462365619, 0.07405724077823318263 ) ) ;
#12979 = CARTESIAN_POINT ( 'NONE',  ( 1.284448818897637956, -0.3937007874015748254, 1.181102362204724310 ) ) ;
#12980 = CARTESIAN_POINT ( 'NONE',  ( 0.1264236179284866091, -1.442421259788756016, 0.1264236179284866091 ) ) ;
#12981 = DIRECTION ( 'NONE',  ( 1.822029033848725028E-16, 0.000000000000000000, 1.000000000000000000 ) ) ;
#12982 = AXIS2_PLACEMENT_3D ( 'NONE', #1930, #6468, #43602 ) ;
#12983 = CARTESIAN_POINT ( 'NONE',  ( -0.8759842519685039353, -0.1787899950787401882, 1.941437007820252081 ) ) ;
#12984 = ORIENTED_EDGE ( 'NONE', *, *, #21541, .F. ) ;
#12985 = CARTESIAN_POINT ( 'NONE',  ( -1.002407869896990045, 0.1264236179284866091, 1.488681102308440751 ) ) ;
#12986 = CARTESIAN_POINT ( 'NONE',  ( 0.8759842519685039353, -0.1787899950787401882, 1.473917322780881722 ) ) ;
#12987 = FACE_OUTER_BOUND ( 'NONE', #12933, .T. ) ;
#12988 = CARTESIAN_POINT ( 'NONE',  ( 0.06523048226347956391, -1.250492125876724314, -0.1574803149606300301 ) ) ;
#12989 = CARTESIAN_POINT ( 'NONE',  ( -0.7495606340400177148, -0.1264236179284866091, 0.6815944881352126172 ) ) ;
#12990 = CARTESIAN_POINT ( 'NONE',  ( -0.7495606340400177148, -0.1264236179284866091, 1.188484251914740275 ) ) ;
#12991 = DIRECTION ( 'NONE',  ( 1.822029033848725028E-16, 0.000000000000000000, 1.000000000000000000 ) ) ;
#12992 = CARTESIAN_POINT ( 'NONE',  ( 1.002407869896990045, 0.1264236179284866091, 0.5831692912848189803 ) ) ;
#12993 = CARTESIAN_POINT ( 'NONE',  ( -1.002407869896990045, 0.1264236179284866091, 0.5388779527021417826 ) ) ;
#12994 = CARTESIAN_POINT ( 'NONE',  ( 0.4330708661417322913, 0.1574803149606299191, 1.186023622047243986 ) ) ;
#12995 = CARTESIAN_POINT ( 'NONE',  ( 0.9412147342319837628, 0.1574803149606300301, 1.660925196742867982 ) ) ;
#12996 = ORIENTED_EDGE ( 'NONE', *, *, #37325, .F. ) ;
#12997 = CARTESIAN_POINT ( 'NONE',  ( -1.033464566929134687, 0.06523048226347956391, 0.2878937007874017295 ) ) ;
#12998 = VECTOR ( 'NONE', #359, 39.37007874015748143 ) ;
#12999 = CARTESIAN_POINT ( 'NONE',  ( 0.8759842519685039353, -0.1787899950787401882, 1.277066929080094448 ) ) ;
#13000 = CARTESIAN_POINT ( 'NONE',  ( 0.008047257146029232477, -0.09851385040156239448, 0.2239393559163176950 ) ) ;
#13001 = CARTESIAN_POINT ( 'NONE',  ( -0.7185039370078739607, 1.928577636452523993E-17, 1.830708661309795149 ) ) ;
#13002 = ORIENTED_EDGE ( 'NONE', *, *, #22296, .F. ) ;
#13003 = CARTESIAN_POINT ( 'NONE',  ( -1.033464566929134687, -0.06523048226347956391, 0.6373031496062994128 ) ) ;
#13004 = EDGE_CURVE ( 'NONE', #18185, #22505, #35529, .T. ) ;
#13005 = CARTESIAN_POINT ( 'NONE',  ( -0.1787899950787401604, -1.593627905237113174, -0.07405724077823318263 ) ) ;
#13006 = ORIENTED_EDGE ( 'NONE', *, *, #22350, .T. ) ;
#13007 = LINE ( 'NONE', #30768, #37263 ) ;
#13008 = CARTESIAN_POINT ( 'NONE',  ( -0.07405724077823318263, -0.5442913385289138706, 0.1787899950787401604 ) ) ;
#13009 = CARTESIAN_POINT ( 'NONE',  ( -0.2741778990008359451, -0.1449014624352428227, 0.9603494317905525435 ) ) ;
#13010 = ORIENTED_EDGE ( 'NONE', *, *, #10725, .T. ) ;
#13011 = CARTESIAN_POINT ( 'NONE',  ( 0.6971942568897637749, 2.189545951927499583E-17, 1.459153543253322693 ) ) ;
#13012 = EDGE_CURVE ( 'NONE', #27963, #23901, #22470, .T. ) ;
#13013 = CARTESIAN_POINT ( 'NONE',  ( -0.1225179410722563866, 0.2247584660037810489, -0.3149606299212600047 ) ) ;
#13014 = CARTESIAN_POINT ( 'NONE',  ( -0.1787899950787401882, -0.3597440944344256208, 0.000000000000000000 ) ) ;
#13015 = CARTESIAN_POINT ( 'NONE',  ( 0.1787899950787401604, -0.7263779527021420046, -0.07405724077823318263 ) ) ;
#13016 = VECTOR ( 'NONE', #27338, 39.37007874015748854 ) ;
#13017 = CARTESIAN_POINT ( 'NONE',  ( 0.000000000000000000, 0.000000000000000000, -0.06545654452343109553 ) ) ;
#13018 = FACE_OUTER_BOUND ( 'NONE', #11961, .T. ) ;
#13019 = CARTESIAN_POINT ( 'NONE',  ( 0.8759842519685039353, 0.1787899950787401882, 1.606791338528913426 ) ) ;
#13020 = CARTESIAN_POINT ( 'NONE',  ( 0.1787899950787401882, 0.08206107114083996401, -2.189545951927503898E-17 ) ) ;
#13021 = CARTESIAN_POINT ( 'NONE',  ( 3.284318927891251994E-17, -1.801673228292693052, 0.1787899950787401882 ) ) ;
#13022 = SHAPE_DEFINITION_REPRESENTATION ( #11952, #4677 ) ;
#13023 = DIRECTION ( 'NONE',  ( 0.5735764363510447161, 0.8191520442889925757, 0.000000000000000000 ) ) ;
#13024 = CARTESIAN_POINT ( 'NONE',  ( 0.9500414927467378812, 0.1787899950787401604, 0.5019685038832442103 ) ) ;
#13025 = DIMENSIONAL_EXPONENTS ( 1.000000000000000000, 0.000000000000000000, 0.000000000000000000, 0.000000000000000000, 0.000000000000000000, 0.000000000000000000, 0.000000000000000000 ) ;
#13026 = CIRCLE ( 'NONE', #35997, 0.09842519685039370636 ) ;
#13027 = CARTESIAN_POINT ( 'NONE',  ( -0.8019270111902716547, -0.1787899950787401604, 0.8809055117572600624 ) ) ;
#13029 = CARTESIAN_POINT ( 'NONE',  ( 0.5660731898098425585, 4.766607801171850497E-17, 0.000000000000000000 ) ) ;
#13028 = CARTESIAN_POINT ( 'NONE',  ( -0.1574803149606297803, -0.9699803149606308628, 0.06523048226347956391 ) ) ;
#13030 = B_SPLINE_CURVE_WITH_KNOTS ( 'NONE', 3,
 ( #22169, #30519, #23307, #8919, #9156, #23066, #23547, #3959, #44208, #19698, #11408, #36807, #34113, #26026, #36573, #120, #34565, #37684, #45552, #12772, #15896, #37924 ),
 .UNSPECIFIED., .F., .F.,
 ( 4, 1, 1, 1, 1, 1, 1, 2, 2, 1, 1, 1, 1, 2, 2, 4 ),
 ( 0.000000000000000000, 0.2499999999999965028, 0.3749999999999947820, 0.4374999999999938938, 0.4687499999999934497, 0.4843749999999932276, 0.4921874999999932832, 0.4960937499999931721, 0.4999999999999930056, 0.6249999999999954481, 0.6874999999999966693, 0.7187499999999973355, 0.7343749999999976685, 0.7421874999999977796, 0.7499999999999978906, 1.000000000000000000 ),
 .UNSPECIFIED. ) ;
#13032 = CARTESIAN_POINT ( 'NONE',  ( -0.8493927667999465747, -0.1716682518494001275, 1.987719807708568709 ) ) ;
#13031 = CARTESIAN_POINT ( 'NONE',  ( -0.1270800023317771588, -1.502012313520053155, -0.1270800023317771588 ) ) ;
#13033 = CARTESIAN_POINT ( 'NONE',  ( -1.094772975963752103E-17, -0.3646653542769452971, -0.1787899950787401882 ) ) ;
#13034 = CARTESIAN_POINT ( 'NONE',  ( -1.033464566929134687, -0.06523048226347956391, 1.257381889656253193 ) ) ;
#13035 = CARTESIAN_POINT ( 'NONE',  ( 1.002407869896990045, 0.1264236179284866091, 1.449311023568283341 ) ) ;
#13036 = CARTESIAN_POINT ( 'NONE',  ( 0.1888124183976733761, 0.07899857248962396938, -0.1764221702779007750 ) ) ;
#13037 = CARTESIAN_POINT ( 'NONE',  ( 0.9500414927467377701, 0.1787899950787401604, 0.4232283464029293896 ) ) ;
#13038 = DIRECTION ( 'NONE',  ( 1.822029033848725028E-16, 0.000000000000000000, 1.000000000000000000 ) ) ;
#13039 = CARTESIAN_POINT ( 'NONE',  ( 0.8107537697050254399, -0.1574803149606297803, 0.8538385825696385156 ) ) ;
#13040 = CARTESIAN_POINT ( 'NONE',  ( 0.000000000000000000, 0.000000000000000000, -0.3149606299212598381 ) ) ;
#13041 = CARTESIAN_POINT ( 'NONE',  ( 0.1787899950787401882, 0.01427165359707061217, -2.189545951927503898E-17 ) ) ;
#13042 = CARTESIAN_POINT ( 'NONE',  ( 0.8107537697050254399, -0.1574803149606297803, 0.4995078739082208230 ) ) ;
#13043 = CARTESIAN_POINT ( 'NONE',  ( 0.8019270111902717657, 0.1787899950787401604, 0.3887795275052913224 ) ) ;
#13044 = CARTESIAN_POINT ( 'NONE',  ( 0.8314340917992454338, -0.1542392197562734157, 0.03937235152828252871 ) ) ;
#13046 = DIRECTION ( 'NONE',  ( -1.000000000000000000, 0.000000000000000000, 0.000000000000000000 ) ) ;
#13045 = CARTESIAN_POINT ( 'NONE',  ( 1.054774247047244540, -0.07405724077823318263, 1.318897637741511364 ) ) ;
#13047 = LINE ( 'NONE', #6464, #20243 ) ;
#13048 = CARTESIAN_POINT ( 'NONE',  ( -1.054774247047244540, 0.07405724077823318263, 1.481299212544662680 ) ) ;
#13049 = CARTESIAN_POINT ( 'NONE',  ( 0.9873396505805591694, -0.1113553986120547346, 0.7431102361129447997 ) ) ;
#13050 = EDGE_LOOP ( 'NONE', ( #19829, #2078, #34637, #40438, #36100 ) ) ;
#13051 = CYLINDRICAL_SURFACE ( 'NONE', #25305, 0.1574803149606299191 ) ;
#13052 = CARTESIAN_POINT ( 'NONE',  ( 0.8019270111902717657, 0.1787899950787401604, 1.023622047190330342 ) ) ;
#13053 = CARTESIAN_POINT ( 'NONE',  ( 3.284318927891251994E-17, -1.294783464513165283, 0.1787899950787401882 ) ) ;
#13054 = CARTESIAN_POINT ( 'NONE',  ( -0.7185039370078746268, 0.06523048226347956391, 0.6077755904436538126 ) ) ;
#13055 = DIRECTION ( 'NONE',  ( 1.822029033848725028E-16, 0.000000000000000000, 1.000000000000000000 ) ) ;
#13056 = CARTESIAN_POINT ( 'NONE',  ( 1.054774247047244540, 0.07405724077823318263, 1.678149606245448622 ) ) ;
#13057 = CARTESIAN_POINT ( 'NONE',  ( -0.9873396505805591694, -0.1113553986120547346, 1.422244094488188892 ) ) ;
#13058 = CARTESIAN_POINT ( 'NONE',  ( 0.7646288533564489232, -0.1113553986120547346, 1.796259842412157415 ) ) ;
#13060 = CARTESIAN_POINT ( 'NONE',  ( -0.7504702239987475210, -0.1105241597664997355, 0.03937007874015843734 ) ) ;
#13059 = CYLINDRICAL_SURFACE ( 'NONE', #9689, 0.1574803149606299191 ) ;
#13061 = CARTESIAN_POINT ( 'NONE',  ( 0.6971942568897626646, -0.07405724077823297447, 0.2066929133320631329 ) ) ;
#13062 = CARTESIAN_POINT ( 'NONE',  ( -1.002407869896990045, -0.1264236179284866091, 0.09596456687537027741 ) ) ;
#13063 = CARTESIAN_POINT ( 'NONE',  ( 0.8107537697050253289, 0.1574803149606300301, 1.390255905404285119 ) ) ;
#13064 = VERTEX_POINT ( 'NONE', #11003 ) ;
#13065 = EDGE_LOOP ( 'NONE', ( #14869, #20884, #13252, #10151 ) ) ;
#13066 = CIRCLE ( 'NONE', #35986, 0.7874015748031496509 ) ;
#13067 = DIRECTION ( 'NONE',  ( -0.5000000000000003331, 0.8660254037844384856, 0.000000000000000000 ) ) ;
#13068 = CARTESIAN_POINT ( 'NONE',  ( -0.03026318032628478802, -0.09782597982458868247, 0.1548971533202315731 ) ) ;
#13069 = CARTESIAN_POINT ( 'NONE',  ( 0.9500414927467378812, 0.1787899950787401604, 0.7037401574265510495 ) ) ;
#13070 = ADVANCED_FACE ( 'NONE', ( #7393 ), #18408, .F. ) ;
#13071 = CARTESIAN_POINT ( 'NONE',  ( -1.054774247047244540, -0.07405724077823318263, 1.633858267662771091 ) ) ;
#13072 = CARTESIAN_POINT ( 'NONE',  ( -0.1574803149606297803, -0.2514763778452289711, 0.06523048226347956391 ) ) ;
#13073 = ORIENTED_EDGE ( 'NONE', *, *, #34714, .T. ) ;
#13074 = VECTOR ( 'NONE', #6883, 39.37007874015748143 ) ;
#13075 = AXIS2_PLACEMENT_3D ( 'NONE', #40813, #33691, #12104 ) ;
#13076 = ORIENTED_EDGE ( 'NONE', *, *, #8911, .T. ) ;
#13077 = EDGE_CURVE ( 'NONE', #2020, #47303, #11418, .T. ) ;
#13078 = DIRECTION ( 'NONE',  ( 0.000000000000000000, 0.8660254037844383745, 0.5000000000000003331 ) ) ;
#13079 = CARTESIAN_POINT ( 'NONE',  ( -0.9873396505805591694, -0.1113553986120547346, 0.7923228346456693272 ) ) ;
#13080 = CARTESIAN_POINT ( 'NONE',  ( 0.07405724077823318263, -1.131029480040261603, -0.1787899950787401604 ) ) ;
#13081 = VERTEX_POINT ( 'NONE', #22003 ) ;
#13082 = CARTESIAN_POINT ( 'NONE',  ( -0.1787899950787401882, -0.1579724408911182820, 0.000000000000000000 ) ) ;
#13083 = VERTEX_POINT ( 'NONE', #18177 ) ;
#13084 = ORIENTED_EDGE ( 'NONE', *, *, #29179, .T. ) ;
#13085 = EDGE_CURVE ( 'NONE', #42441, #17962, #41191, .T. ) ;
#13086 = CARTESIAN_POINT ( 'NONE',  ( -1.033464566929133799, 0.000000000000000000, 1.417322834538141674 ) ) ;
#13087 = EDGE_CURVE ( 'NONE', #47237, #42416, #21013, .T. ) ;
#13088 = CARTESIAN_POINT ( 'NONE',  ( 1.033464566929133799, 0.000000000000000000, 1.820866141732283561 ) ) ;
#13089 = CARTESIAN_POINT ( 'NONE',  ( 3.284318927891251994E-17, -0.5861220471903307860, 0.1787899950787401882 ) ) ;
#13090 = CONICAL_SURFACE ( 'NONE', #24554, 0.08090551181102362266, 0.9599310885968742602 ) ;
#13091 = CARTESIAN_POINT ( 'NONE',  ( -1.054774247047244096, 0.000000000000000000, 0.3026574802611972648 ) ) ;
#13092 = CARTESIAN_POINT ( 'NONE',  ( -0.8107537697050253289, -0.1574803149606297803, 1.021161417322834497 ) ) ;
#13093 = CARTESIAN_POINT ( 'NONE',  ( -1.100456976456230270E-17, -1.113232785960998061, -0.1797182628040039365 ) ) ;
#13094 = CARTESIAN_POINT ( 'NONE',  ( 0.8759842519685039353, 0.000000000000000000, 4.498031496062992574 ) ) ;
#13095 = CARTESIAN_POINT ( 'NONE',  ( 0.6971942568897637749, 2.189545951927499583E-17, 1.070374015694267600 ) ) ;
#13096 = AXIS2_PLACEMENT_3D ( 'NONE', #10448, #6824, #36071 ) ;
#13097 = CARTESIAN_POINT ( 'NONE',  ( 0.5717220857807087109, 4.466152701071653354E-17, 0.000000000000000000 ) ) ;
#13098 = CARTESIAN_POINT ( 'NONE',  ( 1.033464566929133799, 0.000000000000000000, 1.584645669291338654 ) ) ;
#13100 = CARTESIAN_POINT ( 'NONE',  ( -0.8418157620803491392, 0.1549362366669437274, 1.979014853567908627 ) ) ;
#13099 = DIRECTION ( 'NONE',  ( -0.000000000000000000, 0.2432573283306645462, -0.9699617890481188054 ) ) ;
#13102 = CARTESIAN_POINT ( 'NONE',  ( 0.9873396505805591694, -0.1113553986120547346, 1.451771653435779408 ) ) ;
#13101 = CIRCLE ( 'NONE', #23786, 0.1574803149606300579 ) ;
#13103 = DIRECTION ( 'NONE',  ( -1.000000000000000000, 0.000000000000000000, 0.000000000000000000 ) ) ;
#13104 = CARTESIAN_POINT ( 'NONE',  ( 0.03556354040786432330, 0.1286422661082892160, 0.1787899950787401604 ) ) ;
#13105 = DIRECTION ( 'NONE',  ( -1.000000000000000000, 3.469446951953614189E-15, 0.000000000000000000 ) ) ;
#13106 = CARTESIAN_POINT ( 'NONE',  ( 0.6971942568897648851, 0.07405724077823318263, 0.9055118109698584439 ) ) ;
#13107 = CARTESIAN_POINT ( 'NONE',  ( 0.8759842519685039353, 0.1787899950787401882, 1.926673228292693052 ) ) ;
#13108 = CARTESIAN_POINT ( 'NONE',  ( -0.6971942568897637749, 2.189545951927499583E-17, 1.144192913332062966 ) ) ;
#13109 = CARTESIAN_POINT ( 'NONE',  ( 1.033464566929134687, 0.06523048226347956391, 0.3961614172153076763 ) ) ;
#13110 = ORIENTED_EDGE ( 'NONE', *, *, #3191, .F. ) ;
#13111 = CARTESIAN_POINT ( 'NONE',  ( 0.4330708661417322913, 0.000000000000000000, 0.9891732283464564901 ) ) ;
#13112 = CARTESIAN_POINT ( 'NONE',  ( 0.9412147342319837628, -0.1574803149606297803, 1.892224409448819866 ) ) ;
#13113 = CARTESIAN_POINT ( 'NONE',  ( 0.1574803149606299191, -1.612204724301921077, -1.928577636452523993E-17 ) ) ;
#13114 = CARTESIAN_POINT ( 'NONE',  ( -1.033464566929134687, -0.06523048226347956391, 0.3124999998924728462 ) ) ;
#13115 = CARTESIAN_POINT ( 'NONE',  ( 0.008625679036560286728, -0.1524122562640881362, 0.01160289892419911692 ) ) ;
#13116 = EDGE_CURVE ( 'NONE', #8447, #30501, #1843, .T. ) ;
#13117 = ORIENTED_EDGE ( 'NONE', *, *, #29800, .F. ) ;
#13118 = CARTESIAN_POINT ( 'NONE',  ( 0.05938635157346154603, -0.07958416565547918320, 0.2511462791696609798 ) ) ;
#13119 = CARTESIAN_POINT ( 'NONE',  ( 0.1787899950787401882, 0.05856299217974772486, -2.189545951927503898E-17 ) ) ;
#13120 = CARTESIAN_POINT ( 'NONE',  ( 0.8759842519685039353, 0.000000000000000000, 4.498031496062992574 ) ) ;
#13121 = EDGE_CURVE ( 'NONE', #26635, #36995, #41838, .T. ) ;
#13122 = CARTESIAN_POINT ( 'NONE',  ( -0.8019270111902717657, 0.1787899950787401604, 0.6249999999462366729 ) ) ;
#13123 = PLANE ( 'NONE',  #25236 ) ;
#13124 = CARTESIAN_POINT ( 'NONE',  ( -0.08443540605192620396, 0.09133345722616742490, 0.2366842664529267282 ) ) ;
#13125 = EDGE_CURVE ( 'NONE', #5872, #30632, #18292, .T. ) ;
#13126 = ORIENTED_EDGE ( 'NONE', *, *, #16477, .T. ) ;
#13128 = CARTESIAN_POINT ( 'NONE',  ( 0.1264236179284866091, -1.634350393647023614, -0.1264236179284866091 ) ) ;
#13127 = CARTESIAN_POINT ( 'NONE',  ( 0.1113553986120547346, -0.3966535431995590888, 0.1113553986120547346 ) ) ;
#13129 = CARTESIAN_POINT ( 'NONE',  ( -0.8759842519685039353, 0.1574803149606299191, 0.05905511811023622659 ) ) ;
#13130 = VERTEX_POINT ( 'NONE', #19106 ) ;
#13131 = CARTESIAN_POINT ( 'NONE',  ( -1.002407869896990045, -0.1264236179284866091, 0.6520669290800944484 ) ) ;
#13132 = VERTEX_POINT ( 'NONE', #16017 ) ;
#13133 = ( BOUNDED_CURVE ( )  B_SPLINE_CURVE ( 2, ( #11384, #25997, #33445, #560, #22632, #45837, #8960, #9194, #1512 ),
 .UNSPECIFIED., .F., .F. ) 
 B_SPLINE_CURVE_WITH_KNOTS ( ( 3, 2, 2, 2, 3 ),
 ( 0.8599999999999999867, 0.8625000000000000444, 0.8649999999999999911, 0.8675000000000000488, 0.8699999999999999956 ),
 .UNSPECIFIED. ) 
 CURVE ( )  GEOMETRIC_REPRESENTATION_ITEM ( )  RATIONAL_B_SPLINE_CURVE ( ( 1.000000000000000000, 0.9238795325112869605, 1.000000000000000000, 0.9238795325112869605, 1.000000000000000000, 0.9238795325112869605, 1.000000000000000000, 0.9238795325112869605, 1.000000000000000000 ) ) 
 REPRESENTATION_ITEM ( '' )  ) ;
#13134 = VECTOR ( 'NONE', #34138, 39.37007874015748143 ) ;
#13135 = LINE ( 'NONE', #6376, #32082 ) ;
#13136 = CARTESIAN_POINT ( 'NONE',  ( -0.1264236179284866091, -0.6512066453945926092, -0.1264236179284866091 ) ) ;
#13137 = ORIENTED_EDGE ( 'NONE', *, *, #40601, .F. ) ;
#13138 = CARTESIAN_POINT ( 'NONE',  ( 0.2030945033354783491, -0.08956025807989388687, 0.03023235614309822961 ) ) ;
#13139 = DIRECTION ( 'NONE',  ( 0.8191520442889893561, -0.4519843998600455715, 0.3531289150159241386 ) ) ;
#13140 = DIRECTION ( 'NONE',  ( 1.000000000000000000, 0.000000000000000000, 0.000000000000000000 ) ) ;
#13141 = CARTESIAN_POINT ( 'NONE',  ( -1.002407869896990045, 0.1264236179284866091, 0.4207677164816693294 ) ) ;
#13142 = CYLINDRICAL_SURFACE ( 'NONE', #16946, 0.09842519685039370636 ) ;
#13143 = ORIENTED_EDGE ( 'NONE', *, *, #36841, .T. ) ;
#13144 = EDGE_CURVE ( 'NONE', #47403, #3012, #26568, .T. ) ;
#13145 = CARTESIAN_POINT ( 'NONE',  ( -1.054774247047244540, -0.07405724077823318263, 1.717519684985606476 ) ) ;
#13146 = CARTESIAN_POINT ( 'NONE',  ( 0.000000000000000000, 0.000000000000000000, -0.3149606299212598381 ) ) ;
#13147 = ( BOUNDED_CURVE ( )  B_SPLINE_CURVE ( 2, ( #45157, #5154, #16435, #34893, #31066, #35118, #27715, #34406, #13086 ),
 .UNSPECIFIED., .F., .F. ) 
 B_SPLINE_CURVE_WITH_KNOTS ( ( 3, 2, 2, 2, 3 ),
 ( 0.6899999999999999467, 0.6925000000000000044, 0.6949999999999999512, 0.6975000000000000089, 0.6999999999999999556 ),
 .UNSPECIFIED. ) 
 CURVE ( )  GEOMETRIC_REPRESENTATION_ITEM ( )  RATIONAL_B_SPLINE_CURVE ( ( 1.000000000000000000, 0.9238795325112939549, 1.000000000000000000, 0.9238795325112869605, 1.000000000000000000, 0.9238795325112869605, 1.000000000000000000, 0.9238795325112829637, 1.000000000000000000 ) ) 
 REPRESENTATION_ITEM ( '' )  ) ;
#13148 = CARTESIAN_POINT ( 'NONE',  ( -0.7185039370078746268, 0.06523048226347977208, 0.1353346455617644717 ) ) ;
#13149 = CARTESIAN_POINT ( 'NONE',  ( 1.181102362204724310, -0.3937007874015748254, 0.9842519685039370358 ) ) ;
#13150 = CARTESIAN_POINT ( 'NONE',  ( 0.7646288533564489232, 0.1113553986120547346, 0.5757874015748032370 ) ) ;
#13151 = CARTESIAN_POINT ( 'NONE',  ( -0.07444174185955065859, -0.7564414473783218629, -0.1797182628040039087 ) ) ;
#13152 = CARTESIAN_POINT ( 'NONE',  ( 0.2471922904502826812, 0.09572725253288333347, 0.02812286105088213084 ) ) ;
#13153 = ( BOUNDED_CURVE ( )  B_SPLINE_CURVE ( 2, ( #40579, #44887, #4167, #8478, #4391, #8245, #22634, #14742, #12099 ),
 .UNSPECIFIED., .F., .F. ) 
 B_SPLINE_CURVE_WITH_KNOTS ( ( 3, 2, 2, 2, 3 ),
 ( 0.4600000000000000200, 0.4625000000000000222, 0.4650000000000000244, 0.4675000000000000266, 0.4699999999999999734 ),
 .UNSPECIFIED. ) 
 CURVE ( )  GEOMETRIC_REPRESENTATION_ITEM ( )  RATIONAL_B_SPLINE_CURVE ( ( 1.000000000000000000, 0.9238795325112869605, 1.000000000000000000, 0.9238795325112869605, 1.000000000000000000, 0.9238795325112869605, 1.000000000000000000, 0.9238795325112849621, 1.000000000000000000 ) ) 
 REPRESENTATION_ITEM ( '' )  ) ;
#13154 = CARTESIAN_POINT ( 'NONE',  ( -0.9873396505805591694, -0.1113553986120547346, 1.215551180994834723 ) ) ;
#13156 = CARTESIAN_POINT ( 'NONE',  ( -0.8759842519685039353, 0.1574803149606299191, 0.6791338581601890079 ) ) ;
#13155 = CARTESIAN_POINT ( 'NONE',  ( -0.1574803149606300301, -0.4630905511811017616, -0.06523048226347956391 ) ) ;
#13157 = CARTESIAN_POINT ( 'NONE',  ( -0.9873396505805591694, 0.1113553986120547346, 0.4084645669291339098 ) ) ;
#13158 = VERTEX_POINT ( 'NONE', #9043 ) ;
#13159 = CARTESIAN_POINT ( 'NONE',  ( 0.1574803149606300301, 0.03395669291338582890, -0.06523048226347956391 ) ) ;
#13160 = CARTESIAN_POINT ( 'NONE',  ( 0.7185039370078746268, -0.06523048226347956391, 1.094980314960628975 ) ) ;
#13162 = CARTESIAN_POINT ( 'NONE',  ( -0.7185039370078739607, 1.928577636452523993E-17, 1.328740157480315043 ) ) ;
#13161 = DIRECTION ( 'NONE',  ( 0.000000000000000000, 0.000000000000000000, -1.000000000000000000 ) ) ;
#13163 = LINE ( 'NONE', #45232, #22817 ) ;
#13164 = CIRCLE ( 'NONE', #34590, 0.2471922904502826812 ) ;
#13166 = DIRECTION ( 'NONE',  ( 0.000000000000000000, -0.7880107536067206819, 0.6156614753256598460 ) ) ;
#13165 = DIRECTION ( 'NONE',  ( -3.469446951953612217E-15, -1.000000000000000000, 0.000000000000000000 ) ) ;
#13167 = CARTESIAN_POINT ( 'NONE',  ( 0.1264236179284866091, -0.5270669290800944484, -0.1264236179284866091 ) ) ;
#13168 = EDGE_LOOP ( 'NONE', ( #5004, #40027, #37328, #45512 ) ) ;
#13169 = CIRCLE ( 'NONE', #39916, 0.1377952755905509086 ) ;
#13170 = VECTOR ( 'NONE', #44642, 39.37007874015748143 ) ;
#13171 = CARTESIAN_POINT ( 'NONE',  ( 1.054774247047244540, -0.07405724077823318263, 0.8070866141194653620 ) ) ;
#13172 = EDGE_CURVE ( 'NONE', #23076, #23848, #1428, .T. ) ;
#13173 = DIRECTION ( 'NONE',  ( 1.822029033848725028E-16, 0.000000000000000000, 1.000000000000000000 ) ) ;
#13174 = CARTESIAN_POINT ( 'NONE',  ( 0.07405724077823318263, -1.641732283410802573, 0.1787899950787401604 ) ) ;
#13175 = CARTESIAN_POINT ( 'NONE',  ( 0.1264236179284866091, -1.122539370024976391, -0.1264236179284866091 ) ) ;
#13176 = CARTESIAN_POINT ( 'NONE',  ( -0.1574803149606299191, -1.444881889763779625, 0.000000000000000000 ) ) ;
#13177 = ADVANCED_FACE ( 'NONE', ( #38272 ), #20056, .T. ) ;
#13178 = CARTESIAN_POINT ( 'NONE',  ( -0.9873396505805591694, 0.1113553986120547346, 1.392716535433070835 ) ) ;
#13179 = ORIENTED_EDGE ( 'NONE', *, *, #37662, .T. ) ;
#13180 = CARTESIAN_POINT ( 'NONE',  ( -0.8759842519685039353, 0.1787899950787401882, 1.887303149552535420 ) ) ;
#13181 = EDGE_CURVE ( 'NONE', #25968, #23819, #18987, .T. ) ;
#13182 = CARTESIAN_POINT ( 'NONE',  ( 1.002407869896990045, 0.1264236179284866091, 1.843011810969858333 ) ) ;
#13183 = ORIENTED_EDGE ( 'NONE', *, *, #44180, .F. ) ;
#13184 = LINE ( 'NONE', #31633, #39386 ) ;
#13185 = CARTESIAN_POINT ( 'NONE',  ( -0.8019270111902717657, -0.1787899950787401604, 1.584645669237574994 ) ) ;
#13186 = EDGE_CURVE ( 'NONE', #28190, #34488, #39672, .T. ) ;
#13187 = CARTESIAN_POINT ( 'NONE',  ( -1.054774247047244540, 0.07405724077823318263, 0.2657480314422993595 ) ) ;
#13188 = CARTESIAN_POINT ( 'NONE',  ( -0.9412147342319837628, 0.1574803149606300301, 0.5684055118110233895 ) ) ;
#13189 = CARTESIAN_POINT ( 'NONE',  ( -0.6971942568897637749, 2.189545951927499583E-17, 1.779035433017102319 ) ) ;
#13190 = CARTESIAN_POINT ( 'NONE',  ( 0.05264611394417172130, -0.07553294269950974749, -0.2550375247538704815 ) ) ;
#13191 = CARTESIAN_POINT ( 'NONE',  ( -1.033464566929134687, 0.06523048226347956391, 1.705216535433070613 ) ) ;
#13192 = CARTESIAN_POINT ( 'NONE',  ( 0.2559035040615164069, 0.02868498164184919361, -0.03078275702940447625 ) ) ;
#13193 = CARTESIAN_POINT ( 'NONE',  ( -0.1264236179284866091, -0.2082932595678216314, 0.1264236179284866091 ) ) ;
#13194 = CARTESIAN_POINT ( 'NONE',  ( 0.9500414927467377701, 0.1787899950787401604, 1.727362204670645385 ) ) ;
#13195 = CARTESIAN_POINT ( 'NONE',  ( -0.04516133130590834627, -0.09842519685039370636, -0.1820366505350590747 ) ) ;
#13196 = CARTESIAN_POINT ( 'NONE',  ( 0.4330708661417325689, 0.1574803149606300301, -1.186023622047243986 ) ) ;
#13197 = CYLINDRICAL_SURFACE ( 'NONE', #46376, 0.1574803149606299191 ) ;
#13198 = CIRCLE ( 'NONE', #23883, 0.1574803149606299191 ) ;
#13199 = VECTOR ( 'NONE', #38781, 39.37007874015748143 ) ;
#13200 = ORIENTED_EDGE ( 'NONE', *, *, #1287, .F. ) ;
#13201 = VERTEX_POINT ( 'NONE', #41593 ) ;
#13202 = AXIS2_PLACEMENT_3D ( 'NONE', #6257, #43389, #24264 ) ;
#13203 = CIRCLE ( 'NONE', #45310, 0.09940944881889761386 ) ;
#13204 = CARTESIAN_POINT ( 'NONE',  ( -0.07405724077823318263, -1.021653543253323138, 0.1787899950787401604 ) ) ;
#13205 = CARTESIAN_POINT ( 'NONE',  ( -0.1787899950787401882, -1.260334645615527549, 0.000000000000000000 ) ) ;
#13206 = CARTESIAN_POINT ( 'NONE',  ( -1.033464566929133799, 0.000000000000000000, 1.181102362097196989 ) ) ;
#13207 = CARTESIAN_POINT ( 'NONE',  ( -0.1270800023317771588, -0.5079178253310770996, 0.1270800023317771588 ) ) ;
#13208 = CARTESIAN_POINT ( 'NONE',  ( -0.9873396505805591694, -0.1113553986120547346, 0.8612204723334173639 ) ) ;
#13209 = AXIS2_PLACEMENT_3D ( 'NONE', #36601, #36379, #36836 ) ;
#13210 = CARTESIAN_POINT ( 'NONE',  ( -0.1113553986120547346, -0.02263779527559055260, 0.1113553986120547346 ) ) ;
#13211 = CARTESIAN_POINT ( 'NONE',  ( 0.8759842519685039353, -0.1787899950787401882, 0.9965551180564724554 ) ) ;
#13212 = CARTESIAN_POINT ( 'NONE',  ( 0.7185039370078746268, -0.06523048226347956391, 1.085137795168063191 ) ) ;
#13213 = CARTESIAN_POINT ( 'NONE',  ( 0.8019270111902717657, 0.1787899950787401604, 1.929133858213952335 ) ) ;
#13214 = ORIENTED_EDGE ( 'NONE', *, *, #30555, .F. ) ;
#13215 = COLOUR_RGB ( '', 0.66274510, 0.83137255, 0.94901961) ;
#13216 = CYLINDRICAL_SURFACE ( 'NONE', #42020, 0.1574803149606299191 ) ;
#13218 = CARTESIAN_POINT ( 'NONE',  ( 0.07405724077823318263, -0.6476377952218281830, -0.1787899950787401604 ) ) ;
#13217 = CARTESIAN_POINT ( 'NONE',  ( 0.1574803149606299191, -0.9822834644594016229, -1.928577636452523993E-17 ) ) ;
#13219 = CARTESIAN_POINT ( 'NONE',  ( -0.07405724077823318263, -1.385826771599779184, -0.1787899950787401604 ) ) ;
#13220 = CARTESIAN_POINT ( 'NONE',  ( 0.8759842519685039353, -0.1787899950787401882, 0.3715551180564728440 ) ) ;
#13221 = EDGE_CURVE ( 'NONE', #18450, #33511, #42079, .T. ) ;
#13222 = CIRCLE ( 'NONE', #33938, 0.09842519685039370636 ) ;
#13223 = CARTESIAN_POINT ( 'NONE',  ( -0.9500414927467378812, 0.1787899950787401604, 1.958661417269071947 ) ) ;
#13224 = ORIENTED_EDGE ( 'NONE', *, *, #14016, .F. ) ;
#13225 = ORIENTED_EDGE ( 'NONE', *, *, #12430, .T. ) ;
#13226 = CARTESIAN_POINT ( 'NONE',  ( -1.002407869896990045, 0.1264236179284866091, 1.528051181048598384 ) ) ;
#13227 = ADVANCED_FACE ( 'NONE', ( #45442 ), #7570, .F. ) ;
#13228 = CARTESIAN_POINT ( 'NONE',  ( 1.054774247047244096, 0.000000000000000000, 1.405019684985606476 ) ) ;
#13229 = FACE_OUTER_BOUND ( 'NONE', #38520, .T. ) ;
#13230 = CARTESIAN_POINT ( 'NONE',  ( -1.054774247047244540, 0.07405724077823318263, 0.6594488188438737408 ) ) ;
#13231 = VECTOR ( 'NONE', #45769, 39.37007874015748143 ) ;
#13232 = CARTESIAN_POINT ( 'NONE',  ( 1.002407869896990045, 0.1264236179284866091, 0.07135826766277185429 ) ) ;
#13233 = EDGE_CURVE ( 'NONE', #39665, #25724, #8560, .T. ) ;
#13234 = CARTESIAN_POINT ( 'NONE',  ( 0.1545837415703855688, -0.09842296937465562501, -0.08999940835115426141 ) ) ;
#13235 = DIRECTION ( 'NONE',  ( 1.000000000000000000, 0.000000000000000000, 0.000000000000000000 ) ) ;
#13236 = CARTESIAN_POINT ( 'NONE',  ( 0.7495606340400177148, -0.1264236179284866091, 0.6815944881352126172 ) ) ;
#13237 = CARTESIAN_POINT ( 'NONE',  ( -0.6971942568897637749, 2.189545951927499583E-17, 0.5536417322297008115 ) ) ;
#13238 = CARTESIAN_POINT ( 'NONE',  ( 0.1850388559544986211, -0.08126078924503041256, 0.1786007880588302565 ) ) ;
#13239 = CARTESIAN_POINT ( 'NONE',  ( 0.1113553986120547346, -0.08169291338582677919, -0.1113553986120547346 ) ) ;
#13240 = ORIENTED_EDGE ( 'NONE', *, *, #2963, .T. ) ;
#13241 = CARTESIAN_POINT ( 'NONE',  ( -0.2471922904502826812, 0.09842519685039370636, 5.914624404477007554E-17 ) ) ;
#13242 = CARTESIAN_POINT ( 'NONE',  ( -0.7646288533564489232, 0.1113553986120547346, 0.3395669291338583307 ) ) ;
#13243 = CARTESIAN_POINT ( 'NONE',  ( -0.08394057657693032581, -0.09851384873590177116, 0.2125522580681921125 ) ) ;
#13244 = LINE ( 'NONE', #479, #18735 ) ;
#13245 = ORIENTED_EDGE ( 'NONE', *, *, #34990, .F. ) ;
#13246 = CARTESIAN_POINT ( 'NONE',  ( -0.6971942568897637749, 2.189545951927499583E-17, 0.9522637794737952577 ) ) ;
#13247 = CARTESIAN_POINT ( 'NONE',  ( 0.07405724077823318263, -1.578864125709555477, 0.1787899950787401604 ) ) ;
#13248 = ORIENTED_EDGE ( 'NONE', *, *, #6648, .T. ) ;
#13249 = CARTESIAN_POINT ( 'NONE',  ( -1.033464566929133799, 0.000000000000000000, 1.377952755797984263 ) ) ;
#13250 = CARTESIAN_POINT ( 'NONE',  ( -0.1787899950787401604, -0.5492125983714331028, 0.07405724077823318263 ) ) ;
#13251 = FACE_OUTER_BOUND ( 'NONE', #4397, .T. ) ;
#13252 = ORIENTED_EDGE ( 'NONE', *, *, #43149, .T. ) ;
#13253 = EDGE_CURVE ( 'NONE', #3083, #22876, #34450, .T. ) ;
#13254 = ( BOUNDED_CURVE ( )  B_SPLINE_CURVE ( 2, ( #44799, #34517, #16318, #30946, #45508, #19414, #23733, #33831, #38337 ),
 .UNSPECIFIED., .F., .T. ) 
 B_SPLINE_CURVE_WITH_KNOTS ( ( 3, 2, 2, 2, 3 ),
 ( 0.9000000000000000222, 0.9024999999999999689, 0.9050000000000000266, 0.9074999999999999734, 0.9100000000000000311 ),
 .UNSPECIFIED. ) 
 CURVE ( )  GEOMETRIC_REPRESENTATION_ITEM ( )  RATIONAL_B_SPLINE_CURVE ( ( 1.000000000000000000, 0.9238795325112869605, 1.000000000000000000, 0.9238795325112869605, 1.000000000000000000, 0.9238795325112869605, 1.000000000000000000, 0.9238795325112869605, 1.000000000000000000 ) ) 
 REPRESENTATION_ITEM ( '' )  ) ;
#13255 = CARTESIAN_POINT ( 'NONE',  ( -0.1787899950787401604, -0.7066929133320629663, 0.07405724077823318263 ) ) ;
#13256 = VECTOR ( 'NONE', #46558, 39.37007874015748143 ) ;
#13257 = CYLINDRICAL_SURFACE ( 'NONE', #24915, 0.09842519685039310962 ) ;
#13258 = CARTESIAN_POINT ( 'NONE',  ( 0.7646288533564489232, 0.1113553986120547346, 1.432086614065700925 ) ) ;
#13259 = CARTESIAN_POINT ( 'NONE',  ( 0.8019270111902717657, -0.1787899950787401604, 0.2460629920722207375 ) ) ;
#13260 = AXIS2_PLACEMENT_3D ( 'NONE', #7868, #657, #36876 ) ;
#13261 = CONICAL_SURFACE ( 'NONE', #35467, 0.1377952755905510751, 0.9599310885968951323 ) ;
#13262 = CARTESIAN_POINT ( 'NONE',  ( 0.1264236179284866091, 0.07713981129832027384, 0.1264236179284866091 ) ) ;
#13263 = CARTESIAN_POINT ( 'NONE',  ( 0.5113546317124669782, 4.466152701071653354E-17, 0.000000000000000000 ) ) ;
#13264 = CARTESIAN_POINT ( 'NONE',  ( 0.6971942568897637749, 2.189545951927499583E-17, 0.5142716534895434011 ) ) ;
#13265 = CLOSED_SHELL ( 'NONE', ( #21647, #46296, #4302, #20406, #44898, #22446, #4102, #10762, #29809, #17996, #25341, #41850, #34271, #1340, #11400, #38627, #46135, #38942, #45916, #46989, #30484, #3521, #6512, #33745, #26269, #6481 ) ) ;
#13266 = CARTESIAN_POINT ( 'NONE',  ( -0.6971942568897648851, -0.07405724077823297447, 0.8759842519147408302 ) ) ;
#13268 = DIRECTION ( 'NONE',  ( -6.938893903907229955E-15, 0.000000000000000000, -1.000000000000000000 ) ) ;
#13267 = CARTESIAN_POINT ( 'NONE',  ( -0.1113553986120547346, -0.9773622047244094890, -0.1113553986120547346 ) ) ;
#13269 = CARTESIAN_POINT ( 'NONE',  ( -0.1797182628040039087, -1.617661919819267213, -0.07444174185955065859 ) ) ;
#13270 = CARTESIAN_POINT ( 'NONE',  ( 0.9500414927467378812, -0.1787899950787401604, 1.594488188922613237 ) ) ;
#13272 = DIRECTION ( 'NONE',  ( 1.000000000000000000, -0.000000000000000000, -0.000000000000000000 ) ) ;
#13271 = DIRECTION ( 'NONE',  ( -1.000000000000000000, -0.000000000000000000, -0.000000000000000000 ) ) ;
#13273 = CARTESIAN_POINT ( 'NONE',  ( 0.7495606340400177148, 0.1264236179284866091, 0.3518700786863940833 ) ) ;
#13274 = CARTESIAN_POINT ( 'NONE',  ( -1.033464566929133799, 0.000000000000000000, 1.456692913278299084 ) ) ;
#13275 = CARTESIAN_POINT ( 'NONE',  ( 0.1264236179284866091, -0.09891732278088229136, -0.1264236179284866091 ) ) ;
#13276 = CARTESIAN_POINT ( 'NONE',  ( 0.1787899950787401604, -0.06200787396198446239, 0.07405724077823318263 ) ) ;
#13277 = CARTESIAN_POINT ( 'NONE',  ( 1.002407869896990045, 0.1264236179284866091, 0.4601377952218267953 ) ) ;
#13278 = CARTESIAN_POINT ( 'NONE',  ( -0.1264236179284866091, -0.9109251967966299768, -0.1264236179284866091 ) ) ;
#13279 = CARTESIAN_POINT ( 'NONE',  ( 1.033464566929133799, 0.000000000000000000, 1.889763779420031486 ) ) ;
#13280 = EDGE_CURVE ( 'NONE', #9478, #16549, #12893, .T. ) ;
#13281 = DIRECTION ( 'NONE',  ( 0.000000000000000000, -1.000000000000000000, 0.000000000000000000 ) ) ;
#13282 = CARTESIAN_POINT ( 'NONE',  ( -0.6971942568897648851, 0.07405724077823318263, 1.496062992072220821 ) ) ;
#13283 = VERTEX_POINT ( 'NONE', #44731 ) ;
#13284 = CARTESIAN_POINT ( 'NONE',  ( 0.8759842519685039353, 0.000000000000000000, 4.498031496062992574 ) ) ;
#13285 = CARTESIAN_POINT ( 'NONE',  ( 0.6971942568897626646, -0.07405724077823297447, 0.9547244093950547628 ) ) ;
#13286 = VERTEX_POINT ( 'NONE', #4721 ) ;
#13287 = CARTESIAN_POINT ( 'NONE',  ( -0.9412147342319837628, -0.1574803149606297803, 0.5044291337507409434 ) ) ;
#13288 = DIRECTION ( 'NONE',  ( 0.000000000000000000, 0.7880107536067203489, -0.6156614753256604011 ) ) ;
#13289 = CARTESIAN_POINT ( 'NONE',  ( 0.8019270111902717657, 0.1787899950787401604, 1.687992125930489307 ) ) ;
#13290 = CARTESIAN_POINT ( 'NONE',  ( -0.7646288533564489232, 0.1113553986120547346, 1.402559055118110187 ) ) ;
#13291 = EDGE_CURVE ( 'NONE', #46402, #25724, #12171, .T. ) ;
#13292 = DIRECTION ( 'NONE',  ( 0.000000000000000000, 0.000000000000000000, -1.000000000000000000 ) ) ;
#13293 = CARTESIAN_POINT ( 'NONE',  ( 0.000000000000000000, 0.000000000000000000, -0.07924015748031493223 ) ) ;
#13294 = CARTESIAN_POINT ( 'NONE',  ( 1.054774247047244096, 0.000000000000000000, 0.2239173227808822775 ) ) ;
#13295 = CARTESIAN_POINT ( 'NONE',  ( -0.6971942568897637749, 2.189545951927499583E-17, 0.08120078734781142893 ) ) ;
#13296 = CARTESIAN_POINT ( 'NONE',  ( 0.7185039370078746268, 0.06523048226347956391, 1.355807086506646275 ) ) ;
#13297 = ORIENTED_EDGE ( 'NONE', *, *, #15550, .F. ) ;
#13298 = VERTEX_POINT ( 'NONE', #43024 ) ;
#13299 = CARTESIAN_POINT ( 'NONE',  ( 3.284318927891251994E-17, 0.08316929139234625901, 0.1787899950787401882 ) ) ;
#13300 = CARTESIAN_POINT ( 'NONE',  ( -0.8759842519685039353, -0.1787899950787401882, 1.665846456639149764 ) ) ;
#13301 = CARTESIAN_POINT ( 'NONE',  ( 1.033836350893150957, 0.005690288880516385442, 0.03937007863263045776 ) ) ;
#13302 = PLANE ( 'NONE',  #18027 ) ;
#13303 = FACE_OUTER_BOUND ( 'NONE', #20319, .T. ) ;
#13304 = CARTESIAN_POINT ( 'NONE',  ( 3.284318927891251994E-17, -1.187623968229238214, 0.1787899950787401882 ) ) ;
#13305 = AXIS2_PLACEMENT_3D ( 'NONE', #32421, #28591, #32891 ) ;
#13306 = ORIENTED_EDGE ( 'NONE', *, *, #44495, .F. ) ;
#13307 = CARTESIAN_POINT ( 'NONE',  ( 3.284318927891251994E-17, -0.06938976372576398377, 0.1787899950787401882 ) ) ;
#13308 = ORIENTED_EDGE ( 'NONE', *, *, #1438, .F. ) ;
#13309 = EDGE_LOOP ( 'NONE', ( #34696, #24463, #14277, #2705 ) ) ;
#13310 = CARTESIAN_POINT ( 'NONE',  ( 0.9500414927467378812, -0.1787899950787401604, 1.117125984198206412 ) ) ;
#13311 = ADVANCED_FACE ( 'NONE', ( #28455 ), #10475, .T. ) ;
#13312 = CARTESIAN_POINT ( 'NONE',  ( -0.8759842519685039353, 0.1574803149606299191, 0.9153543306011338032 ) ) ;
#13313 = CARTESIAN_POINT ( 'NONE',  ( 0.7646288533564489232, -0.1113553986120547346, 1.766732283464566899 ) ) ;
#13314 = CARTESIAN_POINT ( 'NONE',  ( -0.07405724077823318263, -0.7608267715997808489, -0.1787899950787401604 ) ) ;
#13315 = EDGE_LOOP ( 'NONE', ( #44383, #38974, #19729, #33181, #9683 ) ) ;
#13316 = CARTESIAN_POINT ( 'NONE',  ( -1.002407869896990045, 0.1264236179284866091, 0.3075787401037169411 ) ) ;
#13317 = CARTESIAN_POINT ( 'NONE',  ( -1.033464566929133799, 0.000000000000000000, 1.033464566929133799 ) ) ;
#13318 = CARTESIAN_POINT ( 'NONE',  ( 0.1270800023317771588, -1.167366644228714501, 0.1270800023317771588 ) ) ;
#13319 = FACE_OUTER_BOUND ( 'NONE', #5249, .T. ) ;
#13320 = CARTESIAN_POINT ( 'NONE',  ( 0.9500414927467378812, -0.1787899950787401604, 1.043307086560409269 ) ) ;
#13321 = CARTESIAN_POINT ( 'NONE',  ( 0.8759842519685039353, 0.1787899950787401882, 1.606791338528913426 ) ) ;
#13322 = CARTESIAN_POINT ( 'NONE',  ( 1.002407869896990045, -0.1264236179284866091, 0.1747047243556852092 ) ) ;
#13323 = EDGE_CURVE ( 'NONE', #2820, #4638, #2194, .T. ) ;
#13324 = DIRECTION ( 'NONE',  ( 0.000000000000000000, 0.000000000000000000, 1.000000000000000000 ) ) ;
#13325 = CARTESIAN_POINT ( 'NONE',  ( 0.000000000000000000, 1.205361022782826802E-17, -0.09842519685039370636 ) ) ;
#13326 = CARTESIAN_POINT ( 'NONE',  ( 0.1630380172108122638, -0.08011826877085716225, -0.1387687780145144545 ) ) ;
#13327 = DIRECTION ( 'NONE',  ( 0.000000000000000000, 0.9699617890481186944, 0.2432573283306648515 ) ) ;
#13328 = CARTESIAN_POINT ( 'NONE',  ( -1.094772975963752103E-17, 0.02903543312462964626, -0.1787899950787401882 ) ) ;
#13329 = DIRECTION ( 'NONE',  ( -3.469446951953590129E-15, -1.000000000000000000, 0.000000000000000000 ) ) ;
#13330 = EDGE_CURVE ( 'NONE', #31112, #32653, #1483, .T. ) ;
#13331 = CARTESIAN_POINT ( 'NONE',  ( 0.7495606340400177148, -0.1264236179284866091, 1.149114173174582643 ) ) ;
#13332 = CARTESIAN_POINT ( 'NONE',  ( 0.7495606340400177148, -0.1264236179284866091, 1.902066929080094448 ) ) ;
#13333 = CARTESIAN_POINT ( 'NONE',  ( 0.9412147342319837628, 0.1574803149606300301, 0.3223425195775121432 ) ) ;
#13334 = ORIENTED_EDGE ( 'NONE', *, *, #27094, .F. ) ;
#13335 = VECTOR ( 'NONE', #18648, 39.37007874015748143 ) ;
#13336 = DIRECTION ( 'NONE',  ( 8.180381323125439611E-33, -1.224646799147353947E-16, 1.000000000000000000 ) ) ;
#13337 = CARTESIAN_POINT ( 'NONE',  ( 1.033464566929133799, 0.000000000000000000, 0.2460629921259842590 ) ) ;
#13338 = CARTESIAN_POINT ( 'NONE',  ( -0.8759842519685039353, 0.1574803149606299191, 0.2066929132782996115 ) ) ;
#13339 = CARTESIAN_POINT ( 'NONE',  ( 1.054774247047244540, 0.07405724077823318263, 1.363188976324188895 ) ) ;
#13340 = ADVANCED_FACE ( 'NONE', ( #43274 ), #46630, .T. ) ;
#13342 = DIRECTION ( 'NONE',  ( -1.000000000000000000, 0.000000000000000000, 0.000000000000000000 ) ) ;
#13341 = CARTESIAN_POINT ( 'NONE',  ( 0.1036066153429698738, -0.09660391682274865888, 0.2256134787373819950 ) ) ;
#13343 = CARTESIAN_POINT ( 'NONE',  ( 3.284318927891251994E-17, 0.08809055123486594918, 0.1787899950787401882 ) ) ;
#13344 = CYLINDRICAL_SURFACE ( 'NONE', #22960, 0.1574803149606299191 ) ;
#13345 = ORIENTED_EDGE ( 'NONE', *, *, #31190, .F. ) ;
#13346 = CARTESIAN_POINT ( 'NONE',  ( 1.033464566929134687, -0.06523048226347956391, 0.5191929133858269596 ) ) ;
#13347 = CARTESIAN_POINT ( 'NONE',  ( -0.8107537697050254399, 0.1574803149606300301, 0.2091535431995598104 ) ) ;
#13348 = VERTEX_POINT ( 'NONE', #24149 ) ;
#13349 = ORIENTED_EDGE ( 'NONE', *, *, #10520, .F. ) ;
#13350 = CARTESIAN_POINT ( 'NONE',  ( -0.1264236179284866091, -1.614665354276944909, 0.1264236179284866091 ) ) ;
#13351 = CARTESIAN_POINT ( 'NONE',  ( -0.7495606340400177148, 0.1264236179284866091, 1.026082677111590513 ) ) ;
#13352 = CARTESIAN_POINT ( 'NONE',  ( -0.7495606340400177148, -0.1264236179284866091, 1.936515747977732405 ) ) ;
#13353 = ORIENTED_EDGE ( 'NONE', *, *, #20766, .F. ) ;
#13354 = CARTESIAN_POINT ( 'NONE',  ( -0.9500414927467377701, 0.1787899950787401604, 0.9744094487651340231 ) ) ;
#13355 = CIRCLE ( 'NONE', #41667, 0.1377952755905510751 ) ;
#13356 = CARTESIAN_POINT ( 'NONE',  ( -1.002407869896990045, -0.1264236179284866091, 0.6126968503399370380 ) ) ;
#13357 = CARTESIAN_POINT ( 'NONE',  ( 0.1529906210716822090, 0.1251777869743438687, -0.05500979718732867257 ) ) ;
#13358 = DIRECTION ( 'NONE',  ( 0.000000000000000000, 0.000000000000000000, 1.000000000000000000 ) ) ;
#13359 = CARTESIAN_POINT ( 'NONE',  ( -0.1787899950787401882, -0.6856554642922303433, 0.000000000000000000 ) ) ;
#13360 = ORIENTED_EDGE ( 'NONE', *, *, #44670, .T. ) ;
#13361 = CARTESIAN_POINT ( 'NONE',  ( 0.1078383211903921335, -0.08956014831809350207, 0.1858721435341346429 ) ) ;
#13362 = CARTESIAN_POINT ( 'NONE',  ( -0.04828142644392272725, -0.08854577535781626985, 0.1504058830162713911 ) ) ;
#13363 = CIRCLE ( 'NONE', #31766, 0.1377952755905511861 ) ;
#13364 = EDGE_LOOP ( 'NONE', ( #12089, #19872, #15320, #932 ) ) ;
#13365 = CARTESIAN_POINT ( 'NONE',  ( -1.033464566929133799, 0.000000000000000000, 0.3543307085538902057 ) ) ;
#13366 = CARTESIAN_POINT ( 'NONE',  ( -0.7185039370078766252, -0.06523048226348168721, 1.754429133750741832 ) ) ;
#13367 = CARTESIAN_POINT ( 'NONE',  ( -1.002407869896990045, 0.1264236179284866091, 0.6569881889226141247 ) ) ;
#13368 = ORIENTED_EDGE ( 'NONE', *, *, #45103, .T. ) ;
#13369 = CONICAL_SURFACE ( 'NONE', #19467, 0.08090551181102362266, 0.9599310885968742602 ) ;
#13370 = CARTESIAN_POINT ( 'NONE',  ( -1.002407869896990045, -0.1264236179284866091, 1.596948818843874074 ) ) ;
#13371 = DIRECTION ( 'NONE',  ( -1.000000000000000000, 3.469446951953626022E-15, 0.000000000000000000 ) ) ;
#13372 = CARTESIAN_POINT ( 'NONE',  ( -0.8107537697050234415, -0.1574803149606297803, 0.1845472439869611792 ) ) ;
#13373 = CARTESIAN_POINT ( 'NONE',  ( 0.7185039370078739607, 0.000000000000000000, 4.498031496062992574 ) ) ;
#13374 = CARTESIAN_POINT ( 'NONE',  ( 0.8107537697050253289, 0.1574803149606300301, 0.5339566929133855444 ) ) ;
#13375 = CARTESIAN_POINT ( 'NONE',  ( 0.7185039370078739607, 1.928577636452523993E-17, 0.6496062991050708391 ) ) ;
#13376 = CARTESIAN_POINT ( 'NONE',  ( -0.8107537697050253289, 0.1574803149606300301, 1.193405511703496957 ) ) ;
#13377 = ADVANCED_FACE ( 'NONE', ( #32039 ), #31811, .F. ) ;
#13379 = CARTESIAN_POINT ( 'NONE',  ( -1.033464566929134687, 0.06523048226347956391, 0.6717519683964101596 ) ) ;
#13378 = CARTESIAN_POINT ( 'NONE',  ( -0.06523048226347956391, -0.5073818897637790704, -0.1574803149606300301 ) ) ;
#13380 = CARTESIAN_POINT ( 'NONE',  ( -0.7185039370078739607, 1.928577636452523993E-17, 0.4232283464566928832 ) ) ;
#13381 = VERTEX_POINT ( 'NONE', #31579 ) ;
#13382 = CARTESIAN_POINT ( 'NONE',  ( -0.1574803149606299191, -0.2274162997038020051, -0.9219983537151217323 ) ) ;
#13383 = CARTESIAN_POINT ( 'NONE',  ( 0.9873396505805591694, -0.1113553986120547346, 1.264763779527559029 ) ) ;
#13385 = FACE_OUTER_BOUND ( 'NONE', #29012, .T. ) ;
#13384 = CARTESIAN_POINT ( 'NONE',  ( -0.1586641775163213364, 2.177585298233989164, -3.731703755406937439 ) ) ;
#13386 = DIRECTION ( 'NONE',  ( 0.000000000000000000, 0.000000000000000000, -1.000000000000000000 ) ) ;
#13387 = CARTESIAN_POINT ( 'NONE',  ( 0.06523048226347956391, -0.5812007872940475606, -0.1574803149606300301 ) ) ;
#13388 = EDGE_CURVE ( 'NONE', #32649, #40831, #5276, .T. ) ;
#13390 = CARTESIAN_POINT ( 'NONE',  ( 0.4934383202099732468, 0.08090551181102362266, 0.000000000000000000 ) ) ;
#13389 = CARTESIAN_POINT ( 'NONE',  ( 1.002407869896990045, -0.1264236179284866091, 1.990649606245448844 ) ) ;
#13391 = CARTESIAN_POINT ( 'NONE',  ( -0.7185039370078741827, 0.06523048226347841205, 0.6963582677165353063 ) ) ;
#13393 = VECTOR ( 'NONE', #11296, 39.37007874015748854 ) ;
#13392 = CARTESIAN_POINT ( 'NONE',  ( -0.1787899950787401604, -0.5935039369541101895, -0.07405724077823318263 ) ) ;
#13394 = ORIENTED_EDGE ( 'NONE', *, *, #16001, .F. ) ;
#13395 = LINE ( 'NONE', #42584, #25346 ) ;
#13396 = CARTESIAN_POINT ( 'NONE',  ( 0.8759842519685039353, -0.1787899950787401882, 0.7997047243556849594 ) ) ;
#13397 = EDGE_CURVE ( 'NONE', #26907, #19153, #45920, .T. ) ;
#13398 = CARTESIAN_POINT ( 'NONE',  ( -0.05769625742918065708, 0.07859832706092176324, -0.2521221211081704494 ) ) ;
#13399 = FACE_OUTER_BOUND ( 'NONE', #45385, .T. ) ;
#13400 = CARTESIAN_POINT ( 'NONE',  ( 0.1270800023317771588, 0.05310579671616700442, 0.1270800023317771588 ) ) ;
#13401 = CARTESIAN_POINT ( 'NONE',  ( -0.07405724077823318263, -1.021653543253323138, 0.1787899950787401604 ) ) ;
#13402 = CARTESIAN_POINT ( 'NONE',  ( 0.1574803149606300301, -1.304625984251967630, -0.06523048226347956391 ) ) ;
#13403 = CARTESIAN_POINT ( 'NONE',  ( 0.7646288533564489232, -0.1113553986120547346, 1.284448818790110192 ) ) ;
#13404 = CARTESIAN_POINT ( 'NONE',  ( -0.7646288533564489232, 0.1113553986120547346, 1.402559055118110187 ) ) ;
#13405 = EDGE_CURVE ( 'NONE', #3834, #22756, #46869, .T. ) ;
#13406 = EDGE_LOOP ( 'NONE', ( #37037, #11576, #21512, #20266 ) ) ;
#13407 = CARTESIAN_POINT ( 'NONE',  ( -0.9500414927467378812, -0.1787899950787401604, 1.870078740103715331 ) ) ;
#13408 = CARTESIAN_POINT ( 'NONE',  ( 1.054774247047244540, -0.07405724077823318263, 1.993110236166711013 ) ) ;
#13409 = EDGE_LOOP ( 'NONE', ( #22047, #34109, #8250, #4883 ) ) ;
#13410 = CARTESIAN_POINT ( 'NONE',  ( 0.1574803149606299191, 0.001968504044534917247, -1.928577636452523993E-17 ) ) ;
#13411 = CARTESIAN_POINT ( 'NONE',  ( -0.6971942568897648851, 0.07405724077823318263, 1.574803149552536530 ) ) ;
#13412 = DIRECTION ( 'NONE',  ( 0.000000000000000000, -1.000000000000000000, 0.000000000000000000 ) ) ;
#13413 = CARTESIAN_POINT ( 'NONE',  ( -0.6971942568897626646, 0.07405724077823318263, 0.2017716534895435399 ) ) ;
#13414 = CARTESIAN_POINT ( 'NONE',  ( 1.033464566929134687, -0.06523048226347956391, 1.582185039370079149 ) ) ;
#13415 = CARTESIAN_POINT ( 'NONE',  ( -0.6971942568897648851, -0.07405724077823297447, 1.860236220418677089 ) ) ;
#13416 = CARTESIAN_POINT ( 'NONE',  ( 1.033464566929133799, 0.000000000000000000, 1.417322834538141674 ) ) ;
#13417 = CARTESIAN_POINT ( 'NONE',  ( -0.9412147342319837628, -0.1574803149606297803, 1.892224409448819644 ) ) ;
#13418 = CARTESIAN_POINT ( 'NONE',  ( 0.2559055147610055925, 0.04268399720878558040, -0.03497896297209982658 ) ) ;
#13419 = CARTESIAN_POINT ( 'NONE',  ( 0.07405724077823318263, -0.2796515272843568267, 0.1787899950787401604 ) ) ;
#13420 = CARTESIAN_POINT ( 'NONE',  ( 0.05362475593144094138, -0.09842519685039370636, 0.2150385860745854250 ) ) ;
#13421 = CARTESIAN_POINT ( 'NONE',  ( -0.1184675242425147629, -0.09842519685039370636, 1.713085361781125471 ) ) ;
#13422 = CARTESIAN_POINT ( 'NONE',  ( 0.7185039370078739607, 1.928577636452523993E-17, 1.043307086506645831 ) ) ;
#13423 = ( BOUNDED_CURVE ( )  B_SPLINE_CURVE ( 2, ( #23434, #26083, #26802, #4468, #18637, #420, #40658, #19109, #8323 ),
 .UNSPECIFIED., .F., .T. ) 
 B_SPLINE_CURVE_WITH_KNOTS ( ( 3, 2, 2, 2, 3 ),
 ( 0.9399999999999999467, 0.9425000000000000044, 0.9449999999999999512, 0.9475000000000000089, 0.9499999999999999556 ),
 .UNSPECIFIED. ) 
 CURVE ( )  GEOMETRIC_REPRESENTATION_ITEM ( )  RATIONAL_B_SPLINE_CURVE ( ( 1.000000000000000000, 0.9238795325112899581, 1.000000000000000000, 0.9238795325112869605, 1.000000000000000000, 0.9238795325112869605, 1.000000000000000000, 0.9238795325112799661, 1.000000000000000000 ) ) 
 REPRESENTATION_ITEM ( '' )  ) ;
#13424 = EDGE_LOOP ( 'NONE', ( #22046, #36975, #3266, #32673 ) ) ;
#13425 = AXIS2_PLACEMENT_3D ( 'NONE', #26632, #37152, #41184 ) ;
#13426 = ( BOUNDED_CURVE ( )  B_SPLINE_CURVE ( 2, ( #11636, #33697, #32980, #4648, #21938 ),
 .UNSPECIFIED., .F., .F. ) 
 B_SPLINE_CURVE_WITH_KNOTS ( ( 3, 2, 3 ),
 ( 0.01500000000000034986, 0.01750000000000000167, 0.02000000000000000042 ),
 .UNSPECIFIED. ) 
 CURVE ( )  GEOMETRIC_REPRESENTATION_ITEM ( )  RATIONAL_B_SPLINE_CURVE ( ( 0.9999999999999880096, 0.9238795325112979517, 1.000000000000000000, 0.9238795325112869605, 1.000000000000000000 ) ) 
 REPRESENTATION_ITEM ( '' )  ) ;
#13427 = ORIENTED_EDGE ( 'NONE', *, *, #44066, .F. ) ;
#13428 = VECTOR ( 'NONE', #37630, 39.37007874015748143 ) ;
#13429 = EDGE_CURVE ( 'NONE', #35496, #10953, #13135, .T. ) ;
#13430 = CARTESIAN_POINT ( 'NONE',  ( -0.1787899950787401882, -1.068405511757259951, 0.000000000000000000 ) ) ;
#13431 = CARTESIAN_POINT ( 'NONE',  ( -0.07405724077823318263, -1.149606299158835387, -0.1787899950787401604 ) ) ;
#13432 = CARTESIAN_POINT ( 'NONE',  ( 3.301370929368692659E-17, -0.5423666442287149447, 0.1797182628040039365 ) ) ;
#13433 = CARTESIAN_POINT ( 'NONE',  ( -0.7185039370078739607, 1.928577636452523993E-17, 0.2263779527559055260 ) ) ;
#13434 = CARTESIAN_POINT ( 'NONE',  ( -0.8759842519685039353, 0.1574803149606299191, 0.7972440943806614611 ) ) ;
#13435 = CARTESIAN_POINT ( 'NONE',  ( -0.9873396505805591694, 0.1113553986120547346, 0.6840551181102363376 ) ) ;
#13436 = EDGE_CURVE ( 'NONE', #4424, #39085, #15958, .T. ) ;
#13437 = CARTESIAN_POINT ( 'NONE',  ( -0.1113553986120547346, 0.01673228346456692717, 0.1113553986120547346 ) ) ;
#13438 = CARTESIAN_POINT ( 'NONE',  ( 1.054774247047244540, 0.07405724077823318263, 0.9694881889226144578 ) ) ;
#13440 = DIRECTION ( 'NONE',  ( -1.000000000000000000, 0.000000000000000000, 0.000000000000000000 ) ) ;
#13439 = FACE_OUTER_BOUND ( 'NONE', #26043, .T. ) ;
#13441 = CARTESIAN_POINT ( 'NONE',  ( 0.8759842519685039353, -0.1574803149606299191, 0.1870078739082208508 ) ) ;
#13442 = AXIS2_PLACEMENT_3D ( 'NONE', #11448, #23178, #12160 ) ;
#13443 = VERTEX_POINT ( 'NONE', #46398 ) ;
#13444 = CARTESIAN_POINT ( 'NONE',  ( -0.9873396505805591694, -0.1113553986120547346, 0.7824803148531023211 ) ) ;
#13446 = CARTESIAN_POINT ( 'NONE',  ( -0.1787899950787401882, -0.5959645668753701386, 0.000000000000000000 ) ) ;
#13445 = CARTESIAN_POINT ( 'NONE',  ( -0.1574803149606300301, -1.004429133750739833, -0.06523048226347956391 ) ) ;
#13447 = CARTESIAN_POINT ( 'NONE',  ( 0.1787899950787401882, -1.319389763725763665, -2.189545951927503898E-17 ) ) ;
#13448 = CARTESIAN_POINT ( 'NONE',  ( 0.8759842519685039353, -0.1787899950787401882, 0.3321850393163153226 ) ) ;
#13449 = CARTESIAN_POINT ( 'NONE',  ( -0.6971942568897648851, -0.07405724077823297447, 1.855314960576157635 ) ) ;
#13450 = ORIENTED_EDGE ( 'NONE', *, *, #43336, .T. ) ;
#13451 = CARTESIAN_POINT ( 'NONE',  ( -0.9500414927467378812, -0.1787899950787401604, 1.476377952702141449 ) ) ;
#13452 = CARTESIAN_POINT ( 'NONE',  ( 1.054774247047244096, 0.000000000000000000, 1.444389763725763665 ) ) ;
#13453 = ORIENTED_EDGE ( 'NONE', *, *, #11118, .T. ) ;
#13454 = CIRCLE ( 'NONE', #35630, 0.1574803149606299191 ) ;
#13455 = VECTOR ( 'NONE', #22174, 39.37007874015748143 ) ;
#13456 = CARTESIAN_POINT ( 'NONE',  ( -0.9500414927467378812, 0.1787899950787401604, 0.6249999999462356737 ) ) ;
#13457 = CARTESIAN_POINT ( 'NONE',  ( 0.1287673665127798128, -0.09842951992213312684, -0.1240475571185562509 ) ) ;
#13458 = CARTESIAN_POINT ( 'NONE',  ( 0.8019270111902716547, 0.1787899950787401604, 0.5905511810485987167 ) ) ;
#13459 = CARTESIAN_POINT ( 'NONE',  ( -0.6971942568897637749, 2.189545951927499583E-17, 0.5142716534895434011 ) ) ;
#13460 = CARTESIAN_POINT ( 'NONE',  ( 0.2278981769376444422, -0.05062618494133044184, 0.1538518510339534628 ) ) ;
#13461 = CARTESIAN_POINT ( 'NONE',  ( 0.1377952755905512139, 0.1564960629921262614, -0.9074803149606294195 ) ) ;
#13462 = ORIENTED_EDGE ( 'NONE', *, *, #7734, .T. ) ;
#13463 = CARTESIAN_POINT ( 'NONE',  ( -1.054774247047244096, 0.000000000000000000, 1.444389763725763665 ) ) ;
#13464 = ORIENTED_EDGE ( 'NONE', *, *, #3532, .T. ) ;
#13465 = CARTESIAN_POINT ( 'NONE',  ( -1.033464566929133799, 0.000000000000000000, 0.5216535433070865757 ) ) ;
#13466 = CARTESIAN_POINT ( 'NONE',  ( 0.8759842519685039353, 0.1787899950787401882, 1.296751968450173154 ) ) ;
#13467 = CARTESIAN_POINT ( 'NONE',  ( -0.03865401764462641360, -0.09851384930164665266, 0.2227661591646389883 ) ) ;
#13468 = VERTEX_POINT ( 'NONE', #13574 ) ;
#13469 = CARTESIAN_POINT ( 'NONE',  ( -0.8107537697050254399, -0.1574803149606297803, 0.5487204724409447953 ) ) ;
#13470 = CARTESIAN_POINT ( 'NONE',  ( 0.1787899950787401604, -1.573942865867034246, 0.07405724077823318263 ) ) ;
#13471 = ORIENTED_EDGE ( 'NONE', *, *, #37378, .F. ) ;
#13472 = CARTESIAN_POINT ( 'NONE',  ( -1.094772975963752103E-17, -0.5615157479777322935, -0.1787899950787401882 ) ) ;
#13473 = ORIENTED_EDGE ( 'NONE', *, *, #27252, .T. ) ;
#13474 = CARTESIAN_POINT ( 'NONE',  ( 1.054774247047244540, 0.07405724077823318263, 1.402559055064346971 ) ) ;
#13475 = CONICAL_SURFACE ( 'NONE', #15818, 0.1377952755905510196, 0.9599310885968940221 ) ;
#13476 = ADVANCED_FACE ( 'NONE', ( #9524 ), #634, .T. ) ;
#13477 = PLANE ( 'NONE',  #18511 ) ;
#13478 = CARTESIAN_POINT ( 'NONE',  ( 0.1787899950787401882, -0.2613188975840319284, -2.189545951927503898E-17 ) ) ;
#13479 = ADVANCED_FACE ( 'NONE', ( #29674 ), #43986, .T. ) ;
#13480 = CYLINDRICAL_SURFACE ( 'NONE', #37910, 0.1574803149606299191 ) ;
#13481 = CARTESIAN_POINT ( 'NONE',  ( 0.1631287816244539335, -0.1603246120961979437, 5.150759842524385501E-07 ) ) ;
#13482 = EDGE_CURVE ( 'NONE', #25167, #46714, #9119, .T. ) ;
#13483 = CARTESIAN_POINT ( 'NONE',  ( -0.1264236179284866091, -0.02128538555207338742, -0.1264236179284866091 ) ) ;
#13484 = CARTESIAN_POINT ( 'NONE',  ( 0.07405724077823318263, 0.08562992131360593062, 0.1787899950787401604 ) ) ;
#13485 = CARTESIAN_POINT ( 'NONE',  ( 0.2559055118110235560, -0.1161062301479638820, -0.3006843207781718097 ) ) ;
#13486 = ADVANCED_FACE ( 'NONE', ( #39908 ), #26030, .F. ) ;
#13487 = CARTESIAN_POINT ( 'NONE',  ( 1.054774247047244540, 0.07405724077823318263, 0.4576771653005669016 ) ) ;
#13488 = CARTESIAN_POINT ( 'NONE',  ( -1.054774247047244096, 0.000000000000000000, 0.8144685038832440993 ) ) ;
#13490 = CARTESIAN_POINT ( 'NONE',  ( 0.8759842519685039353, 0.1574803149606299191, 0.9940944880814488460 ) ) ;
#13489 = CARTESIAN_POINT ( 'NONE',  ( -0.1574803149606299191, -0.8543307086614173596, 0.000000000000000000 ) ) ;
#13492 = CARTESIAN_POINT ( 'NONE',  ( -0.7744514135987524694, -0.1376688215221703315, 1.986184949705119385 ) ) ;
#13491 = CARTESIAN_POINT ( 'NONE',  ( -0.1797182628040039087, -1.735772156039738778, -0.07444174185955065859 ) ) ;
#13493 = CARTESIAN_POINT ( 'NONE',  ( 1.002407869896990045, 0.1264236179284866091, 1.488681102308440751 ) ) ;
#13495 = CARTESIAN_POINT ( 'NONE',  ( 0.01230737760510407577, 0.1591122789105269553, -1.502406898952441074E-18 ) ) ;
#13494 = CARTESIAN_POINT ( 'NONE',  ( 0.8759842519685039353, -0.1787899950787401882, 1.941437007820252081 ) ) ;
#13496 = CARTESIAN_POINT ( 'NONE',  ( 1.054774247047244540, 0.07405724077823318263, 0.3789370078202520253 ) ) ;
#13497 = ORIENTED_EDGE ( 'NONE', *, *, #19700, .T. ) ;
#13498 = CARTESIAN_POINT ( 'NONE',  ( -0.3100393700787401619, 0.000000000000000000, 0.7086614173228351632 ) ) ;
#13499 = DIRECTION ( 'NONE',  ( -0.000000000000000000, 1.000000000000000000, -3.995705278811693553E-31 ) ) ;
#13500 = DIRECTION ( 'NONE',  ( 1.822029033848725028E-16, 0.000000000000000000, 1.000000000000000000 ) ) ;
#13501 = CARTESIAN_POINT ( 'NONE',  ( -1.094772975963752103E-17, -0.1333661416785198728, -0.1787899950787401882 ) ) ;
#13502 = CARTESIAN_POINT ( 'NONE',  ( 0.8759842519685039353, 0.1787899950787401882, 0.5831692912848189803 ) ) ;
#13503 = CARTESIAN_POINT ( 'NONE',  ( -1.094772975963752103E-17, -0.8764763778989921317, -0.1787899950787401882 ) ) ;
#13504 = CARTESIAN_POINT ( 'NONE',  ( 0.8624158387615522559, -0.1583668281930513955, 0.03937007853128456775 ) ) ;
#13505 = CARTESIAN_POINT ( 'NONE',  ( 1.033464566929134687, -0.06523048226347956391, 1.966043306979087246 ) ) ;
#13506 = CARTESIAN_POINT ( 'NONE',  ( -0.9500414927467378812, 0.1787899950787401604, 1.407480314906865981 ) ) ;
#13507 = CARTESIAN_POINT ( 'NONE',  ( 0.8107537697050254399, -0.1574803149606297803, 0.4306102362204725642 ) ) ;
#13508 = CARTESIAN_POINT ( 'NONE',  ( 0.7495606340400177148, -0.1264236179284866091, 0.9965551180564724554 ) ) ;
#13509 = ORIENTED_EDGE ( 'NONE', *, *, #46510, .F. ) ;
#13510 = CARTESIAN_POINT ( 'NONE',  ( 0.7646288533564489232, -0.1113553986120547346, 1.491141732283464583 ) ) ;
#13511 = CARTESIAN_POINT ( 'NONE',  ( -0.7185039370078746268, -0.06523048226347956391, 1.449311023622047445 ) ) ;
#13512 = CARTESIAN_POINT ( 'NONE',  ( -0.8019270111902717657, -0.1787899950787401604, 0.9153543306548987957 ) ) ;
#13513 = DIRECTION ( 'NONE',  ( -3.469446951953613794E-15, -1.000000000000000000, 0.000000000000000000 ) ) ;
#13514 = CARTESIAN_POINT ( 'NONE',  ( 0.2821522309711287368, 0.08090551181102362266, 9.908067607274841931E-18 ) ) ;
#13515 = CARTESIAN_POINT ( 'NONE',  ( 0.8019270111902716547, 0.1787899950787401604, 0.1574803149068664809 ) ) ;
#13516 = CARTESIAN_POINT ( 'NONE',  ( -1.054774247047244096, 0.000000000000000000, 0.1402559054580474474 ) ) ;
#13517 = CARTESIAN_POINT ( 'NONE',  ( 0.7646288533564489232, -0.1113553986120547346, 1.599409448711369919 ) ) ;
#13518 = ORIENTED_EDGE ( 'NONE', *, *, #6692, .T. ) ;
#13519 = CARTESIAN_POINT ( 'NONE',  ( 0.8107537697050254399, 0.1574803149606300301, 1.783956692805859001 ) ) ;
#13520 = CARTESIAN_POINT ( 'NONE',  ( -1.054774247047244096, 0.000000000000000000, 1.715059055064346527 ) ) ;
#13521 = ( BOUNDED_CURVE ( )  B_SPLINE_CURVE ( 2, ( #36793, #33459, #30120, #44655, #26499, #41059, #8257, #22882, #12596 ),
 .UNSPECIFIED., .F., .T. ) 
 B_SPLINE_CURVE_WITH_KNOTS ( ( 3, 2, 2, 2, 3 ),
 ( 0.05500000000000000028, 0.05750000000000000250, 0.05999999999999999778, 0.06250000000000000000, 0.06500000000000000222 ),
 .UNSPECIFIED. ) 
 CURVE ( )  GEOMETRIC_REPRESENTATION_ITEM ( )  RATIONAL_B_SPLINE_CURVE ( ( 1.000000000000000000, 0.9238795325112869605, 1.000000000000000000, 0.9238795325112869605, 1.000000000000000000, 0.9238795325112869605, 1.000000000000000000, 0.9238795325112869605, 1.000000000000000000 ) ) 
 REPRESENTATION_ITEM ( '' )  ) ;
#13522 = FACE_OUTER_BOUND ( 'NONE', #4258, .T. ) ;
#13523 = LINE ( 'NONE', #9474, #669 ) ;
#13524 = CARTESIAN_POINT ( 'NONE',  ( 0.1787899950787401604, -1.175320818622938912, -0.07405724077823318263 ) ) ;
#13525 = EDGE_LOOP ( 'NONE', ( #34874, #24093, #16663, #44854, #34630 ) ) ;
#13526 = CARTESIAN_POINT ( 'NONE',  ( -0.1264236179284866091, -0.1924212597887563214, 0.1264236179284866091 ) ) ;
#13527 = ORIENTED_EDGE ( 'NONE', *, *, #960, .F. ) ;
#13528 = ORIENTED_EDGE ( 'NONE', *, *, #35124, .T. ) ;
#13529 = CARTESIAN_POINT ( 'NONE',  ( 0.6971942568897648851, 0.07405724077823318263, 1.062992125930488418 ) ) ;
#13530 = CARTESIAN_POINT ( 'NONE',  ( 0.01230737760510409486, -0.1591122789105269553, -1.990515434288500257E-18 ) ) ;
#13531 = CARTESIAN_POINT ( 'NONE',  ( 0.5555748031496099415, 0.6449983665207553729, -0.7480314960629920185 ) ) ;
#13532 = ADVANCED_FACE ( 'NONE', ( #36355 ), #3967, .T. ) ;
#13533 = CARTESIAN_POINT ( 'NONE',  ( 0.7646288533564489232, -0.1113553986120547346, 1.845472440944881942 ) ) ;
#13534 = CARTESIAN_POINT ( 'NONE',  ( 0.1797182628040039087, -0.2200241245436755921, 0.07444174185955046430 ) ) ;
#13535 = EDGE_CURVE ( 'NONE', #28682, #7400, #16222, .T. ) ;
#13536 = ( BOUNDED_CURVE ( )  B_SPLINE_CURVE ( 2, ( #46324, #42698, #43423, #13507, #3425, #39357, #24760, #13734, #40060 ),
 .UNSPECIFIED., .F., .F. ) 
 B_SPLINE_CURVE_WITH_KNOTS ( ( 3, 2, 2, 2, 3 ),
 ( 0.2099999999999999922, 0.2124999999999999944, 0.2149999999999999967, 0.2174999999999999989, 0.2200000000000000011 ),
 .UNSPECIFIED. ) 
 CURVE ( )  GEOMETRIC_REPRESENTATION_ITEM ( )  RATIONAL_B_SPLINE_CURVE ( ( 1.000000000000000000, 0.9238795325112869605, 1.000000000000000000, 0.9238795325112869605, 1.000000000000000000, 0.9238795325112869605, 1.000000000000000000, 0.9238795325112869605, 1.000000000000000000 ) ) 
 REPRESENTATION_ITEM ( '' )  ) ;
#13537 = CARTESIAN_POINT ( 'NONE',  ( -0.9500414927467377701, 0.1787899950787401604, 0.3494094487651343006 ) ) ;
#13538 = CARTESIAN_POINT ( 'NONE',  ( 3.301370929368692659E-17, -1.329768219031864041, 0.1797182628040039365 ) ) ;
#13539 = CARTESIAN_POINT ( 'NONE',  ( -0.05949606008255010903, 0.2611441659580247543, -0.05295753290290025617 ) ) ;
#13540 = CARTESIAN_POINT ( 'NONE',  ( 0.8019270111902717657, -0.1787899950787401604, 1.038385826717890259 ) ) ;
#13541 = CARTESIAN_POINT ( 'NONE',  ( 0.6971942568897648851, 0.07405724077823318263, 1.574803149552536530 ) ) ;
#13542 = CARTESIAN_POINT ( 'NONE',  ( 0.8019270111902716547, -0.1787899950787401604, 0.2066929133320631329 ) ) ;
#13544 = CARTESIAN_POINT ( 'NONE',  ( -0.8501570456612310700, 0.1562720023928429736, 1.978846797534572044 ) ) ;
#13543 = CARTESIAN_POINT ( 'NONE',  ( 0.4028871391076110364, -0.08090551181102362266, 1.098083891755157578E-17 ) ) ;
#13545 = CARTESIAN_POINT ( 'NONE',  ( 0.000000000000000000, 0.000000000000000000, 0.09842519685039370636 ) ) ;
#13546 = CARTESIAN_POINT ( 'NONE',  ( -0.7185039370078746268, -0.06523048226347956391, 1.715059055010583311 ) ) ;
#13547 = CARTESIAN_POINT ( 'NONE',  ( 0.1787899950787401882, 0.01919291343959027632, -2.189545951927503898E-17 ) ) ;
#13548 = CARTESIAN_POINT ( 'NONE',  ( 0.9500414927467378812, -0.1787899950787401604, 0.1722440944344254266 ) ) ;
#13549 = CARTESIAN_POINT ( 'NONE',  ( 0.2395294000716134131, 3.218313930830148909E-16, -0.8759842519685039353 ) ) ;
#13551 = CARTESIAN_POINT ( 'NONE',  ( -0.7185039370078746268, 0.06523048226347956391, 1.956200787401576102 ) ) ;
#13550 = CARTESIAN_POINT ( 'NONE',  ( 0.9500414927467377701, 0.1787899950787401604, 1.171259842465921741 ) ) ;
#13552 = CARTESIAN_POINT ( 'NONE',  ( 0.8759842519685039353, 0.000000000000000000, 4.498031496062992574 ) ) ;
#13553 = CARTESIAN_POINT ( 'NONE',  ( 0.8107537697050253289, 0.1574803149606300301, 0.4453740156405042727 ) ) ;
#13554 = ORIENTED_EDGE ( 'NONE', *, *, #14082, .F. ) ;
#13555 = FACE_OUTER_BOUND ( 'NONE', #9286, .T. ) ;
#13556 = CARTESIAN_POINT ( 'NONE',  ( 1.029575913376797658, 0.04788448113887518870, 0.03937007987371889811 ) ) ;
#13557 = CARTESIAN_POINT ( 'NONE',  ( -0.9412147342319837628, -0.1574803149606297803, 0.2288385825696384601 ) ) ;
#13558 = ORIENTED_EDGE ( 'NONE', *, *, #46516, .F. ) ;
#13560 = CARTESIAN_POINT ( 'NONE',  ( -0.7185039370078739607, 1.928577636452523993E-17, 0.2165354329633393804 ) ) ;
#13559 = CARTESIAN_POINT ( 'NONE',  ( 0.8107537697050254399, 0.1574803149606300301, 1.232775590443654812 ) ) ;
#13561 = CARTESIAN_POINT ( 'NONE',  ( -0.07405724077823318263, -0.03248031490686641154, 0.1787899950787401604 ) ) ;
#13562 = EDGE_CURVE ( 'NONE', #14046, #32938, #40663, .T. ) ;
#13563 = CARTESIAN_POINT ( 'NONE',  ( 0.1644020957507539848, -0.08115590401245571794, -0.1405661490837558925 ) ) ;
#13564 = CARTESIAN_POINT ( 'NONE',  ( -0.6195511811023656223, 0.000000000000000000, 1.186023622047243986 ) ) ;
#13565 = CARTESIAN_POINT ( 'NONE',  ( 0.7185039370078739607, 0.000000000000000000, 4.498031496062992574 ) ) ;
#13566 = VERTEX_POINT ( 'NONE', #21723 ) ;
#13567 = CARTESIAN_POINT ( 'NONE',  ( -1.054774247047244096, 0.000000000000000000, 1.360728346402929168 ) ) ;
#13568 = CARTESIAN_POINT ( 'NONE',  ( 0.07405724077823318263, -1.671259842465922407, -0.1787899950787401604 ) ) ;
#13569 = CARTESIAN_POINT ( 'NONE',  ( -1.054774247047244540, 0.07405724077823318263, 0.9744094487651340231 ) ) ;
#13570 = CARTESIAN_POINT ( 'NONE',  ( -0.9500414927467378812, 0.1787899950787401604, 1.919291338528913871 ) ) ;
#13571 = ORIENTED_EDGE ( 'NONE', *, *, #17755, .T. ) ;
#13572 = CARTESIAN_POINT ( 'NONE',  ( -0.8019270111902716547, -0.1787899950787401604, 1.112204724355684959 ) ) ;
#13573 = CARTESIAN_POINT ( 'NONE',  ( -0.8759842519685039353, 0.1787899950787401882, 0.6668307086076534773 ) ) ;
#13574 = CARTESIAN_POINT ( 'NONE',  ( -1.033464566929133799, 0.000000000000000000, 0.2460629921259842590 ) ) ;
#13575 = ORIENTED_EDGE ( 'NONE', *, *, #45043, .F. ) ;
#13576 = CARTESIAN_POINT ( 'NONE',  ( -0.1165037417137196885, -0.08956132732375866878, 0.1114237959394338701 ) ) ;
#13577 = DIRECTION ( 'NONE',  ( -1.000000000000000000, 0.000000000000000000, 0.000000000000000000 ) ) ;
#13578 = EDGE_LOOP ( 'NONE', ( #25067, #13785, #37749, #44152 ) ) ;
#13579 = CARTESIAN_POINT ( 'NONE',  ( -0.9412147342319837628, -0.1574803149606297803, 1.734744094488190003 ) ) ;
#13580 = CARTESIAN_POINT ( 'NONE',  ( -0.8019270111902717657, -0.1787899950787401604, 0.5610236219934807700 ) ) ;
#13581 = CARTESIAN_POINT ( 'NONE',  ( 2.892866454678787531E-17, 0.06102362204724409711, 0.1574803149606299191 ) ) ;
#13582 = ADVANCED_FACE ( 'NONE', ( #33243 ), #14535, .T. ) ;
#13583 = ORIENTED_EDGE ( 'NONE', *, *, #13181, .T. ) ;
#13584 = CARTESIAN_POINT ( 'NONE',  ( -0.6971942568897648851, -0.07405724077823297447, 1.663385826717890925 ) ) ;
#13585 = CARTESIAN_POINT ( 'NONE',  ( 1.614954907737318939E-16, -8.878505979408855953E-16, 0.4940944881889759444 ) ) ;
#13586 = AXIS2_PLACEMENT_3D ( 'NONE', #23369, #4896, #41772 ) ;
#13587 = CARTESIAN_POINT ( 'NONE',  ( -1.033464566929133799, 0.000000000000000000, 0.4822834645669291653 ) ) ;
#13588 = DIRECTION ( 'NONE',  ( -1.000000000000000000, -0.000000000000000000, 0.000000000000000000 ) ) ;
#13589 = CARTESIAN_POINT ( 'NONE',  ( 0.9873396505805591694, 0.1113553986120547346, 0.5659448818897637734 ) ) ;
#13590 = CARTESIAN_POINT ( 'NONE',  ( 0.07444174185955046430, -0.7219926284806829075, -0.1797182628040039087 ) ) ;
#13591 = CARTESIAN_POINT ( 'NONE',  ( -0.9873396505805591694, 0.1113553986120547346, 0.9596456692913386544 ) ) ;
#13592 = CARTESIAN_POINT ( 'NONE',  ( -0.7185039370078746268, -0.06523048226347956391, 1.400098425089323140 ) ) ;
#13593 = CARTESIAN_POINT ( 'NONE',  ( 0.06523048226347956391, -0.5910433070866143446, -0.1574803149606300301 ) ) ;
#13594 = CARTESIAN_POINT ( 'NONE',  ( 0.2471922904502826812, 0.03219022224904102836, -0.1427165354330708902 ) ) ;
#13595 = ORIENTED_EDGE ( 'NONE', *, *, #38353, .F. ) ;
#13596 = CARTESIAN_POINT ( 'NONE',  ( -0.2559055118110235560, 0.01785997614104697234, -0.02837153189565116279 ) ) ;
#13597 = CARTESIAN_POINT ( 'NONE',  ( 0.7185039370078746268, 0.06523048226347956391, 1.326279527559055982 ) ) ;
#13599 = CARTESIAN_POINT ( 'NONE',  ( -0.3161444924769509779, 1.798092712879851174, -3.826876940038414610 ) ) ;
#13598 = DIRECTION ( 'NONE',  ( 0.000000000000000000, 1.000000000000000000, 0.000000000000000000 ) ) ;
#13600 = CARTESIAN_POINT ( 'NONE',  ( 1.033464566929133799, 0.000000000000000000, 1.742125984251968518 ) ) ;
#13602 = CARTESIAN_POINT ( 'NONE',  ( 0.7646288533564489232, -0.1113553986120547346, 1.678149606191684962 ) ) ;
#13601 = CARTESIAN_POINT ( 'NONE',  ( 0.6971942568897648851, -0.07405724077823297447, 0.6348425196312760255 ) ) ;
#13603 = CARTESIAN_POINT ( 'NONE',  ( -0.8759842519685039353, 0.1574803149606299191, 0.6889763779527560139 ) ) ;
#13604 = CARTESIAN_POINT ( 'NONE',  ( -0.08091701073424910351, -0.5708661417322834497, 1.112073044918589382 ) ) ;
#13605 = VERTEX_POINT ( 'NONE', #593 ) ;
#13606 = CARTESIAN_POINT ( 'NONE',  ( -1.033464566929134687, -0.06523048226347956391, 1.070374015748031038 ) ) ;
#13607 = CARTESIAN_POINT ( 'NONE',  ( 1.033464566929134687, -0.06523048226347956391, 0.7160433070866151217 ) ) ;
#13608 = CARTESIAN_POINT ( 'NONE',  ( 0.8019270111902717657, -0.1787899950787401604, 0.7578740156942689321 ) ) ;
#13609 = EDGE_LOOP ( 'NONE', ( #27314, #14768 ) ) ;
#13610 = CARTESIAN_POINT ( 'NONE',  ( 0.7185039370078739607, 1.928577636452523993E-17, 1.289370078740157632 ) ) ;
#13611 = FACE_OUTER_BOUND ( 'NONE', #20479, .T. ) ;
#13612 = CARTESIAN_POINT ( 'NONE',  ( -1.100456976456230270E-17, 0.06786957624372617903, -0.1797182628040039365 ) ) ;
#13613 = CARTESIAN_POINT ( 'NONE',  ( -0.07405724077823318263, -0.9822834645131651721, 0.1787899950787401604 ) ) ;
#13614 = CARTESIAN_POINT ( 'NONE',  ( 0.06523048226347956391, -1.457185039370078483, -0.1574803149606300301 ) ) ;
#13615 = CARTESIAN_POINT ( 'NONE',  ( 0.8107537697050253289, -0.1574803149606297803, 1.247539369971212508 ) ) ;
#13616 = EDGE_CURVE ( 'NONE', #9932, #15531, #21956, .T. ) ;
#13617 = CARTESIAN_POINT ( 'NONE',  ( 0.000000000000000000, 0.000000000000000000, -0.3149606299212598381 ) ) ;
#13618 = VECTOR ( 'NONE', #23347, 39.37007874015748143 ) ;
#13619 = ORIENTED_EDGE ( 'NONE', *, *, #4750, .F. ) ;
#13620 = CARTESIAN_POINT ( 'NONE',  ( -0.8019270111902717657, 0.1787899950787401604, 1.889763779473794258 ) ) ;
#13621 = VERTEX_POINT ( 'NONE', #36576 ) ;
#13622 = CARTESIAN_POINT ( 'NONE',  ( -0.8759842519685039353, 0.000000000000000000, 0.000000000000000000 ) ) ;
#13623 = ORIENTED_EDGE ( 'NONE', *, *, #20913, .F. ) ;
#13624 = CARTESIAN_POINT ( 'NONE',  ( -1.002407869896990045, -0.1264236179284866091, 1.951279527505291433 ) ) ;
#13625 = CARTESIAN_POINT ( 'NONE',  ( -1.054774247047244540, 0.07405724077823318263, 1.599409448765135133 ) ) ;
#13626 = CARTESIAN_POINT ( 'NONE',  ( 0.5113546317124669782, -0.09842519685039370636, 0.000000000000000000 ) ) ;
#13627 = B_SPLINE_CURVE_WITH_KNOTS ( 'NONE', 3,
 ( #28025, #9797, #20798, #24406, #28742, #39008, #6175, #39472, #2576, #35439, #17215, #31850, #46429, #446 ),
 .UNSPECIFIED., .F., .F.,
 ( 4, 2, 2, 2, 2, 2, 4 ),
 ( 0.000000000000000000, 0.1249999999999994449, 0.2499999999999991673, 0.3749999999999988898, 0.4374999999999987232, 0.4999999999999985567, 1.000000000000000000 ),
 .UNSPECIFIED. ) ;
#13628 = AXIS2_PLACEMENT_3D ( 'NONE', #31505, #42951, #46088 ) ;
#13629 = CARTESIAN_POINT ( 'NONE',  ( -0.7495606340400177148, 0.1264236179284866091, 0.2386811023084413619 ) ) ;
#13630 = CARTESIAN_POINT ( 'NONE',  ( -0.2471922904502826812, 0.09210780053718727045, 0.04262551151394271265 ) ) ;
#13631 = CARTESIAN_POINT ( 'NONE',  ( -1.054774247047244540, -0.07405724077823318263, 1.835629921206078485 ) ) ;
#13632 = CARTESIAN_POINT ( 'NONE',  ( -0.1478471407235199264, 0.09575019180979009448, 0.2000734843705010146 ) ) ;
#13633 = CARTESIAN_POINT ( 'NONE',  ( -1.033464566929133799, 0.000000000000000000, 1.938976377952756014 ) ) ;
#13634 = CARTESIAN_POINT ( 'NONE',  ( -0.7185039370078766252, -0.06523048226348168721, 1.882381889763779625 ) ) ;
#13635 = CARTESIAN_POINT ( 'NONE',  ( 0.1264236179284866091, -0.3067184564182153794, -0.1264236179284866091 ) ) ;
#13636 = EDGE_CURVE ( 'NONE', #8144, #28387, #39663, .T. ) ;
#13637 = CARTESIAN_POINT ( 'NONE',  ( -0.8107537697050254399, -0.1574803149606297803, 1.493602362204724754 ) ) ;
#13638 = CARTESIAN_POINT ( 'NONE',  ( 0.9873396505805591694, -0.1113553986120547346, 1.058070866034204860 ) ) ;
#13639 = CARTESIAN_POINT ( 'NONE',  ( -0.6971942568897637749, 2.189545951927499583E-17, 0.1599409448281264023 ) ) ;
#13640 = EDGE_CURVE ( 'NONE', #46242, #32499, #14774, .T. ) ;
#13641 = ORIENTED_EDGE ( 'NONE', *, *, #18348, .T. ) ;
#13642 = ORIENTED_EDGE ( 'NONE', *, *, #33323, .F. ) ;
#13643 = CARTESIAN_POINT ( 'NONE',  ( -1.054774247047244540, -0.07405724077823318263, 1.205708661363558365 ) ) ;
#13644 = ORIENTED_EDGE ( 'NONE', *, *, #42513, .F. ) ;
#13645 = ADVANCED_FACE ( 'NONE', ( #17881 ), #29200, .F. ) ;
#13646 = CARTESIAN_POINT ( 'NONE',  ( 0.1264236179284866091, -1.201279527505291433, -0.1264236179284866091 ) ) ;
#13647 = CARTESIAN_POINT ( 'NONE',  ( 0.07405724077823318263, -1.233267716481668774, -0.1787899950787401604 ) ) ;
#13648 = AXIS2_PLACEMENT_3D ( 'NONE', #28975, #46657, #46896 ) ;
#13649 = CARTESIAN_POINT ( 'NONE',  ( 0.2397010884053811242, -0.09842519685039370636, 0.000000000000000000 ) ) ;
#13650 = CARTESIAN_POINT ( 'NONE',  ( 0.1270800023317771588, -0.5669729434413133262, -0.1270800023317771588 ) ) ;
#13651 = FACE_OUTER_BOUND ( 'NONE', #45015, .T. ) ;
#13652 = CARTESIAN_POINT ( 'NONE',  ( -0.9873396505805591694, -0.1113553986120547346, 0.9399606298137322957 ) ) ;
#13653 = CARTESIAN_POINT ( 'NONE',  ( -1.033464566929134687, 0.06523048226347956391, 0.7603346456692923194 ) ) ;
#13654 = CARTESIAN_POINT ( 'NONE',  ( -0.1574803149606299191, -0.1456692913385826960, 0.000000000000000000 ) ) ;
#13655 = ORIENTED_EDGE ( 'NONE', *, *, #33256, .T. ) ;
#13656 = CARTESIAN_POINT ( 'NONE',  ( 0.9873396505805591694, 0.1113553986120547346, 1.815944881782236120 ) ) ;
#13657 = CARTESIAN_POINT ( 'NONE',  ( 1.033464566929133799, 0.000000000000000000, 0.8366141732283465249 ) ) ;
#13658 = CARTESIAN_POINT ( 'NONE',  ( -0.9873396505805591694, 0.1113553986120547346, 1.235236220472440971 ) ) ;
#13660 = CARTESIAN_POINT ( 'NONE',  ( 0.7646288533564489232, 0.1113553986120547346, 1.520669291338582640 ) ) ;
#13659 = CARTESIAN_POINT ( 'NONE',  ( 0.1154865254643520911, 0.2288180556977880420, -0.02742975588280811144 ) ) ;
#13661 = CARTESIAN_POINT ( 'NONE',  ( 0.9412147342319837628, -0.1574803149606297803, 0.2288385825696384601 ) ) ;
#13662 = EDGE_LOOP ( 'NONE', ( #45052, #25788, #10730, #43452, #1111 ) ) ;
#13663 = VERTEX_POINT ( 'NONE', #44914 ) ;
#13664 = CARTESIAN_POINT ( 'NONE',  ( 0.7185039370078741827, -0.06523048226347841205, 0.3764763778452291376 ) ) ;
#13665 = CARTESIAN_POINT ( 'NONE',  ( -1.094772975963752103E-17, -0.5270669290800944484, -0.1787899950787401882 ) ) ;
#13666 = CARTESIAN_POINT ( 'NONE',  ( -0.1264236179284866091, -1.422736220418677311, -0.1264236179284866091 ) ) ;
#13667 = EDGE_LOOP ( 'NONE', ( #11357, #46208, #10113, #2249 ) ) ;
#13668 = ORIENTED_EDGE ( 'NONE', *, *, #6617, .T. ) ;
#13669 = CARTESIAN_POINT ( 'NONE',  ( -0.6971942568897648851, 0.07405724077823318263, 1.382874015694268044 ) ) ;
#13670 = CARTESIAN_POINT ( 'NONE',  ( 0.9500414927467378812, -0.1787899950787401604, 1.555118110182455382 ) ) ;
#13671 = VERTEX_POINT ( 'NONE', #4666 ) ;
#13672 = CARTESIAN_POINT ( 'NONE',  ( 0.000000000000000000, -0.09842519685039370636, 0.000000000000000000 ) ) ;
#13673 = CARTESIAN_POINT ( 'NONE',  ( -0.8759842519685039353, 0.1787899950787401882, 0.7062007873478109987 ) ) ;
#13674 = EDGE_CURVE ( 'NONE', #14505, #13621, #21086, .T. ) ;
#13675 = DIRECTION ( 'NONE',  ( 0.000000000000000000, -1.000000000000000000, 0.000000000000000000 ) ) ;
#13676 = CARTESIAN_POINT ( 'NONE',  ( -1.054774247047244096, 0.000000000000000000, 0.6126968503399370380 ) ) ;
#13677 = CARTESIAN_POINT ( 'NONE',  ( 0.2020936974007922493, -0.07057211410380534455, 0.1687521643630704726 ) ) ;
#13678 = CARTESIAN_POINT ( 'NONE',  ( -1.033464566929134687, -0.06523048226347956391, 0.8735236220472449853 ) ) ;
#13679 = VERTEX_POINT ( 'NONE', #23384 ) ;
#13680 = VERTEX_POINT ( 'NONE', #1544 ) ;
#13681 = DIRECTION ( 'NONE',  ( 0.000000000000000000, 0.000000000000000000, 1.000000000000000000 ) ) ;
#13683 = ( BOUNDED_CURVE ( )  B_SPLINE_CURVE ( 2, ( #31038, #45605, #42001, #23825, #46085, #42947, #28144, #25240, #39597 ),
 .UNSPECIFIED., .F., .T. ) 
 B_SPLINE_CURVE_WITH_KNOTS ( ( 3, 2, 2, 2, 3 ),
 ( 0.04000000000000000083, 0.04250000000000000305, 0.04499999999999999833, 0.04750000000000000056, 0.05000000000000000278 ),
 .UNSPECIFIED. ) 
 CURVE ( )  GEOMETRIC_REPRESENTATION_ITEM ( )  RATIONAL_B_SPLINE_CURVE ( ( 1.000000000000000000, 0.9238795325112869605, 1.000000000000000000, 0.9238795325112869605, 1.000000000000000000, 0.9238795325112869605, 1.000000000000000000, 0.9238795325112869605, 1.000000000000000000 ) ) 
 REPRESENTATION_ITEM ( '' )  ) ;
#13682 = CARTESIAN_POINT ( 'NONE',  ( -0.8107537697050253289, -0.1574803149606297803, 1.493602362204724754 ) ) ;
#13684 = CARTESIAN_POINT ( 'NONE',  ( -0.9873396505805591694, 0.1113553986120547346, 0.5265748031496062520 ) ) ;
#13685 = AXIS2_PLACEMENT_3D ( 'NONE', #38541, #24396, #9786 ) ;
#13686 = EDGE_CURVE ( 'NONE', #9939, #42894, #30132, .T. ) ;
#13687 = CARTESIAN_POINT ( 'NONE',  ( 0.6971942568897648851, -0.07405724077823297447, 1.309055118056473122 ) ) ;
#13688 = CARTESIAN_POINT ( 'NONE',  ( 0.2037444935048909334, -0.09851384560802105284, 0.05109213554274055769 ) ) ;
#13689 = EDGE_LOOP ( 'NONE', ( #9501, #44712, #46621, #5691 ) ) ;
#13690 = CARTESIAN_POINT ( 'NONE',  ( -1.033464566929133799, 0.000000000000000000, 0.9448818896562519720 ) ) ;
#13691 = AXIS2_PLACEMENT_3D ( 'NONE', #19345, #30415, #44964 ) ;
#13692 = CARTESIAN_POINT ( 'NONE',  ( 0.1787899950787401604, -1.687131842244987023, -0.07405724077823318263 ) ) ;
#13693 = VERTEX_POINT ( 'NONE', #30829 ) ;
#13694 = CARTESIAN_POINT ( 'NONE',  ( 0.1264236179284866091, -0.5369094487651339120, 0.1264236179284866091 ) ) ;
#13695 = AXIS2_PLACEMENT_3D ( 'NONE', #41580, #24127, #9020 ) ;
#13696 = CARTESIAN_POINT ( 'NONE',  ( 0.9873396505805591694, 0.1113553986120547346, 0.8021653543307086798 ) ) ;
#13697 = DIRECTION ( 'NONE',  ( 1.822029033848725028E-16, 0.000000000000000000, 1.000000000000000000 ) ) ;
#13698 = ORIENTED_EDGE ( 'NONE', *, *, #39533, .F. ) ;
#13699 = CARTESIAN_POINT ( 'NONE',  ( 0.9500414927467378812, -0.1787899950787401604, 1.432086614119464141 ) ) ;
#13700 = DIRECTION ( 'NONE',  ( 1.000000000000000000, 0.000000000000000000, -0.000000000000000000 ) ) ;
#13701 = CARTESIAN_POINT ( 'NONE',  ( 0.1787899950787401604, -0.2588582676627719792, -0.07405724077823318263 ) ) ;
#13702 = DIRECTION ( 'NONE',  ( -1.000000000000000000, 3.469446951953613794E-15, 0.000000000000000000 ) ) ;
#13703 = CARTESIAN_POINT ( 'NONE',  ( -0.7185039370078760701, -0.06523048226348075740, 0.9670275589475921807 ) ) ;
#13704 = CARTESIAN_POINT ( 'NONE',  ( 1.054774247047244540, 0.07405724077823318263, 1.678149606245448622 ) ) ;
#13705 = CARTESIAN_POINT ( 'NONE',  ( 0.8759842519685039353, -0.1787899950787401882, 0.2485236219934806867 ) ) ;
#13706 = CARTESIAN_POINT ( 'NONE',  ( 3.284318927891251994E-17, 0.07221855145580058366, 0.1787899950787401882 ) ) ;
#13707 = CARTESIAN_POINT ( 'NONE',  ( -0.07405724077823318263, 0.08070866147108628208, 0.1787899950787401604 ) ) ;
#13708 = CARTESIAN_POINT ( 'NONE',  ( 0.8759842519685039353, 0.000000000000000000, 4.498031496062992574 ) ) ;
#13709 = CARTESIAN_POINT ( 'NONE',  ( -0.8070866141732283561, 0.000000000000000000, -0.7574803149606299524 ) ) ;
#13710 = B_SPLINE_CURVE_WITH_KNOTS ( 'NONE', 3,
 ( #12644, #5417, #13115, #34215, #27748, #15277, #3546, #8068, #11216, #44014, #33034, #11927, #32798 ),
 .UNSPECIFIED., .F., .F.,
 ( 4, 2, 2, 1, 2, 2, 4 ),
 ( 0.000000000000000000, 0.2500000000000013323, 0.3750000000000019984, 0.4375000000000021649, 0.4687500000000021649, 0.5000000000000021094, 1.000000000000000000 ),
 .UNSPECIFIED. ) ;
#13711 = CARTESIAN_POINT ( 'NONE',  ( 0.8019270111902717657, 0.1787899950787401604, 0.5856299212060785964 ) ) ;
#13712 = CARTESIAN_POINT ( 'NONE',  ( -0.8759842519685039353, 0.1787899950787401882, 0.8243110235682834519 ) ) ;
#13713 = AXIS2_PLACEMENT_3D ( 'NONE', #39114, #35550, #29584 ) ;
#13715 = CARTESIAN_POINT ( 'NONE',  ( 0.9873396505805591694, 0.1113553986120547346, 1.697834645561763889 ) ) ;
#13714 = CARTESIAN_POINT ( 'NONE',  ( 0.06523048226347956391, -0.8666338582677162172, -0.1574803149606300301 ) ) ;
#13716 = CARTESIAN_POINT ( 'NONE',  ( 0.07444174185955065859, -1.721008376512180860, 0.1797182628040039087 ) ) ;
#13717 = CARTESIAN_POINT ( 'NONE',  ( -1.094772975963752103E-17, -0.3252952755367877757, -0.1787899950787401882 ) ) ;
#13718 = CARTESIAN_POINT ( 'NONE',  ( 0.1968503937007874682, 0.06245656531175267784, -0.1492449156640648367 ) ) ;
#13719 = CARTESIAN_POINT ( 'NONE',  ( 1.054774247047244540, -0.07405724077823318263, 1.599409448765135133 ) ) ;
#13721 = CARTESIAN_POINT ( 'NONE',  ( -0.7185039370078739607, 1.928577636452523993E-17, 1.801181102362204633 ) ) ;
#13720 = CARTESIAN_POINT ( 'NONE',  ( 0.2082510178750321406, 0.06746187776208821540, -0.1651992896369783026 ) ) ;
#13722 = CARTESIAN_POINT ( 'NONE',  ( 0.6971942568897637749, 2.189545951927499583E-17, 0.3174212597887562382 ) ) ;
#13723 = ORIENTED_EDGE ( 'NONE', *, *, #10246, .T. ) ;
#13724 = DIRECTION ( 'NONE',  ( 0.000000000000000000, 0.000000000000000000, 1.000000000000000000 ) ) ;
#13725 = CARTESIAN_POINT ( 'NONE',  ( 0.1264236179284866091, -0.05954724404072461036, -0.1264236179284866091 ) ) ;
#13726 = CONICAL_SURFACE ( 'NONE', #31375, 0.09842519685039370636, 0.9599310885968824758 ) ;
#13727 = CARTESIAN_POINT ( 'NONE',  ( 1.054774247047244540, -0.07405724077823318263, 0.5314960629383620461 ) ) ;
#13728 = CARTESIAN_POINT ( 'NONE',  ( 0.07405724077823318263, -0.8543307086076546986, 0.1787899950787401604 ) ) ;
#13729 = CARTESIAN_POINT ( 'NONE',  ( -0.4620708661417322616, 0.9842519685039370358, -1.186023622047243986 ) ) ;
#13730 = CARTESIAN_POINT ( 'NONE',  ( -0.9412147342319837628, -0.1574803149606297803, 1.528051180994836056 ) ) ;
#13731 = CARTESIAN_POINT ( 'NONE',  ( 1.054774247047244540, 0.07405724077823318263, 0.5364173227808820554 ) ) ;
#13732 = CARTESIAN_POINT ( 'NONE',  ( -0.8019270111902717657, -0.1787899950787401604, 1.466535433017102763 ) ) ;
#13733 = ORIENTED_EDGE ( 'NONE', *, *, #40721, .T. ) ;
#13734 = CARTESIAN_POINT ( 'NONE',  ( 1.033464566929134687, -0.06523048226347956391, 0.4404527559055117503 ) ) ;
#13735 = CARTESIAN_POINT ( 'NONE',  ( 1.054774247047244540, 0.07405724077823318263, 1.171259842465921741 ) ) ;
#13736 = CARTESIAN_POINT ( 'NONE',  ( -0.06523048226347956391, -1.152066929026331676, 0.1574803149606297803 ) ) ;
#13737 = LINE ( 'NONE', #28379, #43857 ) ;
#13738 = CARTESIAN_POINT ( 'NONE',  ( 0.8019270111902717657, -0.1787899950787401604, 1.820866141678520789 ) ) ;
#13739 = CARTESIAN_POINT ( 'NONE',  ( -0.7185039370078746268, 0.06523048226347956391, 1.365649606299211838 ) ) ;
#13740 = CARTESIAN_POINT ( 'NONE',  ( -1.054774247047244540, 0.07405724077823318263, 0.8907480314422986378 ) ) ;
#13741 = ADVANCED_FACE ( 'NONE', ( #40840 ), #11891, .T. ) ;
#13742 = CARTESIAN_POINT ( 'NONE',  ( -0.8759842519685039353, 0.1574803149606299191, 0.5216535431995598104 ) ) ;
#13743 = CARTESIAN_POINT ( 'NONE',  ( -0.5555748031496058337, 0.2597269656108975311, 0.5511811023622046335 ) ) ;
#13744 = CARTESIAN_POINT ( 'NONE',  ( 0.7495606340400177148, 0.1264236179284866091, 0.1205708660879689087 ) ) ;
#13745 = CARTESIAN_POINT ( 'NONE',  ( 0.9873396505805591694, -0.1113553986120547346, 1.648622047136566904 ) ) ;
#13746 = ORIENTED_EDGE ( 'NONE', *, *, #34263, .F. ) ;
#13747 = EDGE_CURVE ( 'NONE', #649, #15059, #45398, .T. ) ;
#13748 = ORIENTED_EDGE ( 'NONE', *, *, #33855, .F. ) ;
#13749 = CARTESIAN_POINT ( 'NONE',  ( 0.9500414927467378812, -0.1787899950787401604, 0.7677165353793073965 ) ) ;
#13750 = ADVANCED_FACE ( 'NONE', ( #19293 ), #40493, .T. ) ;
#13751 = CARTESIAN_POINT ( 'NONE',  ( -0.9500414927467377701, -0.1787899950787401604, 1.707677165300568456 ) ) ;
#13752 = EDGE_CURVE ( 'NONE', #22068, #12322, #28834, .T. ) ;
#13753 = ORIENTED_EDGE ( 'NONE', *, *, #40538, .T. ) ;
#13754 = DIRECTION ( 'NONE',  ( 1.000000000000000000, 0.000000000000000000, 0.000000000000000000 ) ) ;
#13755 = VECTOR ( 'NONE', #37180, 39.37007874015748143 ) ;
#13756 = DIRECTION ( 'NONE',  ( 0.000000000000000000, -1.000000000000000000, 0.000000000000000000 ) ) ;
#13757 = CARTESIAN_POINT ( 'NONE',  ( -1.094772975963752103E-17, -1.207309007599316919, -0.1787899950787401882 ) ) ;
#13758 = EDGE_LOOP ( 'NONE', ( #45992, #34616, #19268, #17011 ) ) ;
#13759 = CARTESIAN_POINT ( 'NONE',  ( 0.1264236179284866091, -0.09399606293836260118, -0.1264236179284866091 ) ) ;
#13760 = ORIENTED_EDGE ( 'NONE', *, *, #24727, .F. ) ;
#13761 = DIRECTION ( 'NONE',  ( 6.944548107256202097E-15, 0.7880107536067212370, -0.6156614753256591799 ) ) ;
#13762 = AXIS2_PLACEMENT_3D ( 'NONE', #39549, #6722, #14171 ) ;
#13763 = FACE_OUTER_BOUND ( 'NONE', #30767, .T. ) ;
#13764 = CARTESIAN_POINT ( 'NONE',  ( 0.8759842519685039353, -0.1787899950787401882, 0.09104330703285078152 ) ) ;
#13765 = APPLICATION_CONTEXT ( 'automotive_design' ) ;
#13766 = CARTESIAN_POINT ( 'NONE',  ( 0.1787899950787401604, -1.444881889710016631, 0.07405724077823318263 ) ) ;
#13767 = VERTEX_POINT ( 'NONE', #37754 ) ;
#13768 = CARTESIAN_POINT ( 'NONE',  ( -0.6971942568897626646, -0.07405724077823297447, 0.3248031495525359746 ) ) ;
#13769 = CARTESIAN_POINT ( 'NONE',  ( -0.7185039370078739607, 1.928577636452523993E-17, 1.948818897530267602 ) ) ;
#13770 = CARTESIAN_POINT ( 'NONE',  ( 0.6971942568897648851, -0.07405724077823297447, 1.190944881836001112 ) ) ;
#13771 = CARTESIAN_POINT ( 'NONE',  ( 1.054774247047244096, 0.000000000000000000, 1.518208661363559031 ) ) ;
#13772 = CARTESIAN_POINT ( 'NONE',  ( 0.7495606340400177148, -0.1264236179284866091, 0.1648622046706460786 ) ) ;
#13773 = CARTESIAN_POINT ( 'NONE',  ( 0.1574803149606299746, 0.4003652867858630282, 0.7276473417831955670 ) ) ;
#13774 = CARTESIAN_POINT ( 'NONE',  ( 0.8107537697050254399, -0.1574803149606297803, 0.8932086613097963701 ) ) ;
#13775 = CARTESIAN_POINT ( 'NONE',  ( 0.1610681367838507072, -0.07955608858867080357, -0.1377952755905511584 ) ) ;
#13776 = CARTESIAN_POINT ( 'NONE',  ( -0.7185039370078739607, 1.928577636452523993E-17, 1.279527558947590515 ) ) ;
#13777 = CARTESIAN_POINT ( 'NONE',  ( -0.9412147342319837628, 0.1574803149606300301, 1.739665354223181470 ) ) ;
#13778 = CARTESIAN_POINT ( 'NONE',  ( 0.6971942568897626646, -0.07405724077823297447, 0.1624015747493861295 ) ) ;
#13779 = CARTESIAN_POINT ( 'NONE',  ( 0.7185039370078766252, -0.06523048226348168721, 1.646161417322834497 ) ) ;
#13781 = CYLINDRICAL_SURFACE ( 'NONE', #42201, 0.1574803149606299191 ) ;
#13780 = CARTESIAN_POINT ( 'NONE',  ( 0.7495606340400177148, 0.1264236179284866091, 1.139271653489543290 ) ) ;
#13782 = VECTOR ( 'NONE', #6892, 39.37007874015748143 ) ;
#13783 = CARTESIAN_POINT ( 'NONE',  ( 1.054774247047244096, 0.000000000000000000, 1.956200787347811110 ) ) ;
#13784 = CARTESIAN_POINT ( 'NONE',  ( 0.7185039370078739607, 1.928577636452523993E-17, 0.4921259841444416971 ) ) ;
#13785 = ORIENTED_EDGE ( 'NONE', *, *, #38260, .F. ) ;
#13786 = LINE ( 'NONE', #32501, #45971 ) ;
#13787 = PRODUCT_DEFINITION_SHAPE ( 'NONE', 'NONE',  #47470 ) ;
#13788 = CARTESIAN_POINT ( 'NONE',  ( -1.033464566929134687, -0.06523048226347956391, 0.3912401573727880555 ) ) ;
#13789 = AXIS2_PLACEMENT_3D ( 'NONE', #24337, #38936, #19552 ) ;
#13790 = ORIENTED_EDGE ( 'NONE', *, *, #8708, .T. ) ;
#13791 = CARTESIAN_POINT ( 'NONE',  ( 0.8019270111902717657, -0.1787899950787401604, 1.505905511757261284 ) ) ;
#13793 = CARTESIAN_POINT ( 'NONE',  ( 0.000000000000000000, 0.1473293504822035527, -0.9532488779249704836 ) ) ;
#13792 = CARTESIAN_POINT ( 'NONE',  ( -1.033464566929133799, 0.000000000000000000, 0.4330708660342047489 ) ) ;
#13794 = VECTOR ( 'NONE', #1416, 39.37007874015748143 ) ;
#13795 = EDGE_LOOP ( 'NONE', ( #27097, #46225, #17036, #10470 ) ) ;
#13796 = CARTESIAN_POINT ( 'NONE',  ( 0.9873396505805591694, 0.1113553986120547346, 0.7234251968503936370 ) ) ;
#13797 = ( BOUNDED_CURVE ( )  B_SPLINE_CURVE ( 2, ( #33667, #780, #44628, #11843, #25760, #22137, #12082, #26470, #4861 ),
 .UNSPECIFIED., .F., .T. ) 
 B_SPLINE_CURVE_WITH_KNOTS ( ( 3, 2, 2, 2, 3 ),
 ( 0.1300000000000000044, 0.1325000000000000067, 0.1350000000000000089, 0.1375000000000000111, 0.1400000000000000133 ),
 .UNSPECIFIED. ) 
 CURVE ( )  GEOMETRIC_REPRESENTATION_ITEM ( )  RATIONAL_B_SPLINE_CURVE ( ( 1.000000000000000000, 0.9238795325112869605, 1.000000000000000000, 0.9238795325112869605, 1.000000000000000000, 0.9238795325112869605, 1.000000000000000000, 0.9238795325112869605, 1.000000000000000000 ) ) 
 REPRESENTATION_ITEM ( '' )  ) ;
#13798 = ADVANCED_FACE ( 'NONE', ( #41542 ), #38227, .T. ) ;
#13799 = VERTEX_POINT ( 'NONE', #4909 ) ;
#13800 = CARTESIAN_POINT ( 'NONE',  ( 0.1607584476970183585, 0.09202339627321219628, 0.1926191378137618593 ) ) ;
#13801 = DIRECTION ( 'NONE',  ( 1.822029033848725028E-16, 0.000000000000000000, 1.000000000000000000 ) ) ;
#13802 = ORIENTED_EDGE ( 'NONE', *, *, #1297, .F. ) ;
#13803 = CARTESIAN_POINT ( 'NONE',  ( 0.8759842519685039353, 0.1787899950787401882, 0.5093503936470236138 ) ) ;
#13804 = AXIS2_PLACEMENT_3D ( 'NONE', #45715, #24184, #19862 ) ;
#13805 = ORIENTED_EDGE ( 'NONE', *, *, #27645, .T. ) ;
#13806 = CARTESIAN_POINT ( 'NONE',  ( -0.8019270111902716547, -0.1787899950787401604, 1.427165354276944687 ) ) ;
#13807 = CARTESIAN_POINT ( 'NONE',  ( 0.07405724077823318263, -1.749999999946236340, -0.1787899950787401604 ) ) ;
#13808 = CARTESIAN_POINT ( 'NONE',  ( -0.7495606340400177148, -0.1264236179284866091, 1.114665354276944909 ) ) ;
#13809 = CARTESIAN_POINT ( 'NONE',  ( -0.8019270111902717657, -0.1787899950787401604, 1.938976377898990799 ) ) ;
#13810 = ORIENTED_EDGE ( 'NONE', *, *, #37885, .F. ) ;
#13811 = CARTESIAN_POINT ( 'NONE',  ( -0.6971942568897648851, 0.07405724077823318263, 1.102362204670646495 ) ) ;
#13812 = EDGE_CURVE ( 'NONE', #3096, #5551, #21348, .T. ) ;
#13813 = CARTESIAN_POINT ( 'NONE',  ( -0.9412147342319837628, -0.1574803149606297803, 0.3567913385826773087 ) ) ;
#13814 = DIRECTION ( 'NONE',  ( 1.000000000000000000, 0.000000000000000000, 0.000000000000000000 ) ) ;
#13815 = CARTESIAN_POINT ( 'NONE',  ( -0.1787899950787401604, -0.7274861729536492572, -0.07405724077823318263 ) ) ;
#13816 = EDGE_LOOP ( 'NONE', ( #35048, #13143, #3510, #34672, #35171 ) ) ;
#13817 = CARTESIAN_POINT ( 'NONE',  ( 0.08374778445418129547, -0.08956243157244035691, 0.1193195044654234288 ) ) ;
#13818 = DIRECTION ( 'NONE',  ( 0.000000000000000000, 0.000000000000000000, -1.000000000000000000 ) ) ;
#13819 = ORIENTED_EDGE ( 'NONE', *, *, #45806, .F. ) ;
#13820 = CARTESIAN_POINT ( 'NONE',  ( 0.9873396505805591694, 0.1113553986120547346, 0.7627952755905511584 ) ) ;
#13821 = LINE ( 'NONE', #25080, #21094 ) ;
#13822 = ( BOUNDED_CURVE ( )  B_SPLINE_CURVE ( 2, ( #19258, #37001, #44401, #25764, #19010, #11618, #33674, #33913, #26475 ),
 .UNSPECIFIED., .F., .F. ) 
 B_SPLINE_CURVE_WITH_KNOTS ( ( 3, 2, 2, 2, 3 ),
 ( 0.05999999999999999778, 0.06250000000000000000, 0.06500000000000000222, 0.06750000000000000444, 0.07000000000000000666 ),
 .UNSPECIFIED. ) 
 CURVE ( )  GEOMETRIC_REPRESENTATION_ITEM ( )  RATIONAL_B_SPLINE_CURVE ( ( 1.000000000000000000, 0.9238795325112869605, 1.000000000000000000, 0.9238795325112869605, 1.000000000000000000, 0.9238795325112869605, 1.000000000000000000, 0.9238795325112869605, 1.000000000000000000 ) ) 
 REPRESENTATION_ITEM ( '' )  ) ;
#13823 = CARTESIAN_POINT ( 'NONE',  ( -0.8759842519685039353, -0.1787899950787401882, 0.5634842519147401640 ) ) ;
#13824 = LINE ( 'NONE', #42783, #19226 ) ;
#13825 = EDGE_LOOP ( 'NONE', ( #33422, #23805, #23782, #27229 ) ) ;
#13826 = CARTESIAN_POINT ( 'NONE',  ( -1.054774247047244096, 0.000000000000000000, 1.601870078686393750 ) ) ;
#13827 = AXIS2_PLACEMENT_3D ( 'NONE', #5591, #16844, #41749 ) ;
#13828 = AXIS2_PLACEMENT_3D ( 'NONE', #45149, #44911, #38217 ) ;
#13829 = CARTESIAN_POINT ( 'NONE',  ( 0.3849708276051176936, 0.09842519685039370636, 0.000000000000000000 ) ) ;
#13830 = DIRECTION ( 'NONE',  ( 0.000000000000000000, 1.000000000000000000, 0.000000000000000000 ) ) ;
#13831 = CARTESIAN_POINT ( 'NONE',  ( 0.9873396505805591694, -0.1113553986120547346, 0.5954724409448819422 ) ) ;
#13832 = CARTESIAN_POINT ( 'NONE',  ( 0.1797182628040039087, -0.8893154631263514576, 0.07444174185955046430 ) ) ;
#13833 = CARTESIAN_POINT ( 'NONE',  ( -0.7185039370078746268, 0.06523048226347956391, 0.9719488188976379561 ) ) ;
#13834 = CARTESIAN_POINT ( 'NONE',  ( 0.1113553986120547346, -0.5541338582677165503, -0.1113553986120547346 ) ) ;
#13835 = DIRECTION ( 'NONE',  ( 0.000000000000000000, 0.000000000000000000, 1.000000000000000000 ) ) ;
#13836 = FACE_OUTER_BOUND ( 'NONE', #40267, .T. ) ;
#13837 = CARTESIAN_POINT ( 'NONE',  ( 1.033464566929133799, 0.000000000000000000, 1.269685039370078705 ) ) ;
#13839 = ( NAMED_UNIT ( * ) SI_UNIT ( $, .STERADIAN. ) SOLID_ANGLE_UNIT ( ) ) ;
#13838 = CARTESIAN_POINT ( 'NONE',  ( 0.7790738941308391619, -0.1411882674591699027, 1.986291969488682252 ) ) ;
#13840 = CARTESIAN_POINT ( 'NONE',  ( 0.7185039370078746268, -0.06523048226347956391, 1.843011811023621327 ) ) ;
#13841 = CARTESIAN_POINT ( 'NONE',  ( 0.06523048226347956391, -0.6599409447743623813, -0.1574803149606300301 ) ) ;
#13843 = CARTESIAN_POINT ( 'NONE',  ( 0.8107537697050234415, -0.1574803149606297803, 0.2632874014672759722 ) ) ;
#13842 = CARTESIAN_POINT ( 'NONE',  ( 1.054774247047244540, 0.07405724077823318263, 0.6151574802611965431 ) ) ;
#13844 = DIRECTION ( 'NONE',  ( 1.822029033848725028E-16, 0.000000000000000000, 1.000000000000000000 ) ) ;
#13845 = CARTESIAN_POINT ( 'NONE',  ( -0.07405724077823318263, -0.6230314960092281362, 0.1787899950787401604 ) ) ;
#13846 = CARTESIAN_POINT ( 'NONE',  ( 0.1476377952755906220, -0.4950321721878526704, -0.8627979602685659222 ) ) ;
#13847 = ORIENTED_EDGE ( 'NONE', *, *, #1262, .T. ) ;
#13848 = CARTESIAN_POINT ( 'NONE',  ( 0.7185039370078739607, 1.928577636452523993E-17, 0.6102362203649134287 ) ) ;
#13849 = FACE_OUTER_BOUND ( 'NONE', #17685, .T. ) ;
#13850 = CARTESIAN_POINT ( 'NONE',  ( 0.6971942568897637749, 2.189545951927499583E-17, 0.7898622046706456068 ) ) ;
#13851 = ORIENTED_EDGE ( 'NONE', *, *, #4362, .F. ) ;
#13852 = CARTESIAN_POINT ( 'NONE',  ( 1.033464566929134687, 0.06523048226347956391, 1.468996062992126150 ) ) ;
#13853 = DIRECTION ( 'NONE',  ( -1.000000000000000000, 0.000000000000000000, 0.000000000000000000 ) ) ;
#13854 = CARTESIAN_POINT ( 'NONE',  ( -0.1797182628040039087, 0.03588138726734815126, -0.07444174185955065859 ) ) ;
#13855 = CARTESIAN_POINT ( 'NONE',  ( -0.07405724077823318263, -1.036417322780882833, -0.1787899950787401604 ) ) ;
#13856 = CARTESIAN_POINT ( 'NONE',  ( 0.1574803149606300301, -1.585137795275590955, 0.06523048226347956391 ) ) ;
#13857 = CARTESIAN_POINT ( 'NONE',  ( 2.700008691033534577E-17, 0.0004086818895575684884, 0.2204724409448818867 ) ) ;
#13858 = EDGE_CURVE ( 'NONE', #40321, #2019, #34181, .T. ) ;
#13859 = CIRCLE ( 'NONE', #10801, 0.7874015748031437667 ) ;
#13860 = CARTESIAN_POINT ( 'NONE',  ( -0.6971942568897626646, -0.07405724077823297447, 0.08366141726907129483 ) ) ;
#13861 = ORIENTED_EDGE ( 'NONE', *, *, #1947, .T. ) ;
#13862 = CARTESIAN_POINT ( 'NONE',  ( -0.7646288533564489232, -0.1113553986120547346, 0.8120078739082204899 ) ) ;
#13863 = ORIENTED_EDGE ( 'NONE', *, *, #9426, .F. ) ;
#13864 = CARTESIAN_POINT ( 'NONE',  ( -1.054774247047244540, -0.07405724077823318263, 1.953740157426552715 ) ) ;
#13865 = VECTOR ( 'NONE', #40632, 39.37007874015748143 ) ;
#13866 = CARTESIAN_POINT ( 'NONE',  ( -0.7495606340400177148, -0.1264236179284866091, 1.464074803095842370 ) ) ;
#13867 = CARTESIAN_POINT ( 'NONE',  ( 0.9500414927467377701, -0.1787899950787401604, 0.8858267715997791836 ) ) ;
#13868 = EDGE_CURVE ( 'NONE', #480, #10797, #15965, .T. ) ;
#13869 = CIRCLE ( 'NONE', #11587, 0.1673228346456689108 ) ;
#13870 = CARTESIAN_POINT ( 'NONE',  ( -1.002407869896990045, 0.1264236179284866091, 0.2682086613635594752 ) ) ;
#13871 = CARTESIAN_POINT ( 'NONE',  ( -0.9500414927467378812, -0.1787899950787401604, 1.909448818843873186 ) ) ;
#13872 = CARTESIAN_POINT ( 'NONE',  ( -0.8107537697050253289, 0.1574803149606300301, 1.833169291338582418 ) ) ;
#13873 = CARTESIAN_POINT ( 'NONE',  ( -1.033464566929133799, 0.000000000000000000, 1.899606299212598604 ) ) ;
#13874 = CARTESIAN_POINT ( 'NONE',  ( 3.284318927891251994E-17, -0.2033719997253019829, 0.1787899950787401882 ) ) ;
#13875 = VECTOR ( 'NONE', #29642, 39.37007874015748143 ) ;
#13876 = CARTESIAN_POINT ( 'NONE',  ( -0.1717103871139409321, -0.09842519685039370636, -0.03673106526238755637 ) ) ;
#13877 = CONTEXT_DEPENDENT_SHAPE_REPRESENTATION ( #6410, #10367 ) ;
#13878 = CARTESIAN_POINT ( 'NONE',  ( 1.033464566929133799, 0.000000000000000000, 0.1574803148531029595 ) ) ;
#13879 = CARTESIAN_POINT ( 'NONE',  ( -0.8019270111902717657, 0.1787899950787401604, 0.2312992125446618197 ) ) ;
#13880 = ORIENTED_EDGE ( 'NONE', *, *, #7041, .F. ) ;
#13881 = VERTEX_POINT ( 'NONE', #15489 ) ;
#13882 = CARTESIAN_POINT ( 'NONE',  ( -0.6971942568897648851, -0.07405724077823297447, 1.190944881836001112 ) ) ;
#13883 = ORIENTED_EDGE ( 'NONE', *, *, #26152, .T. ) ;
#13884 = CARTESIAN_POINT ( 'NONE',  ( -1.094772975963752103E-17, -1.117618110182456714, -0.1787899950787401882 ) ) ;
#13885 = EDGE_CURVE ( 'NONE', #22837, #3723, #42030, .T. ) ;
#13886 = CARTESIAN_POINT ( 'NONE',  ( -0.1787899950787401604, -1.454724409395055096, 0.07405724077823318263 ) ) ;
#13887 = VECTOR ( 'NONE', #12085, 39.37007874015748143 ) ;
#13888 = DIRECTION ( 'NONE',  ( 1.000000000000000000, -3.469446951953613794E-15, 0.000000000000000000 ) ) ;
#13889 = CARTESIAN_POINT ( 'NONE',  ( -0.4620708661417322616, 0.1864803149606299448, -0.7135826771653542844 ) ) ;
#13890 = CARTESIAN_POINT ( 'NONE',  ( -0.8107537697050253289, -0.1574803149606297803, 0.7062007874015745479 ) ) ;
#13891 = VECTOR ( 'NONE', #37761, 39.37007874015748143 ) ;
#13892 = AXIS2_PLACEMENT_3D ( 'NONE', #21219, #21709, #43737 ) ;
#13893 = CARTESIAN_POINT ( 'NONE',  ( 0.8107537697050253289, -0.1574803149606297803, 1.877460629813732407 ) ) ;
#13894 = ORIENTED_EDGE ( 'NONE', *, *, #46906, .F. ) ;
#13895 = CARTESIAN_POINT ( 'NONE',  ( -0.1574803149606299191, 0.3743908788525359688, -3.616772362661643481 ) ) ;
#13896 = CARTESIAN_POINT ( 'NONE',  ( 0.7646288533564489232, -0.1113553986120547346, 0.8218503937007874960 ) ) ;
#13897 = CARTESIAN_POINT ( 'NONE',  ( -0.5555748031496026140, 1.194414586609142903, -0.06082000038405787484 ) ) ;
#13898 = FACE_OUTER_BOUND ( 'NONE', #33571, .T. ) ;
#13899 = DIRECTION ( 'NONE',  ( -1.000000000000000000, 0.000000000000000000, 0.000000000000000000 ) ) ;
#13900 = CARTESIAN_POINT ( 'NONE',  ( 0.7646288533564489232, 0.1113553986120547346, 0.2116141731208196763 ) ) ;
#13901 = ORIENTED_EDGE ( 'NONE', *, *, #25577, .T. ) ;
#13902 = VERTEX_POINT ( 'NONE', #38220 ) ;
#13903 = DIRECTION ( 'NONE',  ( 0.000000000000000000, 0.000000000000000000, -1.000000000000000000 ) ) ;
#13904 = CARTESIAN_POINT ( 'NONE',  ( -0.06523048226347956391, -1.481791338475149322, -0.1574803149606300301 ) ) ;
#13905 = CARTESIAN_POINT ( 'NONE',  ( 0.1787899950787401604, -0.5393700786863945273, 0.07405724077823318263 ) ) ;
#13906 = CARTESIAN_POINT ( 'NONE',  ( 0.1574803149606299191, -0.9921259842519685179, -1.928577636452523993E-17 ) ) ;
#13907 = CARTESIAN_POINT ( 'NONE',  ( 0.8107537697050253289, -0.1574803149606297803, 0.7750984250893222516 ) ) ;
#13908 = DIRECTION ( 'NONE',  ( 0.000000000000000000, 0.7880107536067184615, -0.6156614753256628436 ) ) ;
#13909 = EDGE_CURVE ( 'NONE', #47403, #24855, #388, .T. ) ;
#13910 = CARTESIAN_POINT ( 'NONE',  ( -0.6971942568897626646, 0.07405724077823318263, 0.4330708660879683536 ) ) ;
#13911 = ORIENTED_EDGE ( 'NONE', *, *, #4049, .T. ) ;
#13912 = ORIENTED_EDGE ( 'NONE', *, *, #35276, .F. ) ;
#13913 = CARTESIAN_POINT ( 'NONE',  ( -0.6971942568897637749, 2.189545951927499583E-17, 1.424704724355685181 ) ) ;
#13914 = CARTESIAN_POINT ( 'NONE',  ( 0.6971942568897648851, 0.07405724077823318263, 1.500984251914741607 ) ) ;
#13915 = FACE_OUTER_BOUND ( 'NONE', #19759, .T. ) ;
#13916 = CARTESIAN_POINT ( 'NONE',  ( -1.054774247047244096, 0.000000000000000000, 0.6569881889226141247 ) ) ;
#13917 = CARTESIAN_POINT ( 'NONE',  ( 0.6971942568897626646, -0.07405724077823297447, 0.1673228345919059168 ) ) ;
#13918 = CARTESIAN_POINT ( 'NONE',  ( -1.033464566929133799, 0.000000000000000000, 1.692913385719244213 ) ) ;
#13919 = CARTESIAN_POINT ( 'NONE',  ( 1.054774247047244540, -0.07405724077823318263, 0.7332677164816705506 ) ) ;
#13920 = CARTESIAN_POINT ( 'NONE',  ( -1.002407869896990045, -0.1264236179284866091, 0.6865157479777322935 ) ) ;
#13921 = AXIS2_PLACEMENT_3D ( 'NONE', #19722, #31243, #45820 ) ;
#13922 = ADVANCED_FACE ( 'NONE', ( #5380 ), #17586, .F. ) ;
#13923 = CARTESIAN_POINT ( 'NONE',  ( 0.1986060025684610320, -0.07294156354275010967, 0.1707667409196649000 ) ) ;
#13924 = AXIS2_PLACEMENT_3D ( 'NONE', #9321, #42582, #31145 ) ;
#13925 = CARTESIAN_POINT ( 'NONE',  ( 1.033464566929134687, 0.06523048226347956391, 1.065452755797984041 ) ) ;
#13926 = CARTESIAN_POINT ( 'NONE',  ( -0.06523048226347956391, -0.1432086613097958705, -0.1574803149606300301 ) ) ;
#13927 = CARTESIAN_POINT ( 'NONE',  ( -0.8019270111902717657, -0.1787899950787401604, 1.432086614119464141 ) ) ;
#13928 = CARTESIAN_POINT ( 'NONE',  ( 0.1235961452251413406, -0.09842519685039370636, -0.2140748031496062798 ) ) ;
#13929 = CARTESIAN_POINT ( 'NONE',  ( -0.9412147342319837628, -0.1574803149606297803, 1.498523622047243764 ) ) ;
#13930 = CARTESIAN_POINT ( 'NONE',  ( -0.9873396505805591694, 0.1113553986120547346, 0.4084645669291339098 ) ) ;
#13931 = CARTESIAN_POINT ( 'NONE',  ( 1.054774247047244540, -0.07405724077823318263, 1.363188976324188673 ) ) ;
#13932 = AXIS2_PLACEMENT_3D ( 'NONE', #45338, #44620, #12554 ) ;
#13933 = ORIENTED_EDGE ( 'NONE', *, *, #16088, .F. ) ;
#13934 = AXIS2_PLACEMENT_3D ( 'NONE', #2804, #10505, #10018 ) ;
#13935 = CARTESIAN_POINT ( 'NONE',  ( -0.7185039370078739607, 1.928577636452523993E-17, 0.6200787401574803237 ) ) ;
#13936 = ( BOUNDED_CURVE ( )  B_SPLINE_CURVE ( 2, ( #30076, #7978, #14957, #21902, #29136, #7505, #47302, #44613, #22125 ),
 .UNSPECIFIED., .F., .T. ) 
 B_SPLINE_CURVE_WITH_KNOTS ( ( 3, 2, 2, 2, 3 ),
 ( 0.05500000000000000028, 0.05750000000000000250, 0.05999999999999999778, 0.06250000000000000000, 0.06500000000000000222 ),
 .UNSPECIFIED. ) 
 CURVE ( )  GEOMETRIC_REPRESENTATION_ITEM ( )  RATIONAL_B_SPLINE_CURVE ( ( 1.000000000000000000, 0.9238795325112869605, 1.000000000000000000, 0.9238795325112869605, 1.000000000000000000, 0.9238795325112869605, 1.000000000000000000, 0.9238795325112869605, 1.000000000000000000 ) ) 
 REPRESENTATION_ITEM ( '' )  ) ;
#13937 = ORIENTED_EDGE ( 'NONE', *, *, #19047, .F. ) ;
#13938 = CARTESIAN_POINT ( 'NONE',  ( 0.07405724077823318263, -0.6820866141194646959, -0.1787899950787401604 ) ) ;
#13939 = CARTESIAN_POINT ( 'NONE',  ( 0.7646288533564489232, -0.1113553986120547346, 0.3887795275590551491 ) ) ;
#13940 = ORIENTED_EDGE ( 'NONE', *, *, #5348, .T. ) ;
#13941 = CARTESIAN_POINT ( 'NONE',  ( 0.8759842519685039353, 0.1787899950787401882, 1.370570866087968520 ) ) ;
#13942 = LINE ( 'NONE', #36239, #6250 ) ;
#13943 = CARTESIAN_POINT ( 'NONE',  ( -1.094772975963752103E-17, -0.7977362204186770889, -0.1787899950787401882 ) ) ;
#13944 = CARTESIAN_POINT ( 'NONE',  ( 0.8759842519685039353, 0.000000000000000000, 4.498031496062992574 ) ) ;
#13945 = CARTESIAN_POINT ( 'NONE',  ( -0.9412147342319837628, -0.1574803149606297803, 0.9768700786326298680 ) ) ;
#13946 = CARTESIAN_POINT ( 'NONE',  ( 1.002407869896990045, -0.1264236179284866091, 0.3321850393163153226 ) ) ;
#13947 = CARTESIAN_POINT ( 'NONE',  ( -0.07405724077823318263, -0.1418562516938056128, -0.1787899950787401604 ) ) ;
#13948 = CARTESIAN_POINT ( 'NONE',  ( 0.2559055118110236116, -0.1349029091040385986, -0.2958118747041117436 ) ) ;
#13949 = CARTESIAN_POINT ( 'NONE',  ( 0.4028871391076110364, 0.08090551181102362266, 9.908067607274841931E-18 ) ) ;
#13950 = CARTESIAN_POINT ( 'NONE',  ( 0.8019270111902717657, 0.1787899950787401604, 0.5462598424659214080 ) ) ;
#13951 = VECTOR ( 'NONE', #43968, 39.37007874015748143 ) ;
#13952 = CARTESIAN_POINT ( 'NONE',  ( -1.054774247047244096, 0.000000000000000000, 1.011318897584031484 ) ) ;
#13954 = CARTESIAN_POINT ( 'NONE',  ( 0.9412147342319837628, 0.1574803149606300301, 0.9916338581601894520 ) ) ;
#13953 = FACE_OUTER_BOUND ( 'NONE', #11880, .T. ) ;
#13955 = CARTESIAN_POINT ( 'NONE',  ( -0.07444174185955065859, -1.765299715094856614, 0.1797182628040039087 ) ) ;
#13956 = CARTESIAN_POINT ( 'NONE',  ( -0.07405724077823318263, -0.4409448818359998357, -0.1787899950787401604 ) ) ;
#13957 = DIRECTION ( 'NONE',  ( 8.659560562358463011E-17, 0.7071067811862592478, -0.7071067811868357866 ) ) ;
#13958 = CARTESIAN_POINT ( 'NONE',  ( 1.054774247047244540, 0.07405724077823318263, 1.683070866087970074 ) ) ;
#13960 = CARTESIAN_POINT ( 'NONE',  ( -1.033464566929134687, -0.06523048226347956391, 1.818405511811023167 ) ) ;
#13959 = CARTESIAN_POINT ( 'NONE',  ( 0.7495606340400177148, -0.1264236179284866091, 1.936515747977732405 ) ) ;
#13961 = EDGE_CURVE ( 'NONE', #1966, #22011, #27933, .T. ) ;
#13962 = ORIENTED_EDGE ( 'NONE', *, *, #36802, .F. ) ;
#13963 = AXIS2_PLACEMENT_3D ( 'NONE', #33731, #15501, #44685 ) ;
#13964 = CARTESIAN_POINT ( 'NONE',  ( -0.2374471364664500761, -0.04193537623287351551, -0.1483429027089311902 ) ) ;
#13965 = CARTESIAN_POINT ( 'NONE',  ( 0.000000000000000000, -5.122214988120488358E-16, -8.878505979408856939E-16 ) ) ;
#13966 = CYLINDRICAL_SURFACE ( 'NONE', #16773, 0.1864803149606298893 ) ;
#13967 = CARTESIAN_POINT ( 'NONE',  ( 0.1787899950787401604, -0.1850393700249766959, 0.07405724077823318263 ) ) ;
#13968 = CARTESIAN_POINT ( 'NONE',  ( 0.9500414927467378812, -0.1787899950787401604, 0.6053149605761579677 ) ) ;
#13969 = CARTESIAN_POINT ( 'NONE',  ( 0.07405724077823318263, -1.115157480261196987, -0.1787899950787401604 ) ) ;
#13970 = CARTESIAN_POINT ( 'NONE',  ( 0.8759842519685039353, 0.1787899950787401882, 0.1156496062454492185 ) ) ;
#13971 = CARTESIAN_POINT ( 'NONE',  ( 1.033464566929133799, 0.000000000000000000, 1.968503936900346529 ) ) ;
#13972 = CARTESIAN_POINT ( 'NONE',  ( 0.8759842519685039353, 0.1787899950787401882, 0.5831692912848189803 ) ) ;
#13973 = CYLINDRICAL_SURFACE ( 'NONE', #30426, 0.02900000000000001882 ) ;
#13974 = CARTESIAN_POINT ( 'NONE',  ( -0.8019270111902717657, -0.1787899950787401604, 1.387795275536786610 ) ) ;
#13975 = ORIENTED_EDGE ( 'NONE', *, *, #29207, .T. ) ;
#13976 = CARTESIAN_POINT ( 'NONE',  ( -0.2927617443614863313, -0.1024931984611133912, -0.7432784081755305916 ) ) ;
#13977 = CARTESIAN_POINT ( 'NONE',  ( 1.054774247047244540, 0.07405724077823318263, 1.210629921206079818 ) ) ;
#13978 = CARTESIAN_POINT ( 'NONE',  ( -0.8759842519685039353, -0.1574803149606299191, 0.7381889762704251234 ) ) ;
#13979 = CARTESIAN_POINT ( 'NONE',  ( 0.2471922904502826812, -0.09842519685039370636, 0.1427165354330708902 ) ) ;
#13980 = CARTESIAN_POINT ( 'NONE',  ( 1.054774247047244096, 0.000000000000000000, 1.833169291284818758 ) ) ;
#13981 = CARTESIAN_POINT ( 'NONE',  ( -0.8019270111902717657, 0.1787899950787401604, 0.9005905511273389896 ) ) ;
#13982 = PLANE ( 'NONE',  #43447 ) ;
#13983 = DIRECTION ( 'NONE',  ( 0.000000000000000000, 0.000000000000000000, 1.000000000000000000 ) ) ;
#13984 = CARTESIAN_POINT ( 'NONE',  ( 1.002407869896990045, -0.1264236179284866091, 0.3764763778989925203 ) ) ;
#13985 = EDGE_CURVE ( 'NONE', #25810, #5177, #13523, .T. ) ;
#13986 = PRODUCT_DEFINITION_CONTEXT ( 'detailed design', #12252, 'design' ) ;
#13987 = CARTESIAN_POINT ( 'NONE',  ( -0.7495606340400177148, 0.1264236179284866091, 0.5487204723871811352 ) ) ;
#13988 = CARTESIAN_POINT ( 'NONE',  ( 0.8107537697050253289, 0.1574803149606300301, 1.547736220364914983 ) ) ;
#13989 = EDGE_LOOP ( 'NONE', ( #37680, #15341, #407, #37920, #30565, #1261, #25522, #22502 ) ) ;
#13990 = CARTESIAN_POINT ( 'NONE',  ( -1.094772975963752103E-17, 0.02411417328210995956, -0.1787899950787401882 ) ) ;
#13991 = CARTESIAN_POINT ( 'NONE',  ( 0.1997612633124547232, -0.1801620131153035542, -0.05546260682012722071 ) ) ;
#13992 = CARTESIAN_POINT ( 'NONE',  ( 0.8759842519685039353, -0.1787899950787401882, 0.8439960629383622681 ) ) ;
#13993 = CARTESIAN_POINT ( 'NONE',  ( -0.8759842519685039353, -0.1787899950787401882, 1.783956692859621995 ) ) ;
#13994 = ORIENTED_EDGE ( 'NONE', *, *, #13077, .F. ) ;
#13995 = AXIS2_PLACEMENT_3D ( 'NONE', #41526, #44901, #23368 ) ;
#13996 = CARTESIAN_POINT ( 'NONE',  ( -0.9873396505805591694, 0.1113553986120547346, 0.6446850393700788162 ) ) ;
#13997 = DIRECTION ( 'NONE',  ( -0.000000000000000000, 1.000000000000000000, -0.000000000000000000 ) ) ;
#13998 = CARTESIAN_POINT ( 'NONE',  ( -0.1787899950787401604, -1.239297196575694926, -0.07405724077823318263 ) ) ;
#13999 = ORIENTED_EDGE ( 'NONE', *, *, #14257, .F. ) ;
#14000 = CARTESIAN_POINT ( 'NONE',  ( -0.07405724077823318263, -0.2440944881352131168, -0.1787899950787401604 ) ) ;
#14001 = FACE_OUTER_BOUND ( 'NONE', #19415, .T. ) ;
#14002 = ORIENTED_EDGE ( 'NONE', *, *, #10121, .F. ) ;
#14003 = CIRCLE ( 'NONE', #10179, 0.02899999999999988351 ) ;
#14004 = CARTESIAN_POINT ( 'NONE',  ( -0.9412147342319837628, -0.1574803149606297803, 1.213090551073575662 ) ) ;
#14005 = CARTESIAN_POINT ( 'NONE',  ( -0.8070866141732283561, -0.3937007874015746034, -0.7574803149606299524 ) ) ;
#14006 = CARTESIAN_POINT ( 'NONE',  ( 0.6971942568897637749, 2.189545951927499583E-17, 0.04183070860765386589 ) ) ;
#14007 = AXIS2_PLACEMENT_3D ( 'NONE', #20725, #5890, #2511 ) ;
#14008 = CARTESIAN_POINT ( 'NONE',  ( -0.07405724077823318263, -1.533464566875370805, 0.1787899950787401604 ) ) ;
#14009 = CARTESIAN_POINT ( 'NONE',  ( 0.07405724077823318263, -0.7805118109698575557, 0.1787899950787401604 ) ) ;
#14010 = ADVANCED_FACE ( 'NONE', ( #45864 ), #42720, .T. ) ;
#14011 = CARTESIAN_POINT ( 'NONE',  ( -1.002407869896990045, -0.1264236179284866091, 0.4945866141194645849 ) ) ;
#14012 = CARTESIAN_POINT ( 'NONE',  ( 0.1797182628040039087, -1.243646171787769816, 0.07444174185955046430 ) ) ;
#14013 = CARTESIAN_POINT ( 'NONE',  ( -0.07691592068040527252, 0.2510868047526074176, -0.04147023971058640124 ) ) ;
#14014 = CARTESIAN_POINT ( 'NONE',  ( 1.002407869896990045, 0.1264236179284866091, 1.252460629867496067 ) ) ;
#14015 = CARTESIAN_POINT ( 'NONE',  ( 1.054774247047244540, -0.07405724077823318263, 1.515748031442299526 ) ) ;
#14016 = EDGE_CURVE ( 'NONE', #7415, #28468, #20475, .T. ) ;
#14017 = CARTESIAN_POINT ( 'NONE',  ( 0.9873396505805591694, 0.1113553986120547346, 1.707677165354330562 ) ) ;
#14019 = FACE_OUTER_BOUND ( 'NONE', #28002, .T. ) ;
#14018 = DIRECTION ( 'NONE',  ( 0.000000000000000000, 0.000000000000000000, -1.000000000000000000 ) ) ;
#14020 = CARTESIAN_POINT ( 'NONE',  ( 0.7185039370078739607, 1.928577636452523993E-17, 1.250000000000000000 ) ) ;
#14021 = CARTESIAN_POINT ( 'NONE',  ( -0.06523048226347956391, -0.7583661416247552411, 0.1574803149606297803 ) ) ;
#14022 = CARTESIAN_POINT ( 'NONE',  ( -0.7185039370078746268, -0.06523048226347956391, 1.754429133750741387 ) ) ;
#14023 = CARTESIAN_POINT ( 'NONE',  ( 3.284318927891251994E-17, 0.04872047249470835839, 0.1787899950787401882 ) ) ;
#14024 = CARTESIAN_POINT ( 'NONE',  ( 0.9500414927467378812, 0.1787899950787401604, 0.1082677164816695514 ) ) ;
#14025 = CARTESIAN_POINT ( 'NONE',  ( 0.7022289528609824139, 0.03015070893300095256, 0.03937013461078139875 ) ) ;
#14027 = CARTESIAN_POINT ( 'NONE',  ( -0.3980944881889761366, 0.1864803149606355515, -0.06082000038405668829 ) ) ;
#14026 = CARTESIAN_POINT ( 'NONE',  ( 0.8759842519685039353, 0.1787899950787401882, 1.213090551127338435 ) ) ;
#14028 = CARTESIAN_POINT ( 'NONE',  ( 0.5962569168439626477, 4.766607801171850497E-17, 0.000000000000000000 ) ) ;
#14029 = CARTESIAN_POINT ( 'NONE',  ( 1.033464566929134687, -0.06523048226347956391, 0.5487204723334181411 ) ) ;
#14030 = ORIENTED_EDGE ( 'NONE', *, *, #11713, .F. ) ;
#14031 = CARTESIAN_POINT ( 'NONE',  ( -0.7185039370078739607, 1.928577636452523993E-17, 1.131889763779527547 ) ) ;
#14032 = CARTESIAN_POINT ( 'NONE',  ( 0.8685850549921918518, 0.1748108619810979925, 0.03936985974487598045 ) ) ;
#14033 = CARTESIAN_POINT ( 'NONE',  ( -0.7185039370078746268, -0.06523048226347956391, 1.488681102362205300 ) ) ;
#14034 = CIRCLE ( 'NONE', #30895, 0.2047244094488188948 ) ;
#14035 = CARTESIAN_POINT ( 'NONE',  ( -0.8107537697050253289, 0.1574803149606300301, 0.3272637794200322636 ) ) ;
#14036 = CARTESIAN_POINT ( 'NONE',  ( -0.8107537697050254399, -0.1574803149606297803, 1.532972440944882386 ) ) ;
#14037 = CARTESIAN_POINT ( 'NONE',  ( 0.8019270111902717657, 0.1787899950787401604, 1.412401574749386990 ) ) ;
#14038 = FACE_OUTER_BOUND ( 'NONE', #17821, .T. ) ;
#14039 = CARTESIAN_POINT ( 'NONE',  ( 0.07405724077823318263, -0.02755905506434671789, 0.1787899950787401604 ) ) ;
#14040 = ORIENTED_EDGE ( 'NONE', *, *, #28100, .F. ) ;
#14041 = CARTESIAN_POINT ( 'NONE',  ( 0.2759478392031617933, 0.3740157480314960647, 1.713085361781125915 ) ) ;
#14042 = VERTEX_POINT ( 'NONE', #6315 ) ;
#14043 = CARTESIAN_POINT ( 'NONE',  ( 0.7646288533564489232, -0.1113553986120547346, 1.284448818790110192 ) ) ;
#14044 = CARTESIAN_POINT ( 'NONE',  ( -0.4240551181102362177, -2.591110818884263559E-17, 0.000000000000000000 ) ) ;
#14045 = CARTESIAN_POINT ( 'NONE',  ( 1.054774247047244540, -0.07405724077823318263, 0.5757874015210394658 ) ) ;
#14046 = VERTEX_POINT ( 'NONE', #16880 ) ;
#14047 = CARTESIAN_POINT ( 'NONE',  ( 0.1787899950787401604, -1.720472440891118726, 0.07405724077823318263 ) ) ;
#14048 = CARTESIAN_POINT ( 'NONE',  ( -0.8759842519685039353, -0.1787899950787401882, 1.080216535379306952 ) ) ;
#14049 = CARTESIAN_POINT ( 'NONE',  ( -0.8107537697050234415, -0.1574803149606297803, 0.1943897637795276023 ) ) ;
#14050 = ORIENTED_EDGE ( 'NONE', *, *, #17851, .T. ) ;
#14051 = CARTESIAN_POINT ( 'NONE',  ( -0.6971942568897648851, -0.07405724077823297447, 1.107283464513165727 ) ) ;
#14052 = CARTESIAN_POINT ( 'NONE',  ( -0.8759842519685039353, 0.1787899950787401882, 0.7849409448281259305 ) ) ;
#14053 = CARTESIAN_POINT ( 'NONE',  ( -1.054774247047244096, 0.000000000000000000, 0.2239173227808822775 ) ) ;
#14054 = CARTESIAN_POINT ( 'NONE',  ( 1.284448818897637956, -0.3937007874015748254, 1.181102362204724310 ) ) ;
#14055 = CARTESIAN_POINT ( 'NONE',  ( 0.07405724077823318263, -0.7520924721662473056, 0.1787899950787401604 ) ) ;
#14056 = ORIENTED_EDGE ( 'NONE', *, *, #44105, .F. ) ;
#14057 = CARTESIAN_POINT ( 'NONE',  ( 2.892866454678787531E-17, -0.007874015640504449659, 0.1574803149606299191 ) ) ;
#14058 = DIRECTION ( 'NONE',  ( -0.000000000000000000, 1.000000000000000000, -0.000000000000000000 ) ) ;
#14059 = ORIENTED_EDGE ( 'NONE', *, *, #8941, .F. ) ;
#14060 = ORIENTED_EDGE ( 'NONE', *, *, #35926, .F. ) ;
#14061 = DIRECTION ( 'NONE',  ( 1.822029033848725028E-16, 0.000000000000000000, 1.000000000000000000 ) ) ;
#14062 = CARTESIAN_POINT ( 'NONE',  ( 0.7185039370078739607, 1.928577636452523993E-17, 0.1870078740157480324 ) ) ;
#14063 = CARTESIAN_POINT ( 'NONE',  ( -0.6971942568897637749, 2.189545951927499583E-17, 0.6323818897100157432 ) ) ;
#14064 = CARTESIAN_POINT ( 'NONE',  ( 0.1574803149606300301, -0.01033464566929132716, 0.06523048226347956391 ) ) ;
#14065 = ORIENTED_EDGE ( 'NONE', *, *, #31827, .F. ) ;
#14066 = CARTESIAN_POINT ( 'NONE',  ( -0.8759842519685039353, -0.1787899950787401882, 1.788877952702141672 ) ) ;
#14067 = CONICAL_SURFACE ( 'NONE', #30929, 0.09842519685039370636, 0.9599310885968824758 ) ;
#14068 = ADVANCED_FACE ( 'NONE', ( #13303 ), #2489, .T. ) ;
#14069 = VERTEX_POINT ( 'NONE', #38698 ) ;
#14070 = DIRECTION ( 'NONE',  ( 0.5735764363510330588, -0.6455006197386629063, 0.5043203561029945270 ) ) ;
#14071 = EDGE_CURVE ( 'NONE', #10268, #3060, #9705, .T. ) ;
#14072 = DIRECTION ( 'NONE',  ( -1.000000000000000000, 0.000000000000000000, 0.000000000000000000 ) ) ;
#14073 = CARTESIAN_POINT ( 'NONE',  ( 0.9873396505805591694, -0.1113553986120547346, 0.6348425196850393526 ) ) ;
#14074 = CARTESIAN_POINT ( 'NONE',  ( 0.07444174185955065859, -0.8548666442287150558, 0.1797182628040039087 ) ) ;
#14075 = CARTESIAN_POINT ( 'NONE',  ( 0.2471922904502827090, 0.06732389326662464868, 0.09794877975417727589 ) ) ;
#14076 = CARTESIAN_POINT ( 'NONE',  ( -0.9412147342319837628, -0.1574803149606297803, 1.370570866034205970 ) ) ;
#14077 = AXIS2_PLACEMENT_3D ( 'NONE', #39092, #9885, #24498 ) ;
#14078 = CARTESIAN_POINT ( 'NONE',  ( 0.8759842519685039353, 0.1787899950787401882, 0.7455708660879684091 ) ) ;
#14079 = EDGE_CURVE ( 'NONE', #15113, #30501, #18315, .T. ) ;
#14080 = CARTESIAN_POINT ( 'NONE',  ( 0.06523048226347956391, -0.6451771653543302287, 0.1574803149606297803 ) ) ;
#14081 = FACE_OUTER_BOUND ( 'NONE', #45253, .T. ) ;
#14082 = EDGE_CURVE ( 'NONE', #12702, #27624, #39704, .T. ) ;
#14083 = CARTESIAN_POINT ( 'NONE',  ( 0.7185039370078746268, 0.06523048226347956391, 0.1747047243019218821 ) ) ;
#14084 = CARTESIAN_POINT ( 'NONE',  ( 0.7646288533564489232, 0.1113553986120547346, 1.284448818897637956 ) ) ;
#14086 = PRESENTATION_STYLE_ASSIGNMENT (( #46895 ) ) ;
#14085 = CARTESIAN_POINT ( 'NONE',  ( 0.8586096885590351890, -0.1731299321688159754, 1.987893929421542305 ) ) ;
#14087 = FACE_OUTER_BOUND ( 'NONE', #5895, .T. ) ;
#14088 = ( BOUNDED_CURVE ( )  B_SPLINE_CURVE ( 2, ( #25473, #14673, #21862, #18260, #23, #40981, #30726, #44818, #4806 ),
 .UNSPECIFIED., .F., .T. ) 
 B_SPLINE_CURVE_WITH_KNOTS ( ( 3, 2, 2, 2, 3 ),
 ( 0.6400000000000000133, 0.6424999999999999600, 0.6450000000000000178, 0.6474999999999999645, 0.6500000000000000222 ),
 .UNSPECIFIED. ) 
 CURVE ( )  GEOMETRIC_REPRESENTATION_ITEM ( )  RATIONAL_B_SPLINE_CURVE ( ( 1.000000000000000000, 0.9238795325112869605, 1.000000000000000000, 0.9238795325112869605, 1.000000000000000000, 0.9238795325112869605, 1.000000000000000000, 0.9238795325112829637, 1.000000000000000000 ) ) 
 REPRESENTATION_ITEM ( '' )  ) ;
#14090 = CARTESIAN_POINT ( 'NONE',  ( -1.054774247047244096, 0.000000000000000000, 1.990649606245448844 ) ) ;
#14089 = CARTESIAN_POINT ( 'NONE',  ( 0.8019270111902716547, 0.1787899950787401604, 0.6643700786863951935 ) ) ;
#14091 = CARTESIAN_POINT ( 'NONE',  ( 3.284318927891251994E-17, -0.6599409448281259305, 0.1787899950787401882 ) ) ;
#14092 = CARTESIAN_POINT ( 'NONE',  ( 0.3980944881889800779, 1.061695335278752594, -0.02376411959061622975 ) ) ;
#14093 = CARTESIAN_POINT ( 'NONE',  ( -0.8107537697050254399, 0.1574803149606300301, 1.163877952755904666 ) ) ;
#14094 = CARTESIAN_POINT ( 'NONE',  ( -0.4240551181102362177, -0.2559055118110236116, 3.133938659235354185E-17 ) ) ;
#14095 = CARTESIAN_POINT ( 'NONE',  ( 0.6971942568897648851, -0.07405724077823297447, 0.9891732282926934960 ) ) ;
#14096 = VECTOR ( 'NONE', #29284, 39.37007874015748143 ) ;
#14097 = ORIENTED_EDGE ( 'NONE', *, *, #15392, .F. ) ;
#14098 = CARTESIAN_POINT ( 'NONE',  ( 0.8759842519685039353, 0.000000000000000000, 1.990649606245448844 ) ) ;
#14099 = FACE_OUTER_BOUND ( 'NONE', #26638, .T. ) ;
#14100 = CARTESIAN_POINT ( 'NONE',  ( 0.1787899950787401604, -1.794291338528913426, 0.07405724077823318263 ) ) ;
#14101 = CARTESIAN_POINT ( 'NONE',  ( -0.07405724077823318263, -1.193897637741512696, -0.1787899950787401604 ) ) ;
#14102 = CARTESIAN_POINT ( 'NONE',  ( 0.06523048226347956391, -1.496555118110236782, -0.1574803149606300301 ) ) ;
#14103 = CARTESIAN_POINT ( 'NONE',  ( 0.9873396505805591694, 0.1113553986120547346, 1.235236220472440971 ) ) ;
#14104 = CARTESIAN_POINT ( 'NONE',  ( -1.002407869896990045, -0.1264236179284866091, 0.05659448813521283234 ) ) ;
#14105 = VERTEX_POINT ( 'NONE', #31984 ) ;
#14106 = CARTESIAN_POINT ( 'NONE',  ( -0.06523048226347956391, 0.06840551191855072377, 0.1574803149606297803 ) ) ;
#14107 = ORIENTED_EDGE ( 'NONE', *, *, #5880, .F. ) ;
#14109 = CARTESIAN_POINT ( 'NONE',  ( -0.9500414927467377701, -0.1787899950787401604, 1.988188976324191781 ) ) ;
#14108 = VECTOR ( 'NONE', #22193, 39.37007874015748143 ) ;
#14110 = CARTESIAN_POINT ( 'NONE',  ( -1.054774247047244540, 0.07405724077823318263, 1.560039370024977057 ) ) ;
#14111 = CARTESIAN_POINT ( 'NONE',  ( 0.8019270111902716547, 0.1787899950787401604, 0.9055118109698584439 ) ) ;
#14112 = CARTESIAN_POINT ( 'NONE',  ( -0.6971942568897637749, 2.189545951927499583E-17, 1.104822834591905556 ) ) ;
#14113 = CARTESIAN_POINT ( 'NONE',  ( -0.9500414927467378812, -0.1787899950787401604, 0.3740157479777325711 ) ) ;
#14114 = ( BOUNDED_CURVE ( )  B_SPLINE_CURVE ( 2, ( #291, #7485, #21398, #10402, #32690, #36280, #47038, #36023, #14230 ),
 .UNSPECIFIED., .F., .T. ) 
 B_SPLINE_CURVE_WITH_KNOTS ( ( 3, 2, 2, 2, 3 ),
 ( 0.8100000000000000533, 0.8125000000000000000, 0.8149999999999999467, 0.8175000000000000044, 0.8199999999999999512 ),
 .UNSPECIFIED. ) 
 CURVE ( )  GEOMETRIC_REPRESENTATION_ITEM ( )  RATIONAL_B_SPLINE_CURVE ( ( 1.000000000000000000, 0.9238795325112869605, 1.000000000000000000, 0.9238795325112869605, 1.000000000000000000, 0.9238795325112869605, 1.000000000000000000, 0.9238795325112829637, 1.000000000000000000 ) ) 
 REPRESENTATION_ITEM ( '' )  ) ;
#14115 = CARTESIAN_POINT ( 'NONE',  ( -0.2471922904502825702, 0.05534442469272835008, 0.1143959998688603985 ) ) ;
#14116 = CARTESIAN_POINT ( 'NONE',  ( -0.9500414927467378812, -0.1787899950787401604, 1.830708661363559253 ) ) ;
#14117 = CARTESIAN_POINT ( 'NONE',  ( 0.07564704710180411573, -0.08785038237306361242, -0.2417569064345358731 ) ) ;
#14118 = CARTESIAN_POINT ( 'NONE',  ( -0.7646288533564489232, 0.1113553986120547346, 1.953740157480315043 ) ) ;
#14119 = CARTESIAN_POINT ( 'NONE',  ( 0.2559055093128127512, 0.08129821535987498404, -0.05440291541350525395 ) ) ;
#14120 = CARTESIAN_POINT ( 'NONE',  ( 0.1264236179284866091, -0.4641987713788449099, -0.1264236179284866091 ) ) ;
#14121 = CARTESIAN_POINT ( 'NONE',  ( -0.1490350107398933088, -0.09842519685039370636, -0.1001871157495389797 ) ) ;
#14122 = CONTEXT_DEPENDENT_SHAPE_REPRESENTATION ( #40061, #32171 ) ;
#14123 = DIRECTION ( 'NONE',  ( 0.000000000000000000, 0.000000000000000000, -1.000000000000000000 ) ) ;
#14124 = DIRECTION ( 'NONE',  ( 0.000000000000000000, -0.000000000000000000, 1.000000000000000000 ) ) ;
#14125 = CARTESIAN_POINT ( 'NONE',  ( -0.9500414927467378812, 0.1787899950787401604, 0.1476377952218271561 ) ) ;
#14126 = ORIENTED_EDGE ( 'NONE', *, *, #45532, .T. ) ;
#14127 = CARTESIAN_POINT ( 'NONE',  ( -0.8019270111902716547, -0.1787899950787401604, 1.235236220418678199 ) ) ;
#14128 = ORIENTED_EDGE ( 'NONE', *, *, #18243, .F. ) ;
#14129 = CARTESIAN_POINT ( 'NONE',  ( 0.1787899950787401604, -1.164370078686393306, -0.07405724077823318263 ) ) ;
#14130 = CARTESIAN_POINT ( 'NONE',  ( -0.07405724077823318263, -1.371062992072219489, 0.1787899950787401604 ) ) ;
#14131 = EDGE_CURVE ( 'NONE', #31452, #8537, #26019, .T. ) ;
#14132 = DIRECTION ( 'NONE',  ( 0.000000000000000000, -1.000000000000000000, 0.000000000000000000 ) ) ;
#14133 = CARTESIAN_POINT ( 'NONE',  ( 1.033464566929133799, 0.000000000000000000, 0.3641732283464567121 ) ) ;
#14134 = AXIS2_PLACEMENT_3D ( 'NONE', #15495, #30139, #44679 ) ;
#14135 = DIRECTION ( 'NONE',  ( 0.5735764363510447161, -0.8191520442889925757, 1.003171929053525486E-16 ) ) ;
#14136 = CARTESIAN_POINT ( 'NONE',  ( -0.7185039370078746268, -0.06523048226347956391, 0.9276574802074333270 ) ) ;
#14137 = CARTESIAN_POINT ( 'NONE',  ( -0.8759842519685039353, -0.1574803149606299191, 0.7874015748031496509 ) ) ;
#14138 = CARTESIAN_POINT ( 'NONE',  ( 0.8019270111902717657, 0.1787899950787401604, 0.4724409448281262636 ) ) ;
#14139 = CARTESIAN_POINT ( 'NONE',  ( 0.1574803149606299191, -0.08661417322834646937, -1.928577636452523993E-17 ) ) ;
#14140 = CIRCLE ( 'NONE', #40883, 0.1673228346456689108 ) ;
#14141 = CONICAL_SURFACE ( 'NONE', #11073, 0.1377952755905513804, 0.9599310885968808105 ) ;
#14142 = CARTESIAN_POINT ( 'NONE',  ( 0.9873396505805591694, -0.1113553986120547346, 1.845472440837354178 ) ) ;
#14143 = ORIENTED_EDGE ( 'NONE', *, *, #23981, .T. ) ;
#14144 = ADVANCED_FACE ( 'NONE', ( #28159 ), #42963, .F. ) ;
#14145 = DIRECTION ( 'NONE',  ( -1.000000000000000000, 0.000000000000000000, 0.000000000000000000 ) ) ;
#14146 = CARTESIAN_POINT ( 'NONE',  ( 0.7646288533564489232, -0.1113553986120547346, 0.8612204724409449064 ) ) ;
#14147 = CARTESIAN_POINT ( 'NONE',  ( -1.033464566929134687, 0.06523048226347956391, 1.232775590551180134 ) ) ;
#14148 = CARTESIAN_POINT ( 'NONE',  ( 0.7646288533564489232, 0.1113553986120547346, 0.1722440943806619884 ) ) ;
#14149 = CARTESIAN_POINT ( 'NONE',  ( -0.07405724077823318263, -0.03248031490686641154, 0.1787899950787401604 ) ) ;
#14150 = CARTESIAN_POINT ( 'NONE',  ( -9.642888182262618425E-18, 0.09055118120988918384, -0.1574803149606299191 ) ) ;
#14151 = CARTESIAN_POINT ( 'NONE',  ( 0.7646288533564489232, -0.1113553986120547346, 1.835629921152314825 ) ) ;
#14152 = CARTESIAN_POINT ( 'NONE',  ( 0.1113553986120547346, -1.499015747923968522, 0.1113553986120547346 ) ) ;
#14153 = CARTESIAN_POINT ( 'NONE',  ( -0.1787899950787401882, -0.6353346456155275490, 0.000000000000000000 ) ) ;
#14154 = CARTESIAN_POINT ( 'NONE',  ( 2.892866454678787531E-17, -1.120078740157480324, 0.1574803149606299191 ) ) ;
#14155 = CARTESIAN_POINT ( 'NONE',  ( 1.033464566929133799, 0.000000000000000000, 0.9448818896562519720 ) ) ;
#14156 = LINE ( 'NONE', #24939, #4527 ) ;
#14157 = CARTESIAN_POINT ( 'NONE',  ( -0.8759842519685039353, -0.1787899950787401882, 0.4453740156942677664 ) ) ;
#14158 = ORIENTED_EDGE ( 'NONE', *, *, #28652, .T. ) ;
#14159 = ORIENTED_EDGE ( 'NONE', *, *, #35720, .F. ) ;
#14160 = ORIENTED_EDGE ( 'NONE', *, *, #19162, .F. ) ;
#14161 = CARTESIAN_POINT ( 'NONE',  ( -0.7495606340400177148, 0.1264236179284866091, 1.577263779473795369 ) ) ;
#14162 = VERTEX_POINT ( 'NONE', #21171 ) ;
#14163 = CARTESIAN_POINT ( 'NONE',  ( 1.054774247047244540, -0.07405724077823318263, 1.560039370024977057 ) ) ;
#14164 = ORIENTED_EDGE ( 'NONE', *, *, #30136, .F. ) ;
#14165 = CARTESIAN_POINT ( 'NONE',  ( -1.054774247047244096, 0.000000000000000000, 0.8144685038832440993 ) ) ;
#14166 = CARTESIAN_POINT ( 'NONE',  ( 1.054774247047244096, 0.000000000000000000, 0.2239173227808822775 ) ) ;
#14167 = DIRECTION ( 'NONE',  ( 0.000000000000000000, 0.000000000000000000, 1.000000000000000000 ) ) ;
#14168 = CARTESIAN_POINT ( 'NONE',  ( -0.8019270111902716547, 0.1787899950787401604, 0.6249999999462366729 ) ) ;
#14169 = EDGE_CURVE ( 'NONE', #16814, #33534, #46627, .T. ) ;
#14170 = CARTESIAN_POINT ( 'NONE',  ( 0.7185039370078739607, 1.928577636452523993E-17, 0.9251968502861732668 ) ) ;
#14171 = DIRECTION ( 'NONE',  ( 0.000000000000000000, 0.000000000000000000, 1.000000000000000000 ) ) ;
#14172 = CARTESIAN_POINT ( 'NONE',  ( 0.1574803149606300301, -0.2760826770578272416, 0.06523048226347956391 ) ) ;
#14173 = CARTESIAN_POINT ( 'NONE',  ( -1.002407869896990045, -0.1264236179284866091, 1.439468503883244210 ) ) ;
#14174 = VECTOR ( 'NONE', #40434, 39.37007874015748143 ) ;
#14176 = CARTESIAN_POINT ( 'NONE',  ( -1.033464566929133799, 1.928577636452524610E-17, 2.869337061179095023E-17 ) ) ;
#14175 = AXIS2_PLACEMENT_3D ( 'NONE', #10831, #25194, #7216 ) ;
#14177 = CARTESIAN_POINT ( 'NONE',  ( -0.9412147342319837628, -0.1574803149606297803, 0.4355314960629916299 ) ) ;
#14178 = CARTESIAN_POINT ( 'NONE',  ( 0.6971942568897648851, 0.07405724077823318263, 1.500984251914741829 ) ) ;
#14179 = CARTESIAN_POINT ( 'NONE',  ( -0.1564116827871401549, -0.09851383672212755960, -0.08632843964392854230 ) ) ;
#14180 = CARTESIAN_POINT ( 'NONE',  ( -0.9873396505805591694, 0.1113553986120547346, 0.3592519683964098820 ) ) ;
#14181 = VECTOR ( 'NONE', #35040, 39.37007874015748143 ) ;
#14182 = ORIENTED_EDGE ( 'NONE', *, *, #12683, .F. ) ;
#14183 = CARTESIAN_POINT ( 'NONE',  ( -0.1787899950787401882, -1.748647590276482422, 0.000000000000000000 ) ) ;
#14184 = ORIENTED_EDGE ( 'NONE', *, *, #4524, .F. ) ;
#14185 = ORIENTED_EDGE ( 'NONE', *, *, #11778, .F. ) ;
#14186 = EDGE_CURVE ( 'NONE', #24192, #2855, #17556, .T. ) ;
#14187 = CARTESIAN_POINT ( 'NONE',  ( 0.000000000000000000, 0.000000000000000000, -0.05390369169704170571 ) ) ;
#14188 = CARTESIAN_POINT ( 'NONE',  ( -0.1264236179284866091, -0.9404527558517480346, 0.1264236179284866091 ) ) ;
#14189 = EDGE_CURVE ( 'NONE', #3331, #20293, #45564, .T. ) ;
#14190 = CARTESIAN_POINT ( 'NONE',  ( -0.2471922436403682644, -0.09120620265207400601, -0.04599440333008567028 ) ) ;
#14191 = CARTESIAN_POINT ( 'NONE',  ( 0.1634463062180389892, -0.1606610259913433258, 5.268451237904698604E-07 ) ) ;
#14192 = CARTESIAN_POINT ( 'NONE',  ( 1.054774247047244096, 0.000000000000000000, 1.675688976324189117 ) ) ;
#14193 = CARTESIAN_POINT ( 'NONE',  ( -0.1787899950787401604, -0.09264365326860893313, 0.07405724077823318263 ) ) ;
#14194 = CARTESIAN_POINT ( 'NONE',  ( -0.07405724077823318263, -0.2440944881352131168, -0.1787899950787401604 ) ) ;
#14195 = CARTESIAN_POINT ( 'NONE',  ( 0.1787899950787401882, 0.09301181107738563936, -2.189545951927503898E-17 ) ) ;
#14196 = CARTESIAN_POINT ( 'NONE',  ( 1.033464566929134687, -0.06523048226347956391, 0.1550196849318430659 ) ) ;
#14197 = EDGE_CURVE ( 'NONE', #16549, #22505, #32942, .T. ) ;
#14198 = CARTESIAN_POINT ( 'NONE',  ( 1.002407869896990045, -0.1264236179284866091, 0.6471456692375747721 ) ) ;
#14199 = CARTESIAN_POINT ( 'NONE',  ( -0.6971942568897637749, 2.189545951927499583E-17, 1.031003936954110189 ) ) ;
#14201 = CARTESIAN_POINT ( 'NONE',  ( 0.9873396505805591694, 0.1113553986120547346, 1.117125984251968518 ) ) ;
#14200 = CARTESIAN_POINT ( 'NONE',  ( 2.458936486476969154E-17, 0.1299212598425196763, -0.2007874015748031815 ) ) ;
#14203 = CARTESIAN_POINT ( 'NONE',  ( -0.8901995480705489072, -0.1743753279471531581, 1.988434009720291273 ) ) ;
#14202 = CARTESIAN_POINT ( 'NONE',  ( 0.1797182628040039365, -1.792366644228716721, -2.200913952912460540E-17 ) ) ;
#14204 = VECTOR ( 'NONE', #40958, 39.37007874015748854 ) ;
#14205 = CARTESIAN_POINT ( 'NONE',  ( 0.07405724077823318263, -0.4606299212060784853, 0.1787899950787401604 ) ) ;
#14206 = CARTESIAN_POINT ( 'NONE',  ( 0.6141732283464567121, 9.908067607274841931E-18, -0.08090551181102362266 ) ) ;
#14207 = CARTESIAN_POINT ( 'NONE',  ( 0.6971942568897637749, 2.189545951927499583E-17, 1.700295275536787498 ) ) ;
#14209 = LINE ( 'NONE', #35546, #31575 ) ;
#14208 = CARTESIAN_POINT ( 'NONE',  ( -0.7185039370078739607, 1.928577636452523993E-17, 0.7775590551181102983 ) ) ;
#14210 = CARTESIAN_POINT ( 'NONE',  ( 0.7495606340400177148, -0.1264236179284866091, 0.4798228345919055560 ) ) ;
#14211 = AXIS2_PLACEMENT_3D ( 'NONE', #43874, #10606, #25204 ) ;
#14212 = VECTOR ( 'NONE', #37567, 39.37007874015748143 ) ;
#14213 = ORIENTED_EDGE ( 'NONE', *, *, #34408, .T. ) ;
#14214 = PLANE ( 'NONE',  #7694 ) ;
#14215 = CARTESIAN_POINT ( 'NONE',  ( -0.1377952755905511861, 1.808041534174241898E-17, -0.2103840066576717072 ) ) ;
#14216 = CARTESIAN_POINT ( 'NONE',  ( -0.1787899950787401604, -0.08661417317458304510, -0.07405724077823318263 ) ) ;
#14217 = CARTESIAN_POINT ( 'NONE',  ( 1.054774247047244096, 0.000000000000000000, 0.6126968503399370380 ) ) ;
#14218 = CARTESIAN_POINT ( 'NONE',  ( 3.284318927891251994E-17, -1.014271653489543290, 0.1787899950787401882 ) ) ;
#14219 = CARTESIAN_POINT ( 'NONE',  ( 0.7495606340400177148, 0.1264236179284866091, 0.1205708660879689087 ) ) ;
#14220 = CARTESIAN_POINT ( 'NONE',  ( -0.4330708661417340677, 0.1574803149606330277, -1.186023622047243986 ) ) ;
#14221 = CARTESIAN_POINT ( 'NONE',  ( -0.8019270111902717657, -0.1787899950787401604, 1.584645669237574994 ) ) ;
#14222 = ORIENTED_EDGE ( 'NONE', *, *, #29050, .F. ) ;
#14223 = CARTESIAN_POINT ( 'NONE',  ( 0.8019270111902717657, 0.1787899950787401604, 1.181102362150960428 ) ) ;
#14224 = CARTESIAN_POINT ( 'NONE',  ( -0.1574803149606299191, -1.159448818790110192, 0.000000000000000000 ) ) ;
#14225 = CARTESIAN_POINT ( 'NONE',  ( -0.7646288533564489232, -0.1113553986120547346, 0.6938976376877481478 ) ) ;
#14226 = CARTESIAN_POINT ( 'NONE',  ( 0.9873396505805591694, -0.1113553986120547346, 1.500984251968503935 ) ) ;
#14227 = CARTESIAN_POINT ( 'NONE',  ( 0.9500414927467378812, -0.1787899950787401604, 1.825787401521040243 ) ) ;
#14228 = CARTESIAN_POINT ( 'NONE',  ( -0.9873396505805591694, -0.1113553986120547346, 0.5561023622047244208 ) ) ;
#14229 = CARTESIAN_POINT ( 'NONE',  ( -1.054774247047244540, -0.07405724077823318263, 0.9251968503399374821 ) ) ;
#14230 = CARTESIAN_POINT ( 'NONE',  ( -1.033464566929133799, 0.000000000000000000, 1.624015748031496287 ) ) ;
#14231 = DIRECTION ( 'NONE',  ( 0.000000000000000000, 0.000000000000000000, 1.000000000000000000 ) ) ;
#14232 = CARTESIAN_POINT ( 'NONE',  ( 0.6971942568897626646, 0.07405724077823318263, 0.3198818897100159098 ) ) ;
#14233 = CARTESIAN_POINT ( 'NONE',  ( -0.8019270111902716547, -0.1787899950787401604, 0.2854330708123783977 ) ) ;
#14234 = CARTESIAN_POINT ( 'NONE',  ( -1.002407869896990045, 0.1264236179284866091, 0.7357283464029290565 ) ) ;
#14235 = CARTESIAN_POINT ( 'NONE',  ( 0.7185039370078739607, 1.928577636452523993E-17, 1.594488188868850242 ) ) ;
#14236 = ORIENTED_EDGE ( 'NONE', *, *, #18029, .T. ) ;
#14237 = SHAPE_REPRESENTATION ( 'Pivot Pin', ( #20860 ), #10178 ) ;
#14238 = CARTESIAN_POINT ( 'NONE',  ( -0.1264236179284866091, 0.03887795280966901967, 0.1264236179284866091 ) ) ;
#14239 = EDGE_LOOP ( 'NONE', ( #34849, #9295 ) ) ;
#14240 = CARTESIAN_POINT ( 'NONE',  ( 0.6971942568897626646, 0.07405724077823318263, 0.8316929133320636325 ) ) ;
#14241 = CARTESIAN_POINT ( 'NONE',  ( 1.054774247047244096, 0.000000000000000000, 1.050688976324189117 ) ) ;
#14242 = CARTESIAN_POINT ( 'NONE',  ( -1.002407869896990045, 0.1264236179284866091, 1.916830708607653477 ) ) ;
#14243 = CARTESIAN_POINT ( 'NONE',  ( 1.054774247047244096, 0.000000000000000000, 1.911909448765133801 ) ) ;
#14244 = EDGE_LOOP ( 'NONE', ( #5151, #12465, #29384, #45141 ) ) ;
#14245 = CARTESIAN_POINT ( 'NONE',  ( -1.033464566929133799, 0.000000000000000000, 0.6397637795275591399 ) ) ;
#14246 = CARTESIAN_POINT ( 'NONE',  ( 0.9412147342319837628, -0.1574803149606297803, 1.606791338475149766 ) ) ;
#14247 = CARTESIAN_POINT ( 'NONE',  ( -0.07405724077823318263, -1.268824755630812540, 0.1787899950787401604 ) ) ;
#14248 = ORIENTED_EDGE ( 'NONE', *, *, #27109, .T. ) ;
#14249 = CARTESIAN_POINT ( 'NONE',  ( 0.1787899950787401604, -0.2982283464029296116, 0.07405724077823318263 ) ) ;
#14250 = EDGE_CURVE ( 'NONE', #38848, #27058, #25963, .T. ) ;
#14251 = VECTOR ( 'NONE', #38645, 39.37007874015748143 ) ;
#14252 = ORIENTED_EDGE ( 'NONE', *, *, #2109, .T. ) ;
#14253 = CARTESIAN_POINT ( 'NONE',  ( -0.2471922967771591484, -0.09275221067063765812, 0.04038134086896451314 ) ) ;
#14254 = ADVANCED_FACE ( 'NONE', ( #43926 ), #36978, .T. ) ;
#14255 = CARTESIAN_POINT ( 'NONE',  ( 0.9500414927467378812, 0.1787899950787401604, 0.02952755900135462311 ) ) ;
#14256 = CARTESIAN_POINT ( 'NONE',  ( -0.07405724077823318263, -1.651574803095843258, 0.1787899950787401604 ) ) ;
#14257 = EDGE_CURVE ( 'NONE', #38897, #11192, #10893, .T. ) ;
#14258 = CARTESIAN_POINT ( 'NONE',  ( -1.054774247047244540, 0.07405724077823318263, 0.5413385826234012876 ) ) ;
#14259 = CARTESIAN_POINT ( 'NONE',  ( -0.09722930128650188186, -0.09842519685039370636, 0.1314396626312874239 ) ) ;
#14260 = CARTESIAN_POINT ( 'NONE',  ( -0.7128900651292061630, -0.03685103854907906956, 1.983952560205947568 ) ) ;
#14261 = DIRECTION ( 'NONE',  ( -0.000000000000000000, -0.000000000000000000, -1.000000000000000000 ) ) ;
#14262 = CARTESIAN_POINT ( 'NONE',  ( 0.6971942568897648851, 0.07405724077823318263, 1.264763779473795813 ) ) ;
#14263 = CARTESIAN_POINT ( 'NONE',  ( 1.054774247047244540, 0.07405724077823318263, 1.520669291284818758 ) ) ;
#14264 = VECTOR ( 'NONE', #33610, 39.37007874015748143 ) ;
#14265 = DIRECTION ( 'NONE',  ( -1.000000000000000000, -0.000000000000000000, -0.000000000000000000 ) ) ;
#14266 = CARTESIAN_POINT ( 'NONE',  ( 0.7185039370078739607, 1.928577636452523993E-17, 1.722440944881889813 ) ) ;
#14267 = CYLINDRICAL_SURFACE ( 'NONE', #36587, 0.1574803149606299191 ) ;
#14268 = CARTESIAN_POINT ( 'NONE',  ( 0.6195511811023597382, 0.1864803149606293620, 1.186023622047243986 ) ) ;
#14269 = CARTESIAN_POINT ( 'NONE',  ( -0.7646288533564489232, 0.1113553986120547346, 1.747047243986960652 ) ) ;
#14270 = CARTESIAN_POINT ( 'NONE',  ( 0.8019270111902717657, -0.1787899950787401604, 0.2460629920722207375 ) ) ;
#14271 = CARTESIAN_POINT ( 'NONE',  ( 0.7078001474992028363, 0.05966467328708899981, 0.03937007863263041613 ) ) ;
#14273 = CARTESIAN_POINT ( 'NONE',  ( -0.8759842519685039353, 0.000000000000000000, 0.000000000000000000 ) ) ;
#14272 = CARTESIAN_POINT ( 'NONE',  ( 0.8759842519685039353, 0.1787899950787401882, 1.134350393647023614 ) ) ;
#14274 = CARTESIAN_POINT ( 'NONE',  ( -1.033464566929133799, 0.000000000000000000, 1.112204724409448842 ) ) ;
#14275 = CARTESIAN_POINT ( 'NONE',  ( -1.002407869896990045, 0.1264236179284866091, 1.208169291284818980 ) ) ;
#14276 = CARTESIAN_POINT ( 'NONE',  ( 1.033464566929134687, -0.06523048226347956391, 0.4699803148531029318 ) ) ;
#14277 = ORIENTED_EDGE ( 'NONE', *, *, #20440, .T. ) ;
#14278 = CARTESIAN_POINT ( 'NONE',  ( 0.7646288533564489232, 0.1113553986120547346, 0.2608267716535432879 ) ) ;
#14279 = CARTESIAN_POINT ( 'NONE',  ( 0.9873396505805591694, 0.1113553986120547346, 0.8316929132782993062 ) ) ;
#14280 = CARTESIAN_POINT ( 'NONE',  ( -0.9873396505805591694, 0.1113553986120547346, 0.4379921258767252024 ) ) ;
#14281 = ORIENTED_EDGE ( 'NONE', *, *, #45103, .F. ) ;
#14282 = CARTESIAN_POINT ( 'NONE',  ( 0.8019270111902717657, -0.1787899950787401604, 1.466535433017102763 ) ) ;
#14283 = CARTESIAN_POINT ( 'NONE',  ( -0.9412147342319837628, -0.1574803149606297803, 1.144192913385827737 ) ) ;
#14284 = DIRECTION ( 'NONE',  ( 0.000000000000000000, 0.000000000000000000, 1.000000000000000000 ) ) ;
#14285 = CARTESIAN_POINT ( 'NONE',  ( 0.1264236179284866091, 0.05364173233722803469, 0.1264236179284866091 ) ) ;
#14286 = ORIENTED_EDGE ( 'NONE', *, *, #46789, .F. ) ;
#14287 = CARTESIAN_POINT ( 'NONE',  ( 0.1564216623530370054, -0.01359171937732193448, -0.1403857474672217664 ) ) ;
#14288 = EDGE_LOOP ( 'NONE', ( #36070, #40206, #44846, #15358, #44675, #222, #2725 ) ) ;
#14289 = DIRECTION ( 'NONE',  ( -1.000000000000000000, -1.177520686924250585E-15, 0.000000000000000000 ) ) ;
#14290 = DIRECTION ( 'NONE',  ( -1.000000000000000000, 0.000000000000000000, 0.000000000000000000 ) ) ;
#14291 = CARTESIAN_POINT ( 'NONE',  ( 1.054774247047244540, -0.07405724077823318263, 0.6151574802611974313 ) ) ;
#14292 = ORIENTED_EDGE ( 'NONE', *, *, #3669, .F. ) ;
#14293 = CARTESIAN_POINT ( 'NONE',  ( -0.9500414927467377701, 0.1787899950787401604, 1.486220472387181912 ) ) ;
#14294 = CARTESIAN_POINT ( 'NONE',  ( -0.1574803149606300301, 0.09793307097366882319, -0.06523048226347956391 ) ) ;
#14295 = CARTESIAN_POINT ( 'NONE',  ( -0.6971942568897637749, 2.189545951927499583E-17, 1.149114173174582643 ) ) ;
#14296 = CARTESIAN_POINT ( 'NONE',  ( -1.033464566929134687, -0.06523048226347956391, 0.2042322834645668717 ) ) ;
#14297 = ORIENTED_EDGE ( 'NONE', *, *, #25666, .T. ) ;
#14298 = ADVANCED_FACE ( 'NONE', ( #3199 ), #29132, .T. ) ;
#14299 = CARTESIAN_POINT ( 'NONE',  ( -0.8019270111902716547, 0.1787899950787401604, 1.058070866087969186 ) ) ;
#14300 = CARTESIAN_POINT ( 'NONE',  ( -0.6971942568897626646, -0.07405724077823297447, 0.7972440944344250102 ) ) ;
#14301 = CARTESIAN_POINT ( 'NONE',  ( -0.6971942568897637749, 2.189545951927499583E-17, 0.2042322834108035723 ) ) ;
#14302 = CYLINDRICAL_SURFACE ( 'NONE', #36415, 0.1574803149606299191 ) ;
#14303 = CARTESIAN_POINT ( 'NONE',  ( 0.7185039370078746268, 0.06523048226347956391, 0.8046259841444418637 ) ) ;
#14304 = CARTESIAN_POINT ( 'NONE',  ( -0.1264236179284866091, -0.8086869603552225838, -0.1264236179284866091 ) ) ;
#14305 = ORIENTED_EDGE ( 'NONE', *, *, #41431, .T. ) ;
#14306 = CARTESIAN_POINT ( 'NONE',  ( 0.04463444342724977310, -0.08956241828510866365, 0.1426423949953722625 ) ) ;
#14307 = CARTESIAN_POINT ( 'NONE',  ( -0.7185039370078760701, -0.06523048226348075740, 0.8489173227271181732 ) ) ;
#14308 = ORIENTED_EDGE ( 'NONE', *, *, #6070, .T. ) ;
#14309 = EDGE_CURVE ( 'NONE', #5973, #20673, #28646, .T. ) ;
#14310 = ORIENTED_EDGE ( 'NONE', *, *, #41954, .F. ) ;
#14311 = CARTESIAN_POINT ( 'NONE',  ( 0.8759842519685039353, 0.1574803149606299191, 0.7677165354330708347 ) ) ;
#14312 = DIRECTION ( 'NONE',  ( 1.000000000000000000, 0.000000000000000000, -1.822029033848725275E-16 ) ) ;
#14313 = CARTESIAN_POINT ( 'NONE',  ( -1.054774247047244096, 0.000000000000000000, 0.7701771653005669016 ) ) ;
#14314 = CARTESIAN_POINT ( 'NONE',  ( -0.8107537697050254399, -0.1574803149606297803, 0.5782480313885360879 ) ) ;
#14315 = CARTESIAN_POINT ( 'NONE',  ( -0.6971942568897637749, 2.189545951927499583E-17, 1.739665354276945131 ) ) ;
#14316 = ORIENTED_EDGE ( 'NONE', *, *, #16492, .T. ) ;
#14317 = CARTESIAN_POINT ( 'NONE',  ( 0.002396928536207490728, -0.03415735691519130451, -0.1377928489248547994 ) ) ;
#14318 = CARTESIAN_POINT ( 'NONE',  ( -0.8759842519685039353, 0.1787899950787401882, 0.07627952750529173875 ) ) ;
#14319 = ORIENTED_EDGE ( 'NONE', *, *, #12078, .T. ) ;
#14320 = DIRECTION ( 'NONE',  ( 0.000000000000000000, 0.000000000000000000, 1.000000000000000000 ) ) ;
#14321 = CARTESIAN_POINT ( 'NONE',  ( -1.033464566929134687, 0.06523048226347956391, 1.380413385719244213 ) ) ;
#14322 = CARTESIAN_POINT ( 'NONE',  ( 0.8759842519685039353, -0.1787899950787401882, 0.7258858267178898149 ) ) ;
#14323 = CARTESIAN_POINT ( 'NONE',  ( 0.1574803149606300301, -0.6008858267716538082, 0.06523048226347956391 ) ) ;
#14324 = DIRECTION ( 'NONE',  ( -1.000000000000000000, -0.000000000000000000, 0.000000000000000000 ) ) ;
#14325 = EDGE_LOOP ( 'NONE', ( #5799, #15889, #28057, #12890 ) ) ;
#14326 = CARTESIAN_POINT ( 'NONE',  ( -0.2559055118110235560, 0.1029525201786305882, -0.06857031309820646459 ) ) ;
#14327 = CARTESIAN_POINT ( 'NONE',  ( 0.9412147342319837628, 0.1574803149606300301, 1.277066929133857442 ) ) ;
#14329 = CARTESIAN_POINT ( 'NONE',  ( 0.03901279071809810040, -0.5708661417322835607, 1.224299699984025658 ) ) ;
#14328 = CARTESIAN_POINT ( 'NONE',  ( 0.8497971692482408912, -0.1717431688695388314, 1.987727230376266974 ) ) ;
#14330 = CARTESIAN_POINT ( 'NONE',  ( 0.9412147342319837628, -0.1574803149606297803, 1.852854330708662012 ) ) ;
#14331 = VECTOR ( 'NONE', #41159, 39.37007874015748143 ) ;
#14333 = PLANE ( 'NONE',  #10106 ) ;
#14332 = CARTESIAN_POINT ( 'NONE',  ( 0.6971942568897637749, 2.189545951927499583E-17, 0.7111220471903307860 ) ) ;
#14334 = CARTESIAN_POINT ( 'NONE',  ( 0.07405724077823318263, -0.6820866141194646959, -0.1787899950787401604 ) ) ;
#14335 = CARTESIAN_POINT ( 'NONE',  ( -0.9412147342319837628, -0.1574803149606297803, 0.3863188975302684347 ) ) ;
#14336 = ORIENTED_EDGE ( 'NONE', *, *, #22172, .T. ) ;
#14337 = CARTESIAN_POINT ( 'NONE',  ( 0.6195511811023621807, 0.9842519685039367028, -1.186023622047244430 ) ) ;
#14338 = CARTESIAN_POINT ( 'NONE',  ( 0.1377952755905511861, 0.1564960629921262614, 0.8070866141732283561 ) ) ;
#14339 = CARTESIAN_POINT ( 'NONE',  ( 0.6971942568897626646, -0.07405724077823297447, 0.9104330708123776761 ) ) ;
#14340 = CARTESIAN_POINT ( 'NONE',  ( 0.7185039370078739607, 1.928577636452523993E-17, 0.3051181102362204856 ) ) ;
#14341 = CARTESIAN_POINT ( 'NONE',  ( 0.1787899950787401882, -1.284940944828125930, -2.189545951927503898E-17 ) ) ;
#14342 = CARTESIAN_POINT ( 'NONE',  ( -0.1574803149606300301, -1.486712598425197873, -0.06523048226347956391 ) ) ;
#14343 = CYLINDRICAL_SURFACE ( 'NONE', #40544, 0.1003937007874010356 ) ;
#14344 = CARTESIAN_POINT ( 'NONE',  ( -0.6971942568897626646, 0.07405724077823318263, 0.1574803149068664809 ) ) ;
#14345 = CARTESIAN_POINT ( 'NONE',  ( 0.6971942568897637749, 2.189545951927499583E-17, 1.936515747977732405 ) ) ;
#14346 = ORIENTED_EDGE ( 'NONE', *, *, #7469, .F. ) ;
#14347 = CARTESIAN_POINT ( 'NONE',  ( 0.06523048226347956391, -1.422736220364914095, 0.1574803149606297803 ) ) ;
#14348 = CARTESIAN_POINT ( 'NONE',  ( -0.7495606340400177148, 0.1264236179284866091, 1.892224409395055096 ) ) ;
#14349 = CARTESIAN_POINT ( 'NONE',  ( -0.8759842519685039353, 0.1787899950787401882, 1.606791338528913426 ) ) ;
#14350 = ADVANCED_FACE ( 'NONE', ( #40545 ), #22903, .T. ) ;
#14351 = CARTESIAN_POINT ( 'NONE',  ( -0.8019270111902716547, 0.1787899950787401604, 0.8218503936470251681 ) ) ;
#14352 = CARTESIAN_POINT ( 'NONE',  ( -0.8019270111902717657, -0.1787899950787401604, 0.3690944881352128393 ) ) ;
#14353 = EDGE_CURVE ( 'NONE', #2262, #17766, #43687, .T. ) ;
#14354 = CARTESIAN_POINT ( 'NONE',  ( -0.1850060400416962680, 0.08128102204192841351, -0.1786197838463617626 ) ) ;
#14355 = CARTESIAN_POINT ( 'NONE',  ( -0.6971942568897637749, 2.189545951927499583E-17, 1.897145669237574772 ) ) ;
#14356 = CARTESIAN_POINT ( 'NONE',  ( -0.9873396505805591694, 0.1113553986120547346, 1.904527559055118280 ) ) ;
#14357 = CARTESIAN_POINT ( 'NONE',  ( -0.2713217623817689717, 0.1501096695199156672, -0.9507184613947605722 ) ) ;
#14358 = CARTESIAN_POINT ( 'NONE',  ( 0.07405724077823318263, -0.4223680627174279945, -0.1787899950787401604 ) ) ;
#14359 = CARTESIAN_POINT ( 'NONE',  ( -0.1563790690919384108, -0.09842519685039370636, -0.08631298726982068736 ) ) ;
#14360 = CONTEXT_DEPENDENT_SHAPE_REPRESENTATION ( #9796, #37167 ) ;
#14361 = DIRECTION ( 'NONE',  ( -1.000000000000000000, 0.000000000000000000, 0.000000000000000000 ) ) ;
#14362 = CARTESIAN_POINT ( 'NONE',  ( 0.1574803149606339714, 0.9310112235910574796, -1.064878870394357468 ) ) ;
#14363 = EDGE_CURVE ( 'NONE', #5917, #19054, #12962, .T. ) ;
#14364 = EDGE_CURVE ( 'NONE', #13679, #1767, #6792, .T. ) ;
#14365 = CIRCLE ( 'NONE', #41097, 0.1574803149606299191 ) ;
#14366 = CARTESIAN_POINT ( 'NONE',  ( -0.7495606340400177148, 0.1264236179284866091, 0.1550196849856066983 ) ) ;
#14367 = ORIENTED_EDGE ( 'NONE', *, *, #7307, .T. ) ;
#14368 = CARTESIAN_POINT ( 'NONE',  ( -0.6971942568897648851, -0.07405724077823297447, 1.387795275536786610 ) ) ;
#14369 = EDGE_LOOP ( 'NONE', ( #16469, #13753, #4040, #4301, #14143, #44564, #23058, #34444, #46094, #37583, #47087, #33184 ) ) ;
#14370 = CARTESIAN_POINT ( 'NONE',  ( -0.1787899950787401882, -1.225885826717889815, 0.000000000000000000 ) ) ;
#14371 = CARTESIAN_POINT ( 'NONE',  ( 0.1787899950787401604, -1.321850393647023392, 0.07405724077823318263 ) ) ;
#14372 = ( BOUNDED_CURVE ( )  B_SPLINE_CURVE ( 2, ( #7528, #11381, #43951, #4627, #7765, #41043, #18328, #37005, #22145 ),
 .UNSPECIFIED., .F., .T. ) 
 B_SPLINE_CURVE_WITH_KNOTS ( ( 3, 2, 2, 2, 3 ),
 ( 0.9699999999999999734, 0.9725000000000000311, 0.9749999999999999778, 0.9775000000000000355, 0.9799999999999999822 ),
 .UNSPECIFIED. ) 
 CURVE ( )  GEOMETRIC_REPRESENTATION_ITEM ( )  RATIONAL_B_SPLINE_CURVE ( ( 1.000000000000000000, 0.9238795325112869605, 1.000000000000000000, 0.9238795325112869605, 1.000000000000000000, 0.9238795325112869605, 1.000000000000000000, 0.9238795325112869605, 1.000000000000000000 ) ) 
 REPRESENTATION_ITEM ( '' )  ) ;
#14373 = CARTESIAN_POINT ( 'NONE',  ( 0.7646288533564489232, 0.1113553986120547346, 0.3395669291338583307 ) ) ;
#14374 = DIRECTION ( 'NONE',  ( -1.000000000000000000, 0.000000000000000000, 0.000000000000000000 ) ) ;
#14375 = CARTESIAN_POINT ( 'NONE',  ( -0.8107537697050253289, 0.1574803149606300301, 0.9965551180027087952 ) ) ;
#14376 = CARTESIAN_POINT ( 'NONE',  ( -0.1113553986120547346, -0.1013779527559055121, 0.1113553986120547346 ) ) ;
#14377 = CARTESIAN_POINT ( 'NONE',  ( 0.8759842519685039353, 0.1574803149606299191, 1.742125984144440975 ) ) ;
#14378 = ORIENTED_EDGE ( 'NONE', *, *, #29447, .T. ) ;
#14379 = CARTESIAN_POINT ( 'NONE',  ( -0.1377952755905511861, 0.1564960629921283985, 0.8070866141732283561 ) ) ;
#14380 = CARTESIAN_POINT ( 'NONE',  ( 0.8759842519685039353, -0.1574803149606299191, 0.7480314960629921295 ) ) ;
#14381 = CARTESIAN_POINT ( 'NONE',  ( 0.1643592241977981927, -0.08109105093932868213, -0.1404568431685181695 ) ) ;
#14382 = DIRECTION ( 'NONE',  ( 1.000000000000000000, 0.000000000000000000, -4.336808689942014778E-16 ) ) ;
#14383 = AXIS2_PLACEMENT_3D ( 'NONE', #17366, #42986, #29155 ) ;
#14384 = DIRECTION ( 'NONE',  ( 0.000000000000000000, 0.000000000000000000, 1.000000000000000000 ) ) ;
#14385 = CARTESIAN_POINT ( 'NONE',  ( 0.9873396505805591694, -0.1113553986120547346, 0.1525590550105832555 ) ) ;
#14386 = CARTESIAN_POINT ( 'NONE',  ( -0.1787899950787401882, -0.07923228341080354453, 0.000000000000000000 ) ) ;
#14387 = CARTESIAN_POINT ( 'NONE',  ( 0.4330708661417331795, 0.1864803149606300281, 1.186023622047243986 ) ) ;
#14388 = CARTESIAN_POINT ( 'NONE',  ( -0.1574803149606300301, -1.555610236112946021, -0.06523048226347956391 ) ) ;
#14389 = CARTESIAN_POINT ( 'NONE',  ( 0.1787899950787401882, -0.8124999999462361178, -2.189545951927503898E-17 ) ) ;
#14390 = CARTESIAN_POINT ( 'NONE',  ( -0.7185039370078746268, -0.06523048226347956391, 0.06151574792396910518 ) ) ;
#14392 = VECTOR ( 'NONE', #30974, 39.37007874015748143 ) ;
#14391 = CARTESIAN_POINT ( 'NONE',  ( -0.06523048226347956391, -1.019192913385827293, -0.1574803149606300301 ) ) ;
#14394 = ( BOUNDED_CURVE ( )  B_SPLINE_CURVE ( 2, ( #12833, #24084, #17343, #31977, #9217, #20468, #42715, #46565, #17107, #31748, #9931, #28389, #8311, #45857, #33989, #1115, #35104, #15775, #2250, #27927, #13299, #31514, #31048, #23836, #11119, #3670, #21893, #3439, #18293, #28879, #29125, #21405, #32220, #25250, #46805, #43916, #32934, #7029, #14238, #22113, #10165, #297, #36738, #24773, #13990, #47289, #28640, #21655, #39371, #55, #36515, #10409, #14701, #39840, #25738, #25012, #43439, #43199, #3898, #36287, #40311, #29376, #14944, #10645, #39610, #18052, #33176, #6786, #36031, #40076, #25507, #3192, #7493, #32699, #42958, #43678, #18523, #17820, #7275, #6555, #21165, #35797, #14467, #2941, #32467, #47045, #17578, #10888, #29827, #26441, #524, #34334, #1465 ),
 .UNSPECIFIED., .F., .T. ) 
 B_SPLINE_CURVE_WITH_KNOTS ( ( 3, 2, 2, 2, 2, 2, 2, 2, 2, 2, 2, 2, 2, 2, 2, 2, 2, 2, 2, 2, 2, 2, 2, 2, 2, 2, 2, 2, 2, 2, 2, 2, 2, 2, 2, 2, 2, 2, 2, 2, 2, 2, 2, 2, 2, 2, 3 ),
 ( 0.000000000000000000, 0.01120958318856041767, 0.03362875003688474418, 0.05604791688520911058, 0.07846708373353343535, 0.1008862505818577671, 0.1233054174301821265, 0.1457245842785064582, 0.1681437511268307761, 0.1905629179751551494, 0.2129820848234795228, 0.2354012516718038128, 0.2578204185201281584, 0.2802395853684525040, 0.3026587522167768496, 0.3250779190651011952, 0.3474970859134255963, 0.3699162527617498308, 0.3923354196100741764, 0.4147545864583985220, 0.4371737533067229231, 0.4595929201550472687, 0.4820120870033716143, 0.5044312538516959599, 0.5268504207000203055, 0.5492695875483445400, 0.5716887543966688856, 0.5941079212449933422, 0.6165270880933176878, 0.6389462549416420334, 0.6613654217899663790, 0.6837845886382906135, 0.7062037554866149591, 0.7286229223349393047, 0.7510420891832636503, 0.7734612560315881069, 0.7958804228799124525, 0.8182995897282366871, 0.8407187565765610326, 0.8631379234248853782, 0.8855570902732097238, 0.9079762571215340694, 0.9303954239698584150, 0.9528145908181826496, 0.9752337576665071062, 0.9976529245148314518, 1.000000000000000000 ),
 .UNSPECIFIED. ) 
 CURVE ( )  GEOMETRIC_REPRESENTATION_ITEM ( )  RATIONAL_B_SPLINE_CURVE ( ( 0.9619397662556434803, 0.9619397670555891455, 1.000000000000000000, 0.9238795325112869605, 1.000000000000000000, 0.9238795325112869605, 1.000000000000000000, 0.9238795325112869605, 1.000000000000000000, 0.9238795325112869605, 1.000000000000000000, 0.9238795325112869605, 1.000000000000000000, 0.9238795325112869605, 1.000000000000000000, 0.9238795325112869605, 1.000000000000000000, 0.9238795325112869605, 1.000000000000000000, 0.9238795325112869605, 1.000000000000000000, 0.9238795325112869605, 1.000000000000000000, 0.9238795325112869605, 1.000000000000000000, 0.9238795325112869605, 1.000000000000000000, 0.9238795325112869605, 1.000000000000000000, 0.9238795325112869605, 1.000000000000000000, 0.9238795325112869605, 1.000000000000000000, 0.9238795325112869605, 1.000000000000000000, 0.9238795325112869605, 1.000000000000000000, 0.9238795325112869605, 1.000000000000000000, 0.9238795325112869605, 1.000000000000000000, 0.9238795325112869605, 1.000000000000000000, 0.9238795325112869605, 1.000000000000000000, 0.9238795325112869605, 1.000000000000000000, 0.9238795325112869605, 1.000000000000000000, 0.9238795325112869605, 1.000000000000000000, 0.9238795325112869605, 1.000000000000000000, 0.9238795325112869605, 1.000000000000000000, 0.9238795325112869605, 1.000000000000000000, 0.9238795325112869605, 1.000000000000000000, 0.9238795325112869605, 1.000000000000000000, 0.9238795325112869605, 1.000000000000000000, 0.9238795325112869605, 1.000000000000000000, 0.9238795325112869605, 1.000000000000000000, 0.9238795325112869605, 1.000000000000000000, 0.9238795325112869605, 1.000000000000000000, 0.9238795325112869605, 1.000000000000000000, 0.9238795325112869605, 1.000000000000000000, 0.9238795325112869605, 1.000000000000000000, 0.9238795325112869605, 1.000000000000000000, 0.9238795325112869605, 1.000000000000000000, 0.9238795325112869605, 1.000000000000000000, 0.9238795325112869605, 1.000000000000000000, 0.9238795325112869605, 1.000000000000000000, 0.9238795325112869605, 1.000000000000000000, 0.9238795325112869605, 1.000000000000000000, 0.9920309044323080139, 0.9857303872709801684 ) ) 
 REPRESENTATION_ITEM ( '' )  ) ;
#14393 = CARTESIAN_POINT ( 'NONE',  ( 0.7646288533564489232, -0.1113553986120547346, 0.8907480313885355327 ) ) ;
#14395 = CARTESIAN_POINT ( 'NONE',  ( -1.033464566929133799, 0.000000000000000000, 1.259842519577511810 ) ) ;
#14396 = CARTESIAN_POINT ( 'NONE',  ( -0.6971942568897626646, 0.07405724077823318263, 0.3543307086076538659 ) ) ;
#14397 = ORIENTED_EDGE ( 'NONE', *, *, #2323, .F. ) ;
#14398 = ORIENTED_EDGE ( 'NONE', *, *, #24160, .T. ) ;
#14399 = ORIENTED_EDGE ( 'NONE', *, *, #8109, .T. ) ;
#14400 = CARTESIAN_POINT ( 'NONE',  ( -0.9500414927467378812, -0.1787899950787401604, 1.673228346402929834 ) ) ;
#14401 = VERTEX_POINT ( 'NONE', #44155 ) ;
#14402 = CARTESIAN_POINT ( 'NONE',  ( 0.06523048226347956391, -1.265255905404284453, 0.1574803149606297803 ) ) ;
#14403 = CARTESIAN_POINT ( 'NONE',  ( -1.002407869896990045, -0.1264236179284866091, 0.7701771653005669016 ) ) ;
#14404 = CARTESIAN_POINT ( 'NONE',  ( 1.054774247047244540, 0.07405724077823318263, 0.1476377952218269618 ) ) ;
#14405 = CARTESIAN_POINT ( 'NONE',  ( -1.033464566929133799, 1.928577636452524610E-17, 2.869337061179095023E-17 ) ) ;
#14406 = CARTESIAN_POINT ( 'NONE',  ( 1.054774247047244540, 0.07405724077823318263, 0.6988188975840318173 ) ) ;
#14407 = CARTESIAN_POINT ( 'NONE',  ( -0.9500414927467377701, 0.1787899950787401604, 0.7381889763241898939 ) ) ;
#14408 = CARTESIAN_POINT ( 'NONE',  ( 0.2204724409448818867, 0.07955613945526338049, 0.1377952755905511861 ) ) ;
#14409 = ADVANCED_FACE ( 'NONE', ( #7737 ), #17827, .F. ) ;
#14410 = DIRECTION ( 'NONE',  ( 0.000000000000000000, 0.000000000000000000, 1.000000000000000000 ) ) ;
#14411 = CARTESIAN_POINT ( 'NONE',  ( 0.1574803149606300301, -0.2367125983176700255, 0.06523048226347956391 ) ) ;
#14412 = CARTESIAN_POINT ( 'NONE',  ( -0.7185039370078746268, 0.06523048226347956391, 1.867618110128693720 ) ) ;
#14413 = ORIENTED_EDGE ( 'NONE', *, *, #7127, .T. ) ;
#14414 = CYLINDRICAL_SURFACE ( 'NONE', #1916, 0.009842519685039423719 ) ;
#14415 = CARTESIAN_POINT ( 'NONE',  ( -0.9873396505805591694, 0.1113553986120547346, 0.4872047244094488416 ) ) ;
#14416 = CARTESIAN_POINT ( 'NONE',  ( 0.8759842519685039353, -0.1787899950787401882, 1.473917322780881722 ) ) ;
#14417 = CARTESIAN_POINT ( 'NONE',  ( -1.033464566929134687, -0.06523048226347956391, 1.582185039370079149 ) ) ;
#14418 = ORIENTED_EDGE ( 'NONE', *, *, #43208, .T. ) ;
#14419 = AXIS2_PLACEMENT_3D ( 'NONE', #29743, #40457, #7641 ) ;
#14420 = CARTESIAN_POINT ( 'NONE',  ( -0.1787899950787401604, -1.672368062717427106, -0.07405724077823318263 ) ) ;
#14421 = EDGE_LOOP ( 'NONE', ( #12806, #29972, #28451, #5450 ) ) ;
#14422 = ORIENTED_EDGE ( 'NONE', *, *, #13012, .T. ) ;
#14423 = CARTESIAN_POINT ( 'NONE',  ( -1.033464566929133799, 0.000000000000000000, 1.151574803149606474 ) ) ;
#14424 = CARTESIAN_POINT ( 'NONE',  ( 0.1787899950787401604, -0.9281496062454495100, 0.07405724077823318263 ) ) ;
#14425 = CARTESIAN_POINT ( 'NONE',  ( 1.033464566929133799, 0.000000000000000000, 1.033464566929133799 ) ) ;
#14426 = DIRECTION ( 'NONE',  ( -1.000000000000000000, 0.000000000000000000, 0.000000000000000000 ) ) ;
#14427 = CARTESIAN_POINT ( 'NONE',  ( 0.6971942568897637749, 2.189545951927499583E-17, 1.734744094434425232 ) ) ;
#14428 = CARTESIAN_POINT ( 'NONE',  ( 1.054774247047244540, 0.07405724077823318263, 0.3001968503399373711 ) ) ;
#14429 = CARTESIAN_POINT ( 'NONE',  ( -0.1797182628040039087, -0.1560477465909194950, 0.07444174185955065859 ) ) ;
#14430 = CARTESIAN_POINT ( 'NONE',  ( 0.1264236179284866091, -0.1492381414575852383, -0.1264236179284866091 ) ) ;
#14431 = CARTESIAN_POINT ( 'NONE',  ( -0.1264236179284866091, -0.2711614172690712810, 0.1264236179284866091 ) ) ;
#14432 = DIRECTION ( 'NONE',  ( 1.000000000000000000, 0.000000000000000000, -7.083454193571960199E-15 ) ) ;
#14433 = CARTESIAN_POINT ( 'NONE',  ( 0.8759842519685039353, 0.1787899950787401882, 0.5437992125446614589 ) ) ;
#14434 = EDGE_CURVE ( 'NONE', #47261, #14468, #20817, .T. ) ;
#14435 = CARTESIAN_POINT ( 'NONE',  ( -0.8019270111902716547, 0.1787899950787401604, 0.9448818897100165204 ) ) ;
#14436 = CARTESIAN_POINT ( 'NONE',  ( 0.000000000000000000, 0.000000000000000000, -0.3149606299212598381 ) ) ;
#14437 = CARTESIAN_POINT ( 'NONE',  ( -1.100456976456230270E-17, -1.782524124543677368, -0.1797182628040039365 ) ) ;
#14438 = DIRECTION ( 'NONE',  ( 0.000000000000000000, 0.000000000000000000, -1.000000000000000000 ) ) ;
#14439 = CARTESIAN_POINT ( 'NONE',  ( 0.9500414927467378812, -0.1787899950787401604, 1.673228346402929834 ) ) ;
#14441 = DIRECTION ( 'NONE',  ( 0.000000000000000000, 0.000000000000000000, 1.000000000000000000 ) ) ;
#14440 = LINE ( 'NONE', #36489, #4593 ) ;
#14442 = VERTEX_POINT ( 'NONE', #40316 ) ;
#14443 = CARTESIAN_POINT ( 'NONE',  ( 0.1476377952755906220, 0.5323553679591568333, -0.7566348232351032266 ) ) ;
#14444 = DIRECTION ( 'NONE',  ( 0.000000000000000000, 0.1045284632676499598, -0.9945218953682736229 ) ) ;
#14445 = CARTESIAN_POINT ( 'NONE',  ( -0.1787899950787401604, -0.1998031495525358359, 0.07405724077823318263 ) ) ;
#14446 = CARTESIAN_POINT ( 'NONE',  ( 0.9412147342319837628, 0.1574803149606300301, 0.4798228345381422288 ) ) ;
#14447 = CARTESIAN_POINT ( 'NONE',  ( 0.7495606340400177148, 0.1264236179284866091, 0.6274606298674959559 ) ) ;
#14448 = CARTESIAN_POINT ( 'NONE',  ( 0.1264236179284866091, -1.048720472387181024, 0.1264236179284866091 ) ) ;
#14449 = CARTESIAN_POINT ( 'NONE',  ( 0.9500414927467378812, -0.1787899950787401604, 0.05905511805647267048 ) ) ;
#14450 = DIRECTION ( 'NONE',  ( -3.469446951953614978E-15, -1.000000000000000000, 3.995705278811693553E-31 ) ) ;
#14451 = CARTESIAN_POINT ( 'NONE',  ( -0.9500414927467378812, 0.1787899950787401604, 1.525590551127340433 ) ) ;
#14452 = VERTEX_POINT ( 'NONE', #22120 ) ;
#14453 = CARTESIAN_POINT ( 'NONE',  ( -1.054774247047244096, 0.000000000000000000, 1.208169291284818980 ) ) ;
#14454 = CARTESIAN_POINT ( 'NONE',  ( -0.2741778990008360561, -0.1449014624352426839, -0.7916190721464555491 ) ) ;
#14455 = CARTESIAN_POINT ( 'NONE',  ( 1.054774247047244540, 0.07405724077823318263, 1.092519684985605810 ) ) ;
#14456 = CARTESIAN_POINT ( 'NONE',  ( 1.054774247047244540, 0.07405724077823318263, 1.756889763725764553 ) ) ;
#14457 = CARTESIAN_POINT ( 'NONE',  ( -0.9500414927467378812, -0.1787899950787401604, 0.9596456692375764375 ) ) ;
#14458 = DIRECTION ( 'NONE',  ( -0.000000000000000000, 1.000000000000000000, -0.000000000000000000 ) ) ;
#14459 = CARTESIAN_POINT ( 'NONE',  ( -0.1030451738610134865, -0.2360010733950600459, -0.03001342526388867810 ) ) ;
#14460 = CARTESIAN_POINT ( 'NONE',  ( 0.6971942568897648851, -0.07405724077823297447, 0.3641732282926931630 ) ) ;
#14461 = CARTESIAN_POINT ( 'NONE',  ( -0.6971942568897626646, -0.07405724077823297447, 0.2017716534895435399 ) ) ;
#14462 = PRODUCT_DEFINITION_CONTEXT ( 'detailed design', #7348, 'design' ) ;
#14463 = CARTESIAN_POINT ( 'NONE',  ( -0.7495606340400177148, 0.1264236179284866091, 0.6668307086076534773 ) ) ;
#14464 = CARTESIAN_POINT ( 'NONE',  ( 1.033464566929134687, -0.06523048226347956391, 1.572342519577513142 ) ) ;
#14465 = ORIENTED_EDGE ( 'NONE', *, *, #40238, .F. ) ;
#14466 = EDGE_CURVE ( 'NONE', #43835, #40552, #33728, .T. ) ;
#14467 = CARTESIAN_POINT ( 'NONE',  ( 0.1264236179284866091, -0.06938976372576398377, 0.1264236179284866091 ) ) ;
#14468 = VERTEX_POINT ( 'NONE', #19231 ) ;
#14469 = ORIENTED_EDGE ( 'NONE', *, *, #41793, .F. ) ;
#14470 = CARTESIAN_POINT ( 'NONE',  ( 0.9500414927467378812, 0.1787899950787401604, 0.8612204723871809131 ) ) ;
#14471 = CARTESIAN_POINT ( 'NONE',  ( 0.6971942568897648851, 0.07405724077823318263, 1.107283464513165727 ) ) ;
#14472 = CARTESIAN_POINT ( 'NONE',  ( -0.6971942568897648851, 0.07405724077823318263, 1.811023621993480548 ) ) ;
#14473 = EDGE_CURVE ( 'NONE', #38318, #39969, #3023, .T. ) ;
#14474 = CARTESIAN_POINT ( 'NONE',  ( 0.6971942568897648851, 0.07405724077823318263, 1.968503936954110189 ) ) ;
#14475 = DIRECTION ( 'NONE',  ( -5.159318851433039196E-16, -0.6156614753256610673, -0.7880107536067199048 ) ) ;
#14476 = CARTESIAN_POINT ( 'NONE',  ( 0.07405724077823318263, -1.327879873741049765, -0.1787899950787401604 ) ) ;
#14477 = EDGE_LOOP ( 'NONE', ( #29063, #6350 ) ) ;
#14478 = CARTESIAN_POINT ( 'NONE',  ( -0.1264236179284866091, -0.2416338582139531399, -0.1264236179284866091 ) ) ;
#14479 = CARTESIAN_POINT ( 'NONE',  ( -0.3161444924769509779, 1.025704337919491005, -1.138861239548321524 ) ) ;
#14480 = VERTEX_POINT ( 'NONE', #23315 ) ;
#14481 = CARTESIAN_POINT ( 'NONE',  ( 0.000000000000000000, -0.1193342091828950846, -0.06889763779527559306 ) ) ;
#14482 = CARTESIAN_POINT ( 'NONE',  ( -0.2471889898701305766, -0.06575181108605680780, 0.09853485309532654390 ) ) ;
#14483 = CARTESIAN_POINT ( 'NONE',  ( 0.8019270111902717657, 0.1787899950787401604, 0.03444881884387430981 ) ) ;
#14484 = AXIS2_PLACEMENT_3D ( 'NONE', #2917, #25224, #32674 ) ;
#14485 = CARTESIAN_POINT ( 'NONE',  ( -0.07405724077823318263, -1.740157480261197875, -0.1787899950787401604 ) ) ;
#14486 = VECTOR ( 'NONE', #1008, 39.37007874015748143 ) ;
#14487 = CARTESIAN_POINT ( 'NONE',  ( -0.9500414927467377701, -0.1787899950787401604, 0.5314960629383620461 ) ) ;
#14488 = CARTESIAN_POINT ( 'NONE',  ( -0.9873396505805591694, 0.1113553986120547346, 0.6742125983176693316 ) ) ;
#14490 = CARTESIAN_POINT ( 'NONE',  ( -0.7108390435763994875, 0.01258011831628214061, 1.983038464472898221 ) ) ;
#14489 = CARTESIAN_POINT ( 'NONE',  ( 0.07444174185955065859, -1.248567431630288826, 0.1797182628040039087 ) ) ;
#14491 = CARTESIAN_POINT ( 'NONE',  ( -0.9873396505805591694, 0.1113553986120547346, 1.195866141732283561 ) ) ;
#14492 = CARTESIAN_POINT ( 'NONE',  ( 0.8019270111902717657, -0.1787899950787401604, 1.235236220418678199 ) ) ;
#14493 = CARTESIAN_POINT ( 'NONE',  ( 0.6971942568897648851, 0.07405724077823318263, 1.692913385773008539 ) ) ;
#14494 = CARTESIAN_POINT ( 'NONE',  ( -0.7185039370078739607, 1.928577636452523993E-17, 0.6102362203649134287 ) ) ;
#14495 = LINE ( 'NONE', #25539, #8244 ) ;
#14496 = CARTESIAN_POINT ( 'NONE',  ( 0.000000000000000000, -0.09842519685039370636, 0.000000000000000000 ) ) ;
#14497 = CARTESIAN_POINT ( 'NONE',  ( -0.7185039370078746268, 0.06523048226347956391, 1.788877952648378233 ) ) ;
#14498 = CARTESIAN_POINT ( 'NONE',  ( 0.8759842519685039353, -0.1787899950787401882, 0.1304133857730082613 ) ) ;
#14499 = CARTESIAN_POINT ( 'NONE',  ( 0.7039992537011210416, -0.02173256458483645986, 0.03937460100240990774 ) ) ;
#14501 = CARTESIAN_POINT ( 'NONE',  ( -0.7185039370078746268, -0.06523048226347956391, 0.5339566928058587791 ) ) ;
#14500 = CARTESIAN_POINT ( 'NONE',  ( 0.8759842519685039353, -0.1787899950787401882, 1.232775590497417362 ) ) ;
#14502 = CYLINDRICAL_SURFACE ( 'NONE', #5171, 0.1574803149606299191 ) ;
#14503 = CARTESIAN_POINT ( 'NONE',  ( -0.8019270111902717657, -0.1787899950787401604, 1.190944881836001112 ) ) ;
#14504 = CARTESIAN_POINT ( 'NONE',  ( 0.7185039370078739607, 1.928577636452523993E-17, 0.5314960628845992741 ) ) ;
#14505 = VERTEX_POINT ( 'NONE', #4353 ) ;
#14506 = ADVANCED_FACE ( 'NONE', ( #26686 ), #15900, .F. ) ;
#14507 = CARTESIAN_POINT ( 'NONE',  ( 0.9303600321982549159, 0.1621629823367503609, 0.03937005601395735660 ) ) ;
#14508 = CARTESIAN_POINT ( 'NONE',  ( 0.8107537697050253289, 0.1574803149606300301, 0.2583661417322835052 ) ) ;
#14509 = CARTESIAN_POINT ( 'NONE',  ( 0.1574803149606300023, 0.4814845645395590679, -0.4766254685646189593 ) ) ;
#14510 = CARTESIAN_POINT ( 'NONE',  ( -0.9412147342319837628, -0.1574803149606297803, 0.4256889762704256230 ) ) ;
#14511 = ORIENTED_EDGE ( 'NONE', *, *, #20013, .F. ) ;
#14512 = ORIENTED_EDGE ( 'NONE', *, *, #23827, .T. ) ;
#14513 = CARTESIAN_POINT ( 'NONE',  ( 1.054774247047244096, 0.000000000000000000, 1.400098425143086800 ) ) ;
#14515 = CARTESIAN_POINT ( 'NONE',  ( -1.033464566929136907, -0.06523048226347749612, 1.385334645669292541 ) ) ;
#14514 = CARTESIAN_POINT ( 'NONE',  ( -0.7185039370078746268, -0.06523048226347956391, 1.764271653543307616 ) ) ;
#14516 = CARTESIAN_POINT ( 'NONE',  ( 0.000000000000000000, 0.000000000000000000, -0.1045766232635885612 ) ) ;
#14517 = CARTESIAN_POINT ( 'NONE',  ( 3.284318927891251994E-17, -0.06938976372576398377, 0.1787899950787401882 ) ) ;
#14518 = ORIENTED_EDGE ( 'NONE', *, *, #582, .T. ) ;
#14519 = FACE_OUTER_BOUND ( 'NONE', #45402, .T. ) ;
#14520 = EDGE_CURVE ( 'NONE', #34914, #2197, #3005, .T. ) ;
#14521 = VECTOR ( 'NONE', #15394, 39.37007874015748143 ) ;
#14522 = DIRECTION ( 'NONE',  ( 0.000000000000000000, 0.000000000000000000, 1.000000000000000000 ) ) ;
#14523 = FILL_AREA_STYLE ('',( #3495 ) ) ;
#14524 = CARTESIAN_POINT ( 'NONE',  ( -0.4330708661417340677, 0.1574803149606330277, -1.186023622047243986 ) ) ;
#14525 = CARTESIAN_POINT ( 'NONE',  ( 0.7495606340400177148, -0.1264236179284866091, 0.6422244093950550958 ) ) ;
#14526 = EDGE_LOOP ( 'NONE', ( #37633, #3262, #14367, #1765 ) ) ;
#14527 = CARTESIAN_POINT ( 'NONE',  ( 0.1264236179284866091, -1.801673228292693052, 0.1264236179284866091 ) ) ;
#14528 = CARTESIAN_POINT ( 'NONE',  ( -0.8019270111902717657, 0.1787899950787401604, 1.181102362150960428 ) ) ;
#14529 = VERTEX_POINT ( 'NONE', #22830 ) ;
#14530 = EDGE_CURVE ( 'NONE', #12477, #21515, #29069, .T. ) ;
#14531 = VECTOR ( 'NONE', #34559, 39.37007874015748143 ) ;
#14532 = CARTESIAN_POINT ( 'NONE',  ( -0.8019270111902717657, 0.1787899950787401604, 0.8267716534895444003 ) ) ;
#14533 = ADVANCED_FACE ( 'NONE', ( #5082 ), #15423, .T. ) ;
#14534 = CARTESIAN_POINT ( 'NONE',  ( -0.8759842519685039353, -0.1574803149606299191, 0.3543307086614173040 ) ) ;
#14535 = CYLINDRICAL_SURFACE ( 'NONE', #24413, 0.009842519685039378616 ) ;
#14536 = CARTESIAN_POINT ( 'NONE',  ( 0.07405724077823318263, -0.8948090075993178072, -0.1787899950787401604 ) ) ;
#14537 = CARTESIAN_POINT ( 'NONE',  ( -0.1371053627424283494, -0.08956161432658386878, 0.08897719781895610525 ) ) ;
#14538 = AXIS2_PLACEMENT_3D ( 'NONE', #44250, #28561, #7600 ) ;
#14539 = CARTESIAN_POINT ( 'NONE',  ( -0.07405724077823318263, 0.1102362205262043815, -0.1787899950787401604 ) ) ;
#14540 = ORIENTED_EDGE ( 'NONE', *, *, #35690, .T. ) ;
#14541 = CARTESIAN_POINT ( 'NONE',  ( -0.9412147342319837628, 0.1574803149606300301, 0.5585629920184573827 ) ) ;
#14542 = CARTESIAN_POINT ( 'NONE',  ( -1.054774247047244540, 0.07405724077823318263, 0.7332677164816707727 ) ) ;
#14543 = ORIENTED_EDGE ( 'NONE', *, *, #18190, .F. ) ;
#14544 = AXIS2_PLACEMENT_3D ( 'NONE', #867, #12162, #26788 ) ;
#14545 = CARTESIAN_POINT ( 'NONE',  ( -0.8019270111902716547, 0.1787899950787401604, 0.1181102361667090567 ) ) ;
#14546 = CARTESIAN_POINT ( 'NONE',  ( 0.8107537697050253289, 0.1574803149606300301, 0.6914370078740167402 ) ) ;
#14547 = CARTESIAN_POINT ( 'NONE',  ( 0.1270800023317771588, -0.8031934158822577885, -0.1270800023317771588 ) ) ;
#14548 = DIRECTION ( 'NONE',  ( -1.000000000000000000, -6.679788269418529283E-17, 0.000000000000000000 ) ) ;
#14549 = CARTESIAN_POINT ( 'NONE',  ( -0.7646288533564489232, -0.1113553986120547346, 1.441929133750740277 ) ) ;
#14550 = CARTESIAN_POINT ( 'NONE',  ( 0.6971942568897626646, 0.07405724077823318263, 0.7135826771115916234 ) ) ;
#14551 = CARTESIAN_POINT ( 'NONE',  ( 0.8019270111902716547, 0.1787899950787401604, 1.333661417269071281 ) ) ;
#14552 = CARTESIAN_POINT ( 'NONE',  ( -9.642888182262618425E-18, -0.6279527559055118058, -0.1574803149606299191 ) ) ;
#14553 = CYLINDRICAL_SURFACE ( 'NONE', #16204, 0.1574803149606299191 ) ;
#14554 = CARTESIAN_POINT ( 'NONE',  ( 1.181102362204724310, -0.3937007874015748254, -0.9842519685039370358 ) ) ;
#14555 = CARTESIAN_POINT ( 'NONE',  ( 1.033464566929134687, -0.06523048226347956391, 1.464074803149607140 ) ) ;
#14557 = CARTESIAN_POINT ( 'NONE',  ( 1.033464566929133799, 0.000000000000000000, 1.574803149498771537 ) ) ;
#14556 = CARTESIAN_POINT ( 'NONE',  ( 0.7949805117774454422, -0.1517228856934477454, 1.986644361401757930 ) ) ;
#14558 = AXIS2_PLACEMENT_3D ( 'NONE', #44094, #44789, #238 ) ;
#14559 = CARTESIAN_POINT ( 'NONE',  ( 1.033464566929134687, -0.06523048226347956391, 1.729822834538142784 ) ) ;
#14560 = CARTESIAN_POINT ( 'NONE',  ( -0.1113553986120547346, -0.6131889762704252345, -0.1113553986120547346 ) ) ;
#14562 = DIRECTION ( 'NONE',  ( 0.000000000000000000, -1.000000000000000000, 0.000000000000000000 ) ) ;
#14561 = CARTESIAN_POINT ( 'NONE',  ( 1.002407869896990045, -0.1264236179284866091, 0.7258858267178898149 ) ) ;
#14563 = EDGE_CURVE ( 'NONE', #2430, #31278, #30071, .T. ) ;
#14564 = CARTESIAN_POINT ( 'NONE',  ( 1.033464566929134687, 0.06523048226347956391, 1.547736220472440305 ) ) ;
#14565 = ORIENTED_EDGE ( 'NONE', *, *, #26639, .T. ) ;
#14566 = ADVANCED_FACE ( 'NONE', ( #12301 ), #7936, .F. ) ;
#14567 = CARTESIAN_POINT ( 'NONE',  ( 0.4620708661417345375, 0.6102362204724407491, 1.186023622047243986 ) ) ;
#14568 = CARTESIAN_POINT ( 'NONE',  ( 0.000000000000000000, 0.000000000000000000, -0.3149606299212598381 ) ) ;
#14569 = CARTESIAN_POINT ( 'NONE',  ( 0.7495606340400177148, -0.1264236179284866091, 0.9128937007336377363 ) ) ;
#14570 = CARTESIAN_POINT ( 'NONE',  ( 0.7185039370078739607, 1.928577636452523993E-17, 1.368110236220472675 ) ) ;
#14571 = CARTESIAN_POINT ( 'NONE',  ( 0.1574803149606300301, -1.506397637795275024, 0.06523048226347956391 ) ) ;
#14572 = FACE_OUTER_BOUND ( 'NONE', #36459, .T. ) ;
#14573 = CARTESIAN_POINT ( 'NONE',  ( -0.7495606340400177148, -0.1264236179284866091, 0.04675196845017354913 ) ) ;
#14574 = CARTESIAN_POINT ( 'NONE',  ( 0.06523048226347956391, 0.1176181102362204994, -0.1574803149606297803 ) ) ;
#14575 = EDGE_LOOP ( 'NONE', ( #36427, #10277, #41225, #27340 ) ) ;
#14576 = CARTESIAN_POINT ( 'NONE',  ( -0.1574803149606300301, -0.3351377951680634681, -0.06523048226347956391 ) ) ;
#14577 = CARTESIAN_POINT ( 'NONE',  ( -1.054774247047244540, 0.07405724077823318263, 1.638779527505292988 ) ) ;
#14578 = EDGE_CURVE ( 'NONE', #36213, #26985, #35222, .T. ) ;
#14579 = CARTESIAN_POINT ( 'NONE',  ( -0.6971942568897626646, 0.07405724077823318263, 0.4379921259304882519 ) ) ;
#14580 = VECTOR ( 'NONE', #13271, 39.37007874015748143 ) ;
#14581 = CARTESIAN_POINT ( 'NONE',  ( -0.2471922904502827645, 0.08571147543119535250, 0.06121067491482544420 ) ) ;
#14582 = CARTESIAN_POINT ( 'NONE',  ( 0.6195511811023621807, 0.9842519685039367028, -1.186023622047244430 ) ) ;
#14583 = CARTESIAN_POINT ( 'NONE',  ( 1.033464566929134687, 0.06523048226347956391, 0.2878937007874017850 ) ) ;
#14584 = CARTESIAN_POINT ( 'NONE',  ( 0.08643384275326014554, 0.09202339627320528515, -0.2355304684854532260 ) ) ;
#14585 = CARTESIAN_POINT ( 'NONE',  ( -0.2617290863461584904, 0.1662196327273373908, -0.8981458471588513737 ) ) ;
#14586 = CARTESIAN_POINT ( 'NONE',  ( -0.1787899950787401604, -0.4125255430323886419, -0.07405724077823318263 ) ) ;
#14587 = CARTESIAN_POINT ( 'NONE',  ( -0.1189464023891061012, -0.09842519685039370636, 0.1140809237429826761 ) ) ;
#14588 = FACE_OUTER_BOUND ( 'NONE', #18894, .T. ) ;
#14589 = CARTESIAN_POINT ( 'NONE',  ( 0.4330708661417322913, 0.000000000000000000, -0.9891732283464566011 ) ) ;
#14590 = PRODUCT ( 'Side Bracket', 'Side Bracket', '', ( #16610 ) ) ;
#14591 = CIRCLE ( 'NONE', #1568, 0.09842519685039370636 ) ;
#14592 = CARTESIAN_POINT ( 'NONE',  ( -1.054774247047244540, 0.07405724077823318263, 0.3395669290800945039 ) ) ;
#14593 = CARTESIAN_POINT ( 'NONE',  ( 0.2471902452994138577, -0.09796597228571109206, 0.01325394226265646895 ) ) ;
#14594 = ORIENTED_EDGE ( 'NONE', *, *, #33207, .F. ) ;
#14595 = CARTESIAN_POINT ( 'NONE',  ( -0.8019270111902716547, 0.1787899950787401604, 1.338582677111590069 ) ) ;
#14596 = ORIENTED_EDGE ( 'NONE', *, *, #11487, .F. ) ;
#14597 = CARTESIAN_POINT ( 'NONE',  ( 0.1787899950787401604, -1.169291338528914537, 0.07405724077823318263 ) ) ;
#14598 = CARTESIAN_POINT ( 'NONE',  ( 0.1787899950787401604, -1.439960629867495401, 0.07405724077823318263 ) ) ;
#14599 = FILL_AREA_STYLE_COLOUR ( '', #11051 ) ;
#14600 = CARTESIAN_POINT ( 'NONE',  ( 1.343418747613858155, 2.327466803393307249, 7.874015748031496769E-14 ) ) ;
#14601 = CARTESIAN_POINT ( 'NONE',  ( 0.7185039370078746268, 0.06523048226347956391, 0.3420275590551182798 ) ) ;
#14602 = PLANE ( 'NONE',  #6389 ) ;
#14603 = CARTESIAN_POINT ( 'NONE',  ( -0.8107537697050253289, 0.1574803149606300301, 0.9178149605223947516 ) ) ;
#14604 = CARTESIAN_POINT ( 'NONE',  ( -0.1574803149606300301, -0.1481299212598424508, -0.06523048226347956391 ) ) ;
#14605 = CARTESIAN_POINT ( 'NONE',  ( 0.7185039370078746268, 0.06523048226347956391, 1.828248031388536310 ) ) ;
#14606 = ADVANCED_FACE ( 'NONE', ( #7392 ), #46835, .F. ) ;
#14607 = CARTESIAN_POINT ( 'NONE',  ( -0.4620708661417322616, 0.1864803149606299448, 1.186023622047243986 ) ) ;
#14608 = CARTESIAN_POINT ( 'NONE',  ( 0.8107537697050253289, 0.1574803149606300301, 0.8489173228346468258 ) ) ;
#14609 = CARTESIAN_POINT ( 'NONE',  ( 0.7646288533564489232, 0.1113553986120547346, 1.363188976377952999 ) ) ;
#14610 = ADVANCED_FACE ( 'NONE', ( #10765 ), #9908, .F. ) ;
#14611 = AXIS2_PLACEMENT_3D ( 'NONE', #7414, #22920, #34424 ) ;
#14613 = CARTESIAN_POINT ( 'NONE',  ( 0.7185039370078746268, -0.06523048226347956391, 1.528051181102361378 ) ) ;
#14612 = CARTESIAN_POINT ( 'NONE',  ( 1.044119406988188947, 0.000000000000000000, 1.984498031469181134 ) ) ;
#14614 = CARTESIAN_POINT ( 'NONE',  ( 0.000000000000000000, 0.3740157480314960647, 0.9783464566929134243 ) ) ;
#14615 = ADVANCED_FACE ( 'NONE', ( #10035 ), #13726, .T. ) ;
#14616 = CARTESIAN_POINT ( 'NONE',  ( -0.2713383277233172297, 0.1500775187160213187, 0.9507557288134271811 ) ) ;
#14617 = ORIENTED_EDGE ( 'NONE', *, *, #1308, .T. ) ;
#14618 = ORIENTED_EDGE ( 'NONE', *, *, #39156, .F. ) ;
#14619 = CARTESIAN_POINT ( 'NONE',  ( -0.06523048226347956391, 0.1077755906587081480, 0.1574803149606297803 ) ) ;
#14620 = CARTESIAN_POINT ( 'NONE',  ( 3.284318927891251994E-17, -1.565452755851747924, 0.1787899950787401882 ) ) ;
#14621 = CARTESIAN_POINT ( 'NONE',  ( -0.1113553986120547346, -1.548228346349165285, 0.1113553986120547346 ) ) ;
#14622 = CARTESIAN_POINT ( 'NONE',  ( 0.1264236179284866091, -0.7682086613635590311, -0.1264236179284866091 ) ) ;
#14623 = CARTESIAN_POINT ( 'NONE',  ( -0.7646288533564489232, 0.1113553986120547346, 0.05413385816018952829 ) ) ;
#14624 = VECTOR ( 'NONE', #30485, 39.37007874015748854 ) ;
#14625 = CARTESIAN_POINT ( 'NONE',  ( -0.06523048226347956391, -1.004429133858267598, 0.1574803149606297803 ) ) ;
#14626 = CARTESIAN_POINT ( 'NONE',  ( 0.8759842519685039353, -0.1574803149606299191, 1.013779527451527551 ) ) ;
#14627 = DIRECTION ( 'NONE',  ( 0.000000000000000000, 1.000000000000000000, 0.000000000000000000 ) ) ;
#14628 = CARTESIAN_POINT ( 'NONE',  ( -0.8759842519685039353, 0.1787899950787401882, 0.3863188975840318173 ) ) ;
#14629 = ORIENTED_EDGE ( 'NONE', *, *, #22828, .T. ) ;
#14630 = CARTESIAN_POINT ( 'NONE',  ( -1.054774247047244540, -0.07405724077823318263, 1.599409448765135133 ) ) ;
#14631 = EDGE_LOOP ( 'NONE', ( #5975, #35684, #26323, #46704, #18224 ) ) ;
#14632 = CARTESIAN_POINT ( 'NONE',  ( 1.002407869896990045, 0.1264236179284866091, 1.724901574749385880 ) ) ;
#14633 = ORIENTED_EDGE ( 'NONE', *, *, #32550, .F. ) ;
#14634 = CARTESIAN_POINT ( 'NONE',  ( -0.7495606340400177148, -0.1264236179284866091, 0.7997047243556849594 ) ) ;
#14635 = CARTESIAN_POINT ( 'NONE',  ( 1.054774247047244540, 0.07405724077823318263, 0.3051181101824569919 ) ) ;
#14636 = CARTESIAN_POINT ( 'NONE',  ( 0.8759842519685039353, 0.000000000000000000, 4.498031496062992574 ) ) ;
#14637 = CARTESIAN_POINT ( 'NONE',  ( 0.6971942568897637749, 2.189545951927499583E-17, 0.7554133857730077617 ) ) ;
#14638 = CARTESIAN_POINT ( 'NONE',  ( -0.8019270111902716547, -0.1787899950787401604, 0.7578740156942688211 ) ) ;
#14639 = CARTESIAN_POINT ( 'NONE',  ( 0.002317115957668979941, -0.1025658529674488839, 0.09794161051882110947 ) ) ;
#14640 = LINE ( 'NONE', #17282, #1493 ) ;
#14641 = CARTESIAN_POINT ( 'NONE',  ( -0.8019270111902717657, -0.1787899950787401604, 1.510826771599780294 ) ) ;
#14642 = CARTESIAN_POINT ( 'NONE',  ( -0.8759842519685039353, 0.1574803149606299191, 1.938976377845228249 ) ) ;
#14643 = ORIENTED_EDGE ( 'NONE', *, *, #6749, .F. ) ;
#14644 = CARTESIAN_POINT ( 'NONE',  ( 1.033464566929133799, 1.928577636452524610E-17, 4.498031496062992574 ) ) ;
#14645 = CARTESIAN_POINT ( 'NONE',  ( 0.8019270111902716547, -0.1787899950787401604, 1.510826771599780294 ) ) ;
#14646 = CARTESIAN_POINT ( 'NONE',  ( -0.1407580821002830940, -0.09851383941439428860, -0.1134402804189334618 ) ) ;
#14647 = FACE_OUTER_BOUND ( 'NONE', #4504, .T. ) ;
#14648 = ORIENTED_EDGE ( 'NONE', *, *, #36692, .F. ) ;
#14649 = ( BOUNDED_CURVE ( )  B_SPLINE_CURVE ( 2, ( #36310, #325, #3465, #40331, #22140, #36766, #3926, #14976, #33910 ),
 .UNSPECIFIED., .F., .F. ) 
 B_SPLINE_CURVE_WITH_KNOTS ( ( 3, 2, 2, 2, 3 ),
 ( 0.7199999999999999734, 0.7225000000000000311, 0.7249999999999999778, 0.7275000000000000355, 0.7299999999999999822 ),
 .UNSPECIFIED. ) 
 CURVE ( )  GEOMETRIC_REPRESENTATION_ITEM ( )  RATIONAL_B_SPLINE_CURVE ( ( 1.000000000000000000, 0.9238795325112869605, 1.000000000000000000, 0.9238795325112869605, 1.000000000000000000, 0.9238795325112869605, 1.000000000000000000, 0.9238795325112869605, 1.000000000000000000 ) ) 
 REPRESENTATION_ITEM ( '' )  ) ;
#14650 = AXIS2_PLACEMENT_3D ( 'NONE', #23341, #38176, #19959 ) ;
#14651 = ORIENTED_EDGE ( 'NONE', *, *, #10658, .T. ) ;
#14652 = ORIENTED_EDGE ( 'NONE', *, *, #21097, .F. ) ;
#14653 = AXIS2_PLACEMENT_3D ( 'NONE', #16888, #5634, #45630 ) ;
#14654 = VECTOR ( 'NONE', #6122, 39.37007874015748143 ) ;
#14655 = VECTOR ( 'NONE', #33738, 39.37007874015748143 ) ;
#14656 = DIRECTION ( 'NONE',  ( 0.000000000000000000, 0.000000000000000000, 1.000000000000000000 ) ) ;
#14657 = CARTESIAN_POINT ( 'NONE',  ( -0.1264236179284866091, -0.8715551180564724554, -0.1264236179284866091 ) ) ;
#14658 = CARTESIAN_POINT ( 'NONE',  ( -0.2471922732848683135, -0.07885118474262710342, -0.07559718168567093610 ) ) ;
#14659 = CARTESIAN_POINT ( 'NONE',  ( 0.4736248074375464800, 1.798092712879862276, -3.826876940038421715 ) ) ;
#14660 = CARTESIAN_POINT ( 'NONE',  ( 0.8019270111902717657, 0.1787899950787401604, 0.2706692912848194243 ) ) ;
#14661 = CARTESIAN_POINT ( 'NONE',  ( -0.1270800023317771588, -0.1142170379295021632, 0.1270800023317771588 ) ) ;
#14662 = CARTESIAN_POINT ( 'NONE',  ( -0.1787899950787401604, -0.1320137320087663158, 0.07405724077823318263 ) ) ;
#14663 = CARTESIAN_POINT ( 'NONE',  ( -0.1787899950787401604, -0.3129921259304885850, 0.07405724077823318263 ) ) ;
#14664 = CARTESIAN_POINT ( 'NONE',  ( -1.094772975963752103E-17, -0.09399606293836239301, -0.1787899950787401882 ) ) ;
#14665 = CARTESIAN_POINT ( 'NONE',  ( 0.2471922931865138395, -0.07794380098771452881, -0.07736948232533663594 ) ) ;
#14666 = EDGE_CURVE ( 'NONE', #7011, #5868, #24655, .T. ) ;
#14667 = CARTESIAN_POINT ( 'NONE',  ( 0.6971942568897626646, 0.07405724077823318263, 0.6692913385289144257 ) ) ;
#14668 = ( BOUNDED_CURVE ( )  B_SPLINE_CURVE ( 2, ( #11946, #1126, #26567, #44033, #29944, #15785, #29488, #30414, #4013 ),
 .UNSPECIFIED., .F., .T. ) 
 B_SPLINE_CURVE_WITH_KNOTS ( ( 3, 2, 2, 2, 3 ),
 ( 0.1400000000000000133, 0.1424999999999999878, 0.1449999999999999900, 0.1474999999999999922, 0.1499999999999999944 ),
 .UNSPECIFIED. ) 
 CURVE ( )  GEOMETRIC_REPRESENTATION_ITEM ( )  RATIONAL_B_SPLINE_CURVE ( ( 1.000000000000000000, 0.9238795325112869605, 1.000000000000000000, 0.9238795325112869605, 1.000000000000000000, 0.9238795325112869605, 1.000000000000000000, 0.9238795325112869605, 1.000000000000000000 ) ) 
 REPRESENTATION_ITEM ( '' )  ) ;
#14669 = EDGE_CURVE ( 'NONE', #20105, #3237, #12867, .T. ) ;
#14671 = FACE_OUTER_BOUND ( 'NONE', #39654, .T. ) ;
#14670 = CARTESIAN_POINT ( 'NONE',  ( -0.8075642815980649258, 0.1651804164989427171, 0.03937007874015843040 ) ) ;
#14672 = CARTESIAN_POINT ( 'NONE',  ( 0.000000000000000000, 0.09842519685039370636, 0.000000000000000000 ) ) ;
#14673 = CARTESIAN_POINT ( 'NONE',  ( -1.033464566929134687, 0.06523048226347956391, 1.301673228238930502 ) ) ;
#14674 = CARTESIAN_POINT ( 'NONE',  ( 0.6971942568897637749, 2.189545951927499583E-17, 1.621555118056472455 ) ) ;
#14676 = DIRECTION ( 'NONE',  ( -1.000000000000000000, -0.000000000000000000, 0.000000000000000000 ) ) ;
#14675 = CARTESIAN_POINT ( 'NONE',  ( -0.1854358583624131085, -0.08093302715482435239, 0.1783713581464878017 ) ) ;
#14677 = CARTESIAN_POINT ( 'NONE',  ( 0.7495606340400177148, 0.1264236179284866091, 0.5093503936470236138 ) ) ;
#14678 = ADVANCED_FACE ( 'NONE', ( #31861 ), #46440, .T. ) ;
#14679 = EDGE_CURVE ( 'NONE', #5180, #14871, #21418, .T. ) ;
#14680 = CARTESIAN_POINT ( 'NONE',  ( 0.1264236179284866091, -0.3449803149068665364, 0.1264236179284866091 ) ) ;
#14682 = CARTESIAN_POINT ( 'NONE',  ( -1.054774247047244096, 0.000000000000000000, 1.990649606245448844 ) ) ;
#14681 = CARTESIAN_POINT ( 'NONE',  ( -0.8019270111902717657, 0.1787899950787401604, 0.4330708660879683536 ) ) ;
#14683 = CARTESIAN_POINT ( 'NONE',  ( -1.094772975963752103E-17, -1.073326771599779628, -0.1787899950787401882 ) ) ;
#14684 = CARTESIAN_POINT ( 'NONE',  ( 0.8019270111902717657, 0.1787899950787401604, 0.07874015742655145200 ) ) ;
#14685 = CIRCLE ( 'NONE', #900, 0.7874015748031495399 ) ;
#14686 = CARTESIAN_POINT ( 'NONE',  ( -1.002407869896990045, 0.1264236179284866091, 1.641240157426551161 ) ) ;
#14687 = ORIENTED_EDGE ( 'NONE', *, *, #45544, .F. ) ;
#14688 = CARTESIAN_POINT ( 'NONE',  ( -0.7495606340400177148, -0.1264236179284866091, 1.114665354276944909 ) ) ;
#14689 = CARTESIAN_POINT ( 'NONE',  ( 0.8107537697050254399, -0.1574803149606297803, 1.021161417322834497 ) ) ;
#14690 = CARTESIAN_POINT ( 'NONE',  ( 0.7495606340400177148, 0.1264236179284866091, 1.183562992072220599 ) ) ;
#14691 = CARTESIAN_POINT ( 'NONE',  ( -0.06523048226347956391, -1.127460629813733295, -0.1574803149606300301 ) ) ;
#14692 = CARTESIAN_POINT ( 'NONE',  ( 0.6971942568897648851, -0.07405724077823297447, 1.815944881835999558 ) ) ;
#14693 = CARTESIAN_POINT ( 'NONE',  ( -1.033464566929133799, 0.000000000000000000, 0.6397637795275591399 ) ) ;
#14694 = CARTESIAN_POINT ( 'NONE',  ( -0.6971942568897626646, 0.07405724077823318263, 0.9842519684501742638 ) ) ;
#14695 = CARTESIAN_POINT ( 'NONE',  ( 0.3100393700787401619, 3.796887221765908018E-17, 1.181102362204724310 ) ) ;
#14696 = FACE_OUTER_BOUND ( 'NONE', #14244, .T. ) ;
#14697 = CARTESIAN_POINT ( 'NONE',  ( 1.002407869896990045, 0.1264236179284866091, 0.2682086613635594752 ) ) ;
#14698 = CARTESIAN_POINT ( 'NONE',  ( -1.002407869896990045, -0.1264236179284866091, 0.2928149605761578567 ) ) ;
#14699 = CARTESIAN_POINT ( 'NONE',  ( -0.8019270111902717657, 0.1787899950787401604, 0.7037401574265510495 ) ) ;
#14700 = CARTESIAN_POINT ( 'NONE',  ( 0.9412147342319837628, 0.1574803149606300301, 1.700295275483023172 ) ) ;
#14701 = CARTESIAN_POINT ( 'NONE',  ( 3.284318927891251994E-17, 0.004429133912031243958, 0.1787899950787401882 ) ) ;
#14702 = CARTESIAN_POINT ( 'NONE',  ( 1.054774247047244096, 0.000000000000000000, 0.7357283464029290565 ) ) ;
#14703 = CARTESIAN_POINT ( 'NONE',  ( 1.054774247047244096, 0.000000000000000000, 1.011318897584031484 ) ) ;
#14704 = CARTESIAN_POINT ( 'NONE',  ( -0.8759842519685039353, 0.1787899950787401882, 1.843011810969858333 ) ) ;
#14705 = ORIENTED_EDGE ( 'NONE', *, *, #17009, .F. ) ;
#14706 = CARTESIAN_POINT ( 'NONE',  ( 1.054774247047244096, 0.000000000000000000, 1.951279527505291433 ) ) ;
#14707 = CARTESIAN_POINT ( 'NONE',  ( -0.8107537697050234415, -0.1574803149606297803, 0.1943897637795276023 ) ) ;
#14708 = CARTESIAN_POINT ( 'NONE',  ( 0.1264236179284866091, -1.251600346181994228, -0.1264236179284866091 ) ) ;
#14709 = ORIENTED_EDGE ( 'NONE', *, *, #25221, .T. ) ;
#14710 = CARTESIAN_POINT ( 'NONE',  ( -0.1787899950787401882, -0.3548228345919058890, 0.000000000000000000 ) ) ;
#14711 = CARTESIAN_POINT ( 'NONE',  ( -0.7185039370078739607, 1.928577636452523993E-17, 1.948818897530267602 ) ) ;
#14712 = ORIENTED_EDGE ( 'NONE', *, *, #18645, .F. ) ;
#14713 = CARTESIAN_POINT ( 'NONE',  ( 1.002407869896990045, -0.1264236179284866091, 1.237696850339937038 ) ) ;
#14714 = CIRCLE ( 'NONE', #24667, 0.1870078740157480324 ) ;
#14716 = EDGE_CURVE ( 'NONE', #47206, #7112, #25745, .T. ) ;
#14715 = CARTESIAN_POINT ( 'NONE',  ( 0.1574803149606299191, 1.086379535891623949, -0.03715491745706121784 ) ) ;
#14717 = CARTESIAN_POINT ( 'NONE',  ( -0.2471922904502826812, -0.04197619597928321789, 0.1314166662981948452 ) ) ;
#14718 = CARTESIAN_POINT ( 'NONE',  ( 1.002407869896990045, 0.1264236179284866091, 1.483759842465921075 ) ) ;
#14719 = CARTESIAN_POINT ( 'NONE',  ( 1.033464566929133799, 0.000000000000000000, 1.978346456692913646 ) ) ;
#14720 = AXIS2_PLACEMENT_3D ( 'NONE', #30202, #1857, #16265 ) ;
#14721 = CARTESIAN_POINT ( 'NONE',  ( -0.1264236179284866091, -1.703248031442299304, -0.1264236179284866091 ) ) ;
#14722 = CARTESIAN_POINT ( 'NONE',  ( -0.1264236179284866091, -1.658956692859621995, -0.1264236179284866091 ) ) ;
#14723 = EDGE_CURVE ( 'NONE', #22721, #6712, #42212, .T. ) ;
#14724 = CARTESIAN_POINT ( 'NONE',  ( -0.7495606340400177148, -0.1264236179284866091, 0.5634842519147401640 ) ) ;
#14725 = CARTESIAN_POINT ( 'NONE',  ( -0.1401001227007565297, -0.09842519685039370636, 0.09069709532487360559 ) ) ;
#14726 = CARTESIAN_POINT ( 'NONE',  ( -0.1270800023317771588, -1.452799715094856392, 0.1270800023317771588 ) ) ;
#14727 = CARTESIAN_POINT ( 'NONE',  ( 0.1602931993194444682, -0.1591122789105269553, 0.000000000000000000 ) ) ;
#14728 = VECTOR ( 'NONE', #7586, 39.37007874015748143 ) ;
#14729 = CARTESIAN_POINT ( 'NONE',  ( 0.8019270111902717657, -0.1787899950787401604, 1.274606299158834277 ) ) ;
#14730 = CARTESIAN_POINT ( 'NONE',  ( 0.6971942568897637749, 2.189545951927499583E-17, 1.734744094434425232 ) ) ;
#14731 = DIRECTION ( 'NONE',  ( 1.000000000000000000, 2.114720919224289611E-16, 0.000000000000000000 ) ) ;
#14732 = EDGE_CURVE ( 'NONE', #16491, #13799, #9214, .T. ) ;
#14733 = DIRECTION ( 'NONE',  ( 8.659560562358538199E-17, 0.7071067811862530306, -0.7071067811868418929 ) ) ;
#14734 = LINE ( 'NONE', #37003, #37384 ) ;
#14736 = CARTESIAN_POINT ( 'NONE',  ( 1.033464566929133799, 0.000000000000000000, 0.1574803148531029595 ) ) ;
#14735 = CARTESIAN_POINT ( 'NONE',  ( -0.06523048226347956391, -0.7731299211523151582, -0.1574803149606300301 ) ) ;
#14737 = LINE ( 'NONE', #29408, #26275 ) ;
#14738 = CARTESIAN_POINT ( 'NONE',  ( 0.7017793196824928526, -0.004420539869511170769, 0.03936223978338515561 ) ) ;
#14740 = CARTESIAN_POINT ( 'NONE',  ( 1.033464566929133799, 0.000000000000000000, 0.07874015737278799998 ) ) ;
#14739 = CARTESIAN_POINT ( 'NONE',  ( 0.9500414927467377701, -0.1787899950787401604, 1.274606299158834277 ) ) ;
#14741 = CARTESIAN_POINT ( 'NONE',  ( 0.9873396505805591694, -0.1113553986120547346, 1.225393700787401619 ) ) ;
#14742 = CARTESIAN_POINT ( 'NONE',  ( -0.7185039370078741827, 0.06523048226347841205, 0.9621062991050717272 ) ) ;
#14743 = CARTESIAN_POINT ( 'NONE',  ( -1.002407869896990045, 0.1264236179284866091, 1.247539370024976391 ) ) ;
#14744 = CARTESIAN_POINT ( 'NONE',  ( 0.7646288533564489232, -0.1113553986120547346, 0.6938976376877481478 ) ) ;
#14745 = ORIENTED_EDGE ( 'NONE', *, *, #31742, .F. ) ;
#14746 = CARTESIAN_POINT ( 'NONE',  ( 0.9363197608943458761, 0.1595975290736699748, 0.03936943479083548914 ) ) ;
#14747 = CARTESIAN_POINT ( 'NONE',  ( 0.8107537697050234415, -0.1574803149606297803, 0.2731299212598424231 ) ) ;
#14748 = CARTESIAN_POINT ( 'NONE',  ( -0.4620708661417322616, 0.8070866141732282451, 0.5854071585544579071 ) ) ;
#14749 = CARTESIAN_POINT ( 'NONE',  ( 0.01230737760510397689, 0.07955613945526338049, 0.1377952755905511861 ) ) ;
#14750 = CARTESIAN_POINT ( 'NONE',  ( 1.054774247047244540, 0.07405724077823318263, 1.441929133804504604 ) ) ;
#14751 = PRESENTATION_LAYER_ASSIGNMENT (  '', '', ( #43806 ) ) ;
#14752 = DIRECTION ( 'NONE',  ( 1.000000000000000000, 0.000000000000000000, 0.000000000000000000 ) ) ;
#14753 = CARTESIAN_POINT ( 'NONE',  ( 1.033464566929133799, 0.000000000000000000, 1.190944881889763884 ) ) ;
#14754 = CARTESIAN_POINT ( 'NONE',  ( 0.1787899950787401882, -0.2170275590013547307, -2.189545951927503898E-17 ) ) ;
#14755 = ORIENTED_EDGE ( 'NONE', *, *, #38581, .F. ) ;
#14756 = CARTESIAN_POINT ( 'NONE',  ( -1.033464566929133799, 1.928577636452524610E-17, 2.869337061179095023E-17 ) ) ;
#14757 = AXIS2_PLACEMENT_3D ( 'NONE', #20393, #27633, #9628 ) ;
#14758 = DIRECTION ( 'NONE',  ( 1.000000000000000000, -0.000000000000000000, -0.000000000000000000 ) ) ;
#14759 = CARTESIAN_POINT ( 'NONE',  ( 0.4736248074375433714, 2.559880088878740079, -3.648497683167389649 ) ) ;
#14760 = ORIENTED_EDGE ( 'NONE', *, *, #24214, .F. ) ;
#14761 = CARTESIAN_POINT ( 'NONE',  ( 0.9500414927467378812, -0.1787899950787401604, 0.5708661416785201226 ) ) ;
#14762 = EDGE_LOOP ( 'NONE', ( #31881, #830, #46617, #47123, #42697, #19699, #10699, #45335 ) ) ;
#14763 = CARTESIAN_POINT ( 'NONE',  ( -0.6971942568897637749, 2.189545951927499583E-17, 1.459153543253322693 ) ) ;
#14764 = CARTESIAN_POINT ( 'NONE',  ( 0.1574803149606300301, 0.04379921270595223126, -0.06523048226347956391 ) ) ;
#14765 = CARTESIAN_POINT ( 'NONE',  ( -0.8759842519685039353, 0.1787899950787401882, 1.060531496009228247 ) ) ;
#14766 = ( GEOMETRIC_REPRESENTATION_CONTEXT ( 3 ) GLOBAL_UNCERTAINTY_ASSIGNED_CONTEXT ( ( #32575 ) ) GLOBAL_UNIT_ASSIGNED_CONTEXT ( ( #46283, #42665, #3388 ) ) REPRESENTATION_CONTEXT ( 'NONE', 'WORKASPACE' ) ) ;
#14767 = CIRCLE ( 'NONE', #17040, 0.009842519685039387289 ) ;
#14768 = ORIENTED_EDGE ( 'NONE', *, *, #786, .F. ) ;
#14769 = CARTESIAN_POINT ( 'NONE',  ( -0.9412147342319837628, -0.1574803149606297803, 1.970964566929134021 ) ) ;
#14770 = CARTESIAN_POINT ( 'NONE',  ( -0.6971942568897626646, 0.07405724077823318263, 0.7923228345919055560 ) ) ;
#14771 = EDGE_CURVE ( 'NONE', #34774, #36271, #38593, .T. ) ;
#14772 = CARTESIAN_POINT ( 'NONE',  ( -0.8759842519685039353, -0.1787899950787401882, 0.2140748030958428971 ) ) ;
#14773 = CARTESIAN_POINT ( 'NONE',  ( 0.003457534521343477024, 0.1398629656505299135, -0.03335920195937951138 ) ) ;
#14774 = LINE ( 'NONE', #29438, #9875 ) ;
#14775 = CARTESIAN_POINT ( 'NONE',  ( 0.07405724077823318263, -0.7914625509064031617, 0.1787899950787401604 ) ) ;
#14776 = AXIS2_PLACEMENT_3D ( 'NONE', #33484, #27886, #42447 ) ;
#14777 = ORIENTED_EDGE ( 'NONE', *, *, #41186, .T. ) ;
#14778 = CARTESIAN_POINT ( 'NONE',  ( -1.094772975963752103E-17, 0.1471456693451021758, -0.1787899950787401882 ) ) ;
#14779 = VERTEX_POINT ( 'NONE', #40185 ) ;
#14780 = DIRECTION ( 'NONE',  ( -1.000000000000000000, 0.000000000000000000, 0.000000000000000000 ) ) ;
#14781 = CARTESIAN_POINT ( 'NONE',  ( -1.002407869896990045, -0.1264236179284866091, 0.7652559054580472253 ) ) ;
#14782 = CARTESIAN_POINT ( 'NONE',  ( 0.7185039370078739607, 0.000000000000000000, 4.498031496062992574 ) ) ;
#14783 = ORIENTED_EDGE ( 'NONE', *, *, #45990, .F. ) ;
#14784 = CARTESIAN_POINT ( 'NONE',  ( -0.8759842519685039353, -0.1787899950787401882, 1.867618110182456714 ) ) ;
#14785 = ( BOUNDED_CURVE ( )  B_SPLINE_CURVE ( 2, ( #5599, #31030, #20207, #19739, #16404, #12817, #34375, #2003, #41991 ),
 .UNSPECIFIED., .F., .F. ) 
 B_SPLINE_CURVE_WITH_KNOTS ( ( 3, 2, 2, 2, 3 ),
 ( 0.1000000000000000056, 0.1024999999999999939, 0.1049999999999999961, 0.1074999999999999983, 0.1100000000000000006 ),
 .UNSPECIFIED. ) 
 CURVE ( )  GEOMETRIC_REPRESENTATION_ITEM ( )  RATIONAL_B_SPLINE_CURVE ( ( 1.000000000000000000, 0.9238795325112869605, 1.000000000000000000, 0.9238795325112869605, 1.000000000000000000, 0.9238795325112869605, 1.000000000000000000, 0.9238795325112869605, 1.000000000000000000 ) ) 
 REPRESENTATION_ITEM ( '' )  ) ;
#14786 = B_SPLINE_CURVE_WITH_KNOTS ( 'NONE', 3,
 ( #2041, #10431, #5643, #21186, #38714, #31773, #9949, #28410, #20254, #9720, #24797, #5884, #20491, #46589, #2275, #16901, #35362, #31541, #34901, #27727, #39390, #42289, #24334, #35819, #17601, #27950, #6094, #2966, #32244, #46825, #14013, #28660, #17131, #13539, #42734, #24558, #29857, #32724, #22375, #36538, #43944 ),
 .UNSPECIFIED., .F., .F.,
 ( 4, 1, 1, 1, 1, 1, 1, 2, 2, 1, 1, 1, 1, 2, 2, 2, 1, 1, 1, 1, 2, 2, 1, 1, 1, 1, 1, 2, 2, 4 ),
 ( 0.000000000000000000, 0.1249999999999970579, 0.1874999999999955869, 0.2187499999999950318, 0.2343749999999947820, 0.2421874999999946987, 0.2460937499999945599, 0.2480468749999945044, 0.2499999999999944489, 0.3124999999999964473, 0.3437499999999976685, 0.3593749999999985012, 0.3671874999999988343, 0.3710937499999988343, 0.3749999999999987788, 0.5000000000000011102, 0.5625000000000022204, 0.5937500000000027756, 0.6093750000000029976, 0.6171875000000029976, 0.6210937500000028866, 0.6250000000000027756, 0.6875000000000015543, 0.7187500000000008882, 0.7343750000000005551, 0.7421875000000004441, 0.7460937500000003331, 0.7480468750000002220, 0.7500000000000002220, 1.000000000000000000 ),
 .UNSPECIFIED. ) ;
#14787 = CIRCLE ( 'NONE', #26292, 0.1574803149606300579 ) ;
#14788 = EDGE_CURVE ( 'NONE', #34008, #38222, #29428, .T. ) ;
#14789 = CARTESIAN_POINT ( 'NONE',  ( -0.6971942568897626646, 0.07405724077823318263, 0.04429133852891373180 ) ) ;
#14790 = CARTESIAN_POINT ( 'NONE',  ( 0.8759842519685039353, 0.1574803149606299191, 0.6496062992125984925 ) ) ;
#14791 = CARTESIAN_POINT ( 'NONE',  ( -0.1270800023317771588, -0.9016186127326516475, 0.1270800023317771588 ) ) ;
#14792 = FACE_OUTER_BOUND ( 'NONE', #5492, .T. ) ;
#14793 = CARTESIAN_POINT ( 'NONE',  ( -1.033464566929134687, 0.06523048226347956391, 1.537893700679874298 ) ) ;
#14794 = CARTESIAN_POINT ( 'NONE',  ( 0.6971942568897626646, 0.07405724077823318263, 0.7529527558517473684 ) ) ;
#14795 = PRODUCT_DEFINITION_FORMATION_WITH_SPECIFIED_SOURCE ( 'ANY', '', #5552, .NOT_KNOWN. ) ;
#14796 = CIRCLE ( 'NONE', #41537, 0.3937007874015748254 ) ;
#14797 = CYLINDRICAL_SURFACE ( 'NONE', #22301, 0.1574803149606299191 ) ;
#14798 = EDGE_CURVE ( 'NONE', #26252, #24091, #36620, .T. ) ;
#14799 = CARTESIAN_POINT ( 'NONE',  ( 0.9873396505805591694, 0.1113553986120547346, 1.353346456692913424 ) ) ;
#14800 = FACE_OUTER_BOUND ( 'NONE', #15484, .T. ) ;
#14802 = CARTESIAN_POINT ( 'NONE',  ( 1.033464566929133799, 0.000000000000000000, 0.5216535433070865757 ) ) ;
#14801 = CARTESIAN_POINT ( 'NONE',  ( 0.9373987626270909868, -0.1654231709439420162, 1.989299970918606331 ) ) ;
#14803 = CARTESIAN_POINT ( 'NONE',  ( 1.033464566929133799, 0.000000000000000000, 1.732283464459401623 ) ) ;
#14804 = CLOSED_SHELL ( 'NONE', ( #31070, #18070, #45753, #6493, #9047, #14409, #42647, #19306, #16260, #45323, #7568, #24097, #26805, #5977, #31234, #16585, #35710, #1848, #42716, #25765, #41567, #28656 ) ) ;
#14805 = CARTESIAN_POINT ( 'NONE',  ( -1.002407869896990045, -0.1264236179284866091, 1.985728346402929168 ) ) ;
#14806 = CARTESIAN_POINT ( 'NONE',  ( -0.07405724077823318263, -0.7805118109698575557, 0.1787899950787401604 ) ) ;
#14807 = LINE ( 'NONE', #46663, #2322 ) ;
#14808 = DIRECTION ( 'NONE',  ( 1.000000000000000000, -0.000000000000000000, -0.000000000000000000 ) ) ;
#14809 = CARTESIAN_POINT ( 'NONE',  ( 0.7495606340400177148, 0.1264236179284866091, 1.021161417269070837 ) ) ;
#14810 = CARTESIAN_POINT ( 'NONE',  ( 0.2204724409448818867, 1.205361022782826802E-17, -0.09842519685039370636 ) ) ;
#14811 = CARTESIAN_POINT ( 'NONE',  ( -0.1574803149606299191, -1.720472440944881942, 0.000000000000000000 ) ) ;
#14812 = B_SPLINE_CURVE_WITH_KNOTS ( 'NONE', 3,
 ( #33786, #902, #15563, #8340, #32307 ),
 .UNSPECIFIED., .F., .F.,
 ( 4, 1, 4 ),
 ( 0.000000000000000000, 0.002020725942163689639, 0.004041451884327384482 ),
 .UNSPECIFIED. ) ;
#14813 = VERTEX_POINT ( 'NONE', #3779 ) ;
#14814 = DIRECTION ( 'NONE',  ( -1.000000000000000000, 0.000000000000000000, 0.000000000000000000 ) ) ;
#14815 = CARTESIAN_POINT ( 'NONE',  ( -0.8759842519685039353, 0.1787899950787401882, 0.1500984251430870220 ) ) ;
#14816 = ORIENTED_EDGE ( 'NONE', *, *, #36498, .F. ) ;
#14817 = CARTESIAN_POINT ( 'NONE',  ( 0.2204724409448818867, 0.000000000000000000, 0.09842519685039370636 ) ) ;
#14818 = CARTESIAN_POINT ( 'NONE',  ( -1.054774247047244540, -0.07405724077823318263, 1.712598425143087688 ) ) ;
#14819 = CARTESIAN_POINT ( 'NONE',  ( -0.6971942568897637749, 2.189545951927499583E-17, 0.3223425196312759144 ) ) ;
#14820 = CARTESIAN_POINT ( 'NONE',  ( -0.8759842519685039353, -0.1574803149606299191, 0.1082677164279060994 ) ) ;
#14821 = CARTESIAN_POINT ( 'NONE',  ( 0.9412147342319837628, 0.1574803149606300301, 0.4010826770578274081 ) ) ;
#14822 = CARTESIAN_POINT ( 'NONE',  ( 0.8759842519685039353, 0.000000000000000000, 4.498031496062992574 ) ) ;
#14823 = CARTESIAN_POINT ( 'NONE',  ( 1.054774247047244096, 0.000000000000000000, 0.06151574797773248782 ) ) ;
#14824 = CARTESIAN_POINT ( 'NONE',  ( 1.614954907737318939E-16, 0.1574803149606340824, 0.3937007874015748254 ) ) ;
#14825 = CARTESIAN_POINT ( 'NONE',  ( -1.094772975963752103E-17, -0.4592775115363252336, -0.1787899950787401882 ) ) ;
#14826 = CARTESIAN_POINT ( 'NONE',  ( -0.2128335240989271959, -0.08955970507752815390, -0.1176384946248013735 ) ) ;
#14827 = CARTESIAN_POINT ( 'NONE',  ( 0.3547871005709968273, 1.205361022782824954E-17, -0.09842519685039370636 ) ) ;
#14828 = FACE_OUTER_BOUND ( 'NONE', #20789, .T. ) ;
#14829 = AXIS2_PLACEMENT_3D ( 'NONE', #21068, #39511, #35248 ) ;
#14830 = CARTESIAN_POINT ( 'NONE',  ( -0.7495606340400177148, 0.1264236179284866091, 0.2731299212060791515 ) ) ;
#14831 = VERTEX_POINT ( 'NONE', #14817 ) ;
#14832 = AXIS2_PLACEMENT_3D ( 'NONE', #3861, #14902, #7927 ) ;
#14833 = EDGE_CURVE ( 'NONE', #39969, #46991, #17736, .T. ) ;
#14834 = CARTESIAN_POINT ( 'NONE',  ( -0.7495606340400177148, 0.1264236179284866091, 1.341043307032850462 ) ) ;
#14835 = ORIENTED_EDGE ( 'NONE', *, *, #24269, .T. ) ;
#14836 = CARTESIAN_POINT ( 'NONE',  ( 0.1264236179284866091, -1.398129921206078707, -0.1264236179284866091 ) ) ;
#14837 = CARTESIAN_POINT ( 'NONE',  ( -1.094772975963752103E-17, -1.348917322780881944, -0.1787899950787401882 ) ) ;
#14838 = ADVANCED_FACE ( 'NONE', ( #44718 ), #9697, .T. ) ;
#14839 = DIRECTION ( 'NONE',  ( 0.000000000000000000, 0.000000000000000000, -1.000000000000000000 ) ) ;
#14840 = DIRECTION ( 'NONE',  ( 0.000000000000000000, 0.000000000000000000, 1.000000000000000000 ) ) ;
#14841 = CARTESIAN_POINT ( 'NONE',  ( 0.8107537697050253289, -0.1574803149606297803, 0.3912401574803148763 ) ) ;
#14842 = CARTESIAN_POINT ( 'NONE',  ( 0.1270800023317771588, -0.6063430221814705146, -0.1270800023317771588 ) ) ;
#14843 = DIRECTION ( 'NONE',  ( 3.469446951953615767E-15, 1.000000000000000000, 0.000000000000000000 ) ) ;
#14844 = CARTESIAN_POINT ( 'NONE',  ( -0.8107537697050253289, 0.1574803149606300301, 1.075295275483024504 ) ) ;
#14845 = CARTESIAN_POINT ( 'NONE',  ( 0.6971942568897626646, 0.07405724077823318263, 0.4379921259304882519 ) ) ;
#14846 = CARTESIAN_POINT ( 'NONE',  ( -1.284448818897637956, -0.3937007874015748254, 1.181102362204724310 ) ) ;
#14847 = CARTESIAN_POINT ( 'NONE',  ( -0.1574803149606297803, -0.3400590551181101318, 0.06523048226347956391 ) ) ;
#14848 = ORIENTED_EDGE ( 'NONE', *, *, #19906, .T. ) ;
#14849 = CARTESIAN_POINT ( 'NONE',  ( 1.033464566929134687, -0.06523048226347956391, 1.926673228238929170 ) ) ;
#14850 = VERTEX_POINT ( 'NONE', #22940 ) ;
#14851 = VECTOR ( 'NONE', #11977, 39.37007874015748143 ) ;
#14852 = CARTESIAN_POINT ( 'NONE',  ( -0.9412147342319837628, 0.1574803149606300301, 1.424704724301921521 ) ) ;
#14853 = CARTESIAN_POINT ( 'NONE',  ( 0.9412147342319837628, 0.1574803149606300301, 0.9227362204724416372 ) ) ;
#14854 = LINE ( 'NONE', #11262, #37345 ) ;
#14855 = PRODUCT_DEFINITION ( 'UNKNOWN', '', #32422, #22108 ) ;
#14857 = CARTESIAN_POINT ( 'NONE',  ( -1.033464566929133799, 1.928577636452524610E-17, 2.869337061179095023E-17 ) ) ;
#14856 = CYLINDRICAL_SURFACE ( 'NONE', #26356, 0.1574803149606299191 ) ;
#14858 = DIRECTION ( 'NONE',  ( 0.000000000000000000, -0.9699617890481199156, -0.2432573283306598000 ) ) ;
#14859 = CIRCLE ( 'NONE', #39323, 0.09842519685039370636 ) ;
#14860 = ORIENTED_EDGE ( 'NONE', *, *, #2783, .T. ) ;
#14861 = CARTESIAN_POINT ( 'NONE',  ( -0.1113553986120547346, 0.09547244105240886014, -0.1113553986120547346 ) ) ;
#14862 = CARTESIAN_POINT ( 'NONE',  ( 1.033464566929133799, 0.000000000000000000, 1.387795275590551158 ) ) ;
#14863 = CARTESIAN_POINT ( 'NONE',  ( -0.1264236179284866091, -1.580216535379306952, -0.1264236179284866091 ) ) ;
#14864 = CARTESIAN_POINT ( 'NONE',  ( -0.1113553986120547346, -1.518700787294047005, -0.1113553986120547346 ) ) ;
#14865 = CARTESIAN_POINT ( 'NONE',  ( -0.1787899950787401604, -0.7903543306548983516, 0.07405724077823318263 ) ) ;
#14866 = CARTESIAN_POINT ( 'NONE',  ( 2.892866454678787531E-17, -1.080708661417322913, 0.1574803149606299191 ) ) ;
#14867 = CARTESIAN_POINT ( 'NONE',  ( 0.8107537697050253289, 0.1574803149606300301, 0.9965551180027087952 ) ) ;
#14868 = CARTESIAN_POINT ( 'NONE',  ( 0.000000000000000000, 0.000000000000000000, -0.2495040853978291451 ) ) ;
#14869 = ORIENTED_EDGE ( 'NONE', *, *, #10423, .F. ) ;
#14870 = ORIENTED_EDGE ( 'NONE', *, *, #27350, .T. ) ;
#14871 = VERTEX_POINT ( 'NONE', #24311 ) ;
#14872 = VECTOR ( 'NONE', #46942, 39.37007874015748143 ) ;
#14873 = CARTESIAN_POINT ( 'NONE',  ( -0.7495606340400177148, -0.1264236179284866091, 1.547736220418677089 ) ) ;
#14874 = CARTESIAN_POINT ( 'NONE',  ( 1.054774247047244096, 0.000000000000000000, 1.759350393647023614 ) ) ;
#14875 = CARTESIAN_POINT ( 'NONE',  ( -0.6971942568897637749, 2.189545951927499583E-17, 0.8735236219934803259 ) ) ;
#14876 = DIRECTION ( 'NONE',  ( 0.000000000000000000, 0.000000000000000000, -1.000000000000000000 ) ) ;
#14877 = CARTESIAN_POINT ( 'NONE',  ( 1.002407869896990045, -0.1264236179284866091, 0.2583661416785200671 ) ) ;
#14878 = CARTESIAN_POINT ( 'NONE',  ( -0.7185039370078739607, 1.928577636452523993E-17, 0.2657480314960630197 ) ) ;
#14879 = CARTESIAN_POINT ( 'NONE',  ( -0.8759842519685039353, -0.1787899950787401882, 1.232775590497417362 ) ) ;
#14880 = CARTESIAN_POINT ( 'NONE',  ( -0.8019270111902716547, 0.1787899950787401604, 0.7037401574265510495 ) ) ;
#14881 = CARTESIAN_POINT ( 'NONE',  ( -0.1377952755905511861, 0.1574803149606320007, 0.9084645669291337988 ) ) ;
#14882 = CARTESIAN_POINT ( 'NONE',  ( 0.1179171413540825442, 0.09842519685039370636, 0.2173535775632911005 ) ) ;
#14883 = CARTESIAN_POINT ( 'NONE',  ( -0.6971942568897648851, -0.07405724077823297447, 1.505905511757261284 ) ) ;
#14884 = CARTESIAN_POINT ( 'NONE',  ( -0.7185039370078739607, 1.928577636452523993E-17, 1.870078740049952559 ) ) ;
#14885 = ORIENTED_EDGE ( 'NONE', *, *, #33957, .T. ) ;
#14886 = CARTESIAN_POINT ( 'NONE',  ( -0.7646288533564489232, -0.1113553986120547346, 1.569881889763779625 ) ) ;
#14887 = CARTESIAN_POINT ( 'NONE',  ( 0.1574803149606299746, -0.4410959923581754816, -0.9673892061308019263 ) ) ;
#14888 = CARTESIAN_POINT ( 'NONE',  ( 0.9500414927467377701, -0.1787899950787401604, 1.476377952702141449 ) ) ;
#14889 = CARTESIAN_POINT ( 'NONE',  ( -0.9412147342319837628, -0.1574803149606297803, 1.577263779527559917 ) ) ;
#14890 = EDGE_CURVE ( 'NONE', #27963, #45437, #37464, .T. ) ;
#14891 = VERTEX_POINT ( 'NONE', #27464 ) ;
#14892 = ADVANCED_FACE ( 'NONE', ( #20226 ), #16651, .T. ) ;
#14893 = ORIENTED_EDGE ( 'NONE', *, *, #22956, .F. ) ;
#14894 = AXIS2_PLACEMENT_3D ( 'NONE', #10958, #36364, #47119 ) ;
#14895 = EDGE_CURVE ( 'NONE', #46399, #37690, #6308, .T. ) ;
#14896 = ORIENTED_EDGE ( 'NONE', *, *, #11013, .F. ) ;
#14897 = CIRCLE ( 'NONE', #11848, 0.7874015748031437667 ) ;
#14898 = VECTOR ( 'NONE', #40221, 39.37007874015748143 ) ;
#14899 = CARTESIAN_POINT ( 'NONE',  ( -0.7185039370078739607, 1.928577636452523993E-17, 1.131889763779527547 ) ) ;
#14900 = CARTESIAN_POINT ( 'NONE',  ( -0.07405724077823318263, -0.3917322834108032947, 0.1787899950787401604 ) ) ;
#14901 = CARTESIAN_POINT ( 'NONE',  ( -0.1264236179284866091, -0.9109251967966299768, -0.1264236179284866091 ) ) ;
#14902 = DIRECTION ( 'NONE',  ( 0.000000000000000000, 0.000000000000000000, 1.000000000000000000 ) ) ;
#14903 = ( CONVERSION_BASED_UNIT ( 'INCH', #25920 ) LENGTH_UNIT ( ) NAMED_UNIT ( #16697 ) ) ;
#14904 = CARTESIAN_POINT ( 'NONE',  ( 0.7495606340400177148, 0.1264236179284866091, 1.808562992072220377 ) ) ;
#14905 = CLOSED_SHELL ( 'NONE', ( #33615, #13922, #10071, #4201, #15721, #35465, #34519, #13377, #40384, #39122, #42178, #17365, #14610, #23948, #43223, #18007, #22947, #35019, #42758, #2585, #31351, #24312, #25352, #30250, #42349, #24315, #25675, #4349, #839, #21593, #36484, #19761, #5302, #36719, #31933, #19807, #18602, #15115, #6098, #38307, #7446, #14892, #40453, #15165, #11822, #23753, #28944, #6703, #2065, #1184, #24951, #11435, #22190, #41607, #23990, #23507, #30061, #31618, #632, #42563, #5567, #10141, #19475, #23811, #16464, #26039, #5992, #2737, #28710, #26277 ) ) ;
#14906 = CARTESIAN_POINT ( 'NONE',  ( -0.07444174185955065859, -0.2692367229688725216, 0.1797182628040039087 ) ) ;
#14907 = CARTESIAN_POINT ( 'NONE',  ( -0.07405724077823318263, -0.03740157474938609478, 0.1787899950787401604 ) ) ;
#14908 = CARTESIAN_POINT ( 'NONE',  ( 0.2471922904502827090, -0.09842519685039370636, -0.01321092903673363843 ) ) ;
#14909 = CARTESIAN_POINT ( 'NONE',  ( 1.054774247047244540, 0.07405724077823318263, 0.7332677164816707727 ) ) ;
#14910 = LINE ( 'NONE', #29572, #3984 ) ;
#14911 = DIRECTION ( 'NONE',  ( 0.000000000000000000, -0.7880107536067207930, 0.6156614753256598460 ) ) ;
#14912 = CARTESIAN_POINT ( 'NONE',  ( 1.033464566929134687, 0.06523048226347956391, 0.9473425195775121432 ) ) ;
#14913 = CARTESIAN_POINT ( 'NONE',  ( 1.054774247047244540, 0.07405724077823318263, 1.801181102308441861 ) ) ;
#14915 = CARTESIAN_POINT ( 'NONE',  ( 0.4755220087074803481, 4.766607801171850497E-17, 0.000000000000000000 ) ) ;
#14914 = DIRECTION ( 'NONE',  ( 1.000000000000000000, -3.469446951953625233E-15, -0.000000000000000000 ) ) ;
#14916 = CARTESIAN_POINT ( 'NONE',  ( 0.6971942568897648851, -0.07405724077823297447, 0.5167322834108035723 ) ) ;
#14917 = EDGE_LOOP ( 'NONE', ( #28213, #4260, #34643, #12358 ) ) ;
#14918 = CARTESIAN_POINT ( 'NONE',  ( 0.8759842519685039353, 0.1574803149606299191, 0.09842519685039370636 ) ) ;
#14919 = CARTESIAN_POINT ( 'NONE',  ( 0.1637370714319410780, -0.07819377357278597951, 0.1401549625175002034 ) ) ;
#14921 = CARTESIAN_POINT ( 'NONE',  ( 0.1264236179284866091, -0.2563976377415121966, -0.1264236179284866091 ) ) ;
#14920 = CARTESIAN_POINT ( 'NONE',  ( 0.06523048226347956391, -0.9502952754830243931, 0.1574803149606297803 ) ) ;
#14923 = CARTESIAN_POINT ( 'NONE',  ( 0.1583858528204730998, 0.1020630898162672995, 0.1041062675987153296 ) ) ;
#14922 = CARTESIAN_POINT ( 'NONE',  ( -0.7495606340400177148, -0.1264236179284866091, 0.4847440944344252323 ) ) ;
#14924 = CARTESIAN_POINT ( 'NONE',  ( -0.07405724077823318263, -1.056102362150961982, 0.1787899950787401604 ) ) ;
#14925 = CARTESIAN_POINT ( 'NONE',  ( 0.8019270111902717657, -0.1787899950787401604, 0.2509842519147403861 ) ) ;
#14926 = CARTESIAN_POINT ( 'NONE',  ( 0.1631287816250558131, 0.08016185997947827824, -0.1388454444657191700 ) ) ;
#14927 = CARTESIAN_POINT ( 'NONE',  ( -0.6971942568897648851, -0.07405724077823297447, 1.540354330654897685 ) ) ;
#14928 = EDGE_LOOP ( 'NONE', ( #25651, #18758, #18437 ) ) ;
#14929 = CONICAL_SURFACE ( 'NONE', #8032, 0.2559055118110236116, 0.7853981633974518317 ) ;
#14930 = CARTESIAN_POINT ( 'NONE',  ( -0.7495606340400177148, 0.1264236179284866091, 1.222933070812378009 ) ) ;
#14931 = CARTESIAN_POINT ( 'NONE',  ( -1.033464566929133799, 0.000000000000000000, 0.8759842519685039353 ) ) ;
#14932 = CARTESIAN_POINT ( 'NONE',  ( 0.8759842519685039353, 0.1787899950787401882, 1.257381889710015743 ) ) ;
#14933 = AXIS2_PLACEMENT_3D ( 'NONE', #30644, #23436, #9290 ) ;
#14934 = CARTESIAN_POINT ( 'NONE',  ( 0.1574803149606299191, -1.179133858160189119, -1.928577636452523993E-17 ) ) ;
#14935 = CARTESIAN_POINT ( 'NONE',  ( 0.7495606340400177148, -0.1264236179284866091, 0.05167322829269323931 ) ) ;
#14936 = CARTESIAN_POINT ( 'NONE',  ( -0.9500414927467378812, -0.1787899950787401604, 0.9990157479777320715 ) ) ;
#14937 = CARTESIAN_POINT ( 'NONE',  ( 0.000000000000000000, 0.000000000000000000, -0.06545654452343109553 ) ) ;
#14938 = CARTESIAN_POINT ( 'NONE',  ( -0.1889095778403545312, -0.1864272366437806083, -0.04769437235514253220 ) ) ;
#14939 = CARTESIAN_POINT ( 'NONE',  ( 0.6971942568897637749, 2.189545951927499583E-17, 0.2436023621509610382 ) ) ;
#14940 = CARTESIAN_POINT ( 'NONE',  ( -1.054774247047244540, -0.07405724077823318263, 0.2165354330171024577 ) ) ;
#14941 = CARTESIAN_POINT ( 'NONE',  ( -0.8019270111902717657, -0.1787899950787401604, 0.6791338582139527791 ) ) ;
#14942 = CARTESIAN_POINT ( 'NONE',  ( 1.033464566929133799, 0.000000000000000000, 1.692913385719244213 ) ) ;
#14943 = ORIENTED_EDGE ( 'NONE', *, *, #21420, .T. ) ;
#14944 = CARTESIAN_POINT ( 'NONE',  ( 0.1264236179284866091, -0.02017716530056720692, -0.1264236179284866091 ) ) ;
#14945 = ORIENTED_EDGE ( 'NONE', *, *, #35872, .F. ) ;
#14946 = CARTESIAN_POINT ( 'NONE',  ( 0.8759842519685039353, 0.1787899950787401882, 1.099901574749385880 ) ) ;
#14947 = CARTESIAN_POINT ( 'NONE',  ( -1.002407869896990045, 0.1264236179284866091, 1.838090551127338657 ) ) ;
#14948 = ORIENTED_EDGE ( 'NONE', *, *, #18881, .T. ) ;
#14949 = EDGE_CURVE ( 'NONE', #46224, #24436, #18354, .T. ) ;
#14950 = CARTESIAN_POINT ( 'NONE',  ( 0.9500414927467378812, 0.1787899950787401604, 1.958661417269071947 ) ) ;
#14951 = EDGE_CURVE ( 'NONE', #9031, #39913, #38998, .T. ) ;
#14952 = DIRECTION ( 'NONE',  ( 0.000000000000000000, 0.000000000000000000, 1.000000000000000000 ) ) ;
#14953 = CARTESIAN_POINT ( 'NONE',  ( 0.1787899950787401604, -1.416462550906403939, 0.07405724077823318263 ) ) ;
#14954 = EDGE_LOOP ( 'NONE', ( #16872, #9471, #6621, #15891 ) ) ;
#14955 = CARTESIAN_POINT ( 'NONE',  ( -0.1264236179284866091, -0.2711614172690712810, 0.1264236179284866091 ) ) ;
#14956 = EDGE_CURVE ( 'NONE', #12585, #22114, #28152, .T. ) ;
#14957 = CARTESIAN_POINT ( 'NONE',  ( -0.1113553986120547346, 0.02657480325713335034, 0.1113553986120547346 ) ) ;
#14958 = ORIENTED_EDGE ( 'NONE', *, *, #45634, .F. ) ;
#14959 = CARTESIAN_POINT ( 'NONE',  ( 0.8759842519685039353, -0.1787899950787401882, 1.272145669237574772 ) ) ;
#14960 = VECTOR ( 'NONE', #26368, 39.37007874015748143 ) ;
#14961 = EDGE_CURVE ( 'NONE', #40610, #12359, #42801, .T. ) ;
#14962 = DIRECTION ( 'NONE',  ( 0.000000000000000000, 0.000000000000000000, 1.000000000000000000 ) ) ;
#14963 = CARTESIAN_POINT ( 'NONE',  ( -0.1377952755905511861, 0.1564960629921283985, 0.8070866141732283561 ) ) ;
#14964 = ( BOUNDED_CURVE ( )  B_SPLINE_CURVE ( 2, ( #21287, #3069, #17699, #6904, #21526, #36164, #3318, #47172, #29003 ),
 .UNSPECIFIED., .F., .F. ) 
 B_SPLINE_CURVE_WITH_KNOTS ( ( 3, 2, 2, 2, 3 ),
 ( 0.7399999999999999911, 0.7425000000000000488, 0.7449999999999999956, 0.7475000000000000533, 0.7500000000000000000 ),
 .UNSPECIFIED. ) 
 CURVE ( )  GEOMETRIC_REPRESENTATION_ITEM ( )  RATIONAL_B_SPLINE_CURVE ( ( 1.000000000000000000, 0.9238795325112869605, 1.000000000000000000, 0.9238795325112869605, 1.000000000000000000, 0.9238795325112869605, 1.000000000000000000, 0.9238795325112869605, 1.000000000000000000 ) ) 
 REPRESENTATION_ITEM ( '' )  ) ;
#14965 = CARTESIAN_POINT ( 'NONE',  ( 0.6971942568897626646, -0.07405724077823297447, 0.2017716534895435399 ) ) ;
#14966 = AXIS2_PLACEMENT_3D ( 'NONE', #16021, #5199, #44967 ) ;
#14967 = VECTOR ( 'NONE', #39723, 39.37007874015748143 ) ;
#14968 = CONICAL_SURFACE ( 'NONE', #15762, 0.1377952755905509641, 0.9599310885968941331 ) ;
#14969 = VECTOR ( 'NONE', #38807, 39.37007874015748143 ) ;
#14970 = CARTESIAN_POINT ( 'NONE',  ( -0.1787899950787401604, -1.582677165300567346, -0.07405724077823318263 ) ) ;
#14971 = CARTESIAN_POINT ( 'NONE',  ( 0.1264236179284866091, -1.718011810969858333, 0.1264236179284866091 ) ) ;
#14972 = CARTESIAN_POINT ( 'NONE',  ( -1.054774247047244540, 0.07405724077823318263, 0.4625984251430869665 ) ) ;
#14973 = CARTESIAN_POINT ( 'NONE',  ( 0.2362204724409449064, 0.3740157480314960647, 0.9783464566929134243 ) ) ;
#14975 = CARTESIAN_POINT ( 'NONE',  ( -0.7115070055584155062, -0.02845177017965971542, 1.983791088683289017 ) ) ;
#14974 = CARTESIAN_POINT ( 'NONE',  ( 0.07444174185955065859, -1.406047746590921133, 0.1797182628040039087 ) ) ;
#14976 = CARTESIAN_POINT ( 'NONE',  ( 0.7185039370078746268, 0.06523048226347956391, 1.444389763779527991 ) ) ;
#14977 = CARTESIAN_POINT ( 'NONE',  ( 0.6971942568897648851, -0.07405724077823297447, 1.427165354276944687 ) ) ;
#14978 = CARTESIAN_POINT ( 'NONE',  ( 0.8759842519685039353, -0.1787899950787401882, 1.626476377898992132 ) ) ;
#14979 = CARTESIAN_POINT ( 'NONE',  ( 0.7185039370078739607, 1.928577636452523993E-17, 1.515748031388535200 ) ) ;
#14980 = CARTESIAN_POINT ( 'NONE',  ( 0.06841996760812382727, 0.1299212598425196763, 0.1651804176431311000 ) ) ;
#14981 = LINE ( 'NONE', #36543, #29810 ) ;
#14983 = DIRECTION ( 'NONE',  ( -1.000000000000000000, 0.000000000000000000, 0.000000000000000000 ) ) ;
#14982 = CARTESIAN_POINT ( 'NONE',  ( 0.1574803149606300301, -0.8223425195775115881, -0.06523048226347956391 ) ) ;
#14984 = CARTESIAN_POINT ( 'NONE',  ( 1.033464566929134687, -0.06523048226347956391, 0.5487204723334181411 ) ) ;
#14985 = CARTESIAN_POINT ( 'NONE',  ( 0.8759842519685039353, -0.1787899950787401882, 0.2878937007336381804 ) ) ;
#14986 = CARTESIAN_POINT ( 'NONE',  ( 0.7233020866430639462, -0.07417860294387490505, 0.03937367257947978899 ) ) ;
#14988 = DIRECTION ( 'NONE',  ( 1.822029033848725028E-16, 0.000000000000000000, 1.000000000000000000 ) ) ;
#14987 = CARTESIAN_POINT ( 'NONE',  ( 0.8759842519685039353, -0.1787899950787401882, 1.272145669237574772 ) ) ;
#14989 = DIRECTION ( 'NONE',  ( -1.000000000000000000, 0.000000000000000000, 0.000000000000000000 ) ) ;
#14990 = CARTESIAN_POINT ( 'NONE',  ( -0.7185039370078746268, 0.06523048226347956391, 0.7750984251968497940 ) ) ;
#14991 = CARTESIAN_POINT ( 'NONE',  ( -0.8019270111902717657, -0.1787899950787401604, 1.269685039316314601 ) ) ;
#14992 = CARTESIAN_POINT ( 'NONE',  ( 0.7185039370078746268, 0.06523048226347956391, 0.6865157479239701876 ) ) ;
#14993 = ORIENTED_EDGE ( 'NONE', *, *, #26981, .T. ) ;
#14994 = LINE ( 'NONE', #15465, #39844 ) ;
#14995 = CARTESIAN_POINT ( 'NONE',  ( 0.9412147342319837628, 0.1574803149606300301, 0.6865157480314956207 ) ) ;
#14996 = ORIENTED_EDGE ( 'NONE', *, *, #2487, .F. ) ;
#14997 = CARTESIAN_POINT ( 'NONE',  ( 1.033464566929134687, 0.06523048226347956391, 0.2878937007874017295 ) ) ;
#14998 = CARTESIAN_POINT ( 'NONE',  ( -0.1270800023317771588, 0.1220034345114427293, 0.1270800023317771588 ) ) ;
#14999 = PRODUCT_DEFINITION_SHAPE ( 'NONE', 'NONE',  #6390 ) ;
#15000 = CARTESIAN_POINT ( 'NONE',  ( -0.9873396505805591694, 0.1113553986120547346, 1.589566929133858331 ) ) ;
#15001 = CARTESIAN_POINT ( 'NONE',  ( 0.6971942568897648851, -0.07405724077823297447, 1.579724409395055318 ) ) ;
#15002 = AXIS2_PLACEMENT_3D ( 'NONE', #3548, #21758, #21990 ) ;
#15003 = CARTESIAN_POINT ( 'NONE',  ( -0.9412147342319837628, -0.1574803149606297803, 1.094980314853103653 ) ) ;
#15005 = CARTESIAN_POINT ( 'NONE',  ( -0.9412147342319837628, -0.1574803149606297803, 0.1205708661417322358 ) ) ;
#15004 = CARTESIAN_POINT ( 'NONE',  ( 0.1631207519397639694, -0.08463291909044137751, 0.1344936127548389537 ) ) ;
#15006 = CARTESIAN_POINT ( 'NONE',  ( -0.07405724077823318263, -0.2293307086076536994, 0.1787899950787401604 ) ) ;
#15007 = ORIENTED_EDGE ( 'NONE', *, *, #586, .F. ) ;
#15008 = FACE_OUTER_BOUND ( 'NONE', #25978, .T. ) ;
#15009 = CARTESIAN_POINT ( 'NONE',  ( 0.2275913475568078770, -0.05179116514251743547, -0.1540331450889871889 ) ) ;
#15010 = CARTESIAN_POINT ( 'NONE',  ( 1.054774247047244540, 0.07405724077823318263, 0.5807086613635594752 ) ) ;
#15011 = EDGE_LOOP ( 'NONE', ( #38695, #19381, #8892, #42251 ) ) ;
#15012 = CARTESIAN_POINT ( 'NONE',  ( 0.9500414927467377701, -0.1787899950787401604, 0.8070866141194653620 ) ) ;
#15013 = CARTESIAN_POINT ( 'NONE',  ( -1.002407869896990045, 0.1264236179284866091, 1.444389763725763665 ) ) ;
#15014 = CARTESIAN_POINT ( 'NONE',  ( 0.1574803149606300301, 0.08316929144610965552, -0.06523048226347956391 ) ) ;
#15015 = CARTESIAN_POINT ( 'NONE',  ( -1.054774247047244096, 0.000000000000000000, 1.247539370024976391 ) ) ;
#15016 = CIRCLE ( 'NONE', #19566, 0.2114570894355444486 ) ;
#15017 = CIRCLE ( 'NONE', #428, 0.009842519685039399432 ) ;
#15018 = VERTEX_POINT ( 'NONE', #9466 ) ;
#15019 = EDGE_CURVE ( 'NONE', #38566, #26779, #14394, .T. ) ;
#15020 = CARTESIAN_POINT ( 'NONE',  ( -0.9500414927467378812, -0.1787899950787401604, 0.2559055117572600624 ) ) ;
#15021 = CARTESIAN_POINT ( 'NONE',  ( 0.008625679036625592128, 0.1524122562642153123, -0.01160289892401995641 ) ) ;
#15022 = CARTESIAN_POINT ( 'NONE',  ( 0.1787899950787401604, -0.9046515272843580480, 0.07405724077823318263 ) ) ;
#15023 = EDGE_LOOP ( 'NONE', ( #12941, #41951, #4898, #37019 ) ) ;
#15024 = CARTESIAN_POINT ( 'NONE',  ( 0.7521669337840648506, 0.1290358749737920141, 0.03937007777616036847 ) ) ;
#15025 = VERTEX_POINT ( 'NONE', #37434 ) ;
#15026 = ADVANCED_FACE ( 'NONE', ( #4831 ), #22587, .T. ) ;
#15027 = CARTESIAN_POINT ( 'NONE',  ( -0.7646288533564489232, -0.1113553986120547346, 0.2608267715460161340 ) ) ;
#15028 = CARTESIAN_POINT ( 'NONE',  ( -0.8019270111902717657, -0.1787899950787401604, 0.7578740156942689321 ) ) ;
#15029 = PLANE ( 'NONE',  #12379 ) ;
#15030 = ORIENTED_EDGE ( 'NONE', *, *, #2845, .T. ) ;
#15031 = CARTESIAN_POINT ( 'NONE',  ( -0.6971942568897648851, -0.07405724077823297447, 1.820866141678520789 ) ) ;
#15032 = CIRCLE ( 'NONE', #34163, 0.7874015748031496509 ) ;
#15033 = CARTESIAN_POINT ( 'NONE',  ( -0.07405724077823318263, -0.4852362204186770889, -0.1787899950787401604 ) ) ;
#15034 = CARTESIAN_POINT ( 'NONE',  ( -0.7646288533564489232, 0.1113553986120547346, 0.9301181102362204856 ) ) ;
#15035 = CARTESIAN_POINT ( 'NONE',  ( 0.1270800023317771588, -0.9606737308428878741, -0.1270800023317771588 ) ) ;
#15036 = DIRECTION ( 'NONE',  ( 0.000000000000000000, 1.000000000000000000, 0.000000000000000000 ) ) ;
#15037 = CARTESIAN_POINT ( 'NONE',  ( -0.7185039370078746268, 0.06523048226347956391, 1.473917322727117840 ) ) ;
#15038 = CARTESIAN_POINT ( 'NONE',  ( 1.054774247047244096, 0.000000000000000000, 0.6963582676627716461 ) ) ;
#15039 = AXIS2_PLACEMENT_3D ( 'NONE', #32822, #10778, #25851 ) ;
#15040 = CARTESIAN_POINT ( 'NONE',  ( 1.033464566929133799, 0.000000000000000000, 1.348425196850393748 ) ) ;
#15042 = CARTESIAN_POINT ( 'NONE',  ( 0.9873396505805591694, -0.1113553986120547346, 1.569881889656251861 ) ) ;
#15041 = CARTESIAN_POINT ( 'NONE',  ( 0.7291528398006205114, 0.07205607647759287859, 1.981831347760247164 ) ) ;
#15043 = DIRECTION ( 'NONE',  ( 1.776356839400250070E-15, 0.000000000000000000, 1.000000000000000000 ) ) ;
#15044 = EDGE_CURVE ( 'NONE', #32278, #10690, #34290, .T. ) ;
#15046 = CARTESIAN_POINT ( 'NONE',  ( 0.1559665883013474363, 0.09131739707178464227, 0.1174241798378301144 ) ) ;
#15045 = CARTESIAN_POINT ( 'NONE',  ( 0.8759842519685039353, -0.1787899950787401882, 0.8390748030958424808 ) ) ;
#15047 = CARTESIAN_POINT ( 'NONE',  ( -0.07405724077823318263, -0.7165354330171036512, -0.1787899950787401604 ) ) ;
#15048 = ORIENTED_EDGE ( 'NONE', *, *, #30836, .F. ) ;
#15049 = CARTESIAN_POINT ( 'NONE',  ( 1.033464566929133799, 0.000000000000000000, 1.072834645669291431 ) ) ;
#15050 = CARTESIAN_POINT ( 'NONE',  ( -0.4338976377952755703, -2.656856766417909227E-17, 0.000000000000000000 ) ) ;
#15051 = CARTESIAN_POINT ( 'NONE',  ( 0.9500414927467378812, 0.1787899950787401604, 1.092519684985605810 ) ) ;
#15052 = APPLICATION_CONTEXT ( 'automotive_design' ) ;
#15053 = FACE_OUTER_BOUND ( 'NONE', #2944, .T. ) ;
#15054 = CARTESIAN_POINT ( 'NONE',  ( 0.06523048226347956391, -1.732775590551180134, -0.1574803149606300301 ) ) ;
#15055 = CARTESIAN_POINT ( 'NONE',  ( 0.1602931993194442739, 0.07955613945526338049, -0.1377952755905511861 ) ) ;
#15056 = ORIENTED_EDGE ( 'NONE', *, *, #5913, .T. ) ;
#15057 = FACE_OUTER_BOUND ( 'NONE', #42561, .T. ) ;
#15058 = CARTESIAN_POINT ( 'NONE',  ( -0.8759842519685039353, -0.1787899950787401882, 0.2091535432533232486 ) ) ;
#15059 = VERTEX_POINT ( 'NONE', #37200 ) ;
#15060 = CARTESIAN_POINT ( 'NONE',  ( 0.9412147342319837628, 0.1574803149606300301, 0.3321850393700786497 ) ) ;
#15061 = CARTESIAN_POINT ( 'NONE',  ( 0.1787899950787401604, -1.439960629867495401, -0.07405724077823318263 ) ) ;
#15062 = CARTESIAN_POINT ( 'NONE',  ( -0.7495606340400177148, -0.1264236179284866091, 1.660925196796630088 ) ) ;
#15063 = CARTESIAN_POINT ( 'NONE',  ( -0.6971942568897648851, -0.07405724077823297447, 0.9104330708123777871 ) ) ;
#15064 = CARTESIAN_POINT ( 'NONE',  ( -0.8759842519685039353, -0.1787899950787401882, 0.4109251967966299213 ) ) ;
#15065 = ADVANCED_FACE ( 'NONE', ( #1236 ), #26909, .T. ) ;
#15066 = CARTESIAN_POINT ( 'NONE',  ( -0.9873396505805591694, -0.1113553986120547346, 0.1624015748031496231 ) ) ;
#15067 = DIRECTION ( 'NONE',  ( 0.000000000000000000, 0.6156614753256575145, 0.7880107536067224583 ) ) ;
#15068 = CARTESIAN_POINT ( 'NONE',  ( 0.04076295239693379646, 0.06762482675903873364, -0.2618985693268080506 ) ) ;
#15069 = FACE_OUTER_BOUND ( 'NONE', #42876, .T. ) ;
#15070 = CARTESIAN_POINT ( 'NONE',  ( 0.1787899950787401604, -0.3485491650796322949, -0.07405724077823318263 ) ) ;
#15071 = CARTESIAN_POINT ( 'NONE',  ( -0.1917820371396724566, -0.08955957972813564927, -0.1527325450606088486 ) ) ;
#15072 = CARTESIAN_POINT ( 'NONE',  ( 0.000000000000000000, 0.6241017553149654784, 0.3240160679609099259 ) ) ;
#15073 = DIRECTION ( 'NONE',  ( -0.4999999999999998890, 0.000000000000000000, 0.8660254037844388186 ) ) ;
#15074 = EDGE_CURVE ( 'NONE', #13158, #7079, #16084, .T. ) ;
#15075 = CARTESIAN_POINT ( 'NONE',  ( 0.2559055118110236671, -0.1364700349299463877, -0.1001271636663048775 ) ) ;
#15076 = CARTESIAN_POINT ( 'NONE',  ( -0.8019270111902717657, 0.1787899950787401604, 0.3494094487651343006 ) ) ;
#15077 = ( BOUNDED_CURVE ( )  B_SPLINE_CURVE ( 2, ( #15916, #19485, #30543, #41493, #23335, #3922, #9662, #12796, #20662 ),
 .UNSPECIFIED., .F., .F. ) 
 B_SPLINE_CURVE_WITH_KNOTS ( ( 3, 2, 2, 2, 3 ),
 ( 0.6300000000000000044, 0.6324999999999999512, 0.6350000000000000089, 0.6374999999999999556, 0.6400000000000000133 ),
 .UNSPECIFIED. ) 
 CURVE ( )  GEOMETRIC_REPRESENTATION_ITEM ( )  RATIONAL_B_SPLINE_CURVE ( ( 1.000000000000000000, 0.9238795325112899581, 1.000000000000000000, 0.9238795325112869605, 1.000000000000000000, 0.9238795325112869605, 1.000000000000000000, 0.9238795325112869605, 1.000000000000000000 ) ) 
 REPRESENTATION_ITEM ( '' )  ) ;
#15078 = CARTESIAN_POINT ( 'NONE',  ( 1.033464566929134687, 0.06523048226347956391, 0.7997047244094481755 ) ) ;
#15079 = VERTEX_POINT ( 'NONE', #30062 ) ;
#15080 = CARTESIAN_POINT ( 'NONE',  ( -1.054774247047244540, -0.07405724077823318263, 1.402559055064346749 ) ) ;
#15081 = ORIENTED_EDGE ( 'NONE', *, *, #38885, .F. ) ;
#15082 = CARTESIAN_POINT ( 'NONE',  ( -0.1787899950787401604, -1.307086614119465695, -0.07405724077823318263 ) ) ;
#15083 = CARTESIAN_POINT ( 'NONE',  ( 0.1264236179284866091, -1.471948818843874074, -0.1264236179284866091 ) ) ;
#15084 = AXIS2_PLACEMENT_3D ( 'NONE', #12541, #22591, #27162 ) ;
#15085 = DIRECTION ( 'NONE',  ( 0.9999965023344152826, 0.002644866525197000530, -7.000000000000001727E-15 ) ) ;
#15086 = CARTESIAN_POINT ( 'NONE',  ( 0.7185039370078746268, 0.06523048226347956391, 0.4207677165354331561 ) ) ;
#15087 = DIRECTION ( 'NONE',  ( 0.000000000000000000, 0.000000000000000000, -1.000000000000000000 ) ) ;
#15088 = CARTESIAN_POINT ( 'NONE',  ( -0.9412147342319837628, -0.1574803149606297803, 1.055610236112945799 ) ) ;
#15089 = CARTESIAN_POINT ( 'NONE',  ( 0.7495606340400177148, 0.1264236179284866091, 0.3961614172690708924 ) ) ;
#15090 = CARTESIAN_POINT ( 'NONE',  ( -0.7646288533564489232, -0.1113553986120547346, 1.687992125984252079 ) ) ;
#15091 = CARTESIAN_POINT ( 'NONE',  ( 0.1113553986120547346, -0.2391732283464566844, -0.1113553986120547346 ) ) ;
#15092 = CARTESIAN_POINT ( 'NONE',  ( 0.7646288533564489232, 0.1113553986120547346, 1.904527558947590515 ) ) ;
#15093 = ORIENTED_EDGE ( 'NONE', *, *, #43868, .T. ) ;
#15094 = CARTESIAN_POINT ( 'NONE',  ( -0.1264236179284866091, -0.2071850393163153503, -0.1264236179284866091 ) ) ;
#15095 = CARTESIAN_POINT ( 'NONE',  ( 0.9412147342319837628, -0.1574803149606297803, 0.04183070866141735261 ) ) ;
#15096 = CARTESIAN_POINT ( 'NONE',  ( 1.033464566929133799, 0.000000000000000000, 0.9547244094488189781 ) ) ;
#15097 = CARTESIAN_POINT ( 'NONE',  ( -0.2362204724409465995, 0.1574803149606323616, -0.9891732283464564901 ) ) ;
#15098 = ( BOUNDED_CURVE ( )  B_SPLINE_CURVE ( 2, ( #12156, #18614, #7831, #44944, #4697, #33275, #7594, #29927, #4220 ),
 .UNSPECIFIED., .F., .T. ) 
 B_SPLINE_CURVE_WITH_KNOTS ( ( 3, 2, 2, 2, 3 ),
 ( 0.4600000000000000200, 0.4625000000000000222, 0.4650000000000000244, 0.4675000000000000266, 0.4699999999999999734 ),
 .UNSPECIFIED. ) 
 CURVE ( )  GEOMETRIC_REPRESENTATION_ITEM ( )  RATIONAL_B_SPLINE_CURVE ( ( 1.000000000000000000, 0.9238795325112869605, 1.000000000000000000, 0.9238795325112869605, 1.000000000000000000, 0.9238795325112869605, 1.000000000000000000, 0.9238795325112849621, 1.000000000000000000 ) ) 
 REPRESENTATION_ITEM ( '' )  ) ;
#15099 = EDGE_CURVE ( 'NONE', #44104, #31513, #27585, .T. ) ;
#15100 = CARTESIAN_POINT ( 'NONE',  ( -0.7185039370078739607, 0.000000000000000000, 2.007874015640504162 ) ) ;
#15101 = CARTESIAN_POINT ( 'NONE',  ( -0.1337103929845034622, -0.08955973559652113947, 0.09286901502511588080 ) ) ;
#15102 = CARTESIAN_POINT ( 'NONE',  ( -0.2665307357296562429, 0.1584585643853060888, 0.9308013911357060355 ) ) ;
#15103 = EDGE_LOOP ( 'NONE', ( #3492, #17210, #42277 ) ) ;
#15104 = LINE ( 'NONE', #33561, #8809 ) ;
#15105 = CARTESIAN_POINT ( 'NONE',  ( 0.5415383587465882886, 4.466152701071653354E-17, 0.000000000000000000 ) ) ;
#15106 = CARTESIAN_POINT ( 'NONE',  ( -0.07405724077823318263, -1.567913385773008095, 0.1787899950787401604 ) ) ;
#15107 = CARTESIAN_POINT ( 'NONE',  ( -0.1787899950787401604, -0.6771653542769455747, -0.07405724077823318263 ) ) ;
#15108 = CARTESIAN_POINT ( 'NONE',  ( -0.06523048226347956391, -1.161909448818897461, 0.1574803149606297803 ) ) ;
#15109 = CARTESIAN_POINT ( 'NONE',  ( 1.033464566929134687, 0.06523048226347956391, 1.065452755797984041 ) ) ;
#15110 = FACE_OUTER_BOUND ( 'NONE', #18912, .T. ) ;
#15111 = ORIENTED_EDGE ( 'NONE', *, *, #44348, .T. ) ;
#15112 = ORIENTED_EDGE ( 'NONE', *, *, #24241, .F. ) ;
#15113 = VERTEX_POINT ( 'NONE', #15654 ) ;
#15114 = CARTESIAN_POINT ( 'NONE',  ( -0.8019270111902717657, -0.1787899950787401604, 1.589566929080094448 ) ) ;
#15115 = ADVANCED_FACE ( 'NONE', ( #30514 ), #37919, .T. ) ;
#15116 = CARTESIAN_POINT ( 'NONE',  ( 0.8759842519685039353, -0.1787899950787401882, 1.670767716481669440 ) ) ;
#15117 = CARTESIAN_POINT ( 'NONE',  ( -1.002407869896990045, 0.1264236179284866091, 0.8193897637257637756 ) ) ;
#15118 = CARTESIAN_POINT ( 'NONE',  ( -1.033464566929133799, 0.000000000000000000, 0.7480314959554645871 ) ) ;
#15119 = CARTESIAN_POINT ( 'NONE',  ( 0.8019270111902717657, 0.1787899950787401604, 0.3149606298674962890 ) ) ;
#15120 = CARTESIAN_POINT ( 'NONE',  ( -1.033464566929133799, 0.000000000000000000, 1.496062992018456494 ) ) ;
#15121 = CARTESIAN_POINT ( 'NONE',  ( -0.9500414927467377701, 0.1787899950787401604, 1.171259842465921741 ) ) ;
#15122 = CARTESIAN_POINT ( 'NONE',  ( -0.8019270111902716547, -0.1787899950787401604, 0.7972440944344248992 ) ) ;
#15123 = DIRECTION ( 'NONE',  ( 0.000000000000000000, -0.7880107536067207930, 0.6156614753256598460 ) ) ;
#15124 = EDGE_CURVE ( 'NONE', #22445, #28080, #4125, .T. ) ;
#15125 = DIRECTION ( 'NONE',  ( -1.000000000000000000, 0.000000000000000000, 0.000000000000000000 ) ) ;
#15126 = CARTESIAN_POINT ( 'NONE',  ( -0.9500414927467378812, 0.1787899950787401604, 1.648622047190331230 ) ) ;
#15127 = CARTESIAN_POINT ( 'NONE',  ( -0.9412147342319837628, -0.1574803149606297803, 1.882381889656251861 ) ) ;
#15128 = ORIENTED_EDGE ( 'NONE', *, *, #43493, .F. ) ;
#15129 = CARTESIAN_POINT ( 'NONE',  ( -0.7185039370078739607, 1.928577636452523993E-17, 1.604330708661417360 ) ) ;
#15130 = CARTESIAN_POINT ( 'NONE',  ( 1.033464566929133355, 0.06523048226348168721, 1.626476377952755570 ) ) ;
#15131 = CARTESIAN_POINT ( 'NONE',  ( 1.002407869896990045, -0.1264236179284866091, 1.478838582623401399 ) ) ;
#15132 = CARTESIAN_POINT ( 'NONE',  ( 0.06901435990846417623, -0.09851382358029528441, 0.1342407315491202791 ) ) ;
#15133 = DIRECTION ( 'NONE',  ( 0.000000000000000000, 0.000000000000000000, -1.000000000000000000 ) ) ;
#15134 = ORIENTED_EDGE ( 'NONE', *, *, #33690, .F. ) ;
#15135 = EDGE_CURVE ( 'NONE', #28233, #22011, #709, .T. ) ;
#15136 = ORIENTED_EDGE ( 'NONE', *, *, #18130, .F. ) ;
#15137 = EDGE_LOOP ( 'NONE', ( #13819, #20209, #9040, #1 ) ) ;
#15138 = CARTESIAN_POINT ( 'NONE',  ( -0.1787899950787401604, -0.8690944881352120621, 0.07405724077823318263 ) ) ;
#15139 = CARTESIAN_POINT ( 'NONE',  ( 0.1264236179284866091, -0.3745078739619845942, -0.1264236179284866091 ) ) ;
#15140 = CARTESIAN_POINT ( 'NONE',  ( 0.07405724077823318263, -1.036417322780882833, -0.1787899950787401604 ) ) ;
#15141 = CYLINDRICAL_SURFACE ( 'NONE', #5658, 0.3912448816427701037 ) ;
#15142 = CARTESIAN_POINT ( 'NONE',  ( 1.002407869896990045, -0.1264236179284866091, 1.749507873961984483 ) ) ;
#15143 = CARTESIAN_POINT ( 'NONE',  ( 0.8107537697050253289, 0.1574803149606300301, 0.2977362204724410821 ) ) ;
#15144 = CARTESIAN_POINT ( 'NONE',  ( 3.301370929368692659E-17, -0.1486658568271399528, 0.1797182628040039365 ) ) ;
#15145 = CARTESIAN_POINT ( 'NONE',  ( 0.7185039370078739607, 1.928577636452523993E-17, 0.1082677165354330728 ) ) ;
#15146 = CARTESIAN_POINT ( 'NONE',  ( 0.1264236179284866091, -0.03001968498560653523, 0.1264236179284866091 ) ) ;
#15147 = DIRECTION ( 'NONE',  ( 0.000000000000000000, -1.000000000000000000, 0.000000000000000000 ) ) ;
#15148 = CARTESIAN_POINT ( 'NONE',  ( 0.8759842519685039353, -0.1787899950787401882, 0.7603346456155274380 ) ) ;
#15149 = CIRCLE ( 'NONE', #581, 0.09842519685039310962 ) ;
#15151 = CARTESIAN_POINT ( 'NONE',  ( 0.9412147342319837628, -0.1574803149606297803, 1.134350393593259732 ) ) ;
#15150 = CARTESIAN_POINT ( 'NONE',  ( 0.05572156214699040822, 0.2633233733571749835, -0.05578523004296867538 ) ) ;
#15153 = CARTESIAN_POINT ( 'NONE',  ( -0.8989048142471400826, -0.1738438585959865001, 1.988589590799940687 ) ) ;
#15152 = CARTESIAN_POINT ( 'NONE',  ( 0.2821522309711287368, 4.616380251121755931E-17, 0.000000000000000000 ) ) ;
#15154 = FACE_OUTER_BOUND ( 'NONE', #1074, .T. ) ;
#15155 = CARTESIAN_POINT ( 'NONE',  ( 0.9500414927467378812, -0.1787899950787401604, 1.830708661363559253 ) ) ;
#15156 = LINE ( 'NONE', #44346, #12494 ) ;
#15157 = EDGE_CURVE ( 'NONE', #954, #6423, #4541, .T. ) ;
#15158 = CARTESIAN_POINT ( 'NONE',  ( 0.9873396505805591694, 0.1113553986120547346, 0.05413385826771653642 ) ) ;
#15159 = CARTESIAN_POINT ( 'NONE',  ( 0.1608764814808673338, -0.1607246848665348227, -0.002792769038232397350 ) ) ;
#15160 = CARTESIAN_POINT ( 'NONE',  ( 0.1787899950787401604, -0.3375984251430867999, -0.07405724077823318263 ) ) ;
#15161 = CARTESIAN_POINT ( 'NONE',  ( 0.5057057357416000487, 4.766607801171850497E-17, 0.000000000000000000 ) ) ;
#15162 = CARTESIAN_POINT ( 'NONE',  ( 0.07405724077823318263, -1.169291338528914537, 0.1787899950787401604 ) ) ;
#15163 = CARTESIAN_POINT ( 'NONE',  ( 0.6971942568897626646, -0.07405724077823297447, 0.2066929133320631329 ) ) ;
#15164 = DIRECTION ( 'NONE',  ( -0.000000000000000000, 0.6156614753256597350, 0.7880107536067206819 ) ) ;
#15165 = ADVANCED_FACE ( 'NONE', ( #18977 ), #999, .F. ) ;
#15166 = CARTESIAN_POINT ( 'NONE',  ( -1.054774247047244540, 0.07405724077823318263, 1.520669291284818758 ) ) ;
#15167 = ORIENTED_EDGE ( 'NONE', *, *, #46577, .T. ) ;
#15168 = CARTESIAN_POINT ( 'NONE',  ( -1.054774247047244096, 0.000000000000000000, 1.168799212544661348 ) ) ;
#15169 = CARTESIAN_POINT ( 'NONE',  ( -0.3161444924769509779, 1.209494567139727250, -1.479906699140296045 ) ) ;
#15170 = ADVANCED_FACE ( 'NONE', ( #8430 ), #38847, .T. ) ;
#15171 = CARTESIAN_POINT ( 'NONE',  ( 1.002407869896990045, -0.1264236179284866091, 1.321358267662771757 ) ) ;
#15172 = CARTESIAN_POINT ( 'NONE',  ( 0.06523048226347956391, -1.211122047136568236, -0.1574803149606300301 ) ) ;
#15173 = CARTESIAN_POINT ( 'NONE',  ( 0.8019270111902717657, 0.1787899950787401604, 1.924212598371433325 ) ) ;
#15174 = CARTESIAN_POINT ( 'NONE',  ( -0.7495606340400177148, 0.1264236179284866091, 1.099901574749385880 ) ) ;
#15175 = CARTESIAN_POINT ( 'NONE',  ( -0.4620708661417322616, 0.6529540528279709211, 0.4629603087243968074 ) ) ;
#15176 = CARTESIAN_POINT ( 'NONE',  ( -1.033464566929133799, 0.000000000000000000, 0.3641732283464567121 ) ) ;
#15177 = CARTESIAN_POINT ( 'NONE',  ( 0.8759842519685039353, -0.1787899950787401882, 0.4502952755367874427 ) ) ;
#15178 = CARTESIAN_POINT ( 'NONE',  ( -0.6971942568897626646, -0.07405724077823297447, 0.3198818897100159098 ) ) ;
#15179 = CARTESIAN_POINT ( 'NONE',  ( -1.002407869896990045, -0.1264236179284866091, 0.7258858267178898149 ) ) ;
#15180 = CARTESIAN_POINT ( 'NONE',  ( 1.033464566929133799, 0.000000000000000000, 1.732283464459401623 ) ) ;
#15181 = ORIENTED_EDGE ( 'NONE', *, *, #14833, .F. ) ;
#15182 = DIRECTION ( 'NONE',  ( -1.000000000000000000, 0.000000000000000000, 0.000000000000000000 ) ) ;
#15183 = CARTESIAN_POINT ( 'NONE',  ( -1.033464566929134687, 0.06523048226347956391, 0.1304133858267717272 ) ) ;
#15184 = CARTESIAN_POINT ( 'NONE',  ( 0.8019270111902716547, 0.1787899950787401604, 1.062992125930488418 ) ) ;
#15185 = CARTESIAN_POINT ( 'NONE',  ( 0.5358894627757212481, 1.205361022782824954E-17, -0.09842519685039370636 ) ) ;
#15186 = VERTEX_POINT ( 'NONE', #2415 ) ;
#15187 = CARTESIAN_POINT ( 'NONE',  ( 0.7185039370078739607, 1.928577636452523993E-17, 0.3051181102362204856 ) ) ;
#15188 = CARTESIAN_POINT ( 'NONE',  ( -0.07405724077823318263, -1.465675149331600480, 0.1787899950787401604 ) ) ;
#15189 = EDGE_LOOP ( 'NONE', ( #37385, #31133, #31022, #12059 ) ) ;
#15190 = CARTESIAN_POINT ( 'NONE',  ( -0.1264236179284866091, -0.3991141731745826982, -0.1264236179284866091 ) ) ;
#15191 = CARTESIAN_POINT ( 'NONE',  ( -1.033464566929133799, 0.000000000000000000, 1.692913385719244213 ) ) ;
#15192 = ORIENTED_EDGE ( 'NONE', *, *, #11778, .T. ) ;
#15193 = CARTESIAN_POINT ( 'NONE',  ( 0.6971942568897637749, 2.189545951927499583E-17, 1.262303149552535420 ) ) ;
#15194 = DIRECTION ( 'NONE',  ( 0.000000000000000000, -1.000000000000000000, 0.000000000000000000 ) ) ;
#15195 = CYLINDRICAL_SURFACE ( 'NONE', #31534, 0.1574803149606299191 ) ;
#15196 = CARTESIAN_POINT ( 'NONE',  ( -0.7646288533564489232, 0.1113553986120547346, 1.441929133858267598 ) ) ;
#15197 = CARTESIAN_POINT ( 'NONE',  ( 0.6971942568897626646, -0.07405724077823297447, 0.1624015747493861295 ) ) ;
#15198 = CARTESIAN_POINT ( 'NONE',  ( -0.1787899950787401604, -1.700787401521039355, -0.07405724077823318263 ) ) ;
#15199 = CARTESIAN_POINT ( 'NONE',  ( 0.1787899950787401604, -1.754921259788755128, 0.07405724077823318263 ) ) ;
#15200 = PRODUCT_CONTEXT ( 'NONE', #37994, 'mechanical' ) ;
#15201 = CARTESIAN_POINT ( 'NONE',  ( 0.1184675242425320824, 0.3740157480314960647, 1.713085361781127913 ) ) ;
#15202 = CARTESIAN_POINT ( 'NONE',  ( -0.6971942568897637749, 2.189545951927499583E-17, 0.6766732282926929409 ) ) ;
#15203 = AXIS2_PLACEMENT_3D ( 'NONE', #7824, #148, #33743 ) ;
#15204 = SURFACE_SIDE_STYLE ('',( #30322 ) ) ;
#15205 = CARTESIAN_POINT ( 'NONE',  ( -0.1270800023317771588, -1.374059557614541349, 0.1270800023317771588 ) ) ;
#15206 = CARTESIAN_POINT ( 'NONE',  ( -0.9412147342319837628, 0.1574803149606300301, 1.198326771653543732 ) ) ;
#15207 = CARTESIAN_POINT ( 'NONE',  ( 0.8019270111902717657, -0.1787899950787401604, 1.353346456639149986 ) ) ;
#15208 = CARTESIAN_POINT ( 'NONE',  ( 0.9500414927467377701, -0.1787899950787401604, 1.707677165300568456 ) ) ;
#15210 = EDGE_CURVE ( 'NONE', #10497, #28468, #45319, .T. ) ;
#15209 = LINE ( 'NONE', #44635, #34567 ) ;
#15211 = CYLINDRICAL_SURFACE ( 'NONE', #39698, 0.1574803149606299191 ) ;
#15212 = DIRECTION ( 'NONE',  ( 0.000000000000000000, 1.000000000000000000, 0.000000000000000000 ) ) ;
#15213 = CARTESIAN_POINT ( 'NONE',  ( 0.1264236179284866091, 0.1373031496600628232, -0.1264236179284866091 ) ) ;
#15214 = DIRECTION ( 'NONE',  ( 1.000000000000000000, -0.000000000000000000, -0.000000000000000000 ) ) ;
#15215 = AXIS2_PLACEMENT_3D ( 'NONE', #11658, #22417, #28946 ) ;
#15216 = EDGE_CURVE ( 'NONE', #37608, #44070, #34004, .T. ) ;
#15217 = CARTESIAN_POINT ( 'NONE',  ( 1.002407869896990045, 0.1264236179284866091, 1.247539370024976391 ) ) ;
#15218 = DIRECTION ( 'NONE',  ( -1.000000000000000000, 0.000000000000000000, 0.000000000000000000 ) ) ;
#15219 = LINE ( 'NONE', #29868, #42913 ) ;
#15220 = CARTESIAN_POINT ( 'NONE',  ( -1.002407869896990045, 0.1264236179284866091, 1.168799212544661348 ) ) ;
#15221 = CARTESIAN_POINT ( 'NONE',  ( 0.9873396505805591694, -0.1113553986120547346, 0.5856299211523157133 ) ) ;
#15222 = VERTEX_POINT ( 'NONE', #38144 ) ;
#15223 = CARTESIAN_POINT ( 'NONE',  ( -0.4338976377952755703, -0.2362204724409449064, 0.000000000000000000 ) ) ;
#15224 = EDGE_CURVE ( 'NONE', #32938, #33816, #22653, .T. ) ;
#15225 = CARTESIAN_POINT ( 'NONE',  ( 0.8376409825901903750, 0.1727894281041914559, 0.03936911855021455603 ) ) ;
#15226 = ORIENTED_EDGE ( 'NONE', *, *, #22130, .T. ) ;
#15227 = CARTESIAN_POINT ( 'NONE',  ( 0.1270800023317771588, -0.01579184107910856436, -0.1270800023317771588 ) ) ;
#15228 = CARTESIAN_POINT ( 'NONE',  ( -0.8107537697050234415, -0.1574803149606297803, 0.3026574802074336046 ) ) ;
#15229 = CARTESIAN_POINT ( 'NONE',  ( -0.1264236179284866091, -1.152066929080094448, -0.1264236179284866091 ) ) ;
#15230 = VERTEX_POINT ( 'NONE', #9866 ) ;
#15231 = FACE_OUTER_BOUND ( 'NONE', #2768, .T. ) ;
#15232 = CARTESIAN_POINT ( 'NONE',  ( 0.7495606340400177148, 0.1264236179284866091, 1.651082677111590513 ) ) ;
#15233 = EDGE_CURVE ( 'NONE', #18913, #18496, #45546, .T. ) ;
#15234 = CARTESIAN_POINT ( 'NONE',  ( -0.1574803149606299191, 1.928577636452524610E-17, -0.0009999999999999347518 ) ) ;
#15236 = CARTESIAN_POINT ( 'NONE',  ( -0.7185039370078739607, 1.928577636452523993E-17, 1.368110236220472675 ) ) ;
#15235 = CARTESIAN_POINT ( 'NONE',  ( 0.1605229034655323017, -0.09306627081912521859, 0.1197794644537587411 ) ) ;
#15237 = CARTESIAN_POINT ( 'NONE',  ( 0.6971942568897637749, 2.189545951927499583E-17, 0.04675196845017354913 ) ) ;
#15238 = CARTESIAN_POINT ( 'NONE',  ( 0.07405724077823318263, -0.1456692912848192578, 0.1787899950787401604 ) ) ;
#15239 = ORIENTED_EDGE ( 'NONE', *, *, #8941, .T. ) ;
#15240 = CARTESIAN_POINT ( 'NONE',  ( -0.1113553986120547346, 0.08562992125984252023, -0.1113553986120547346 ) ) ;
#15241 = CARTESIAN_POINT ( 'NONE',  ( -0.03810507699822204830, -0.06563552548610597503, 0.2634293601846930954 ) ) ;
#15242 = CARTESIAN_POINT ( 'NONE',  ( 0.9500414927467377701, 0.1787899950787401604, 0.9005905511273391006 ) ) ;
#15243 = CARTESIAN_POINT ( 'NONE',  ( -1.054774247047244096, 0.000000000000000000, 1.478838582623401399 ) ) ;
#15244 = CARTESIAN_POINT ( 'NONE',  ( 0.1574803149606300301, -0.03986220461688239070, 0.06523048226347956391 ) ) ;
#15245 = ORIENTED_EDGE ( 'NONE', *, *, #32097, .F. ) ;
#15246 = ( BOUNDED_CURVE ( )  B_SPLINE_CURVE ( 2, ( #1919, #5041, #19661, #34524, #19893, #1680, #16327, #41911, #38585 ),
 .UNSPECIFIED., .F., .F. ) 
 B_SPLINE_CURVE_WITH_KNOTS ( ( 3, 2, 2, 2, 3 ),
 ( 0.2899999999999999800, 0.2924999999999999822, 0.2949999999999999845, 0.2974999999999999867, 0.2999999999999999889 ),
 .UNSPECIFIED. ) 
 CURVE ( )  GEOMETRIC_REPRESENTATION_ITEM ( )  RATIONAL_B_SPLINE_CURVE ( ( 1.000000000000000000, 0.9238795325112869605, 1.000000000000000000, 0.9238795325112869605, 1.000000000000000000, 0.9238795325112869605, 1.000000000000000000, 0.9238795325112869605, 1.000000000000000000 ) ) 
 REPRESENTATION_ITEM ( '' )  ) ;
#15247 = AXIS2_PLACEMENT_3D ( 'NONE', #45360, #41507, #16162 ) ;
#15248 = CARTESIAN_POINT ( 'NONE',  ( -1.002407869896990045, -0.1264236179284866091, 0.3764763778989925203 ) ) ;
#15249 = DIRECTION ( 'NONE',  ( 1.000000000000000000, 0.000000000000000000, -0.000000000000000000 ) ) ;
#15250 = CARTESIAN_POINT ( 'NONE',  ( -0.1377952755905511584, 0.1574803149606320007, 0.7066929133858274037 ) ) ;
#15251 = CARTESIAN_POINT ( 'NONE',  ( -0.1264236179284866091, -0.9956948343709705052, 0.1264236179284866091 ) ) ;
#15252 = ORIENTED_EDGE ( 'NONE', *, *, #17641, .F. ) ;
#15253 = CARTESIAN_POINT ( 'NONE',  ( -0.7185039370078739607, 0.000000000000000000, -2.869337061179095023E-17 ) ) ;
#15254 = ORIENTED_EDGE ( 'NONE', *, *, #21878, .F. ) ;
#15255 = CARTESIAN_POINT ( 'NONE',  ( 1.054774247047244540, 0.07405724077823318263, 1.008858267662772423 ) ) ;
#15256 = AXIS2_PLACEMENT_3D ( 'NONE', #25621, #33057, #7852 ) ;
#15257 = CARTESIAN_POINT ( 'NONE',  ( -0.9412147342319837628, -0.1574803149606297803, 0.5831692912310552090 ) ) ;
#15258 = AXIS2_PLACEMENT_3D ( 'NONE', #44021, #870, #11453 ) ;
#15259 = CARTESIAN_POINT ( 'NONE',  ( -0.7185039370078739607, 1.928577636452523993E-17, 0.6594488188976378451 ) ) ;
#15260 = CARTESIAN_POINT ( 'NONE',  ( -0.9873396505805591694, 0.1113553986120547346, 0.9202755905511811330 ) ) ;
#15261 = FACE_OUTER_BOUND ( 'NONE', #35123, .T. ) ;
#15262 = CARTESIAN_POINT ( 'NONE',  ( -1.100456976456230270E-17, -1.073862707220840651, -0.1797182628040039365 ) ) ;
#15263 = CARTESIAN_POINT ( 'NONE',  ( 0.1476377952755906220, 0.2573565155132549465, -0.3015174453633734930 ) ) ;
#15264 = CARTESIAN_POINT ( 'NONE',  ( -0.8107537697050253289, 0.1574803149606300301, 1.587106299105073060 ) ) ;
#15265 = CARTESIAN_POINT ( 'NONE',  ( 0.6971942568897626646, 0.07405724077823318263, 0.9498031495525356416 ) ) ;
#15266 = DIRECTION ( 'NONE',  ( -1.000000000000000000, 0.000000000000000000, 0.000000000000000000 ) ) ;
#15267 = CARTESIAN_POINT ( 'NONE',  ( 0.8107537697050253289, -0.1574803149606297803, 1.375492125984252523 ) ) ;
#15269 = CARTESIAN_POINT ( 'NONE',  ( 2.892866454678787531E-17, 0.1102362205799679168, 0.1574803149606299191 ) ) ;
#15268 = CARTESIAN_POINT ( 'NONE',  ( 0.7102373793000918978, 0.005418808439761009510, 1.983169977139155993 ) ) ;
#15270 = CARTESIAN_POINT ( 'NONE',  ( 0.2759478392031617933, -0.09842519685039370636, 1.713085361781125915 ) ) ;
#15271 = ADVANCED_FACE ( 'NONE', ( #42192 ), #19085, .T. ) ;
#15272 = CARTESIAN_POINT ( 'NONE',  ( 0.9500414927467377701, -0.1787899950787401604, 0.8415354330171020969 ) ) ;
#15273 = CIRCLE ( 'NONE', #12982, 0.08090551181102362266 ) ;
#15274 = CARTESIAN_POINT ( 'NONE',  ( -0.1787899950787401604, -0.8297244093950564281, -0.07405724077823318263 ) ) ;
#15275 = VERTEX_POINT ( 'NONE', #28091 ) ;
#15276 = ADVANCED_FACE ( 'NONE', ( #1709 ), #24249, .T. ) ;
#15277 = CARTESIAN_POINT ( 'NONE',  ( 0.004734662961502830204, -0.1434636420619076758, 0.02711672434618991184 ) ) ;
#15278 = CARTESIAN_POINT ( 'NONE',  ( 0.9500414927467378812, 0.1787899950787401604, 1.171259842465921741 ) ) ;
#15279 = ADVANCED_FACE ( 'NONE', ( #16357 ), #20866, .F. ) ;
#15280 = CYLINDRICAL_SURFACE ( 'NONE', #8092, 0.1003937007874010356 ) ;
#15281 = CARTESIAN_POINT ( 'NONE',  ( -9.642888182262618425E-18, -1.651574803149606474, -0.1574803149606299191 ) ) ;
#15282 = FACE_OUTER_BOUND ( 'NONE', #4913, .T. ) ;
#15283 = ORIENTED_EDGE ( 'NONE', *, *, #3073, .F. ) ;
#15284 = FACE_BOUND ( 'NONE', #1299, .T. ) ;
#15285 = CARTESIAN_POINT ( 'NONE',  ( -0.8759842519685039353, 0.1787899950787401882, 0.1894685038832444879 ) ) ;
#15286 = VECTOR ( 'NONE', #408, 39.37007874015748143 ) ;
#15287 = CARTESIAN_POINT ( 'NONE',  ( 0.7185039370078739607, 1.928577636452523993E-17, 0.3444881889763780070 ) ) ;
#15288 = CARTESIAN_POINT ( 'NONE',  ( -1.002407869896990045, -0.1264236179284866091, 1.670767716481669440 ) ) ;
#15289 = CARTESIAN_POINT ( 'NONE',  ( -1.054774247047244096, 0.000000000000000000, 0.8882874015210394658 ) ) ;
#15290 = CARTESIAN_POINT ( 'NONE',  ( -0.7495606340400177148, -0.1264236179284866091, 0.4453740156942677664 ) ) ;
#15291 = CARTESIAN_POINT ( 'NONE',  ( -1.033464566929133799, 1.928577636452524610E-17, 2.869337061179095023E-17 ) ) ;
#15292 = DIRECTION ( 'NONE',  ( -1.000000000000000000, 0.000000000000000000, 0.000000000000000000 ) ) ;
#15293 = CARTESIAN_POINT ( 'NONE',  ( 0.04878249046419585316, 0.07306521771081567196, -0.2572684868648978385 ) ) ;
#15294 = CARTESIAN_POINT ( 'NONE',  ( -0.3070711847658871285, 0.04416910270118660359, -0.7142167645079522398 ) ) ;
#15295 = CARTESIAN_POINT ( 'NONE',  ( -0.1787899950787401882, -0.6069153068119154115, 0.000000000000000000 ) ) ;
#15296 = CARTESIAN_POINT ( 'NONE',  ( -0.1204886227201696774, -0.08955993428987342464, 0.1930813601014000069 ) ) ;
#15297 = CARTESIAN_POINT ( 'NONE',  ( -0.1574803149606299191, 1.126631386849005212, -3.440787370833235492 ) ) ;
#15298 = CARTESIAN_POINT ( 'NONE',  ( -0.4330708661417322913, 0.1864803149606299448, 1.186023622047243986 ) ) ;
#15299 = CARTESIAN_POINT ( 'NONE',  ( -0.8759842519685039353, -0.1574803149606299191, 1.171259842412157637 ) ) ;
#15300 = CARTESIAN_POINT ( 'NONE',  ( -0.6971942568897637749, 2.189545951927499583E-17, 0.3567913385289137596 ) ) ;
#15301 = CARTESIAN_POINT ( 'NONE',  ( -0.1264236179284866091, -1.753568850119002098, -0.1264236179284866091 ) ) ;
#15303 = ORIENTED_EDGE ( 'NONE', *, *, #22, .T. ) ;
#15302 = VECTOR ( 'NONE', #21992, 39.37007874015748143 ) ;
#15304 = EDGE_LOOP ( 'NONE', ( #32357, #24069, #10655, #33477 ) ) ;
#15305 = CARTESIAN_POINT ( 'NONE',  ( -0.6971942568897648851, 0.07405724077823318263, 1.500984251914741829 ) ) ;
#15306 = VERTEX_POINT ( 'NONE', #35278 ) ;
#15307 = CARTESIAN_POINT ( 'NONE',  ( -0.1787899950787401882, -1.304625984198204636, 0.000000000000000000 ) ) ;
#15308 = AXIS2_PLACEMENT_3D ( 'NONE', #21585, #36226, #40947 ) ;
#15309 = CARTESIAN_POINT ( 'NONE',  ( 0.1264236179284866091, -1.511318897584031484, -0.1264236179284866091 ) ) ;
#15310 = DIRECTION ( 'NONE',  ( -0.0001414325466099314820, 0.05347417367636585206, -0.9985692228115508051 ) ) ;
#15311 = CARTESIAN_POINT ( 'NONE',  ( 1.033464566929134687, -0.06523048226347956391, 0.5191929133858269596 ) ) ;
#15312 = DIRECTION ( 'NONE',  ( -1.000000000000000000, 0.000000000000000000, 0.000000000000000000 ) ) ;
#15313 = CARTESIAN_POINT ( 'NONE',  ( -0.7185039370078746268, -0.06523048226347956391, 1.045767716427905114 ) ) ;
#15314 = CARTESIAN_POINT ( 'NONE',  ( 0.8759842519685039353, 0.1787899950787401882, 0.5487204723871811352 ) ) ;
#15315 = CARTESIAN_POINT ( 'NONE',  ( -0.8070866141732283561, -0.3937007874015746034, -0.6590551181102368705 ) ) ;
#15316 = ( REPRESENTATION_RELATIONSHIP ('NONE','NONE', #9609, #9335 ) REPRESENTATION_RELATIONSHIP_WITH_TRANSFORMATION ( #46053 )SHAPE_REPRESENTATION_RELATIONSHIP( ) ) ;
#15317 = CARTESIAN_POINT ( 'NONE',  ( -9.642888182262618425E-18, -0.2736220472440945017, -0.1574803149606299191 ) ) ;
#15318 = ORIENTED_EDGE ( 'NONE', *, *, #28067, .F. ) ;
#15319 = DIRECTION ( 'NONE',  ( 1.000000000000000000, 0.000000000000000000, 0.000000000000000000 ) ) ;
#15320 = ORIENTED_EDGE ( 'NONE', *, *, #30247, .T. ) ;
#15321 = CARTESIAN_POINT ( 'NONE',  ( -0.1487246401439196453, -0.09667468234190848553, -0.09990315886301043280 ) ) ;
#15322 = CARTESIAN_POINT ( 'NONE',  ( -0.8019270111902716547, 0.1787899950787401604, 1.023622047190330342 ) ) ;
#15323 = CARTESIAN_POINT ( 'NONE',  ( 1.033464566929134687, -0.06523048226347956391, 0.9128937007874008414 ) ) ;
#15324 = DIRECTION ( 'NONE',  ( 0.000000000000000000, 0.000000000000000000, 1.000000000000000000 ) ) ;
#15325 = ADVANCED_FACE ( 'NONE', ( #5550 ), #31686, .T. ) ;
#15326 = CARTESIAN_POINT ( 'NONE',  ( -0.9873396505805591694, -0.1113553986120547346, 0.8316929133858268486 ) ) ;
#15327 = CARTESIAN_POINT ( 'NONE',  ( -0.1690507553807868990, -0.08956027919751255451, -0.02600493670471536872 ) ) ;
#15328 = EDGE_LOOP ( 'NONE', ( #23045, #41791, #6973, #23452, #15735 ) ) ;
#15329 = DIRECTION ( 'NONE',  ( 5.310452730157438139E-15, 0.7880107536067220142, -0.6156614753256581807 ) ) ;
#15330 = CARTESIAN_POINT ( 'NONE',  ( -0.2833779466431470828, 0.1260493684579866713, 0.7654247733636371231 ) ) ;
#15331 = ORIENTED_EDGE ( 'NONE', *, *, #41846, .T. ) ;
#15332 = EDGE_CURVE ( 'NONE', #26580, #24404, #3039, .T. ) ;
#15333 = VERTEX_POINT ( 'NONE', #13461 ) ;
#15334 = CARTESIAN_POINT ( 'NONE',  ( 0.8759842519685039353, -0.1574803149606299191, 0.8267716535433071723 ) ) ;
#15335 = CARTESIAN_POINT ( 'NONE',  ( 0.7185039370078766252, -0.06523048226348168721, 1.370570866141733068 ) ) ;
#15336 = CARTESIAN_POINT ( 'NONE',  ( -0.1787899950787401604, -1.538385826717890703, -0.07405724077823318263 ) ) ;
#15337 = CARTESIAN_POINT ( 'NONE',  ( -1.094772975963752103E-17, -0.8026574802611967652, -0.1787899950787401882 ) ) ;
#15338 = CARTESIAN_POINT ( 'NONE',  ( -0.06523048226347956391, -1.137303149606299080, -0.1574803149606300301 ) ) ;
#15339 = CARTESIAN_POINT ( 'NONE',  ( 0.9412147342319837628, 0.1574803149606300301, 1.188484251860977503 ) ) ;
#15340 = CARTESIAN_POINT ( 'NONE',  ( -1.002407869896990045, -0.1264236179284866091, 0.4896653542769449086 ) ) ;
#15341 = ORIENTED_EDGE ( 'NONE', *, *, #6749, .T. ) ;
#15342 = ORIENTED_EDGE ( 'NONE', *, *, #35660, .F. ) ;
#15343 = CARTESIAN_POINT ( 'NONE',  ( -0.9500414927467378812, -0.1787899950787401604, 1.712598425143087688 ) ) ;
#15344 = CARTESIAN_POINT ( 'NONE',  ( 0.8759842519685039353, -0.1787899950787401882, 1.631397637741511808 ) ) ;
#15345 = CARTESIAN_POINT ( 'NONE',  ( 0.1113553986120547346, -1.331692913278299084, -0.1113553986120547346 ) ) ;
#15346 = DIRECTION ( 'NONE',  ( 0.000000000000000000, 0.000000000000000000, -1.000000000000000000 ) ) ;
#15347 = CARTESIAN_POINT ( 'NONE',  ( 0.6971942568897626646, -0.07405724077823297447, 0.2460629920722207375 ) ) ;
#15348 = CIRCLE ( 'NONE', #8448, 0.09940944881889761386 ) ;
#15349 = CARTESIAN_POINT ( 'NONE',  ( 0.2759478392031617933, -0.5708661417322835607, 1.713085361781125915 ) ) ;
#15350 = CARTESIAN_POINT ( 'NONE',  ( -1.002407869896990045, 0.1264236179284866091, 1.286909448765133801 ) ) ;
#15351 = CARTESIAN_POINT ( 'NONE',  ( -0.8759842519685039353, -0.1787899950787401882, 0.9178149605761574126 ) ) ;
#15352 = AXIS2_PLACEMENT_3D ( 'NONE', #18404, #26565, #22948 ) ;
#15353 = CARTESIAN_POINT ( 'NONE',  ( -0.6971942568897626646, -0.07405724077823297447, 0.1279527558517483676 ) ) ;
#15354 = ( BOUNDED_CURVE ( )  B_SPLINE_CURVE ( 2, ( #35388, #25557, #13796, #40128, #2531, #2762, #46615, #31800, #46383 ),
 .UNSPECIFIED., .F., .T. ) 
 B_SPLINE_CURVE_WITH_KNOTS ( ( 3, 2, 2, 2, 3 ),
 ( 0.3599999999999999867, 0.3624999999999999889, 0.3649999999999999911, 0.3674999999999999933, 0.3699999999999999956 ),
 .UNSPECIFIED. ) 
 CURVE ( )  GEOMETRIC_REPRESENTATION_ITEM ( )  RATIONAL_B_SPLINE_CURVE ( ( 1.000000000000000000, 0.9238795325112869605, 1.000000000000000000, 0.9238795325112869605, 1.000000000000000000, 0.9238795325112869605, 1.000000000000000000, 0.9238795325112869605, 1.000000000000000000 ) ) 
 REPRESENTATION_ITEM ( '' )  ) ;
#15355 = CARTESIAN_POINT ( 'NONE',  ( 0.1235961452251413406, 0.09842519685039370636, 0.2140748031496062798 ) ) ;
#15356 = CARTESIAN_POINT ( 'NONE',  ( -0.8759842519685039353, 0.1787899950787401882, 1.611712598371433103 ) ) ;
#15357 = CARTESIAN_POINT ( 'NONE',  ( -1.033464566929134687, -0.06523048226347956391, 1.926673228238929170 ) ) ;
#15358 = ORIENTED_EDGE ( 'NONE', *, *, #37069, .F. ) ;
#15359 = CARTESIAN_POINT ( 'NONE',  ( -0.8759842519685039353, -0.1574803149606299191, 1.653543307086614345 ) ) ;
#15360 = CARTESIAN_POINT ( 'NONE',  ( 0.2066929133858268486, -0.3022687907404924545, -1.075852903322848331 ) ) ;
#15361 = CARTESIAN_POINT ( 'NONE',  ( 0.6971942568897648851, -0.07405724077823297447, 1.584645669237574994 ) ) ;
#15362 = CARTESIAN_POINT ( 'NONE',  ( 0.08192804256358189596, -0.09851382410610984297, 0.1254088401684838594 ) ) ;
#15363 = DIRECTION ( 'NONE',  ( 0.000000000000000000, 0.000000000000000000, -1.000000000000000000 ) ) ;
#15364 = CARTESIAN_POINT ( 'NONE',  ( 0.7646288533564489232, 0.1113553986120547346, 0.2903543306011346359 ) ) ;
#15365 = EDGE_LOOP ( 'NONE', ( #41480, #13073 ) ) ;
#15366 = EDGE_CURVE ( 'NONE', #45855, #21785, #20631, .T. ) ;
#15367 = EDGE_LOOP ( 'NONE', ( #39727, #43485 ) ) ;
#15368 = EDGE_LOOP ( 'NONE', ( #36075, #6492, #27475, #29725, #5385 ) ) ;
#15369 = ORIENTED_EDGE ( 'NONE', *, *, #21818, .F. ) ;
#15370 = CARTESIAN_POINT ( 'NONE',  ( 0.1787899950787401604, -0.8494094487651332459, -0.07405724077823318263 ) ) ;
#15371 = ( BOUNDED_CURVE ( )  B_SPLINE_CURVE ( 2, ( #15693, #12088, #33206, #3700, #40107, #18324, #84, #332, #14979 ),
 .UNSPECIFIED., .F., .T. ) 
 B_SPLINE_CURVE_WITH_KNOTS ( ( 3, 2, 2, 2, 3 ),
 ( 0.7399999999999999911, 0.7425000000000000488, 0.7449999999999999956, 0.7475000000000000533, 0.7500000000000000000 ),
 .UNSPECIFIED. ) 
 CURVE ( )  GEOMETRIC_REPRESENTATION_ITEM ( )  RATIONAL_B_SPLINE_CURVE ( ( 1.000000000000000000, 0.9238795325112869605, 1.000000000000000000, 0.9238795325112869605, 1.000000000000000000, 0.9238795325112869605, 1.000000000000000000, 0.9238795325112829637, 1.000000000000000000 ) ) 
 REPRESENTATION_ITEM ( '' )  ) ;
#15372 = CARTESIAN_POINT ( 'NONE',  ( 0.1264236179284866091, -1.048720472387181024, 0.1264236179284866091 ) ) ;
#15373 = ORIENTED_EDGE ( 'NONE', *, *, #35190, .T. ) ;
#15374 = CIRCLE ( 'NONE', #29210, 0.1377952755905521298 ) ;
#15375 = DIRECTION ( 'NONE',  ( -3.469446951953613794E-15, -1.000000000000000000, 0.000000000000000000 ) ) ;
#15376 = ( CONVERSION_BASED_UNIT ( 'INCH', #11307 ) LENGTH_UNIT ( ) NAMED_UNIT ( #5666 ) ) ;
#15377 = CARTESIAN_POINT ( 'NONE',  ( 0.6971942568897648851, 0.07405724077823318263, 1.811023621993480548 ) ) ;
#15378 = CARTESIAN_POINT ( 'NONE',  ( 0.1797182628040039087, -0.3381343607641479343, 0.07444174185955046430 ) ) ;
#15379 = LINE ( 'NONE', #40736, #25743 ) ;
#15380 = CARTESIAN_POINT ( 'NONE',  ( 0.1787899950787401604, -0.06692913380450424277, 0.07405724077823318263 ) ) ;
#15381 = CARTESIAN_POINT ( 'NONE',  ( -0.9873396505805591694, 0.1113553986120547346, 1.067913385719243990 ) ) ;
#15382 = EDGE_CURVE ( 'NONE', #6831, #28708, #27159, .T. ) ;
#15383 = CARTESIAN_POINT ( 'NONE',  ( 1.054774247047244540, -0.07405724077823318263, 0.8070866141194653620 ) ) ;
#15384 = ADVANCED_FACE ( 'NONE', ( #7439 ), #3801, .T. ) ;
#15386 = DIRECTION ( 'NONE',  ( 0.000000000000000000, 0.000000000000000000, 1.000000000000000000 ) ) ;
#15385 = LINE ( 'NONE', #41199, #33894 ) ;
#15387 = DIRECTION ( 'NONE',  ( 0.000000000000000000, 0.000000000000000000, 1.000000000000000000 ) ) ;
#15388 = CARTESIAN_POINT ( 'NONE',  ( 0.7185039370078739607, 1.928577636452523993E-17, 0.4625984251968504046 ) ) ;
#15389 = CARTESIAN_POINT ( 'NONE',  ( 1.002407869896990045, 0.1264236179284866091, 1.803641732229700700 ) ) ;
#15390 = AXIS2_PLACEMENT_3D ( 'NONE', #37483, #33921, #26484 ) ;
#15391 = DIRECTION ( 'NONE',  ( 0.000000000000000000, -0.000000000000000000, 1.000000000000000000 ) ) ;
#15392 = EDGE_CURVE ( 'NONE', #7011, #37113, #9496, .T. ) ;
#15393 = CARTESIAN_POINT ( 'NONE',  ( 0.9412147342319837628, -0.1574803149606297803, 0.1205708661417322497 ) ) ;
#15394 = DIRECTION ( 'NONE',  ( 0.000000000000000000, 0.000000000000000000, -1.000000000000000000 ) ) ;
#15395 = CARTESIAN_POINT ( 'NONE',  ( -0.1787899950787401604, -0.3179133857730082058, 0.07405724077823318263 ) ) ;
#15396 = CARTESIAN_POINT ( 'NONE',  ( 0.1600714537641689805, 0.1485828198929401989, 0.02360507234453745537 ) ) ;
#15397 = CARTESIAN_POINT ( 'NONE',  ( -0.1264236179284866091, -1.216043307032850462, 0.1264236179284866091 ) ) ;
#15398 = CARTESIAN_POINT ( 'NONE',  ( 1.002407869896990045, 0.1264236179284866091, 0.1894685038832444879 ) ) ;
#15399 = DIRECTION ( 'NONE',  ( 0.000000000000000000, -0.6156614753256497430, -0.7880107536067285645 ) ) ;
#15400 = CARTESIAN_POINT ( 'NONE',  ( -0.6971942568897648851, -0.07405724077823297447, 1.697834645615527771 ) ) ;
#15401 = ORIENTED_EDGE ( 'NONE', *, *, #27999, .F. ) ;
#15402 = CARTESIAN_POINT ( 'NONE',  ( -0.8019270111902717657, -0.1787899950787401604, 1.353346456639149986 ) ) ;
#15403 = CARTESIAN_POINT ( 'NONE',  ( -0.8759842519685039353, 0.000000000000000000, 0.000000000000000000 ) ) ;
#15404 = CARTESIAN_POINT ( 'NONE',  ( 1.002407869896990045, 0.1264236179284866091, 1.331200787347811110 ) ) ;
#15405 = CARTESIAN_POINT ( 'NONE',  ( 0.7495606340400177148, 0.1264236179284866091, 1.926673228292693052 ) ) ;
#15406 = CARTESIAN_POINT ( 'NONE',  ( -0.8019270111902717657, -0.1787899950787401604, 1.072834645615528659 ) ) ;
#15407 = CARTESIAN_POINT ( 'NONE',  ( -0.1393745452458122480, -0.09844044251944331081, -0.1120857077816562464 ) ) ;
#15408 = CARTESIAN_POINT ( 'NONE',  ( 1.033464566929134687, 0.06523048226347956391, 1.193405511811024278 ) ) ;
#15409 = CARTESIAN_POINT ( 'NONE',  ( 0.6971942568897648851, 0.07405724077823318263, 0.3986220471903311746 ) ) ;
#15410 = CARTESIAN_POINT ( 'NONE',  ( -0.6971942568897648851, -0.07405724077823297447, 0.3592519684501735422 ) ) ;
#15411 = CARTESIAN_POINT ( 'NONE',  ( -1.002407869896990045, 0.1264236179284866091, 0.8538385826234016207 ) ) ;
#15412 = ORIENTED_EDGE ( 'NONE', *, *, #5787, .F. ) ;
#15413 = VECTOR ( 'NONE', #41811, 39.37007874015748143 ) ;
#15414 = CARTESIAN_POINT ( 'NONE',  ( -0.7185039370078739607, 1.928577636452523993E-17, 1.368110236220472675 ) ) ;
#15415 = CARTESIAN_POINT ( 'NONE',  ( -0.8107537697050234415, -0.1574803149606297803, 0.07627952755905517690 ) ) ;
#15416 = CARTESIAN_POINT ( 'NONE',  ( -0.1819224463268279690, -0.09851385391904804445, -0.1710117998103236336 ) ) ;
#15417 = EDGE_LOOP ( 'NONE', ( #17471, #10465, #45672, #45932 ) ) ;
#15418 = VECTOR ( 'NONE', #25103, 39.37007874015748143 ) ;
#15419 = CARTESIAN_POINT ( 'NONE',  ( -0.7185039370078739607, 1.928577636452523993E-17, 1.289370078740157632 ) ) ;
#15420 = CONICAL_SURFACE ( 'NONE', #3142, 0.09842519685039370636, 0.9599310885968824758 ) ;
#15421 = CARTESIAN_POINT ( 'NONE',  ( -1.002407869896990045, -0.1264236179284866091, 0.8882874015210394658 ) ) ;
#15422 = CARTESIAN_POINT ( 'NONE',  ( 0.1559665883013232335, -0.09131739707178367083, -0.1174241798378320850 ) ) ;
#15423 = CYLINDRICAL_SURFACE ( 'NONE', #35163, 0.7874015748031496509 ) ;
#15424 = CARTESIAN_POINT ( 'NONE',  ( 0.07405724077823318263, -1.382013732008767537, 0.1787899950787401604 ) ) ;
#15425 = ORIENTED_EDGE ( 'NONE', *, *, #41756, .F. ) ;
#15426 = CARTESIAN_POINT ( 'NONE',  ( 3.284318927891251994E-17, -0.5024606298674960669, 0.1787899950787401882 ) ) ;
#15427 = ORIENTED_EDGE ( 'NONE', *, *, #40661, .F. ) ;
#15428 = CARTESIAN_POINT ( 'NONE',  ( 0.6971942568897648851, -0.07405724077823297447, 1.146653543253323582 ) ) ;
#15429 = CARTESIAN_POINT ( 'NONE',  ( 0.9412147342319837628, 0.1574803149606300301, 1.592027559055119612 ) ) ;
#15430 = FACE_OUTER_BOUND ( 'NONE', #31986, .T. ) ;
#15431 = CARTESIAN_POINT ( 'NONE',  ( -1.033464566929133799, 0.000000000000000000, 1.427165354330708569 ) ) ;
#15432 = CARTESIAN_POINT ( 'NONE',  ( 1.002407869896990045, 0.1264236179284866091, 0.1845472440407248116 ) ) ;
#15433 = EDGE_CURVE ( 'NONE', #5246, #12477, #40013, .T. ) ;
#15434 = CARTESIAN_POINT ( 'NONE',  ( 0.07405724077823318263, -1.789370078686394194, -0.1787899950787401604 ) ) ;
#15435 = CARTESIAN_POINT ( 'NONE',  ( -0.07405724077823318263, -1.622047244040725866, -0.1787899950787401604 ) ) ;
#15436 = LENGTH_MEASURE_WITH_UNIT ( LENGTH_MEASURE( 0.02539999999999999897 ), #30317 ) ;
#15437 = DIRECTION ( 'NONE',  ( -1.000000000000000000, -0.000000000000000000, 0.000000000000000000 ) ) ;
#15438 = CIRCLE ( 'NONE', #35324, 0.2559055118110236116 ) ;
#15439 = CARTESIAN_POINT ( 'NONE',  ( -0.7495606340400177148, -0.1264236179284866091, 0.7209645668753701386 ) ) ;
#15440 = ADVANCED_FACE ( 'NONE', ( #39773 ), #10096, .T. ) ;
#15442 = CARTESIAN_POINT ( 'NONE',  ( -0.7185039370078739607, 1.928577636452523993E-17, 1.564960629921259949 ) ) ;
#15441 = CARTESIAN_POINT ( 'NONE',  ( 0.06523048226347956391, -0.6845472440944881942, 0.1574803149606297803 ) ) ;
#15443 = CARTESIAN_POINT ( 'NONE',  ( -0.07444174185955065859, -1.410969006433440365, 0.1797182628040039087 ) ) ;
#15444 = FACE_OUTER_BOUND ( 'NONE', #31318, .T. ) ;
#15445 = CARTESIAN_POINT ( 'NONE',  ( 1.928577636452524610E-17, -0.09842519685039370636, -0.1574803149606299191 ) ) ;
#15446 = CARTESIAN_POINT ( 'NONE',  ( 0.8759842519685039353, -0.1787899950787401882, 1.355807086560409491 ) ) ;
#15447 = CARTESIAN_POINT ( 'NONE',  ( 0.9500414927467377701, 0.1787899950787401604, 1.683070866087970074 ) ) ;
#15448 = CARTESIAN_POINT ( 'NONE',  ( 0.9500414927467377701, -0.1787899950787401604, 0.2509842519147403861 ) ) ;
#15449 = CIRCLE ( 'NONE', #10104, 0.1013779527559039162 ) ;
#15450 = VECTOR ( 'NONE', #39879, 39.37007874015748143 ) ;
#15451 = CARTESIAN_POINT ( 'NONE',  ( -1.033464566929133799, 0.000000000000000000, 1.653543306979086580 ) ) ;
#15452 = CARTESIAN_POINT ( 'NONE',  ( -0.7185039370078739607, 1.928577636452523993E-17, 1.525590551181102317 ) ) ;
#15453 = CIRCLE ( 'NONE', #16948, 0.1864803149606299448 ) ;
#15454 = CARTESIAN_POINT ( 'NONE',  ( 0.1968503937007874682, 0.07021257666614930115, -0.1553045758542778432 ) ) ;
#15455 = CARTESIAN_POINT ( 'NONE',  ( -0.7646288533564489232, -0.1113553986120547346, 1.018700787401574770 ) ) ;
#15456 = CARTESIAN_POINT ( 'NONE',  ( 0.7185039370078746268, 0.06523048226347956391, 0.7652559054042838982 ) ) ;
#15457 = CARTESIAN_POINT ( 'NONE',  ( 0.6971942568897637749, 2.189545951927499583E-17, 0.3567913385289137596 ) ) ;
#15458 = CARTESIAN_POINT ( 'NONE',  ( 0.7368992853545974775, -0.09446756238934114758, 0.03937007758462267998 ) ) ;
#15459 = CARTESIAN_POINT ( 'NONE',  ( 0.6971942568897648851, -0.07405724077823297447, 1.225393700733637514 ) ) ;
#15460 = DIRECTION ( 'NONE',  ( 0.000000000000000000, 0.000000000000000000, -1.000000000000000000 ) ) ;
#15461 = DIRECTION ( 'NONE',  ( 0.000000000000000000, -0.7880107536067181284, 0.6156614753256632877 ) ) ;
#15462 = CARTESIAN_POINT ( 'NONE',  ( -0.8759842519685039353, 0.1787899950787401882, 1.291830708607653477 ) ) ;
#15463 = CARTESIAN_POINT ( 'NONE',  ( 0.9412147342319837628, 0.1574803149606300301, 0.5979330707586145710 ) ) ;
#15464 = VERTEX_POINT ( 'NONE', #25440 ) ;
#15465 = CARTESIAN_POINT ( 'NONE',  ( 0.7185039370078739607, 0.000000000000000000, 4.498031496062992574 ) ) ;
#15466 = CARTESIAN_POINT ( 'NONE',  ( -7.957671378281915615E-17, -8.878505979408855953E-16, -0.2933070866141737065 ) ) ;
#15467 = EDGE_LOOP ( 'NONE', ( #35076, #2485, #481, #20634 ) ) ;
#15468 = CARTESIAN_POINT ( 'NONE',  ( -0.1270800023317771588, -0.03547688044918728689, 0.1270800023317771588 ) ) ;
#15469 = CARTESIAN_POINT ( 'NONE',  ( 0.07405724077823318263, -1.292322834591905778, 0.1787899950787401604 ) ) ;
#15470 = LINE ( 'NONE', #19274, #40119 ) ;
#15471 = CARTESIAN_POINT ( 'NONE',  ( -0.7646288533564489232, -0.1113553986120547346, 1.176181102362204633 ) ) ;
#15472 = CARTESIAN_POINT ( 'NONE',  ( 0.7185039370078739607, 1.928577636452523993E-17, 0.5807086614173228023 ) ) ;
#15474 = CARTESIAN_POINT ( 'NONE',  ( -0.7646288533564489232, 0.1113553986120547346, 0.7627952754830236159 ) ) ;
#15473 = CARTESIAN_POINT ( 'NONE',  ( 0.1592537043533252261, -0.09805585504228191140, 0.1110897172141831063 ) ) ;
#15475 = CARTESIAN_POINT ( 'NONE',  ( 1.054774247047244540, 0.07405724077823318263, 0.06889763774151215492 ) ) ;
#15476 = CARTESIAN_POINT ( 'NONE',  ( -0.1264236179284866091, -0.1136811023084411398, 0.1264236179284866091 ) ) ;
#15477 = CARTESIAN_POINT ( 'NONE',  ( 0.8107537697050253289, 0.1574803149606300301, 1.311515747923968744 ) ) ;
#15478 = DIRECTION ( 'NONE',  ( -9.917966281713120965E-31, 1.000000000000000000, -1.406820448837680035E-16 ) ) ;
#15479 = CARTESIAN_POINT ( 'NONE',  ( 1.002407869896990045, -0.1264236179284866091, 0.6914370078202519698 ) ) ;
#15480 = CARTESIAN_POINT ( 'NONE',  ( 1.002407869896990045, -0.1264236179284866091, 0.9276574802611967652 ) ) ;
#15481 = CARTESIAN_POINT ( 'NONE',  ( -0.6971942568897637749, 2.189545951927499583E-17, 1.537893700733637736 ) ) ;
#15482 = CARTESIAN_POINT ( 'NONE',  ( -0.1574803149606297803, -0.09399606288459895487, 0.06523048226347956391 ) ) ;
#15483 = CARTESIAN_POINT ( 'NONE',  ( -0.8019270111902717657, 0.1787899950787401604, 1.220472440891118504 ) ) ;
#15484 = EDGE_LOOP ( 'NONE', ( #5420, #33361, #16884, #26578 ) ) ;
#15485 = CIRCLE ( 'NONE', #26179, 0.09842519685039370636 ) ;
#15486 = VECTOR ( 'NONE', #971, 39.37007874015748143 ) ;
#15487 = CARTESIAN_POINT ( 'NONE',  ( -0.9500414927467378812, 0.1787899950787401604, 0.3494094487651343006 ) ) ;
#15488 = CARTESIAN_POINT ( 'NONE',  ( 0.001106411046829904390, 0.1325885082367477263, -0.04596204078519285086 ) ) ;
#15489 = CARTESIAN_POINT ( 'NONE',  ( 0.7185039370078739607, 1.928577636452523993E-17, 1.683070866141732402 ) ) ;
#15490 = CARTESIAN_POINT ( 'NONE',  ( 3.284318927891251994E-17, -0.9514034957882933075, 0.1787899950787401882 ) ) ;
#15491 = ORIENTED_EDGE ( 'NONE', *, *, #43402, .T. ) ;
#15492 = CARTESIAN_POINT ( 'NONE',  ( 0.1787899950787401604, 0.1003937008411650705, -0.07405724077823318263 ) ) ;
#15493 = ORIENTED_EDGE ( 'NONE', *, *, #38625, .T. ) ;
#15494 = EDGE_CURVE ( 'NONE', #8469, #1467, #38864, .T. ) ;
#15495 = CARTESIAN_POINT ( 'NONE',  ( 0.2362204724409449064, 0.3740157480314960647, 0.9783464566929134243 ) ) ;
#15496 = CIRCLE ( 'NONE', #13209, 0.2431102362204724532 ) ;
#15497 = EDGE_CURVE ( 'NONE', #18901, #10582, #8632, .T. ) ;
#15498 = PLANE ( 'NONE',  #34687 ) ;
#15499 = CARTESIAN_POINT ( 'NONE',  ( -0.7495606340400177148, 0.1264236179284866091, 0.2386811023084413619 ) ) ;
#15500 = CARTESIAN_POINT ( 'NONE',  ( -0.9873396505805591694, -0.1113553986120547346, 0.8316929133858268486 ) ) ;
#15501 = DIRECTION ( 'NONE',  ( -0.000000000000000000, -0.6156614753256605121, -0.7880107536067204599 ) ) ;
#15502 = CARTESIAN_POINT ( 'NONE',  ( -0.3161444924769509779, 2.177585298233989164, -3.731703755406937439 ) ) ;
#15503 = CARTESIAN_POINT ( 'NONE',  ( -0.1797182628040039087, -0.9877406599767465378, -0.07444174185955065859 ) ) ;
#15504 = CARTESIAN_POINT ( 'NONE',  ( 1.033464566929134687, 0.06523048226347956391, 0.4060039370078741827 ) ) ;
#15505 = CARTESIAN_POINT ( 'NONE',  ( -0.8107537697050253289, 0.1574803149606300301, 1.508366141624757129 ) ) ;
#15506 = CARTESIAN_POINT ( 'NONE',  ( 0.7495606340400177148, -0.1264236179284866091, 0.9178149605761574126 ) ) ;
#15507 = CARTESIAN_POINT ( 'NONE',  ( 0.6971942568897648851, -0.07405724077823297447, 1.343503936954111966 ) ) ;
#15508 = CARTESIAN_POINT ( 'NONE',  ( -0.7646288533564489232, 0.1113553986120547346, 0.4576771653543307283 ) ) ;
#15509 = AXIS2_PLACEMENT_3D ( 'NONE', #47255, #36252, #43648 ) ;
#15510 = CARTESIAN_POINT ( 'NONE',  ( 0.7185039370078746268, 0.06523048226347956391, 1.365649606299211838 ) ) ;
#15512 = CARTESIAN_POINT ( 'NONE',  ( 1.033464566929133799, 0.000000000000000000, 1.860236220472440971 ) ) ;
#15511 = CARTESIAN_POINT ( 'NONE',  ( 0.7459936014081097744, -0.1092670104579866602, 1.985467488891498045 ) ) ;
#15513 = CARTESIAN_POINT ( 'NONE',  ( 0.000000000000000000, 1.205361022782826802E-17, -0.09842519685039370636 ) ) ;
#15515 = CARTESIAN_POINT ( 'NONE',  ( 0.1637370714319413278, 0.1604746447930040509, -0.002359686926948953087 ) ) ;
#15514 = CARTESIAN_POINT ( 'NONE',  ( 0.6971942568897648851, 0.07405724077823318263, 0.8661417322297002563 ) ) ;
#15516 = CARTESIAN_POINT ( 'NONE',  ( 1.054774247047244540, 0.07405724077823318263, 1.761811023568284229 ) ) ;
#15517 = CARTESIAN_POINT ( 'NONE',  ( -0.1264236179284866091, -0.7436023621509606496, 0.1264236179284866091 ) ) ;
#15518 = ORIENTED_EDGE ( 'NONE', *, *, #16733, .T. ) ;
#15519 = CARTESIAN_POINT ( 'NONE',  ( 0.9412147342319837628, 0.1574803149606300301, 1.080216535433071501 ) ) ;
#15520 = ( GEOMETRIC_REPRESENTATION_CONTEXT ( 3 ) GLOBAL_UNCERTAINTY_ASSIGNED_CONTEXT ( ( #7724 ) ) GLOBAL_UNIT_ASSIGNED_CONTEXT ( ( #39041, #2614, #2841 ) ) REPRESENTATION_CONTEXT ( 'NONE', 'WORKASPACE' ) ) ;
#15522 = LINE ( 'NONE', #22691, #28260 ) ;
#15521 = VECTOR ( 'NONE', #1932, 39.37007874015748143 ) ;
#15523 = CARTESIAN_POINT ( 'NONE',  ( -0.7646288533564489232, 0.1113553986120547346, 0.1328740156405045225 ) ) ;
#15524 = CARTESIAN_POINT ( 'NONE',  ( 0.8019270111902717657, 0.1787899950787401604, 1.097440944828127041 ) ) ;
#15525 = FACE_OUTER_BOUND ( 'NONE', #39289, .T. ) ;
#15526 = CARTESIAN_POINT ( 'NONE',  ( -0.1574803149606297803, -1.678641732283464583, 0.06523048226347956391 ) ) ;
#15527 = FACE_OUTER_BOUND ( 'NONE', #20527, .T. ) ;
#15528 = ORIENTED_EDGE ( 'NONE', *, *, #39349, .T. ) ;
#15529 = CARTESIAN_POINT ( 'NONE',  ( 0.1555687797274982465, -0.1458529223346498038, -0.02296587926509181116 ) ) ;
#15530 = CARTESIAN_POINT ( 'NONE',  ( -0.6971942568897626646, -0.07405724077823297447, 0.2805118109698587214 ) ) ;
#15531 = VERTEX_POINT ( 'NONE', #24706 ) ;
#15533 = ORIENTED_EDGE ( 'NONE', *, *, #23850, .F. ) ;
#15532 = MECHANICAL_DESIGN_GEOMETRIC_PRESENTATION_REPRESENTATION (  '', ( #23184 ), #18587 ) ;
#15534 = CARTESIAN_POINT ( 'NONE',  ( -0.8759842519685039353, -0.1574803149606299191, 0.7086614173228346081 ) ) ;
#15535 = ORIENTED_EDGE ( 'NONE', *, *, #19757, .T. ) ;
#15536 = CARTESIAN_POINT ( 'NONE',  ( 0.1787899950787401604, -1.597440944828127485, -0.07405724077823318263 ) ) ;
#15537 = CARTESIAN_POINT ( 'NONE',  ( -0.8019270111902717657, -0.1787899950787401604, 1.781496062938362934 ) ) ;
#15538 = CARTESIAN_POINT ( 'NONE',  ( -0.6971942568897648851, -0.07405724077823297447, 0.9498031495525356416 ) ) ;
#15539 = CARTESIAN_POINT ( 'NONE',  ( -0.6971942568897626646, -0.07405724077823297447, 0.5610236219934807700 ) ) ;
#15540 = CARTESIAN_POINT ( 'NONE',  ( -1.033464566929133799, 0.000000000000000000, 0.1673228346456692994 ) ) ;
#15541 = DIRECTION ( 'NONE',  ( 0.000000000000000000, -1.000000000000000000, 0.000000000000000000 ) ) ;
#15542 = CARTESIAN_POINT ( 'NONE',  ( -0.8107537697050254399, 0.1574803149606300301, 1.675688976377952999 ) ) ;
#15543 = CARTESIAN_POINT ( 'NONE',  ( -0.1264236179284866091, -0.6118365666544350878, -0.1264236179284866091 ) ) ;
#15544 = CARTESIAN_POINT ( 'NONE',  ( 0.03780438559997598841, -0.08956001823431022912, 0.2156824087300551196 ) ) ;
#15545 = CARTESIAN_POINT ( 'NONE',  ( 0.7185039370078746268, 0.06523048226347956391, 1.798720472440944240 ) ) ;
#15546 = EDGE_CURVE ( 'NONE', #11723, #42642, #22170, .T. ) ;
#15547 = CARTESIAN_POINT ( 'NONE',  ( 0.2559054473914413874, -0.04584745133446761767, -0.03612980868771894366 ) ) ;
#15548 = CARTESIAN_POINT ( 'NONE',  ( -1.054774247047244096, 0.000000000000000000, 0.3371062991588349989 ) ) ;
#15549 = CARTESIAN_POINT ( 'NONE',  ( 0.7185039370078739607, 1.928577636452523993E-17, 1.200787401467275695 ) ) ;
#15550 = EDGE_CURVE ( 'NONE', #33336, #22445, #14640, .T. ) ;
#15551 = AXIS2_PLACEMENT_3D ( 'NONE', #8426, #34330, #26437 ) ;
#15552 = ORIENTED_EDGE ( 'NONE', *, *, #45320, .T. ) ;
#15553 = CARTESIAN_POINT ( 'NONE',  ( 0.1574803149606299191, 0.6241017553149685870, 0.3240160679609074834 ) ) ;
#15554 = ADVANCED_FACE ( 'NONE', ( #43616 ), #34438, .F. ) ;
#15555 = CARTESIAN_POINT ( 'NONE',  ( -0.9500414927467377701, 0.1787899950787401604, 1.491141732229701145 ) ) ;
#15556 = ORIENTED_EDGE ( 'NONE', *, *, #19453, .F. ) ;
#15557 = PRODUCT_DEFINITION_FORMATION_WITH_SPECIFIED_SOURCE ( 'ANY', '', #19185, .NOT_KNOWN. ) ;
#15558 = AXIS2_PLACEMENT_3D ( 'NONE', #38599, #5058, #5532 ) ;
#15559 = ADVANCED_FACE ( 'NONE', ( #10342 ), #10589, .T. ) ;
#15560 = CARTESIAN_POINT ( 'NONE',  ( 0.1264236179284866091, -1.368602362150960650, 0.1264236179284866091 ) ) ;
#15561 = CARTESIAN_POINT ( 'NONE',  ( 0.1787899950787401604, -1.518700787347811554, 0.07405724077823318263 ) ) ;
#15562 = SURFACE_STYLE_FILL_AREA ( #1856 ) ;
#15563 = CARTESIAN_POINT ( 'NONE',  ( 0.1498753904841986506, 0.1193342091828952928, 0.06889763779527559306 ) ) ;
#15564 = CARTESIAN_POINT ( 'NONE',  ( 0.8759842519685039353, -0.1574803149606299191, 0.4330708661417322913 ) ) ;
#15565 = DIRECTION ( 'NONE',  ( 1.000000000000000000, 0.000000000000000000, 0.000000000000000000 ) ) ;
#15566 = CARTESIAN_POINT ( 'NONE',  ( -0.9873396505805591694, 0.1113553986120547346, 1.146653543199559033 ) ) ;
#15567 = CARTESIAN_POINT ( 'NONE',  ( 0.8759842519685039353, 0.1787899950787401882, 0.5880905511273386566 ) ) ;
#15568 = CARTESIAN_POINT ( 'NONE',  ( 0.6971942568897644410, 0.03556354196195587319, 0.04064907242275180022 ) ) ;
#15570 = CARTESIAN_POINT ( 'NONE',  ( -0.1184675242425147629, -0.09842519685039370636, 1.870565676741754668 ) ) ;
#15569 = CARTESIAN_POINT ( 'NONE',  ( -0.1113553986120547346, -0.2982283464566929387, 0.1113553986120547346 ) ) ;
#15571 = CARTESIAN_POINT ( 'NONE',  ( 0.7185039370078739607, 1.928577636452523993E-17, 1.948818897530267602 ) ) ;
#15572 = ORIENTED_EDGE ( 'NONE', *, *, #18368, .F. ) ;
#15573 = CARTESIAN_POINT ( 'NONE',  ( 0.1476377952755906220, 0.3743908788525356912, -3.616772362661642148 ) ) ;
#15574 = CARTESIAN_POINT ( 'NONE',  ( -0.8759842519685039353, -0.1787899950787401882, 1.001476377898992132 ) ) ;
#15575 = CARTESIAN_POINT ( 'NONE',  ( 0.8759842519685039353, -0.1574803149606299191, 0.9842519685039370358 ) ) ;
#15576 = DIRECTION ( 'NONE',  ( 0.000000000000000000, -0.000000000000000000, 1.000000000000000000 ) ) ;
#15577 = CARTESIAN_POINT ( 'NONE',  ( 0.1574803149606299191, -0.5492125983176693316, -1.928577636452523993E-17 ) ) ;
#15578 = CARTESIAN_POINT ( 'NONE',  ( -1.181102362204724310, -0.3937007874015748254, 0.9842519685039370358 ) ) ;
#15579 = CARTESIAN_POINT ( 'NONE',  ( -0.1217943169637149825, -0.08954727061951725520, 0.1064691133493027853 ) ) ;
#15580 = ORIENTED_EDGE ( 'NONE', *, *, #17261, .T. ) ;
#15581 = CARTESIAN_POINT ( 'NONE',  ( 0.1608809399420511876, -0.08280523680090119687, -0.1377952755905511861 ) ) ;
#15582 = CARTESIAN_POINT ( 'NONE',  ( 0.4028871391076110364, 0.08090551181102362266, 0.000000000000000000 ) ) ;
#15583 = CARTESIAN_POINT ( 'NONE',  ( -0.1113553986120547346, -0.03248031496062991907, -0.1113553986120547346 ) ) ;
#15584 = CARTESIAN_POINT ( 'NONE',  ( 0.1787899950787401604, -1.597440944828127485, 0.07405724077823318263 ) ) ;
#15585 = CARTESIAN_POINT ( 'NONE',  ( 0.1787899950787401604, -0.8543307086076546986, 0.07405724077823318263 ) ) ;
#15586 = CARTESIAN_POINT ( 'NONE',  ( -0.1574803149606300301, -1.211122047244094002, -0.06523048226347956391 ) ) ;
#15587 = CARTESIAN_POINT ( 'NONE',  ( 0.7646288533564489232, -0.1113553986120547346, 1.126968503829480328 ) ) ;
#15588 = CARTESIAN_POINT ( 'NONE',  ( -0.7185039370078766252, -0.06523048226348168721, 1.646161417322834497 ) ) ;
#15589 = ORIENTED_EDGE ( 'NONE', *, *, #19950, .T. ) ;
#15590 = EDGE_LOOP ( 'NONE', ( #21468, #14643, #35548, #36815 ) ) ;
#15591 = CARTESIAN_POINT ( 'NONE',  ( -0.8019270111902717657, 0.1787899950787401604, 1.692913385773008539 ) ) ;
#15592 = CARTESIAN_POINT ( 'NONE',  ( -0.7646288533564489232, 0.1113553986120547346, 0.6545275590551181688 ) ) ;
#15593 = CARTESIAN_POINT ( 'NONE',  ( 1.002407869896990045, 0.1264236179284866091, 1.685531496009228469 ) ) ;
#15594 = CARTESIAN_POINT ( 'NONE',  ( 0.1574803149606300301, -1.299704724301920855, 0.06523048226347956391 ) ) ;
#15596 = CARTESIAN_POINT ( 'NONE',  ( 0.7646288533564489232, 0.1113553986120547346, 1.471456692805858113 ) ) ;
#15595 = CIRCLE ( 'NONE', #42341, 0.3100393700787401619 ) ;
#15597 = CARTESIAN_POINT ( 'NONE',  ( 0.6971942568897626646, -0.07405724077823297447, 0.2854330708123783422 ) ) ;
#15598 = CARTESIAN_POINT ( 'NONE',  ( -1.054774247047244540, 0.07405724077823318263, 1.441929133804504604 ) ) ;
#15599 = CARTESIAN_POINT ( 'NONE',  ( 1.033464566929133799, 0.000000000000000000, 1.259842519577511810 ) ) ;
#15600 = CARTESIAN_POINT ( 'NONE',  ( -0.8759842519685039353, 0.1787899950787401882, 1.173720472387181246 ) ) ;
#15601 = CARTESIAN_POINT ( 'NONE',  ( -0.6971942568897637749, 2.189545951927499583E-17, 0.08612204719033110523 ) ) ;
#15602 = CARTESIAN_POINT ( 'NONE',  ( 0.000000000000000000, 0.000000000000000000, -0.3149606299212598381 ) ) ;
#15603 = CARTESIAN_POINT ( 'NONE',  ( -0.7495606340400177148, -0.1264236179284866091, 1.587106299158834721 ) ) ;
#15604 = CARTESIAN_POINT ( 'NONE',  ( -0.6971942568897626646, 0.07405724077823318263, 0.08366141726907129483 ) ) ;
#15605 = CARTESIAN_POINT ( 'NONE',  ( -0.8107537697050253289, 0.1574803149606300301, 1.596948818897636402 ) ) ;
#15606 = CARTESIAN_POINT ( 'NONE',  ( 0.7646288533564489232, 0.1113553986120547346, 1.638779527559055316 ) ) ;
#15607 = CARTESIAN_POINT ( 'NONE',  ( 1.002407869896990045, -0.1264236179284866091, 1.596948818843874074 ) ) ;
#15608 = CARTESIAN_POINT ( 'NONE',  ( -0.1818951543555252237, -0.09842519685039370636, -0.1709882076668135797 ) ) ;
#15609 = DIRECTION ( 'NONE',  ( -1.000000000000000000, 0.000000000000000000, 0.000000000000000000 ) ) ;
#15610 = CARTESIAN_POINT ( 'NONE',  ( -0.2559125663627066505, 0.04383012413643278676, -0.3128473781736403891 ) ) ;
#15611 = ORIENTED_EDGE ( 'NONE', *, *, #20592, .F. ) ;
#15612 = EDGE_CURVE ( 'NONE', #11278, #43605, #35967, .T. ) ;
#15613 = ORIENTED_EDGE ( 'NONE', *, *, #44105, .T. ) ;
#15614 = ORIENTED_EDGE ( 'NONE', *, *, #18938, .T. ) ;
#15615 = ADVANCED_FACE ( 'NONE', ( #4292 ), #33113, .T. ) ;
#15616 = CARTESIAN_POINT ( 'NONE',  ( -0.1264236179284866091, -0.9060039369541103005, 0.1264236179284866091 ) ) ;
#15617 = CARTESIAN_POINT ( 'NONE',  ( 0.1787899950787401882, -1.083169291284818980, -2.189545951927503898E-17 ) ) ;
#15618 = ORIENTED_EDGE ( 'NONE', *, *, #13674, .T. ) ;
#15619 = CARTESIAN_POINT ( 'NONE',  ( 0.6195511811023619586, 0.8070866141732275789, 0.5854071585544579071 ) ) ;
#15620 = CARTESIAN_POINT ( 'NONE',  ( 1.002407869896990045, 0.1264236179284866091, 1.838090551127338657 ) ) ;
#15621 = CARTESIAN_POINT ( 'NONE',  ( -0.1797182628040039365, -0.3947288489531244338, 0.000000000000000000 ) ) ;
#15622 = CARTESIAN_POINT ( 'NONE',  ( 0.1377952755905511861, 0.1574803149606299191, 0.8070866141732283561 ) ) ;
#15623 = VECTOR ( 'NONE', #7870, 39.37007874015748143 ) ;
#15624 = CARTESIAN_POINT ( 'NONE',  ( -0.8759842519685039353, 0.1574803149606299191, 1.072834645561763889 ) ) ;
#15625 = CARTESIAN_POINT ( 'NONE',  ( 1.002407869896990045, -0.1264236179284866091, 0.8046259841982047467 ) ) ;
#15627 = CARTESIAN_POINT ( 'NONE',  ( -0.8759842491179902213, 0.1574803149606299191, 1.978346456692913646 ) ) ;
#15626 = CARTESIAN_POINT ( 'NONE',  ( 0.04075098337900059237, 0.2719666410387984179, -0.06815351164857791355 ) ) ;
#15628 = CARTESIAN_POINT ( 'NONE',  ( -0.1574803149606299191, 0.5257908685547681982, -0.4487896632427120225 ) ) ;
#15629 = VECTOR ( 'NONE', #37392, 39.37007874015748143 ) ;
#15630 = CARTESIAN_POINT ( 'NONE',  ( 0.7646288533564489232, -0.1113553986120547346, 1.254921259842519676 ) ) ;
#15631 = CARTESIAN_POINT ( 'NONE',  ( 1.054774247047244096, 0.000000000000000000, 1.759350393647023614 ) ) ;
#15632 = CARTESIAN_POINT ( 'NONE',  ( 0.9412147342319837628, 0.1574803149606300301, 0.05659448818897635375 ) ) ;
#15633 = CARTESIAN_POINT ( 'NONE',  ( 0.000000000000000000, 0.3883517482604934012, -0.6419475548153109612 ) ) ;
#15634 = CARTESIAN_POINT ( 'NONE',  ( 0.07405724077823318263, -0.3720472440407247561, -0.1787899950787401604 ) ) ;
#15635 = PLANE ( 'NONE',  #21697 ) ;
#15636 = ADVANCED_FACE ( 'NONE', ( #23009 ), #33823, .T. ) ;
#15637 = CARTESIAN_POINT ( 'NONE',  ( 0.1264236179284866091, -1.206200787347811110, 0.1264236179284866091 ) ) ;
#15638 = CARTESIAN_POINT ( 'NONE',  ( 1.054774247047244540, -0.07405724077823318263, 0.2608267715997796832 ) ) ;
#15639 = ( BOUNDED_CURVE ( )  B_SPLINE_CURVE ( 2, ( #34249, #1865, #1147, #37832, #41144, #31131, #16037, #16501, #44753 ),
 .UNSPECIFIED., .F., .T. ) 
 B_SPLINE_CURVE_WITH_KNOTS ( ( 3, 2, 2, 2, 3 ),
 ( 0.8699999999999999956, 0.8725000000000000533, 0.8750000000000000000, 0.8774999999999999467, 0.8800000000000000044 ),
 .UNSPECIFIED. ) 
 CURVE ( )  GEOMETRIC_REPRESENTATION_ITEM ( )  RATIONAL_B_SPLINE_CURVE ( ( 1.000000000000000000, 0.9238795325112899581, 1.000000000000000000, 0.9238795325112869605, 1.000000000000000000, 0.9238795325112869605, 1.000000000000000000, 0.9238795325112869605, 1.000000000000000000 ) ) 
 REPRESENTATION_ITEM ( '' )  ) ;
#15640 = CARTESIAN_POINT ( 'NONE',  ( 0.7185039370078746268, 0.06523048226347956391, 0.06643700787401589369 ) ) ;
#15641 = CARTESIAN_POINT ( 'NONE',  ( -1.002407869896990045, 0.1264236179284866091, 1.719980314906866203 ) ) ;
#15642 = EDGE_LOOP ( 'NONE', ( #19926, #29287, #34158, #37432 ) ) ;
#15643 = CARTESIAN_POINT ( 'NONE',  ( -0.8759842519685039353, -0.1787899950787401882, 1.316437007820252081 ) ) ;
#15644 = CARTESIAN_POINT ( 'NONE',  ( 1.033464566929134687, -0.06523048226347956391, 1.031003937007875182 ) ) ;
#15645 = B_SPLINE_CURVE_WITH_KNOTS ( 'NONE', 3,
 ( #16790, #38359, #2858, #17495, #5530, #20145 ),
 .UNSPECIFIED., .F., .F.,
 ( 4, 2, 4 ),
 ( 0.000000000000000000, 0.5000000000000000000, 1.000000000000000000 ),
 .UNSPECIFIED. ) ;
#15646 = CARTESIAN_POINT ( 'NONE',  ( 0.8019270111902717657, 0.1787899950787401604, 1.963582677111591401 ) ) ;
#15647 = CARTESIAN_POINT ( 'NONE',  ( -1.002407869896990045, 0.1264236179284866091, 1.090059055064346527 ) ) ;
#15648 = CARTESIAN_POINT ( 'NONE',  ( 0.7185039370078739607, 1.928577636452523993E-17, 0.6496062991050708391 ) ) ;
#15649 = CARTESIAN_POINT ( 'NONE',  ( -0.1230701032824740720, -0.09842685872290869720, -0.1297086761450524928 ) ) ;
#15650 = CARTESIAN_POINT ( 'NONE',  ( -1.033464566929134687, 0.06523048226347956391, 1.341043306979086358 ) ) ;
#15651 = CARTESIAN_POINT ( 'NONE',  ( 0.7495606340400177148, -0.1264236179284866091, 0.5241141731745827537 ) ) ;
#15652 = CARTESIAN_POINT ( 'NONE',  ( -0.8019270111902716547, -0.1787899950787401604, 0.3248031495525355861 ) ) ;
#15653 = ORIENTED_EDGE ( 'NONE', *, *, #43594, .T. ) ;
#15654 = CARTESIAN_POINT ( 'NONE',  ( 0.2383973256948909436, -0.5708661417322835607, 1.112073044918588494 ) ) ;
#15655 = ORIENTED_EDGE ( 'NONE', *, *, #40139, .F. ) ;
#15656 = CARTESIAN_POINT ( 'NONE',  ( -0.9412147342319837628, -0.1574803149606297803, 0.1599409448818898405 ) ) ;
#15657 = CARTESIAN_POINT ( 'NONE',  ( 0.9500414927467377701, 0.1787899950787401604, 1.136811023568283119 ) ) ;
#15658 = CARTESIAN_POINT ( 'NONE',  ( -0.09073039027163543047, -0.09851385255785906347, -0.2376265320636606060 ) ) ;
#15659 = VERTEX_POINT ( 'NONE', #34057 ) ;
#15660 = CYLINDRICAL_SURFACE ( 'NONE', #45476, 0.1787899950787401049 ) ;
#15661 = ( BOUNDED_SURFACE ( )  B_SPLINE_SURFACE ( 3, 2, ( 
 ( #4216, #394, #40865 ),
 ( #15046, #29696, #44237 ),
 ( #11442, #26059, #26309 ),
 ( #40629, #7827, #18845 ),
 ( #33747, #8061, #37290 ),
 ( #856, #15515, #23874 ) ),
 .UNSPECIFIED., .F., .F., .T. ) 
 B_SPLINE_SURFACE_WITH_KNOTS ( ( 4, 2, 4 ),
 ( 3, 3 ),
 ( 0.01651999345535504898, 0.01858032176739835006, 0.02064065007944164767 ),
 ( 0.000000000000000000, 1.000000000000000000 ),
 .UNSPECIFIED. ) 
 GEOMETRIC_REPRESENTATION_ITEM ( )  RATIONAL_B_SPLINE_SURFACE ( (
 ( 1.000000000000000000, 0.8047781103519390244, 1.000000000000000000),
 ( 1.000000000000000000, 0.8123785825606629762, 1.000000000000000000),
 ( 1.000000000000000000, 0.8190671539785250310, 1.000000000000000000),
 ( 1.000000000000000000, 0.8192352254837930170, 1.000000000000000000),
 ( 1.000000000000000000, 0.8126129677209299462, 1.000000000000000000),
 ( 1.000000000000000000, 0.8047712537969730073, 1.000000000000000000) ) ) 
 REPRESENTATION_ITEM ( '' )  SURFACE ( )  ) ;
#15662 = EDGE_CURVE ( 'NONE', #25448, #18659, #20537, .T. ) ;
#15663 = CARTESIAN_POINT ( 'NONE',  ( -0.9873396505805591694, 0.1113553986120547346, 1.461614173120818760 ) ) ;
#15664 = CARTESIAN_POINT ( 'NONE',  ( -0.8019270111902717657, -0.1787899950787401604, 0.04921259837143338034 ) ) ;
#15665 = CARTESIAN_POINT ( 'NONE',  ( -0.07405724077823318263, -1.505045228071758778, 0.1787899950787401604 ) ) ;
#15666 = AXIS2_PLACEMENT_3D ( 'NONE', #23026, #34304, #23514 ) ;
#15667 = ORIENTED_EDGE ( 'NONE', *, *, #1913, .T. ) ;
#15668 = CARTESIAN_POINT ( 'NONE',  ( -0.1787899950787401882, -0.3941929133320630219, 0.000000000000000000 ) ) ;
#15669 = CARTESIAN_POINT ( 'NONE',  ( -0.2559061023261890999, 0.06403729604667574016, -0.3104221027878572570 ) ) ;
#15670 = CARTESIAN_POINT ( 'NONE',  ( -0.2611872605799124836, -0.1670510767787602990, 0.8870424230945959110 ) ) ;
#15671 = EDGE_LOOP ( 'NONE', ( #35774, #9404, #30807, #36200, #17262, #41632 ) ) ;
#15672 = EDGE_CURVE ( 'NONE', #19219, #6112, #19138, .T. ) ;
#15673 = FACE_OUTER_BOUND ( 'NONE', #46744, .T. ) ;
#15674 = CARTESIAN_POINT ( 'NONE',  ( 1.614954907737318939E-16, 0.1574803149606340824, 0.3937007874015748254 ) ) ;
#15675 = CARTESIAN_POINT ( 'NONE',  ( -0.4330708661417322913, 0.1574803149606299191, 1.186023622047243986 ) ) ;
#15676 = CARTESIAN_POINT ( 'NONE',  ( 0.6971942568897648851, 0.07405724077823318263, 1.653543307032850462 ) ) ;
#15677 = CARTESIAN_POINT ( 'NONE',  ( 0.8019270111902717657, 0.1787899950787401604, 0.2312992125446618197 ) ) ;
#15678 = CARTESIAN_POINT ( 'NONE',  ( 0.1787899950787401882, 0.1214311498809974438, -2.189545951927503898E-17 ) ) ;
#15679 = DIRECTION ( 'NONE',  ( 0.7301731215444999812, 0.000000000000000000, 0.6832621843582160626 ) ) ;
#15680 = FACE_OUTER_BOUND ( 'NONE', #5084, .T. ) ;
#15682 = VERTEX_POINT ( 'NONE', #697 ) ;
#15681 = CIRCLE ( 'NONE', #21789, 0.02900000000000001882 ) ;
#15683 = CARTESIAN_POINT ( 'NONE',  ( -1.002407869896990045, -0.1264236179284866091, 0.5733267715997795166 ) ) ;
#15685 = CARTESIAN_POINT ( 'NONE',  ( 1.033464566929133799, 0.000000000000000000, 0.3641732283464567121 ) ) ;
#15684 = CARTESIAN_POINT ( 'NONE',  ( -0.1574803149606300301, -0.7386811023622060768, -0.06523048226347956391 ) ) ;
#15686 = CARTESIAN_POINT ( 'NONE',  ( 0.1797182628040039087, -1.356835148165722371, -0.07444174185955065859 ) ) ;
#15687 = LINE ( 'NONE', #1499, #37080 ) ;
#15688 = CARTESIAN_POINT ( 'NONE',  ( 0.1476377952755906220, 1.117014023967195735, -3.442880580079816788 ) ) ;
#15689 = CARTESIAN_POINT ( 'NONE',  ( 1.054774247047244096, 0.000000000000000000, 1.326279527505291433 ) ) ;
#15690 = CARTESIAN_POINT ( 'NONE',  ( 0.7495606340400177148, -0.1264236179284866091, 1.897145669237574772 ) ) ;
#15691 = AXIS2_PLACEMENT_3D ( 'NONE', #36128, #29226, #145 ) ;
#15692 = AXIS2_PLACEMENT_3D ( 'NONE', #23339, #22619, #11613 ) ;
#15694 = ORIENTED_EDGE ( 'NONE', *, *, #30183, .T. ) ;
#15693 = CARTESIAN_POINT ( 'NONE',  ( 1.033464566929133799, 0.000000000000000000, 1.496062992018456494 ) ) ;
#15695 = DIRECTION ( 'NONE',  ( 0.000000000000000000, 0.000000000000000000, -1.000000000000000000 ) ) ;
#15696 = DIRECTION ( 'NONE',  ( 0.000000000000000000, -1.000000000000000000, 0.000000000000000000 ) ) ;
#15697 = CARTESIAN_POINT ( 'NONE',  ( -0.1264236179284866091, 0.1176181102899840625, 0.1264236179284866091 ) ) ;
#15698 = CARTESIAN_POINT ( 'NONE',  ( -0.7646288533564489232, 0.1113553986120547346, 1.235236220364913207 ) ) ;
#15699 = CARTESIAN_POINT ( 'NONE',  ( 0.8759842519685039353, -0.1787899950787401882, 0.2485236219934806867 ) ) ;
#15700 = EDGE_CURVE ( 'NONE', #16187, #10690, #22285, .T. ) ;
#15701 = CARTESIAN_POINT ( 'NONE',  ( -0.1567662409572586624, 1.924205194239609999E-17, -0.0004999999999998990712 ) ) ;
#15702 = FACE_OUTER_BOUND ( 'NONE', #22126, .T. ) ;
#15703 = CARTESIAN_POINT ( 'NONE',  ( -1.054774247047244540, 0.07405724077823318263, 1.323818897584032817 ) ) ;
#15704 = CARTESIAN_POINT ( 'NONE',  ( 0.9873396505805591694, -0.1113553986120547346, 0.7037401573727875004 ) ) ;
#15705 = ORIENTED_EDGE ( 'NONE', *, *, #1123, .F. ) ;
#15706 = CARTESIAN_POINT ( 'NONE',  ( -0.9412147342319837628, 0.1574803149606300301, 1.749507874015747699 ) ) ;
#15707 = DIRECTION ( 'NONE',  ( -0.8191520442889947962, 0.4519843998600418522, -0.3531289150159164225 ) ) ;
#15708 = ORIENTED_EDGE ( 'NONE', *, *, #18654, .F. ) ;
#15709 = CARTESIAN_POINT ( 'NONE',  ( 0.07444174185955046430, -0.01333121115784871406, -0.1797182628040039087 ) ) ;
#15711 = CARTESIAN_POINT ( 'NONE',  ( 0.07405724077823318263, -1.159448818843874074, -0.1787899950787401604 ) ) ;
#15710 = CARTESIAN_POINT ( 'NONE',  ( 0.1113553986120547346, -1.056102362097196989, -0.1113553986120547346 ) ) ;
#15712 = CARTESIAN_POINT ( 'NONE',  ( -1.033464566929133799, 0.000000000000000000, 0.7972440944881890035 ) ) ;
#15713 = CARTESIAN_POINT ( 'NONE',  ( 0.6971942568897637749, 2.189545951927499583E-17, 1.537893700733637736 ) ) ;
#15714 = CARTESIAN_POINT ( 'NONE',  ( -0.8107537697050253289, 0.1574803149606300301, 1.242618110236220819 ) ) ;
#15715 = CARTESIAN_POINT ( 'NONE',  ( 0.7646288533564489232, 0.1113553986120547346, 0.5757874015748032370 ) ) ;
#15717 = CARTESIAN_POINT ( 'NONE',  ( 0.4399002236966062518, 0.8539303365987028771, -1.004656681308842447 ) ) ;
#15716 = DIRECTION ( 'NONE',  ( 0.000000000000000000, 0.000000000000000000, -1.000000000000000000 ) ) ;
#15718 = CARTESIAN_POINT ( 'NONE',  ( 0.5660731898098425585, 4.766607801171850497E-17, 0.000000000000000000 ) ) ;
#15719 = ORIENTED_EDGE ( 'NONE', *, *, #19544, .T. ) ;
#15720 = CARTESIAN_POINT ( 'NONE',  ( -0.2471922904502826812, -0.09842519685039370636, -0.1427165354330708902 ) ) ;
#15721 = ADVANCED_FACE ( 'NONE', ( #33347 ), #26861, .F. ) ;
#15722 = CARTESIAN_POINT ( 'NONE',  ( -0.8019270111902716547, -0.1787899950787401604, 1.545275590497419138 ) ) ;
#15723 = CARTESIAN_POINT ( 'NONE',  ( -0.06523048226347956391, -0.04970472430192178492, 0.1574803149606297803 ) ) ;
#15724 = CARTESIAN_POINT ( 'NONE',  ( -1.002407869896990045, 0.1264236179284866091, 1.331200787347811110 ) ) ;
#15725 = EDGE_CURVE ( 'NONE', #27223, #13283, #13026, .T. ) ;
#15726 = ORIENTED_EDGE ( 'NONE', *, *, #41511, .F. ) ;
#15727 = ADVANCED_FACE ( 'NONE', ( #30005 ), #5377, .T. ) ;
#15728 = CARTESIAN_POINT ( 'NONE',  ( -1.054774247047244540, -0.07405724077823318263, 0.3001968503399373711 ) ) ;
#15729 = DIRECTION ( 'NONE',  ( 0.000000000000000000, 0.000000000000000000, -1.000000000000000000 ) ) ;
#15730 = VECTOR ( 'NONE', #45030, 39.37007874015748143 ) ;
#15731 = DIRECTION ( 'NONE',  ( 0.000000000000000000, 1.000000000000000000, 0.000000000000000000 ) ) ;
#15732 = CARTESIAN_POINT ( 'NONE',  ( 0.1264236179284866091, -1.015379873741049099, -0.1264236179284866091 ) ) ;
#15733 = ORIENTED_EDGE ( 'NONE', *, *, #42258, .F. ) ;
#15734 = CARTESIAN_POINT ( 'NONE',  ( -0.1264236179284866091, 0.004429133912031228346, 0.1264236179284866091 ) ) ;
#15735 = ORIENTED_EDGE ( 'NONE', *, *, #16611, .F. ) ;
#15736 = CIRCLE ( 'NONE', #3457, 0.1013779527559055538 ) ;
#15737 = AXIS2_PLACEMENT_3D ( 'NONE', #29450, #136, #11427 ) ;
#15738 = ORIENTED_EDGE ( 'NONE', *, *, #14434, .T. ) ;
#15739 = ADVANCED_FACE ( 'NONE', ( #36682 ), #29770, .T. ) ;
#15740 = DIRECTION ( 'NONE',  ( 0.000000000000000000, 0.000000000000000000, -1.000000000000000000 ) ) ;
#15741 = CARTESIAN_POINT ( 'NONE',  ( 0.000000000000000000, 0.09842519685039370636, 0.000000000000000000 ) ) ;
#15742 = CARTESIAN_POINT ( 'NONE',  ( -0.07405724077823318263, -0.5492125983714331028, 0.1787899950787401604 ) ) ;
#15743 = CARTESIAN_POINT ( 'NONE',  ( -0.9500414927467377701, -0.1787899950787401604, 0.2165354330171024577 ) ) ;
#15744 = CARTESIAN_POINT ( 'NONE',  ( -1.033464566929134687, -0.06523048226347956391, 0.8735236220472449853 ) ) ;
#15745 = CARTESIAN_POINT ( 'NONE',  ( -0.07444174185955065859, -0.9532918410791076935, -0.1797182628040039087 ) ) ;
#15746 = CARTESIAN_POINT ( 'NONE',  ( 0.1502195169528062479, 0.1299212598425197041, -0.07817644135598977861 ) ) ;
#15747 = CARTESIAN_POINT ( 'NONE',  ( -1.033464566929134687, -0.06523048226347956391, 1.572342519577513142 ) ) ;
#15748 = CARTESIAN_POINT ( 'NONE',  ( 0.8759842519685039353, -0.1787899950787401882, 0.9227362204186770889 ) ) ;
#15749 = CARTESIAN_POINT ( 'NONE',  ( -1.033464566929133799, 0.000000000000000000, 0.4429133858267716439 ) ) ;
#15750 = CARTESIAN_POINT ( 'NONE',  ( 0.7646288533564489232, 0.1113553986120547346, 1.520669291338582640 ) ) ;
#15752 = CARTESIAN_POINT ( 'NONE',  ( -0.1377952755905511861, 1.808041534174241898E-17, -0.2886241641379866385 ) ) ;
#15751 = CARTESIAN_POINT ( 'NONE',  ( 0.7440012176947153888, -0.1067469361137101808, 1.985406665012090510 ) ) ;
#15753 = CARTESIAN_POINT ( 'NONE',  ( 0.7185039370078739607, 1.928577636452523993E-17, 1.870078740049952559 ) ) ;
#15754 = CARTESIAN_POINT ( 'NONE',  ( -0.06523048226347956391, -0.6943897636720013367, -0.1574803149606300301 ) ) ;
#15755 = CARTESIAN_POINT ( 'NONE',  ( 0.1787899950787401604, 0.1003937008411650705, -0.07405724077823318263 ) ) ;
#15756 = CARTESIAN_POINT ( 'NONE',  ( -0.2066929133858267931, 0.04819563354825918966, -0.1381030546566545669 ) ) ;
#15757 = CARTESIAN_POINT ( 'NONE',  ( 1.002407869896990045, -0.1264236179284866091, 0.8439960629383622681 ) ) ;
#15758 = CARTESIAN_POINT ( 'NONE',  ( 0.6971942568897637749, 2.189545951927499583E-17, 1.818405511757259729 ) ) ;
#15759 = CONICAL_SURFACE ( 'NONE', #44792, 0.08090551181102362266, 0.7853981633974511656 ) ;
#15760 = CARTESIAN_POINT ( 'NONE',  ( 0.1264236179284866091, -0.8124999999462361178, 0.1264236179284866091 ) ) ;
#15761 = ORIENTED_EDGE ( 'NONE', *, *, #32638, .T. ) ;
#15762 = AXIS2_PLACEMENT_3D ( 'NONE', #13017, #42215, #9418 ) ;
#15763 = AXIS2_PLACEMENT_3D ( 'NONE', #32289, #39438, #35857 ) ;
#15764 = DIRECTION ( 'NONE',  ( 0.000000000000000000, 0.000000000000000000, -1.000000000000000000 ) ) ;
#15765 = CARTESIAN_POINT ( 'NONE',  ( 0.1113553986120547346, -1.725393700679874076, -0.1113553986120547346 ) ) ;
#15766 = CARTESIAN_POINT ( 'NONE',  ( -0.8759842519685039353, -0.1574803149606299191, 0.1082677164279060994 ) ) ;
#15767 = CARTESIAN_POINT ( 'NONE',  ( 0.6971942568897648851, 0.07405724077823318263, 1.220472440891118504 ) ) ;
#15768 = EDGE_CURVE ( 'NONE', #38536, #4180, #32950, .T. ) ;
#15769 = DIRECTION ( 'NONE',  ( -0.000000000000000000, 1.000000000000000000, -3.995705278811693553E-31 ) ) ;
#15770 = CARTESIAN_POINT ( 'NONE',  ( -9.642888182262618425E-18, -1.690944881889763884, -0.1574803149606299191 ) ) ;
#15771 = CARTESIAN_POINT ( 'NONE',  ( -0.8759842519685039353, -0.1574803149606299191, 0.5118110236220472231 ) ) ;
#15772 = DIRECTION ( 'NONE',  ( 1.000000000000000000, 0.000000000000000000, -1.822029033848725275E-16 ) ) ;
#15773 = CARTESIAN_POINT ( 'NONE',  ( -0.8759842519685039353, 0.1787899950787401882, 0.3075787401037169411 ) ) ;
#15774 = EDGE_CURVE ( 'NONE', #36149, #24840, #34509, .T. ) ;
#15775 = CARTESIAN_POINT ( 'NONE',  ( 0.1787899950787401604, 0.09055118115612578733, 0.07405724077823318263 ) ) ;
#15776 = ORIENTED_EDGE ( 'NONE', *, *, #39156, .T. ) ;
#15777 = CARTESIAN_POINT ( 'NONE',  ( -0.07405724077823318263, -1.548228346402928723, -0.1787899950787401604 ) ) ;
#15778 = CARTESIAN_POINT ( 'NONE',  ( -1.033464566929136907, -0.06523048226347749612, 1.857775590551182798 ) ) ;
#15779 = CARTESIAN_POINT ( 'NONE',  ( -1.054774247047244540, -0.07405724077823318263, 1.791338582623401177 ) ) ;
#15780 = CARTESIAN_POINT ( 'NONE',  ( -0.9500414927467377701, -0.1787899950787401604, 0.8809055117572600624 ) ) ;
#15781 = CARTESIAN_POINT ( 'NONE',  ( -0.9500414927467378812, 0.1787899950787401604, 0.5068897637257642197 ) ) ;
#15782 = ( BOUNDED_CURVE ( )  B_SPLINE_CURVE ( 2, ( #46348, #28403, #35585, #21178, #13312, #42508, #24325, #31067, #16665 ),
 .UNSPECIFIED., .F., .T. ) 
 B_SPLINE_CURVE_WITH_KNOTS ( ( 3, 2, 2, 2, 3 ),
 ( 0.4400000000000000022, 0.4425000000000000044, 0.4450000000000000067, 0.4475000000000000089, 0.4500000000000000111 ),
 .UNSPECIFIED. ) 
 CURVE ( )  GEOMETRIC_REPRESENTATION_ITEM ( )  RATIONAL_B_SPLINE_CURVE ( ( 1.000000000000000000, 0.9238795325112869605, 1.000000000000000000, 0.9238795325112869605, 1.000000000000000000, 0.9238795325112869605, 1.000000000000000000, 0.9238795325112869605, 1.000000000000000000 ) ) 
 REPRESENTATION_ITEM ( '' )  ) ;
#15783 = CARTESIAN_POINT ( 'NONE',  ( 0.7185039370078739607, 1.928577636452523993E-17, 0.4921259841444416971 ) ) ;
#15784 = DIRECTION ( 'NONE',  ( 0.000000000000000000, -1.000000000000000000, 0.000000000000000000 ) ) ;
#15785 = CARTESIAN_POINT ( 'NONE',  ( -0.8107537697050254399, 0.1574803149606300301, 0.3272637794200322636 ) ) ;
#15786 = CARTESIAN_POINT ( 'NONE',  ( -0.1534195868007020847, 0.9251089822459547252, -1.060267534067255157 ) ) ;
#15787 = CARTESIAN_POINT ( 'NONE',  ( -0.1264236179284866091, -0.5626239682292386579, 0.1264236179284866091 ) ) ;
#15788 = CARTESIAN_POINT ( 'NONE',  ( -0.1891223223152169453, -0.08955981945756850970, 0.1329000297558324828 ) ) ;
#15789 = CYLINDRICAL_SURFACE ( 'NONE', #12680, 0.04921259842519678379 ) ;
#15790 = CARTESIAN_POINT ( 'NONE',  ( 1.181102362204724310, 0.000000000000000000, 0.9842519685039370358 ) ) ;
#15791 = VECTOR ( 'NONE', #45190, 39.37007874015748143 ) ;
#15792 = CARTESIAN_POINT ( 'NONE',  ( -1.054774247047244540, 0.07405724077823318263, 0.5364173227808821665 ) ) ;
#15793 = CARTESIAN_POINT ( 'NONE',  ( 0.8107537697050254399, 0.1574803149606300301, 1.193405511703496957 ) ) ;
#15794 = VERTEX_POINT ( 'NONE', #9104 ) ;
#15795 = EDGE_CURVE ( 'NONE', #38992, #28962, #33175, .T. ) ;
#15796 = DIRECTION ( 'NONE',  ( 0.000000000000000000, 0.000000000000000000, 1.000000000000000000 ) ) ;
#15797 = CARTESIAN_POINT ( 'NONE',  ( -0.7495606340400177148, 0.1264236179284866091, 1.577263779473795369 ) ) ;
#15798 = CARTESIAN_POINT ( 'NONE',  ( -0.07405724077823318263, -1.375984251914741163, 0.1787899950787401604 ) ) ;
#15799 = CARTESIAN_POINT ( 'NONE',  ( -0.1264236179284866091, -1.540846456639149542, -0.1264236179284866091 ) ) ;
#15800 = CARTESIAN_POINT ( 'NONE',  ( 1.033464566929134687, 0.06523048226347956391, 0.9571850393700783721 ) ) ;
#15801 = DIRECTION ( 'NONE',  ( -1.000000000000000000, 0.000000000000000000, 0.000000000000000000 ) ) ;
#15802 = CARTESIAN_POINT ( 'NONE',  ( -0.8107537697050253289, -0.1574803149606297803, 1.129429133750740277 ) ) ;
#15803 = CARTESIAN_POINT ( 'NONE',  ( 0.8759842519685039353, -0.1787899950787401882, 0.5684055117572598403 ) ) ;
#15805 = CARTESIAN_POINT ( 'NONE',  ( 0.1476377952755906220, -0.9875035750853327077, -1.463737590216208861 ) ) ;
#15804 = CARTESIAN_POINT ( 'NONE',  ( -0.1574803149606300301, -0.2662401574803150983, -0.06523048226347956391 ) ) ;
#15806 = CARTESIAN_POINT ( 'NONE',  ( 1.033464566929133799, 0.000000000000000000, 1.968503936900346529 ) ) ;
#15807 = ORIENTED_EDGE ( 'NONE', *, *, #34172, .F. ) ;
#15808 = CARTESIAN_POINT ( 'NONE',  ( -0.1343543525242022474, -0.09328364641522272904, -0.1179723892412200270 ) ) ;
#15809 = CARTESIAN_POINT ( 'NONE',  ( 0.9412147342319837628, -0.1574803149606297803, 0.9867125984251976512 ) ) ;
#15810 = CARTESIAN_POINT ( 'NONE',  ( -0.2559055118110236116, -0.1477471161312047254, -0.2921040715117803055 ) ) ;
#15811 = CARTESIAN_POINT ( 'NONE',  ( 0.1113553986120547346, -0.5541338581601890079, 0.1113553986120547346 ) ) ;
#15812 = DIRECTION ( 'NONE',  ( 0.000000000000000000, 0.000000000000000000, -1.000000000000000000 ) ) ;
#15813 = CARTESIAN_POINT ( 'NONE',  ( -1.033464566929133799, 0.000000000000000000, 1.269685039370078705 ) ) ;
#15814 = CARTESIAN_POINT ( 'NONE',  ( -0.1666288720097009179, -0.08956157984806185912, 0.02185444682987447082 ) ) ;
#15815 = ORIENTED_EDGE ( 'NONE', *, *, #6602, .T. ) ;
#15816 = CARTESIAN_POINT ( 'NONE',  ( 0.1526812815691464542, -0.02763205629824401835, -0.1377952755905511861 ) ) ;
#15817 = CARTESIAN_POINT ( 'NONE',  ( -0.6195511811023656223, 0.9842519685039375910, -0.8759842519685044904 ) ) ;
#15818 = AXIS2_PLACEMENT_3D ( 'NONE', #22649, #3946, #23124 ) ;
#15819 = CARTESIAN_POINT ( 'NONE',  ( 0.9500414927467378812, 0.1787899950787401604, 0.7381889763241898939 ) ) ;
#15820 = EDGE_CURVE ( 'NONE', #32649, #40086, #12949, .T. ) ;
#15821 = VERTEX_POINT ( 'NONE', #42606 ) ;
#15822 = DIRECTION ( 'NONE',  ( -1.000000000000000000, 5.464378949326940770E-15, -4.275490733183370330E-15 ) ) ;
#15823 = CARTESIAN_POINT ( 'NONE',  ( -0.1574803149606299191, -0.02755905511811023584, 0.000000000000000000 ) ) ;
#15824 = CARTESIAN_POINT ( 'NONE',  ( -0.1264236179284866091, -1.698326771599779628, -0.1264236179284866091 ) ) ;
#15825 = CARTESIAN_POINT ( 'NONE',  ( 0.1787899950787401882, -0.9306102361667086820, -2.189545951927503898E-17 ) ) ;
#15826 = CARTESIAN_POINT ( 'NONE',  ( -0.1113553986120547346, -1.213582677165354395, -0.1113553986120547346 ) ) ;
#15827 = CARTESIAN_POINT ( 'NONE',  ( 0.7185039370078746268, -0.06523048226347956391, 1.085137795168063413 ) ) ;
#15828 = EDGE_CURVE ( 'NONE', #25294, #21453, #39771, .T. ) ;
#15829 = CARTESIAN_POINT ( 'NONE',  ( -0.02900000000000056352, 0.5288907983920048128, -0.7507079620615672022 ) ) ;
#15830 = ORIENTED_EDGE ( 'NONE', *, *, #34649, .F. ) ;
#15831 = ORIENTED_EDGE ( 'NONE', *, *, #10750, .T. ) ;
#15832 = CARTESIAN_POINT ( 'NONE',  ( -1.002407869896990045, -0.1264236179284866091, 1.793799212544661348 ) ) ;
#15833 = EDGE_CURVE ( 'NONE', #13064, #11651, #36514, .T. ) ;
#15834 = CARTESIAN_POINT ( 'NONE',  ( 0.9500414927467378812, -0.1787899950787401604, 1.791338582623401177 ) ) ;
#15835 = ORIENTED_EDGE ( 'NONE', *, *, #3757, .T. ) ;
#15836 = CARTESIAN_POINT ( 'NONE',  ( -1.002407869896990045, -0.1264236179284866091, 0.8882874015210394658 ) ) ;
#15837 = CARTESIAN_POINT ( 'NONE',  ( -0.1574803149606299191, 1.928577636452524610E-17, -0.2748405511811023438 ) ) ;
#15838 = CARTESIAN_POINT ( 'NONE',  ( 0.8759842519685039353, -0.1787899950787401882, 0.4109251967966299213 ) ) ;
#15839 = CARTESIAN_POINT ( 'NONE',  ( -0.8759842519685039353, 0.1787899950787401882, 1.449311023568283341 ) ) ;
#15840 = EDGE_CURVE ( 'NONE', #47099, #16198, #38099, .T. ) ;
#15841 = CARTESIAN_POINT ( 'NONE',  ( -1.002407869896990045, -0.1264236179284866091, 1.237696850339937038 ) ) ;
#15842 = CARTESIAN_POINT ( 'NONE',  ( -0.6971942568897626646, -0.07405724077823297447, 0.9498031495525356416 ) ) ;
#15843 = CARTESIAN_POINT ( 'NONE',  ( -0.8019270111902717657, -0.1787899950787401604, 0.05413385821395302888 ) ) ;
#15844 = CARTESIAN_POINT ( 'NONE',  ( 0.06179214533981935986, 0.08095196624129888385, 0.2497573591203926524 ) ) ;
#15845 = CARTESIAN_POINT ( 'NONE',  ( -0.8019270111902717657, -0.1787899950787401604, 1.707677165300566235 ) ) ;
#15846 = CARTESIAN_POINT ( 'NONE',  ( -1.002407869896990045, -0.1264236179284866091, 0.06151574797773248782 ) ) ;
#15847 = CARTESIAN_POINT ( 'NONE',  ( -1.033464566929134687, 0.06523048226347956391, 1.547736220472440749 ) ) ;
#15848 = LINE ( 'NONE', #38575, #38153 ) ;
#15849 = CARTESIAN_POINT ( 'NONE',  ( 0.8019270111902716547, 0.1787899950787401604, 1.614173228292692386 ) ) ;
#15850 = CARTESIAN_POINT ( 'NONE',  ( -0.2415622317366385718, -0.09842519685039370636, -0.02995051380158457108 ) ) ;
#15851 = DIRECTION ( 'NONE',  ( 0.000000000000000000, 1.000000000000000000, 0.000000000000000000 ) ) ;
#15852 = CARTESIAN_POINT ( 'NONE',  ( -2.048885995248196921E-16, 1.086379535891622172, -0.03715491745705894189 ) ) ;
#15853 = VERTEX_POINT ( 'NONE', #16309 ) ;
#15854 = ORIENTED_EDGE ( 'NONE', *, *, #41961, .T. ) ;
#15855 = VERTEX_POINT ( 'NONE', #23967 ) ;
#15856 = CARTESIAN_POINT ( 'NONE',  ( -1.094772975963752103E-17, -0.8420275590013542866, -0.1787899950787401882 ) ) ;
#15857 = CARTESIAN_POINT ( 'NONE',  ( 0.1787899950787401604, -1.046259842465921297, 0.07405724077823318263 ) ) ;
#15858 = CARTESIAN_POINT ( 'NONE',  ( -0.8107537697050254399, 0.1574803149606300301, 1.281988188976378895 ) ) ;
#15859 = CARTESIAN_POINT ( 'NONE',  ( -1.100456976456230270E-17, -0.3258312111578488546, -0.1797182628040039365 ) ) ;
#15860 = DIRECTION ( 'NONE',  ( -0.000000000000000000, 1.000000000000000000, -0.000000000000000000 ) ) ;
#15861 = CARTESIAN_POINT ( 'NONE',  ( -1.033464566929134687, 0.06523048226347956391, 1.065452755797984041 ) ) ;
#15862 = CARTESIAN_POINT ( 'NONE',  ( 0.6971942568897626646, 0.07405724077823318263, 0.7086614172690703928 ) ) ;
#15863 = CARTESIAN_POINT ( 'NONE',  ( 0.008625679036592873508, 0.08625453335789746989, 0.1261914363108047332 ) ) ;
#15864 = CARTESIAN_POINT ( 'NONE',  ( -0.7185039370078746268, -0.06523048226347956391, 0.06151574792396910518 ) ) ;
#15865 = CARTESIAN_POINT ( 'NONE',  ( 0.8019270111902717657, -0.1787899950787401604, 1.825787401521040243 ) ) ;
#15866 = CARTESIAN_POINT ( 'NONE',  ( 0.8759842519685039353, -0.1574803149606299191, 0.03937007874015747977 ) ) ;
#15867 = LINE ( 'NONE', #45299, #14521 ) ;
#15868 = CARTESIAN_POINT ( 'NONE',  ( -1.094772975963752103E-17, -0.4089566928596221063, -0.1787899950787401882 ) ) ;
#15869 = DIRECTION ( 'NONE',  ( 1.000000000000000000, 0.000000000000000000, 0.000000000000000000 ) ) ;
#15871 = VECTOR ( 'NONE', #41724, 39.37007874015748143 ) ;
#15870 = CARTESIAN_POINT ( 'NONE',  ( -0.1787899950787401604, -1.223425196796630532, -0.07405724077823318263 ) ) ;
#15872 = CARTESIAN_POINT ( 'NONE',  ( 1.054774247047244540, 0.07405724077823318263, 0.2263779527021421711 ) ) ;
#15873 = ADVANCED_FACE ( 'NONE', ( #38805 ), #2137, .F. ) ;
#15874 = FACE_OUTER_BOUND ( 'NONE', #35512, .T. ) ;
#15875 = CARTESIAN_POINT ( 'NONE',  ( -0.8759842519685039353, -0.1787899950787401882, 1.744586614119464807 ) ) ;
#15876 = EDGE_LOOP ( 'NONE', ( #7806, #27096, #1466, #41116, #46969, #3682 ) ) ;
#15877 = CARTESIAN_POINT ( 'NONE',  ( -0.6971942568897637749, 2.189545951927499583E-17, 1.267224409395055096 ) ) ;
#15878 = CARTESIAN_POINT ( 'NONE',  ( -0.5555748031496068329, 1.092739197465708640E-15, -0.7480314960629921295 ) ) ;
#15879 = CARTESIAN_POINT ( 'NONE',  ( 0.7495606340400177148, 0.1264236179284866091, 1.301673228292692830 ) ) ;
#15880 = CARTESIAN_POINT ( 'NONE',  ( -1.054774247047244540, 0.07405724077823318263, 0.5413385826234012876 ) ) ;
#15881 = CARTESIAN_POINT ( 'NONE',  ( -0.9500414927467378812, -0.1787899950787401604, 1.235236220418678199 ) ) ;
#15882 = CARTESIAN_POINT ( 'NONE',  ( 0.3425196850393700809, 4.616380251121755931E-17, 0.000000000000000000 ) ) ;
#15883 = ADVANCED_FACE ( 'NONE', ( #20114 ), #27352, .T. ) ;
#15884 = CARTESIAN_POINT ( 'NONE',  ( -0.1302006108103286042, -0.09843743769978773039, -0.1225641731413484731 ) ) ;
#15885 = FACE_OUTER_BOUND ( 'NONE', #7083, .T. ) ;
#15886 = CARTESIAN_POINT ( 'NONE',  ( 0.8019270111902716547, -0.1787899950787401604, 0.4478346456155276045 ) ) ;
#15887 = CARTESIAN_POINT ( 'NONE',  ( -1.054774247047244540, -0.07405724077823318263, 0.3740157479777325711 ) ) ;
#15888 = CARTESIAN_POINT ( 'NONE',  ( -0.8759842519685039353, -0.1787899950787401882, 0.8390748030958424808 ) ) ;
#15889 = ORIENTED_EDGE ( 'NONE', *, *, #8504, .F. ) ;
#15890 = CARTESIAN_POINT ( 'NONE',  ( 0.000000000000000000, 0.000000000000000000, 0.000000000000000000 ) ) ;
#15891 = ORIENTED_EDGE ( 'NONE', *, *, #44348, .F. ) ;
#15892 = CARTESIAN_POINT ( 'NONE',  ( 1.054774247047244540, 0.07405724077823318263, 0.9350393700249758355 ) ) ;
#15893 = CARTESIAN_POINT ( 'NONE',  ( -0.8759842519685039353, -0.1574803149606299191, 0.2755905511811023723 ) ) ;
#15894 = CARTESIAN_POINT ( 'NONE',  ( 0.6971942568897648851, 0.07405724077823318263, 1.225393700733637514 ) ) ;
#15895 = CARTESIAN_POINT ( 'NONE',  ( -0.1522882881087165574, -0.09851385314725177866, -0.2000479292304901680 ) ) ;
#15896 = CARTESIAN_POINT ( 'NONE',  ( -0.2559055118110236671, -0.01424369123639110390, -0.02740704184215039807 ) ) ;
#15897 = ORIENTED_EDGE ( 'NONE', *, *, #16527, .F. ) ;
#15898 = CARTESIAN_POINT ( 'NONE',  ( -0.8070866141732283561, -0.0009842519685049383633, 0.7574803149606299524 ) ) ;
#15899 = FACE_OUTER_BOUND ( 'NONE', #29823, .T. ) ;
#15900 = PLANE ( 'NONE',  #25196 ) ;
#15901 = CARTESIAN_POINT ( 'NONE',  ( -0.07405724077823318263, -1.401698771378846464, -0.1787899950787401604 ) ) ;
#15902 = ORIENTED_EDGE ( 'NONE', *, *, #30363, .T. ) ;
#15903 = DIRECTION ( 'NONE',  ( 0.000000000000000000, 0.7071067811862530306, 0.7071067811868418929 ) ) ;
#15904 = CARTESIAN_POINT ( 'NONE',  ( 0.07405724077823318263, -0.3818897637257640532, 0.1787899950787401604 ) ) ;
#15905 = CARTESIAN_POINT ( 'NONE',  ( 0.4736248074375866701, -0.09842519685039370636, 1.713085361781129690 ) ) ;
#15906 = ORIENTED_EDGE ( 'NONE', *, *, #16997, .F. ) ;
#15907 = CARTESIAN_POINT ( 'NONE',  ( 0.0003553830333942996095, 0.1260611533336402912, 0.05724849586090775128 ) ) ;
#15908 = DIRECTION ( 'NONE',  ( 0.000000000000000000, 0.000000000000000000, -1.000000000000000000 ) ) ;
#15909 = VECTOR ( 'NONE', #8476, 39.37007874015748143 ) ;
#15910 = CARTESIAN_POINT ( 'NONE',  ( 0.1264236179284866091, -0.2170275590013547307, -0.1264236179284866091 ) ) ;
#15911 = CARTESIAN_POINT ( 'NONE',  ( 1.002407869896990045, -0.1264236179284866091, 0.1747047243556852092 ) ) ;
#15912 = CARTESIAN_POINT ( 'NONE',  ( -1.094772975963752103E-17, -1.747539370024976391, -0.1787899950787401882 ) ) ;
#15913 = CARTESIAN_POINT ( 'NONE',  ( 0.008382045503145925391, -0.06595839018091839701, -0.1377952755905513804 ) ) ;
#15914 = ( BOUNDED_CURVE ( )  B_SPLINE_CURVE ( 2, ( #444, #26598, #4749, #41150, #36654, #29517, #14609, #36890, #33321 ),
 .UNSPECIFIED., .F., .T. ) 
 B_SPLINE_CURVE_WITH_KNOTS ( ( 3, 2, 2, 2, 3 ),
 ( 0.6800000000000000488, 0.6824999999999999956, 0.6850000000000000533, 0.6875000000000000000, 0.6899999999999999467 ),
 .UNSPECIFIED. ) 
 CURVE ( )  GEOMETRIC_REPRESENTATION_ITEM ( )  RATIONAL_B_SPLINE_CURVE ( ( 1.000000000000000000, 0.9238795325112869605, 1.000000000000000000, 0.9238795325112869605, 1.000000000000000000, 0.9238795325112869605, 1.000000000000000000, 0.9238795325112829637, 1.000000000000000000 ) ) 
 REPRESENTATION_ITEM ( '' )  ) ;
#15915 = CARTESIAN_POINT ( 'NONE',  ( -1.054774247047244540, -0.07405724077823318263, 0.6151574802611973203 ) ) ;
#15916 = CARTESIAN_POINT ( 'NONE',  ( -0.7185039370078739607, 1.928577636452523993E-17, 1.279527558947590515 ) ) ;
#15918 = DIRECTION ( 'NONE',  ( 1.000000000000000000, 2.114720919224289611E-16, 0.000000000000000000 ) ) ;
#15917 = CARTESIAN_POINT ( 'NONE',  ( 0.06523048226347956391, -0.7632874015748020158, 0.1574803149606297803 ) ) ;
#15919 = CARTESIAN_POINT ( 'NONE',  ( -0.07444174185955065859, -1.568449321394070006, 0.1797182628040039087 ) ) ;
#15920 = DIRECTION ( 'NONE',  ( 1.000000000000000000, 0.000000000000000000, 0.000000000000000000 ) ) ;
#15921 = CARTESIAN_POINT ( 'NONE',  ( 0.7495606340400177148, 0.1264236179284866091, 1.341043307032850462 ) ) ;
#15922 = CARTESIAN_POINT ( 'NONE',  ( 1.002407869896990045, -0.1264236179284866091, 1.867618110182456714 ) ) ;
#15923 = ORIENTED_EDGE ( 'NONE', *, *, #4801, .T. ) ;
#15925 = ORIENTED_EDGE ( 'NONE', *, *, #31630, .T. ) ;
#15924 = FACE_OUTER_BOUND ( 'NONE', #43960, .T. ) ;
#15926 = CARTESIAN_POINT ( 'NONE',  ( -0.9873396505805591694, -0.1113553986120547346, 1.451771653435779408 ) ) ;
#15927 = CARTESIAN_POINT ( 'NONE',  ( -0.8759842519685039353, 0.000000000000000000, 0.000000000000000000 ) ) ;
#15929 = CARTESIAN_POINT ( 'NONE',  ( -0.07405724077823318263, -0.01279527553678766298, -0.1787899950787401604 ) ) ;
#15928 = CARTESIAN_POINT ( 'NONE',  ( -0.06523048226347956391, -0.8518700786326312002, -0.1574803149606300301 ) ) ;
#15930 = CARTESIAN_POINT ( 'NONE',  ( 0.7646288533564489232, -0.1113553986120547346, 0.4970472439869613734 ) ) ;
#15931 = CARTESIAN_POINT ( 'NONE',  ( 0.9500414927467378812, -0.1787899950787401604, 0.4872047243556847929 ) ) ;
#15932 = EDGE_CURVE ( 'NONE', #30455, #34571, #2362, .T. ) ;
#15933 = DIRECTION ( 'NONE',  ( 0.000000000000000000, 0.000000000000000000, 1.000000000000000000 ) ) ;
#15934 = DIRECTION ( 'NONE',  ( 0.000000000000000000, 0.000000000000000000, 1.000000000000000000 ) ) ;
#15935 = VECTOR ( 'NONE', #3929, 39.37007874015748143 ) ;
#15936 = LINE ( 'NONE', #30563, #23791 ) ;
#15937 = CARTESIAN_POINT ( 'NONE',  ( -0.6971942568897637749, 2.189545951927499583E-17, 1.341043307032850462 ) ) ;
#15938 = CARTESIAN_POINT ( 'NONE',  ( 0.7185039370078746268, -0.06523048226347956391, 0.8882874014672753615 ) ) ;
#15939 = ORIENTED_EDGE ( 'NONE', *, *, #21878, .T. ) ;
#15940 = FACE_OUTER_BOUND ( 'NONE', #36114, .T. ) ;
#15941 = LINE ( 'NONE', #801, #28394 ) ;
#15942 = ORIENTED_EDGE ( 'NONE', *, *, #30758, .T. ) ;
#15943 = CARTESIAN_POINT ( 'NONE',  ( 0.1797182628040039365, 0.01865697781852925299, -2.200913952912460540E-17 ) ) ;
#15944 = CARTESIAN_POINT ( 'NONE',  ( 0.1264236179284866091, -1.368602362150960650, 0.1264236179284866091 ) ) ;
#15945 = CARTESIAN_POINT ( 'NONE',  ( -0.8759842519685039353, -0.1574803149606299191, 0.5807086613097960370 ) ) ;
#15946 = CARTESIAN_POINT ( 'NONE',  ( 0.7495606340400177148, 0.1264236179284866091, 1.572342519631275692 ) ) ;
#15947 = CARTESIAN_POINT ( 'NONE',  ( -0.8759842519685039353, -0.1574803149606299191, 1.220472440944881942 ) ) ;
#15948 = EDGE_CURVE ( 'NONE', #20413, #42967, #7667, .T. ) ;
#15949 = CARTESIAN_POINT ( 'NONE',  ( 0.1644020957507539848, 0.1623118080249112138, 1.367956046207553540E-19 ) ) ;
#15951 = CARTESIAN_POINT ( 'NONE',  ( -0.7185039370078739607, 1.928577636452523993E-17, 0.7677165353255432922 ) ) ;
#15950 = DIRECTION ( 'NONE',  ( 1.822029033848725028E-16, 0.000000000000000000, 1.000000000000000000 ) ) ;
#15952 = CARTESIAN_POINT ( 'NONE',  ( -0.7185039370078739607, 1.928577636452523993E-17, 0.4921259841444416971 ) ) ;
#15953 = B_SPLINE_CURVE_WITH_KNOTS ( 'NONE', 3,
 ( #17344, #35573, #9467, #28390, #9698, #2483, #24774, #2942, #13991, #20469, #35105, #2251, #35254, #46236, #6933, #20609, #43587, #10069, #28787, #6218, #20843, #28541, #39283, #9840, #35484, #21075, #2849, #46475, #10557, #6458, #36193, #39519, #35713, #47201, #10315, #2623, #31894, #17726, #17487, #17024, #38825 ),
 .UNSPECIFIED., .F., .F.,
 ( 4, 1, 1, 1, 1, 1, 1, 2, 2, 1, 1, 1, 1, 2, 2, 2, 1, 1, 1, 1, 2, 2, 1, 1, 1, 1, 1, 2, 2, 4 ),
 ( 0.000000000000000000, 0.1250000000000026368, 0.1875000000000038303, 0.2187500000000044131, 0.2343750000000046352, 0.2421875000000046629, 0.2460937500000047740, 0.2480468750000047462, 0.2500000000000046629, 0.3125000000000010547, 0.3437499999999993894, 0.3593749999999987232, 0.3671874999999983347, 0.3710937499999981681, 0.3749999999999980016, 0.4999999999999946709, 0.5624999999999930056, 0.5937499999999921174, 0.6093749999999916733, 0.6171874999999913403, 0.6210937499999912292, 0.6249999999999911182, 0.6874999999999893419, 0.7187499999999884537, 0.7343749999999880096, 0.7421874999999876765, 0.7460937499999875655, 0.7480468749999874545, 0.7499999999999873435, 1.000000000000000000 ),
 .UNSPECIFIED. ) ;
#15954 = CARTESIAN_POINT ( 'NONE',  ( 0.7185039370078746268, -0.06523048226347956391, 1.478838582569637294 ) ) ;
#15955 = ORIENTED_EDGE ( 'NONE', *, *, #4758, .T. ) ;
#15956 = ORIENTED_EDGE ( 'NONE', *, *, #5961, .F. ) ;
#15957 = CIRCLE ( 'NONE', #40385, 0.09842519685039370636 ) ;
#15958 = ( BOUNDED_CURVE ( )  B_SPLINE_CURVE ( 2, ( #38969, #35637, #6134, #20758, #2544, #38752, #20291, #34934, #42329 ),
 .UNSPECIFIED., .F., .T. ) 
 B_SPLINE_CURVE_WITH_KNOTS ( ( 3, 2, 2, 2, 3 ),
 ( 0.02000000000000000042, 0.02249999999999999917, 0.02500000000000000139, 0.02750000000000000014, 0.02999999999999999889 ),
 .UNSPECIFIED. ) 
 CURVE ( )  GEOMETRIC_REPRESENTATION_ITEM ( )  RATIONAL_B_SPLINE_CURVE ( ( 1.000000000000000000, 0.9238795325112869605, 1.000000000000000000, 0.9238795325112869605, 1.000000000000000000, 0.9238795325112869605, 1.000000000000000000, 0.9238795325112869605, 1.000000000000000000 ) ) 
 REPRESENTATION_ITEM ( '' )  ) ;
#15959 = CARTESIAN_POINT ( 'NONE',  ( 0.9873396505805591694, -0.1113553986120547346, 0.5954724409448819422 ) ) ;
#15960 = CARTESIAN_POINT ( 'NONE',  ( 0.8759842519685039353, 0.1787899950787401882, 0.9817913385289134265 ) ) ;
#15961 = CARTESIAN_POINT ( 'NONE',  ( 0.1113553986120547346, -0.04232283453814220803, 0.1113553986120547346 ) ) ;
#15962 = CARTESIAN_POINT ( 'NONE',  ( -0.8019270111902717657, -0.1787899950787401604, 1.274606299158834277 ) ) ;
#15963 = ORIENTED_EDGE ( 'NONE', *, *, #2746, .T. ) ;
#15964 = CARTESIAN_POINT ( 'NONE',  ( 0.8759842519685039353, 0.1574803149606299191, 1.860236220364913207 ) ) ;
#15965 = LINE ( 'NONE', #8986, #26754 ) ;
#15966 = CARTESIAN_POINT ( 'NONE',  ( 0.1787899950787401604, -1.022761763504828059, 0.07405724077823318263 ) ) ;
#15967 = EDGE_LOOP ( 'NONE', ( #35114, #36362, #17529, #28807 ) ) ;
#15968 = CARTESIAN_POINT ( 'NONE',  ( 0.1264236179284866091, 0.09301181107738563936, 0.1264236179284866091 ) ) ;
#15969 = ORIENTED_EDGE ( 'NONE', *, *, #39973, .F. ) ;
#15970 = VERTEX_POINT ( 'NONE', #1904 ) ;
#15971 = APPLICATION_CONTEXT ( 'automotive_design' ) ;
#15972 = CARTESIAN_POINT ( 'NONE',  ( 0.004259712139235173438, -0.04573943165073560135, 0.1377945059011559392 ) ) ;
#15973 = CARTESIAN_POINT ( 'NONE',  ( 0.000000000000000000, 0.000000000000000000, -0.3139606299212599483 ) ) ;
#15974 = AXIS2_PLACEMENT_3D ( 'NONE', #39230, #16968, #2568 ) ;
#15975 = CARTESIAN_POINT ( 'NONE',  ( 3.284318927891251994E-17, -0.7042322834108031282, 0.1787899950787401882 ) ) ;
#15976 = AXIS2_PLACEMENT_3D ( 'NONE', #40488, #36926, #21837 ) ;
#15977 = CARTESIAN_POINT ( 'NONE',  ( -1.054774247047244540, 0.07405724077823318263, 0.1476377952218269340 ) ) ;
#15978 = CARTESIAN_POINT ( 'NONE',  ( -0.7185039370078746268, 0.06523048226347956391, 0.9325787401574799906 ) ) ;
#15979 = CARTESIAN_POINT ( 'NONE',  ( 0.000000000000000000, -0.5708661417322835607, 0.9783464566929281903 ) ) ;
#15980 = CARTESIAN_POINT ( 'NONE',  ( 0.1797182628040039365, -1.044335148165722593, -2.200913952912460540E-17 ) ) ;
#15981 = CARTESIAN_POINT ( 'NONE',  ( 0.7646288533564489232, -0.1113553986120547346, 1.097440944881889813 ) ) ;
#15982 = CARTESIAN_POINT ( 'NONE',  ( 1.054774247047244540, 0.07405724077823318263, 0.8956692912848198684 ) ) ;
#15983 = CARTESIAN_POINT ( 'NONE',  ( 0.4632545931758527691, 0.08090551181102362266, 0.000000000000000000 ) ) ;
#15984 = CARTESIAN_POINT ( 'NONE',  ( 0.8107537697050253289, 0.1574803149606300301, 1.557578740157481212 ) ) ;
#15986 = CARTESIAN_POINT ( 'NONE',  ( -0.1658511544270574734, -0.1997399692762479584, -0.3128573757128095267 ) ) ;
#15985 = CARTESIAN_POINT ( 'NONE',  ( 0.7100035458928386500, 0.0008589249953504293073, 1.983251210439181067 ) ) ;
#15987 = CARTESIAN_POINT ( 'NONE',  ( -0.8759842519685039353, 0.000000000000000000, 0.000000000000000000 ) ) ;
#15988 = CARTESIAN_POINT ( 'NONE',  ( -1.033464566929133799, 0.000000000000000000, 1.614173228238929170 ) ) ;
#15989 = LINE ( 'NONE', #30855, #26875 ) ;
#15990 = EDGE_CURVE ( 'NONE', #18113, #5859, #16764, .T. ) ;
#15991 = CARTESIAN_POINT ( 'NONE',  ( 0.9500414927467377701, -0.1787899950787401604, 0.9596456692375763264 ) ) ;
#15992 = CARTESIAN_POINT ( 'NONE',  ( 1.054774247047244096, 0.000000000000000000, 1.877460629867496067 ) ) ;
#15993 = CARTESIAN_POINT ( 'NONE',  ( 0.07405724077823318263, -0.9576771653005667906, -0.1787899950787401604 ) ) ;
#15994 = CARTESIAN_POINT ( 'NONE',  ( 0.7646288533564489232, 0.1113553986120547346, 0.4084645668216063119 ) ) ;
#15995 = ORIENTED_EDGE ( 'NONE', *, *, #10990, .F. ) ;
#15996 = CARTESIAN_POINT ( 'NONE',  ( 0.7185039370078739607, 1.928577636452523993E-17, 1.092519685039370136 ) ) ;
#15997 = CARTESIAN_POINT ( 'NONE',  ( -0.06523048226347956391, -1.678641732175937706, -0.1574803149606300301 ) ) ;
#15998 = CARTESIAN_POINT ( 'NONE',  ( -1.033464566929134687, -0.06523048226347956391, 0.1156496061916856694 ) ) ;
#15999 = DIRECTION ( 'NONE',  ( -1.000000000000000000, 0.000000000000000000, 0.000000000000000000 ) ) ;
#16000 = CARTESIAN_POINT ( 'NONE',  ( 1.002407869896990045, 0.1264236179284866091, 1.129429133804503937 ) ) ;
#16001 = EDGE_CURVE ( 'NONE', #30540, #3096, #44254, .T. ) ;
#16002 = CARTESIAN_POINT ( 'NONE',  ( 0.1574803149606299191, 1.928577636452524918E-17, -0.0009999999999999347518 ) ) ;
#16003 = CARTESIAN_POINT ( 'NONE',  ( -0.1574803149606299191, -1.799212598425196763, 0.000000000000000000 ) ) ;
#16004 = LINE ( 'NONE', #12412, #45142 ) ;
#16005 = VECTOR ( 'NONE', #16451, 39.37007874015748143 ) ;
#16006 = PLANE ( 'NONE',  #38231 ) ;
#16007 = CARTESIAN_POINT ( 'NONE',  ( -1.002407869896990045, 0.1264236179284866091, 0.2632874015210397434 ) ) ;
#16008 = ORIENTED_EDGE ( 'NONE', *, *, #20066, .T. ) ;
#16009 = TOROIDAL_SURFACE ( 'NONE', #37386, 0.7874015748031496509, 0.04921259842519685318 ) ;
#16010 = CARTESIAN_POINT ( 'NONE',  ( 0.1264236179284866091, -1.526082677111590513, 0.1264236179284866091 ) ) ;
#16011 = CARTESIAN_POINT ( 'NONE',  ( -0.6971942568897648851, -0.07405724077823297447, 1.894685039316315489 ) ) ;
#16012 = AXIS2_PLACEMENT_3D ( 'NONE', #7801, #32526, #44212 ) ;
#16013 = CARTESIAN_POINT ( 'NONE',  ( -1.002407869896990045, 0.1264236179284866091, 0.5437992125446614589 ) ) ;
#16014 = DIRECTION ( 'NONE',  ( 1.000000000000000000, 0.000000000000000000, 0.000000000000000000 ) ) ;
#16015 = DIRECTION ( 'NONE',  ( -1.000000000000000000, 0.000000000000000000, 0.000000000000000000 ) ) ;
#16016 = DIRECTION ( 'NONE',  ( -0.000000000000000000, 1.000000000000000000, -0.000000000000000000 ) ) ;
#16017 = CARTESIAN_POINT ( 'NONE',  ( -0.2824199087359778315, 0.8539303365987040983, -1.004656681308842225 ) ) ;
#16018 = CARTESIAN_POINT ( 'NONE',  ( 0.07405724077823318263, -0.6339822359457745193, 0.1787899950787401604 ) ) ;
#16019 = CARTESIAN_POINT ( 'NONE',  ( -0.1609361112149740314, -0.08956130496922656836, -0.06600197363463798650 ) ) ;
#16020 = DIRECTION ( 'NONE',  ( 0.000000000000000000, -0.7880107536067207930, 0.6156614753256598460 ) ) ;
#16021 = CARTESIAN_POINT ( 'NONE',  ( 0.4632545931758527691, 4.616380251121755931E-17, 0.000000000000000000 ) ) ;
#16022 = DIRECTION ( 'NONE',  ( -3.469446951953614978E-15, -1.000000000000000000, 3.995705278811693553E-31 ) ) ;
#16023 = CARTESIAN_POINT ( 'NONE',  ( 0.2559026586320093388, -0.1036163276257849458, -0.07053060040796885199 ) ) ;
#16024 = CARTESIAN_POINT ( 'NONE',  ( -0.6971942568897637749, 2.189545951927499583E-17, 0.4749015747493858242 ) ) ;
#16025 = CARTESIAN_POINT ( 'NONE',  ( -0.9412147342319837628, -0.1574803149606297803, 0.3961614173228344415 ) ) ;
#16026 = CARTESIAN_POINT ( 'NONE',  ( 0.2944196465027555387, -0.09842519685039370636, 1.205361022782828805E-17 ) ) ;
#16027 = CARTESIAN_POINT ( 'NONE',  ( -0.6971942568897648851, 0.07405724077823318263, 1.579724409395055318 ) ) ;
#16028 = CARTESIAN_POINT ( 'NONE',  ( 0.1787899950787401882, -1.560531496009228247, -2.189545951927503898E-17 ) ) ;
#16029 = CARTESIAN_POINT ( 'NONE',  ( -0.1787899950787401604, -1.572834645615527327, 0.07405724077823318263 ) ) ;
#16030 = AXIS2_PLACEMENT_3D ( 'NONE', #13040, #28616, #20678 ) ;
#16031 = CARTESIAN_POINT ( 'NONE',  ( 0.1634876958211989029, -0.08035719075736870443, 0.1391819764462846332 ) ) ;
#16032 = DIRECTION ( 'NONE',  ( -1.000000000000000000, 0.000000000000000000, 0.000000000000000000 ) ) ;
#16033 = CARTESIAN_POINT ( 'NONE',  ( -0.9412147342319837628, -0.1574803149606297803, 1.291830708553889817 ) ) ;
#16034 = ADVANCED_FACE ( 'NONE', ( #28512 ), #39958, .T. ) ;
#16035 = CARTESIAN_POINT ( 'NONE',  ( 1.054774247047244540, 0.07405724077823318263, 0.5413385826234012876 ) ) ;
#16037 = CARTESIAN_POINT ( 'NONE',  ( 0.9873396505805591694, -0.1113553986120547346, 1.766732283357039135 ) ) ;
#16036 = CARTESIAN_POINT ( 'NONE',  ( 0.1574803149606300301, -0.4384842519685039908, -0.06523048226347956391 ) ) ;
#16038 = CARTESIAN_POINT ( 'NONE',  ( -0.7646288533564489232, 0.1113553986120547346, 0.4183070866141732624 ) ) ;
#16039 = ORIENTED_EDGE ( 'NONE', *, *, #30319, .T. ) ;
#16040 = DIRECTION ( 'NONE',  ( 0.000000000000000000, 0.000000000000000000, -1.000000000000000000 ) ) ;
#16041 = CARTESIAN_POINT ( 'NONE',  ( 0.7646288533564489232, -0.1113553986120547346, 1.058070866141732402 ) ) ;
#16042 = DIRECTION ( 'NONE',  ( 1.000000000000000000, 0.000000000000000000, 0.000000000000000000 ) ) ;
#16043 = VECTOR ( 'NONE', #39615, 39.37007874015748143 ) ;
#16044 = DIRECTION ( 'NONE',  ( -0.000000000000000000, 1.000000000000000000, 0.000000000000000000 ) ) ;
#16045 = CARTESIAN_POINT ( 'NONE',  ( 0.1574803149606299746, 0.1473293504822046074, -0.9532488779249699284 ) ) ;
#16047 = DIRECTION ( 'NONE',  ( 0.000000000000000000, 0.000000000000000000, -1.000000000000000000 ) ) ;
#16046 = CARTESIAN_POINT ( 'NONE',  ( -0.3690944881889761664, 0.1574803149606353592, -0.7480314960629921295 ) ) ;
#16048 = CARTESIAN_POINT ( 'NONE',  ( -0.09718287230280656108, -0.08956224776672244703, 0.1265413919071203541 ) ) ;
#16049 = CARTESIAN_POINT ( 'NONE',  ( 0.07405724077823318263, -0.5393700786863945273, 0.1787899950787401604 ) ) ;
#16050 = ORIENTED_EDGE ( 'NONE', *, *, #23236, .T. ) ;
#16051 = CIRCLE ( 'NONE', #1435, 0.1968503937007874405 ) ;
#16052 = CARTESIAN_POINT ( 'NONE',  ( 0.7185039370078746268, -0.06523048226347956391, 0.8587598425196851792 ) ) ;
#16053 = CARTESIAN_POINT ( 'NONE',  ( -1.033464566929134687, 0.06523048226347956391, 1.114665354330708125 ) ) ;
#16054 = ORIENTED_EDGE ( 'NONE', *, *, #45091, .T. ) ;
#16055 = CARTESIAN_POINT ( 'NONE',  ( 0.7185039370078739607, 1.928577636452523993E-17, 1.289370078740157632 ) ) ;
#16056 = CARTESIAN_POINT ( 'NONE',  ( 1.033464566929133799, 0.000000000000000000, 1.505905511811023612 ) ) ;
#16057 = CARTESIAN_POINT ( 'NONE',  ( -0.1264236179284866091, -1.727854330654897685, 0.1264236179284866091 ) ) ;
#16058 = CARTESIAN_POINT ( 'NONE',  ( -0.1787899950787401604, -0.9478346456155283262, 0.07405724077823318263 ) ) ;
#16059 = CARTESIAN_POINT ( 'NONE',  ( 2.892866454678787531E-17, -1.198818897637795367, 0.1574803149606299191 ) ) ;
#16060 = CARTESIAN_POINT ( 'NONE',  ( 0.7185039370078739607, 1.928577636452523993E-17, 1.082677165246803241 ) ) ;
#16061 = CARTESIAN_POINT ( 'NONE',  ( -0.8107537697050254399, -0.1574803149606297803, 1.651082677165354839 ) ) ;
#16062 = CARTESIAN_POINT ( 'NONE',  ( -0.6971942568897635528, 0.03556354040785144471, 0.04064907247438850901 ) ) ;
#16063 = EDGE_CURVE ( 'NONE', #8144, #21819, #17627, .T. ) ;
#16064 = ORIENTED_EDGE ( 'NONE', *, *, #33421, .F. ) ;
#16065 = ORIENTED_EDGE ( 'NONE', *, *, #10024, .T. ) ;
#16066 = CARTESIAN_POINT ( 'NONE',  ( 0.9500414927467378812, -0.1787899950787401604, 1.870078740103715331 ) ) ;
#16067 = ORIENTED_EDGE ( 'NONE', *, *, #38250, .T. ) ;
#16068 = CARTESIAN_POINT ( 'NONE',  ( -0.1574803149606299191, -1.395669291231055098, 0.000000000000000000 ) ) ;
#16069 = PLANE ( 'NONE',  #4948 ) ;
#16070 = CARTESIAN_POINT ( 'NONE',  ( 0.9500414927467378812, -0.1787899950787401604, 0.4527559054580477249 ) ) ;
#16071 = CARTESIAN_POINT ( 'NONE',  ( -0.7495606340400177148, -0.1264236179284866091, 1.385334645615527549 ) ) ;
#16072 = CARTESIAN_POINT ( 'NONE',  ( -1.033464566929133799, 0.000000000000000000, 0.4035433070866141780 ) ) ;
#16073 = CARTESIAN_POINT ( 'NONE',  ( -1.002407869896990045, 0.1264236179284866091, 1.405019684985606476 ) ) ;
#16074 = CARTESIAN_POINT ( 'NONE',  ( -1.054774247047244540, 0.07405724077823318263, 0.06889763774151215492 ) ) ;
#16075 = DIRECTION ( 'NONE',  ( 0.4999999999999998890, 0.000000000000000000, -0.8660254037844388186 ) ) ;
#16076 = CARTESIAN_POINT ( 'NONE',  ( -0.8759842519685039353, -0.1787899950787401882, 1.670767716481669440 ) ) ;
#16077 = CARTESIAN_POINT ( 'NONE',  ( -0.7495606340400177148, 0.1264236179284866091, 0.1205708660879689087 ) ) ;
#16078 = CARTESIAN_POINT ( 'NONE',  ( -0.9873396505805591694, 0.1113553986120547346, 1.707677165354330562 ) ) ;
#16079 = CARTESIAN_POINT ( 'NONE',  ( -0.7646288533564489232, 0.1113553986120547346, 0.3001968503937008093 ) ) ;
#16080 = CARTESIAN_POINT ( 'NONE',  ( 1.054774247047244540, 0.07405724077823318263, 1.564960629867495845 ) ) ;
#16081 = CARTESIAN_POINT ( 'NONE',  ( -0.2037826476351566884, -0.09842519685039370636, 0.1181336077123911338 ) ) ;
#16082 = DIRECTION ( 'NONE',  ( 1.000000000000000000, 0.000000000000000000, -1.822029033848725275E-16 ) ) ;
#16083 = CARTESIAN_POINT ( 'NONE',  ( 0.9873396505805591694, 0.1113553986120547346, 0.2805118109160948947 ) ) ;
#16084 = CIRCLE ( 'NONE', #28315, 0.09842519685039370636 ) ;
#16085 = ORIENTED_EDGE ( 'NONE', *, *, #18503, .T. ) ;
#16086 = AXIS2_PLACEMENT_3D ( 'NONE', #23598, #38211, #27465 ) ;
#16087 = ORIENTED_EDGE ( 'NONE', *, *, #19646, .T. ) ;
#16088 = EDGE_CURVE ( 'NONE', #6854, #22637, #43559, .T. ) ;
#16089 = CARTESIAN_POINT ( 'NONE',  ( 3.284318927891251994E-17, -0.9404527558517480346, 0.1787899950787401882 ) ) ;
#16090 = EDGE_CURVE ( 'NONE', #799, #5551, #26561, .T. ) ;
#16091 = CARTESIAN_POINT ( 'NONE',  ( 0.1264236179284866091, -1.117618110182456714, -0.1264236179284866091 ) ) ;
#16092 = CYLINDRICAL_SURFACE ( 'NONE', #20965, 0.1574803149606299191 ) ;
#16093 = CARTESIAN_POINT ( 'NONE',  ( 0.6971942568897637749, 2.189545951927499583E-17, 1.852854330654897685 ) ) ;
#16094 = CARTESIAN_POINT ( 'NONE',  ( -0.1270800023317771588, -0.3110674316302897702, 0.1270800023317771588 ) ) ;
#16095 = EDGE_CURVE ( 'NONE', #12054, #23661, #4009, .T. ) ;
#16096 = CARTESIAN_POINT ( 'NONE',  ( 1.229559056033039366E-16, 0.000000000000000000, 0.3937007874015748254 ) ) ;
#16097 = CARTESIAN_POINT ( 'NONE',  ( 0.1787899950787401604, -0.1850393700249766959, 0.07405724077823318263 ) ) ;
#16098 = CARTESIAN_POINT ( 'NONE',  ( -0.8107537697050254399, -0.1574803149606297803, 0.8932086613097963701 ) ) ;
#16099 = CARTESIAN_POINT ( 'NONE',  ( 0.9500414927467378812, -0.1787899950787401604, 0.9990157479777320715 ) ) ;
#16100 = AXIS2_PLACEMENT_3D ( 'NONE', #19806, #45430, #12649 ) ;
#16101 = LINE ( 'NONE', #18949, #42270 ) ;
#16102 = CARTESIAN_POINT ( 'NONE',  ( 0.7185039370078739607, 1.928577636452523993E-17, 1.250000000000000000 ) ) ;
#16103 = CARTESIAN_POINT ( 'NONE',  ( 1.033464566929134687, 0.06523048226347956391, 0.04183070855389029591 ) ) ;
#16104 = EDGE_LOOP ( 'NONE', ( #3113, #8682, #20150, #21932 ) ) ;
#16105 = LINE ( 'NONE', #45054, #13755 ) ;
#16106 = CARTESIAN_POINT ( 'NONE',  ( -0.1787899950787401882, -0.3991141731745826982, 0.000000000000000000 ) ) ;
#16107 = CARTESIAN_POINT ( 'NONE',  ( 0.1574803149606299746, 0.5900595452500136950, -0.7440755677556079029 ) ) ;
#16108 = VECTOR ( 'NONE', #23662, 39.37007874015748143 ) ;
#16109 = CARTESIAN_POINT ( 'NONE',  ( -0.07405724077823318263, -1.188976377898991688, -0.1787899950787401604 ) ) ;
#16110 = CARTESIAN_POINT ( 'NONE',  ( -1.002407869896990045, -0.1264236179284866091, 1.710137795221826851 ) ) ;
#16111 = ORIENTED_EDGE ( 'NONE', *, *, #46727, .F. ) ;
#16112 = CARTESIAN_POINT ( 'NONE',  ( -0.8019270111902717657, 0.1787899950787401604, 1.377952755851748146 ) ) ;
#16114 = AXIS2_PLACEMENT_3D ( 'NONE', #32374, #46952, #43353 ) ;
#16113 = CARTESIAN_POINT ( 'NONE',  ( -0.8759842519685039353, 0.000000000000000000, 4.498031496062992574 ) ) ;
#16115 = CARTESIAN_POINT ( 'NONE',  ( 0.9500414927467378812, -0.1787899950787401604, 1.358267716481669662 ) ) ;
#16116 = CARTESIAN_POINT ( 'NONE',  ( 0.7495606340400177148, 0.1264236179284866091, 0.08120078734781142893 ) ) ;
#16117 = CARTESIAN_POINT ( 'NONE',  ( -0.9500414927467378812, -0.1787899950787401604, 1.195866141678520345 ) ) ;
#16118 = DIRECTION ( 'NONE',  ( 0.8191520442889991260, 1.003171929053533745E-16, -0.5735764363510355013 ) ) ;
#16119 = CARTESIAN_POINT ( 'NONE',  ( -0.08452081858070546738, -0.09842406081630053483, -0.1575734998833499545 ) ) ;
#16120 = DIRECTION ( 'NONE',  ( 0.000000000000000000, -1.000000000000000000, 0.000000000000000000 ) ) ;
#16121 = CARTESIAN_POINT ( 'NONE',  ( 0.7495606340400177148, -0.1264236179284866091, 0.4060039369541102450 ) ) ;
#16122 = CARTESIAN_POINT ( 'NONE',  ( -0.6971942568897648851, -0.07405724077823297447, 0.3986220471903311746 ) ) ;
#16123 = CARTESIAN_POINT ( 'NONE',  ( -0.05467468201772657937, -0.07678538764759451629, 0.2538665577330194156 ) ) ;
#16124 = CARTESIAN_POINT ( 'NONE',  ( 0.4755220087074803481, 4.766607801171850497E-17, 0.000000000000000000 ) ) ;
#16125 = ORIENTED_EDGE ( 'NONE', *, *, #18830, .F. ) ;
#16126 = CARTESIAN_POINT ( 'NONE',  ( -0.9412147342319837628, -0.1574803149606297803, 0.2780511811023620439 ) ) ;
#16127 = CARTESIAN_POINT ( 'NONE',  ( 0.7185039370078692977, 0.06523048226347515077, 1.946358267609008097 ) ) ;
#16128 = CARTESIAN_POINT ( 'NONE',  ( 0.7185039370078739607, 1.928577636452523993E-17, 1.279527558947590515 ) ) ;
#16129 = ORIENTED_EDGE ( 'NONE', *, *, #10122, .F. ) ;
#16130 = CARTESIAN_POINT ( 'NONE',  ( 1.054774247047244540, -0.07405724077823318263, 1.988188976324187562 ) ) ;
#16131 = CARTESIAN_POINT ( 'NONE',  ( -0.8019270111902717657, -0.1787899950787401604, 1.038385826717890259 ) ) ;
#16132 = VECTOR ( 'NONE', #20973, 39.37007874015748854 ) ;
#16133 = CARTESIAN_POINT ( 'NONE',  ( 0.1608809465420318885, -0.1607368455565696963, 0.002813831971227527366 ) ) ;
#16134 = CARTESIAN_POINT ( 'NONE',  ( -0.6971942568897626646, -0.07405724077823297447, 0.04429133852891373180 ) ) ;
#16135 = ORIENTED_EDGE ( 'NONE', *, *, #42244, .F. ) ;
#16136 = CARTESIAN_POINT ( 'NONE',  ( -0.7646288533564489232, 0.1113553986120547346, 0.1722440943806619884 ) ) ;
#16137 = CARTESIAN_POINT ( 'NONE',  ( 0.1264236179284866091, -0.4483267715997795166, -0.1264236179284866091 ) ) ;
#16138 = CARTESIAN_POINT ( 'NONE',  ( 0.8070866141732283561, -0.0009842519685049383633, -0.6590551181102368705 ) ) ;
#16139 = VERTEX_POINT ( 'NONE', #21524 ) ;
#16140 = EDGE_CURVE ( 'NONE', #4083, #19285, #38315, .T. ) ;
#16141 = CARTESIAN_POINT ( 'NONE',  ( 0.8107537697050254399, 0.1574803149606300301, 1.468996062884598830 ) ) ;
#16142 = CARTESIAN_POINT ( 'NONE',  ( 0.8107537697050254399, -0.1574803149606297803, 0.7357283463491665065 ) ) ;
#16143 = ADVANCED_FACE ( 'NONE', ( #33996 ), #32179, .T. ) ;
#16144 = DIRECTION ( 'NONE',  ( 1.000000000000000000, 0.000000000000000000, -1.822029033848725275E-16 ) ) ;
#16145 = CARTESIAN_POINT ( 'NONE',  ( 0.7495606340400177148, 0.1264236179284866091, 1.651082677111590513 ) ) ;
#16146 = EDGE_CURVE ( 'NONE', #28970, #12246, #23750, .T. ) ;
#16147 = CARTESIAN_POINT ( 'NONE',  ( -0.1264236179284866091, -1.732775590497417362, 0.1264236179284866091 ) ) ;
#16148 = CYLINDRICAL_SURFACE ( 'NONE', #27266, 0.1574803149606299191 ) ;
#16149 = EDGE_CURVE ( 'NONE', #39085, #17112, #43198, .T. ) ;
#16150 = CARTESIAN_POINT ( 'NONE',  ( -0.7495606340400177148, -0.1264236179284866091, 0.6422244093950550958 ) ) ;
#16152 = CARTESIAN_POINT ( 'NONE',  ( 1.033464566929133799, 0.000000000000000000, 0.9842519683964094934 ) ) ;
#16151 = CARTESIAN_POINT ( 'NONE',  ( 0.1113553986120547346, -0.7509842519685040463, -0.1113553986120547346 ) ) ;
#16153 = CARTESIAN_POINT ( 'NONE',  ( 0.1797182628040039087, -1.553685541866510755, -0.07444174185955065859 ) ) ;
#16154 = CARTESIAN_POINT ( 'NONE',  ( 0.5314960629921260393, -1.928577636452524610E-17, 4.498031496062992574 ) ) ;
#16155 = CARTESIAN_POINT ( 'NONE',  ( 0.2471922904502825702, 0.07746962187842010295, -0.07828042841528085050 ) ) ;
#16156 = CARTESIAN_POINT ( 'NONE',  ( 0.9500414927467378812, 0.1787899950787401604, 1.569881889710015299 ) ) ;
#16157 = CARTESIAN_POINT ( 'NONE',  ( 0.7495606340400177148, 0.1264236179284866091, 1.808562992072220377 ) ) ;
#16158 = CARTESIAN_POINT ( 'NONE',  ( 0.8019270111902716547, -0.1787899950787401604, 0.2854330708123783977 ) ) ;
#16160 = ORIENTED_EDGE ( 'NONE', *, *, #29035, .T. ) ;
#16159 = CARTESIAN_POINT ( 'NONE',  ( 0.2397010884053811242, -3.032960542342102697E-32, 0.09842519685039370636 ) ) ;
#16161 = DIRECTION ( 'NONE',  ( 1.000000000000000000, -3.469446951953625233E-15, -2.725366053876155610E-32 ) ) ;
#16162 = DIRECTION ( 'NONE',  ( -1.000000000000000000, 0.000000000000000000, 0.000000000000000000 ) ) ;
#16163 = CARTESIAN_POINT ( 'NONE',  ( -0.1787899950787401882, -0.005413385773008132923, 0.000000000000000000 ) ) ;
#16164 = CARTESIAN_POINT ( 'NONE',  ( 1.002407869896990045, 0.1264236179284866091, 0.4995078739619842612 ) ) ;
#16165 = CARTESIAN_POINT ( 'NONE',  ( 0.5538057742782149795, 4.616380251121755931E-17, 0.000000000000000000 ) ) ;
#16166 = AXIS2_PLACEMENT_3D ( 'NONE', #30911, #45952, #2110 ) ;
#16167 = CARTESIAN_POINT ( 'NONE',  ( 0.7185039370078739607, 0.000000000000000000, 4.498031496062992574 ) ) ;
#16168 = CARTESIAN_POINT ( 'NONE',  ( -1.002407869896990045, -0.1264236179284866091, 1.316437007820252081 ) ) ;
#16169 = CARTESIAN_POINT ( 'NONE',  ( 0.7185039370078746268, -0.06523048226347956391, 0.8095472439869610959 ) ) ;
#16170 = VERTEX_POINT ( 'NONE', #637 ) ;
#16171 = CARTESIAN_POINT ( 'NONE',  ( 0.2642359194686346169, 4.766607801171850497E-17, 0.000000000000000000 ) ) ;
#16172 = CARTESIAN_POINT ( 'NONE',  ( 0.6971942568897637749, 2.189545951927499583E-17, 1.031003936954110189 ) ) ;
#16173 = EDGE_LOOP ( 'NONE', ( #25575, #23822, #39678, #5013 ) ) ;
#16174 = CARTESIAN_POINT ( 'NONE',  ( -0.1787899950787401882, -1.383366141678519678, 0.000000000000000000 ) ) ;
#16175 = CARTESIAN_POINT ( 'NONE',  ( -0.8107537697050253289, 0.1574803149606300301, 0.5634842518609766149 ) ) ;
#16176 = CIRCLE ( 'NONE', #805, 0.09842519685039310962 ) ;
#16177 = CARTESIAN_POINT ( 'NONE',  ( -0.7185039370078739607, 1.928577636452523993E-17, 0.8169291338582678197 ) ) ;
#16178 = CARTESIAN_POINT ( 'NONE',  ( 0.8019270111902717657, 0.1787899950787401604, 1.727362204670645385 ) ) ;
#16179 = CARTESIAN_POINT ( 'NONE',  ( -1.033464566929133799, 0.000000000000000000, 1.309055118110236338 ) ) ;
#16180 = DIRECTION ( 'NONE',  ( -1.000000000000000000, 0.000000000000000000, 0.000000000000000000 ) ) ;
#16182 = CARTESIAN_POINT ( 'NONE',  ( 0.1377952755905510474, 0.000000000000000000, -0.2610569382242185488 ) ) ;
#16181 = CARTESIAN_POINT ( 'NONE',  ( -0.8107537697050254399, 0.1574803149606300301, 0.7308070866141727073 ) ) ;
#16183 = CARTESIAN_POINT ( 'NONE',  ( -0.8107537697050254399, -0.1574803149606297803, 0.4995078739082208230 ) ) ;
#16184 = CONICAL_SURFACE ( 'NONE', #26125, 0.09842519685039310962, 0.7853981633972314524 ) ;
#16185 = CARTESIAN_POINT ( 'NONE',  ( 1.033464566929133799, 0.000000000000000000, 1.338582677057826853 ) ) ;
#16186 = ORIENTED_EDGE ( 'NONE', *, *, #22560, .T. ) ;
#16187 = VERTEX_POINT ( 'NONE', #19103 ) ;
#16188 = CARTESIAN_POINT ( 'NONE',  ( 0.1184675242425352465, -0.09842519685039370636, 2.185526306663015728 ) ) ;
#16189 = VECTOR ( 'NONE', #7771, 39.37007874015748143 ) ;
#16190 = CARTESIAN_POINT ( 'NONE',  ( 0.1574803149606300301, -0.0004921258767249256719, 0.06523048226347956391 ) ) ;
#16191 = CARTESIAN_POINT ( 'NONE',  ( -1.002407869896990045, 0.1264236179284866091, 1.488681102308440751 ) ) ;
#16192 = CARTESIAN_POINT ( 'NONE',  ( 0.9873396505805591694, 0.1113553986120547346, 1.855314960522393530 ) ) ;
#16193 = CARTESIAN_POINT ( 'NONE',  ( -1.033464566929136907, -0.06523048226347749612, 1.887303149498772425 ) ) ;
#16194 = CARTESIAN_POINT ( 'NONE',  ( -0.1264236179284866091, -1.044907432796167157, -0.1264236179284866091 ) ) ;
#16195 = ORIENTED_EDGE ( 'NONE', *, *, #15224, .T. ) ;
#16196 = EDGE_CURVE ( 'NONE', #27058, #9479, #12271, .T. ) ;
#16197 = CARTESIAN_POINT ( 'NONE',  ( -1.094772975963752103E-17, 0.02903543312462964626, -0.1787899950787401882 ) ) ;
#16198 = VERTEX_POINT ( 'NONE', #15783 ) ;
#16199 = ORIENTED_EDGE ( 'NONE', *, *, #22462, .F. ) ;
#16200 = DIRECTION ( 'NONE',  ( 0.000000000000000000, 0.000000000000000000, -1.000000000000000000 ) ) ;
#16201 = CARTESIAN_POINT ( 'NONE',  ( 1.033464566929133799, 0.000000000000000000, 0.1181102361129454797 ) ) ;
#16202 = ( BOUNDED_CURVE ( )  B_SPLINE_CURVE ( 2, ( #45124, #9449, #16628, #37724, #24063 ),
 .UNSPECIFIED., .F., .F. ) 
 B_SPLINE_CURVE_WITH_KNOTS ( ( 3, 2, 3 ),
 ( 0.9799999999999999822, 0.9825000000000000400, 0.9850000000591240257 ),
 .UNSPECIFIED. ) 
 CURVE ( )  GEOMETRIC_REPRESENTATION_ITEM ( )  RATIONAL_B_SPLINE_CURVE ( ( 1.000000000000000000, 0.9238795325112869605, 1.000000000000000000, 0.9238795325112869605, 1.000000000000000000 ) ) 
 REPRESENTATION_ITEM ( '' )  ) ;
#16203 = EDGE_CURVE ( 'NONE', #30928, #44478, #37311, .T. ) ;
#16204 = AXIS2_PLACEMENT_3D ( 'NONE', #2562, #17195, #46416 ) ;
#16205 = CARTESIAN_POINT ( 'NONE',  ( 0.9873396505805591694, -0.1113553986120547346, 1.776574803149606252 ) ) ;
#16206 = VECTOR ( 'NONE', #8276, 39.37007874015748143 ) ;
#16207 = AXIS2_PLACEMENT_3D ( 'NONE', #16586, #35508, #10094 ) ;
#16208 = CARTESIAN_POINT ( 'NONE',  ( 0.1264236179284866091, -0.6107283464029291675, -0.1264236179284866091 ) ) ;
#16209 = EDGE_CURVE ( 'NONE', #398, #7779, #3787, .T. ) ;
#16210 = VECTOR ( 'NONE', #25280, 39.37007874015748143 ) ;
#16211 = CARTESIAN_POINT ( 'NONE',  ( -1.002407869896990045, 0.1264236179284866091, 0.1894685038832444879 ) ) ;
#16212 = CARTESIAN_POINT ( 'NONE',  ( 0.2007874015748031815, 0.000000000000000000, 0.000000000000000000 ) ) ;
#16213 = CARTESIAN_POINT ( 'NONE',  ( -0.1797182628040039365, -1.103390266275958709, 0.000000000000000000 ) ) ;
#16214 = CARTESIAN_POINT ( 'NONE',  ( -1.033464566929133799, 0.000000000000000000, 1.033464566929133799 ) ) ;
#16215 = CARTESIAN_POINT ( 'NONE',  ( 0.7495606340400177148, -0.1264236179284866091, 1.035925196796629866 ) ) ;
#16216 = CARTESIAN_POINT ( 'NONE',  ( 1.054774247047244096, 0.000000000000000000, 0.1402559054580474474 ) ) ;
#16217 = FACE_OUTER_BOUND ( 'NONE', #17502, .T. ) ;
#16218 = CARTESIAN_POINT ( 'NONE',  ( 1.033464566929134687, 0.06523048226347956391, 1.547736220472440749 ) ) ;
#16220 = CARTESIAN_POINT ( 'NONE',  ( -0.7185039370078739607, 0.000000000000000000, -2.869337061179095023E-17 ) ) ;
#16219 = CARTESIAN_POINT ( 'NONE',  ( 0.7599549351170132860, 0.1127937001634502223, 1.980848792121916668 ) ) ;
#16221 = DIRECTION ( 'NONE',  ( 1.822029033848725028E-16, 0.000000000000000000, 1.000000000000000000 ) ) ;
#16222 = ( BOUNDED_CURVE ( )  B_SPLINE_CURVE ( 2, ( #21466, #10950, #25570, #3256, #3508, #11190, #4191, #14303, #18819 ),
 .UNSPECIFIED., .F., .F. ) 
 B_SPLINE_CURVE_WITH_KNOTS ( ( 3, 2, 2, 2, 3 ),
 ( 0.3800000000000000044, 0.3825000000000000067, 0.3850000000000000089, 0.3875000000000000111, 0.3900000000000000133 ),
 .UNSPECIFIED. ) 
 CURVE ( )  GEOMETRIC_REPRESENTATION_ITEM ( )  RATIONAL_B_SPLINE_CURVE ( ( 1.000000000000000000, 0.9238795325112869605, 1.000000000000000000, 0.9238795325112869605, 1.000000000000000000, 0.9238795325112869605, 1.000000000000000000, 0.9238795325112869605, 1.000000000000000000 ) ) 
 REPRESENTATION_ITEM ( '' )  ) ;
#16223 = CARTESIAN_POINT ( 'NONE',  ( -0.2066929133858267931, 0.5900595452500136950, -0.7440755677556079029 ) ) ;
#16224 = CARTESIAN_POINT ( 'NONE',  ( 0.6971942568897648851, -0.07405724077823297447, 1.028543307032851573 ) ) ;
#16225 = CARTESIAN_POINT ( 'NONE',  ( 1.054774247047244096, 0.000000000000000000, 1.759350393647023614 ) ) ;
#16226 = CARTESIAN_POINT ( 'NONE',  ( 1.033464566929133799, 0.000000000000000000, 0.3149606298137326843 ) ) ;
#16227 = ORIENTED_EDGE ( 'NONE', *, *, #39049, .F. ) ;
#16228 = CARTESIAN_POINT ( 'NONE',  ( 1.033464566929133799, 0.000000000000000000, 1.614173228238929170 ) ) ;
#16229 = CARTESIAN_POINT ( 'NONE',  ( 0.06523048226347956391, -1.683562992018456272, -0.1574803149606300301 ) ) ;
#16230 = CARTESIAN_POINT ( 'NONE',  ( -1.033464566929133799, 0.000000000000000000, 0.1968503935932602311 ) ) ;
#16231 = CARTESIAN_POINT ( 'NONE',  ( 0.8019270111902717657, -0.1787899950787401604, 1.230314960576156746 ) ) ;
#16232 = AXIS2_PLACEMENT_3D ( 'NONE', #31007, #13268, #23566 ) ;
#16233 = ORIENTED_EDGE ( 'NONE', *, *, #18654, .T. ) ;
#16234 = CARTESIAN_POINT ( 'NONE',  ( 0.3547871005709968273, 4.766607801171850497E-17, 0.000000000000000000 ) ) ;
#16235 = CARTESIAN_POINT ( 'NONE',  ( 0.07405724077823318263, 0.1299212598962831977, 0.1787899950787401604 ) ) ;
#16236 = EDGE_CURVE ( 'NONE', #3991, #3105, #44488, .T. ) ;
#16237 = CARTESIAN_POINT ( 'NONE',  ( -0.6971942568897637749, -2.189545951927502049E-17, 1.978346456692913646 ) ) ;
#16238 = AXIS2_PLACEMENT_3D ( 'NONE', #26114, #4499, #19134 ) ;
#16239 = CARTESIAN_POINT ( 'NONE',  ( -1.002407869896990045, -0.1264236179284866091, 0.6077755904974173617 ) ) ;
#16240 = CARTESIAN_POINT ( 'NONE',  ( 0.6141732283464567121, 0.000000000000000000, 0.000000000000000000 ) ) ;
#16241 = CARTESIAN_POINT ( 'NONE',  ( -0.05557684098944758871, 0.07733267719194715506, 0.2533457667601751728 ) ) ;
#16242 = ( REPRESENTATION_RELATIONSHIP ('NONE','NONE', #9609, #40498 ) REPRESENTATION_RELATIONSHIP_WITH_TRANSFORMATION ( #9174 )SHAPE_REPRESENTATION_RELATIONSHIP( ) ) ;
#16243 = CARTESIAN_POINT ( 'NONE',  ( 3.284318927891251994E-17, -1.531003936954110189, 0.1787899950787401882 ) ) ;
#16244 = VECTOR ( 'NONE', #36470, 39.37007874015748143 ) ;
#16245 = CARTESIAN_POINT ( 'NONE',  ( -1.054774247047244540, 0.07405724077823318263, 1.756889763725764553 ) ) ;
#16246 = ORIENTED_EDGE ( 'NONE', *, *, #6215, .F. ) ;
#16247 = CARTESIAN_POINT ( 'NONE',  ( -0.8759842519685039353, 0.1787899950787401882, 1.016240157426551161 ) ) ;
#16248 = ORIENTED_EDGE ( 'NONE', *, *, #38544, .T. ) ;
#16249 = CARTESIAN_POINT ( 'NONE',  ( 0.3123359580052492146, 0.08090551181102362266, 9.908067607274841931E-18 ) ) ;
#16250 = CARTESIAN_POINT ( 'NONE',  ( -0.3100393700787401619, 0.01127274112884939748, -1.043307086614172263 ) ) ;
#16251 = CARTESIAN_POINT ( 'NONE',  ( -1.094772975963752103E-17, -0.5773877477567976868, -0.1787899950787401882 ) ) ;
#16252 = CARTESIAN_POINT ( 'NONE',  ( 0.1974933268882626269, -0.08956039363871731718, -0.04058527935846337892 ) ) ;
#16253 = CARTESIAN_POINT ( 'NONE',  ( -0.1574803149606299191, 0.08669520607260540468, -0.1182208702464774136 ) ) ;
#16254 = CARTESIAN_POINT ( 'NONE',  ( -0.7495606340400177148, -0.1264236179284866091, 0.5191929133320630774 ) ) ;
#16255 = CARTESIAN_POINT ( 'NONE',  ( -0.07405724077823318263, -1.820005857993018505, 0.1787899950787401604 ) ) ;
#16256 = EDGE_CURVE ( 'NONE', #42055, #16808, #376, .T. ) ;
#16257 = ORIENTED_EDGE ( 'NONE', *, *, #30083, .F. ) ;
#16258 = CARTESIAN_POINT ( 'NONE',  ( -0.8019270111902716547, -0.1787899950787401604, 1.510826771599780294 ) ) ;
#16259 = VECTOR ( 'NONE', #3872, 39.37007874015748143 ) ;
#16260 = ADVANCED_FACE ( 'NONE', ( #11943 ), #37084, .T. ) ;
#16261 = CARTESIAN_POINT ( 'NONE',  ( 0.07405724077823318263, -1.513779527505292322, -0.1787899950787401604 ) ) ;
#16262 = DIRECTION ( 'NONE',  ( 0.000000000000000000, 0.000000000000000000, 1.000000000000000000 ) ) ;
#16263 = AXIS2_PLACEMENT_3D ( 'NONE', #42316, #6118, #20743 ) ;
#16264 = CARTESIAN_POINT ( 'NONE',  ( 1.033464566929134687, 0.06523048226347956391, 1.026082677057828185 ) ) ;
#16265 = DIRECTION ( 'NONE',  ( 0.000000000000000000, -1.224646799147353207E-16, 1.000000000000000000 ) ) ;
#16266 = CARTESIAN_POINT ( 'NONE',  ( 0.8759842519685039353, 0.1574803149606299191, 0.4921259842519685179 ) ) ;
#16267 = CARTESIAN_POINT ( 'NONE',  ( -0.1797182628040039087, -0.7515201875358006323, -0.07444174185955065859 ) ) ;
#16268 = CARTESIAN_POINT ( 'NONE',  ( -1.033464566929133799, 0.000000000000000000, 1.653543306979086580 ) ) ;
#16269 = CARTESIAN_POINT ( 'NONE',  ( -0.9873396505805591694, -0.1113553986120547346, 1.254921259734991912 ) ) ;
#16270 = CARTESIAN_POINT ( 'NONE',  ( 1.002407869896990045, 0.1264236179284866091, 0.5831692912848189803 ) ) ;
#16272 = DIRECTION ( 'NONE',  ( 0.000000000000000000, 0.000000000000000000, 1.000000000000000000 ) ) ;
#16271 = CARTESIAN_POINT ( 'NONE',  ( -0.06523048226347956391, -0.4286417322834646937, -0.1574803149606300301 ) ) ;
#16273 = CIRCLE ( 'NONE', #14720, 0.01968503937007875723 ) ;
#16274 = AXIS2_PLACEMENT_3D ( 'NONE', #46784, #10147, #39591 ) ;
#16275 = DIRECTION ( 'NONE',  ( 0.000000000000000000, -0.7880107536067207930, 0.6156614753256598460 ) ) ;
#16276 = ORIENTED_EDGE ( 'NONE', *, *, #27598, .T. ) ;
#16277 = CARTESIAN_POINT ( 'NONE',  ( 0.9412147342319837628, 0.1574803149606300301, 1.582185039262551607 ) ) ;
#16278 = CARTESIAN_POINT ( 'NONE',  ( 1.033464566929134687, 0.06523048226347956391, 1.114665354330708125 ) ) ;
#16279 = CARTESIAN_POINT ( 'NONE',  ( -0.9263122037349271753, -0.1687466150977034174, 1.989089231315331885 ) ) ;
#16281 = CARTESIAN_POINT ( 'NONE',  ( -0.7185039370078778465, -0.06523048226348396317, 1.951279527451527329 ) ) ;
#16280 = CARTESIAN_POINT ( 'NONE',  ( 0.8107537697050254399, 0.1574803149606300301, 0.1796259842519686567 ) ) ;
#16282 = FACE_BOUND ( 'NONE', #24824, .T. ) ;
#16283 = CARTESIAN_POINT ( 'NONE',  ( -0.1264236179284866091, -0.5073818897100158543, 0.1264236179284866091 ) ) ;
#16284 = ORIENTED_EDGE ( 'NONE', *, *, #43207, .T. ) ;
#16285 = CONICAL_SURFACE ( 'NONE', #36151, 0.09842519685039370636, 0.9599310885968824758 ) ;
#16286 = CARTESIAN_POINT ( 'NONE',  ( 0.7495606340400177148, 0.1264236179284866091, 0.7062007873478109987 ) ) ;
#16287 = ORIENTED_EDGE ( 'NONE', *, *, #6443, .F. ) ;
#16288 = CARTESIAN_POINT ( 'NONE',  ( -0.8759842519685039353, 0.000000000000000000, 0.000000000000000000 ) ) ;
#16289 = CARTESIAN_POINT ( 'NONE',  ( 0.9873396505805591694, -0.1113553986120547346, 0.9104330708661417804 ) ) ;
#16290 = CARTESIAN_POINT ( 'NONE',  ( -0.07405724077823318263, -1.700787401521039355, -0.1787899950787401604 ) ) ;
#16291 = CARTESIAN_POINT ( 'NONE',  ( -0.1787899950787401604, -0.9133858267178897039, -0.07405724077823318263 ) ) ;
#16292 = CARTESIAN_POINT ( 'NONE',  ( 0.1113553986120547346, -1.420275590551181244, -0.1113553986120547346 ) ) ;
#16293 = CARTESIAN_POINT ( 'NONE',  ( 1.033464566929134687, -0.06523048226347956391, 1.296751968396409049 ) ) ;
#16294 = EDGE_CURVE ( 'NONE', #12116, #4993, #39034, .T. ) ;
#16295 = CARTESIAN_POINT ( 'NONE',  ( 0.1564636162838598521, 0.1358284121151826784, -0.04551197418441087217 ) ) ;
#16296 = ORIENTED_EDGE ( 'NONE', *, *, #12646, .F. ) ;
#16297 = VERTEX_POINT ( 'NONE', #25843 ) ;
#16298 = CARTESIAN_POINT ( 'NONE',  ( -1.002407869896990045, -0.1264236179284866091, 1.715059055064346527 ) ) ;
#16299 = CARTESIAN_POINT ( 'NONE',  ( 0.8019270111902717657, 0.1787899950787401604, 1.850393700733638624 ) ) ;
#16300 = ORIENTED_EDGE ( 'NONE', *, *, #5750, .F. ) ;
#16301 = CARTESIAN_POINT ( 'NONE',  ( -0.1574803149606299191, -1.356299212490897466, 0.000000000000000000 ) ) ;
#16302 = CARTESIAN_POINT ( 'NONE',  ( 0.4736248074375449257, 2.177585298233984279, -3.731703755406948986 ) ) ;
#16303 = CARTESIAN_POINT ( 'NONE',  ( 1.002407869896990045, -0.1264236179284866091, 0.4552165353793071745 ) ) ;
#16304 = CARTESIAN_POINT ( 'NONE',  ( -0.7495606340400177148, -0.1264236179284866091, 1.345964566875370139 ) ) ;
#16305 = CARTESIAN_POINT ( 'NONE',  ( -0.8070866141732283561, -0.0009842519685049383633, 0.7574803149606299524 ) ) ;
#16306 = CARTESIAN_POINT ( 'NONE',  ( -1.002407869896990045, -0.1264236179284866091, 0.9227362204186770889 ) ) ;
#16307 = CARTESIAN_POINT ( 'NONE',  ( -0.9500414927467378812, 0.1787899950787401604, 0.03444881884387430981 ) ) ;
#16308 = ( GEOMETRIC_REPRESENTATION_CONTEXT ( 3 ) GLOBAL_UNCERTAINTY_ASSIGNED_CONTEXT ( ( #37360 ) ) GLOBAL_UNIT_ASSIGNED_CONTEXT ( ( #31442, #28313, #31914 ) ) REPRESENTATION_CONTEXT ( 'NONE', 'WORKASPACE' ) ) ;
#16309 = CARTESIAN_POINT ( 'NONE',  ( 0.6971942568897643300, 0.000000000000000000, 1.995570866087968520 ) ) ;
#16310 = CARTESIAN_POINT ( 'NONE',  ( -1.002407869896990045, -0.1264236179284866091, 1.793799212544661348 ) ) ;
#16311 = CARTESIAN_POINT ( 'NONE',  ( -0.7495606340400177148, 0.1264236179284866091, 0.08120078734781142893 ) ) ;
#16312 = CARTESIAN_POINT ( 'NONE',  ( -0.1806410355270206824, 0.08353766247254197641, 0.1811399203779236189 ) ) ;
#16313 = CARTESIAN_POINT ( 'NONE',  ( -0.7185039370078746268, 0.06523048226347956391, 1.719980314960629864 ) ) ;
#16314 = DIRECTION ( 'NONE',  ( 0.000000000000000000, 0.000000000000000000, -1.000000000000000000 ) ) ;
#16315 = EDGE_CURVE ( 'NONE', #44357, #42566, #4011, .T. ) ;
#16316 = CARTESIAN_POINT ( 'NONE',  ( 0.1815364857181279989, -0.09842519685039370636, -0.08952795644902836192 ) ) ;
#16317 = CARTESIAN_POINT ( 'NONE',  ( 0.7185039370078746268, -0.06523048226347956391, 1.006397637687749258 ) ) ;
#16318 = CARTESIAN_POINT ( 'NONE',  ( -0.9873396505805591694, 0.1113553986120547346, 1.786417322834645605 ) ) ;
#16319 = AXIS2_PLACEMENT_3D ( 'NONE', #8238, #18329, #18788 ) ;
#16320 = EDGE_CURVE ( 'NONE', #36603, #33652, #5559, .T. ) ;
#16321 = ORIENTED_EDGE ( 'NONE', *, *, #45438, .T. ) ;
#16322 = CIRCLE ( 'NONE', #20130, 0.1013779527559055538 ) ;
#16323 = ORIENTED_EDGE ( 'NONE', *, *, #3852, .T. ) ;
#16324 = EDGE_CURVE ( 'NONE', #16297, #13158, #12663, .T. ) ;
#16325 = CARTESIAN_POINT ( 'NONE',  ( 3.284318927891251994E-17, -1.250492125930488196, 0.1787899950787401882 ) ) ;
#16326 = PRODUCT_DEFINITION ( 'UNKNOWN', '', #12514, #13986 ) ;
#16327 = CARTESIAN_POINT ( 'NONE',  ( -0.9873396505805591694, -0.1113553986120547346, 0.5954724409448819422 ) ) ;
#16328 = CARTESIAN_POINT ( 'NONE',  ( -0.1270800023317771588, -0.2815398725751716569, -0.1270800023317771588 ) ) ;
#16329 = CARTESIAN_POINT ( 'NONE',  ( 0.1574803149606300301, -1.806594488081449512, -0.06523048226347956391 ) ) ;
#16330 = CARTESIAN_POINT ( 'NONE',  ( -0.9873396505805591694, -0.1113553986120547346, 0.8218503935932598425 ) ) ;
#16331 = B_SPLINE_CURVE_WITH_KNOTS ( 'NONE', 3,
 ( #28973, #18146, #29460, #3986, #39688, #47384, #32316, #18380, #32789, #14801, #146, #21259, #46894, #39936, #10259, #36600, #7365, #28730, #33022, #43530, #44005, #21747, #14085, #25593, #36378, #43774, #25821, #3758, #18607, #14328, #10500, #47144, #33266, #43300, #25098, #10977, #40165, #17668, #11208, #40399, #7585, #21495, #10745, #14556, #6875, #22199, #25354, #13838, #7124, #36835, #36129, #3284, #21977, #17906, #3535, #29227, #28482, #43053, #24863, #39465, #6640, #35884, #3037, #27015, #18841, #15511, #15751, #33967, #34201, #4212, #1328, #12394, #30386, #40861, #41561, #5168, #8056, #45172, #11912, #19318, #37530, #44465, #29691, #26055, #23404, #11678, #22439, #390, #41328, #1094, #44932, #26303, #37059, #30155, #33496, #15985, #37777, #26534, #12147, #15268, #29919, #23158, #19069, #40626, #44694, #33740, #22682, #851, #30607, #8768, #37284, #41094, #26770, #8529, #38007, #4438, #15041, #44232, #4930, #8289, #11438, #7822, #22917, #4688, #19554, #27255, #42297, #31080, #16219, #12630, #9955, #45644, #9006, #39167, #27955, #20496, #35137, #12861, #23631, #16682, #38241, #38478, #23866, #28179, #42523, #20023, #27494, #1566, #27732, #5399, #20724, #2047, #30849, #6338 ),
 .UNSPECIFIED., .F., .F.,
 ( 4, 2, 2, 2, 2, 1, 1, 1, 2, 2, 2, 2, 2, 1, 1, 1, 1, 2, 2, 2, 2, 2, 1, 1, 2, 2, 2, 2, 2, 1, 1, 2, 2, 2, 2, 1, 1, 1, 1, 2, 2, 2, 2, 2, 1, 2, 2, 2, 2, 2, 1, 1, 2, 2, 2, 2, 2, 2, 1, 1, 2, 2, 2, 2, 1, 1, 2, 2, 2, 2, 1, 2, 2, 2, 2, 1, 2, 2, 2, 2, 2, 2, 1, 1, 2, 2, 2, 2, 2, 4 ),
 ( 0.000000000000000000, 0.06249999999999325540, 0.09374999999998989697, 0.1093749999999879818, 0.1171874999999868022, 0.1210937499999859834, 0.1230468749999855532, 0.1240234374999851508, 0.1245117187499849426, 0.1249999999999847344, 0.1874999999999227007, 0.2187499999998916977, 0.2343749999998764877, 0.2421874999998691880, 0.2460937499998655520, 0.2480468749998637756, 0.2490234374998628597, 0.2495117187498623879, 0.2499999999998619160, 0.2812499999998631650, 0.2968749999998637756, 0.3046874999998641087, 0.3085937499998644418, 0.3105468749998647748, 0.3115234374998647748, 0.3124999999998648303, 0.3437499999998624989, 0.3593749999998612776, 0.3671874999998610001, 0.3710937499998608891, 0.3730468749998611111, 0.3740234374998612221, 0.3749999999998613331, 0.4062499999998746558, 0.4218749999998813172, 0.4296874999998846478, 0.4335937499998864242, 0.4355468749998873124, 0.4365234374998879230, 0.4370117187498884226, 0.4374999999998889777, 0.4687499999998933076, 0.4843749999998955835, 0.4921874999998967493, 0.4960937499998973599, 0.4980468749998976374, 0.4999999999998979150, 0.5312499999999020783, 0.5468749999999039657, 0.5546874999999050759, 0.5585937499999054090, 0.5605468749999055200, 0.5615234374999057421, 0.5624999999999059641, 0.5937499999999119593, 0.6093749999999149569, 0.6171874999999164002, 0.6210937499999171774, 0.6230468749999175104, 0.6240234374999177325, 0.6245117187499178435, 0.6249999999999179545, 0.6562499999999251710, 0.6718749999999289457, 0.6796874999999307221, 0.6835937499999317213, 0.6855468749999321654, 0.6874999999999326095, 0.7187499999999397149, 0.7343749999999433786, 0.7421874999999452660, 0.7460937499999461542, 0.7499999999999470424, 0.7812499999999529265, 0.7968749999999555911, 0.8046874999999568123, 0.8085937499999573674, 0.8105468749999575895, 0.8115234374999577005, 0.8124999999999578115, 0.8437499999999675815, 0.8593749999999722444, 0.8671874999999742428, 0.8710937499999750200, 0.8730468749999753530, 0.8749999999999756861, 0.9062499999999810152, 0.9218749999999840128, 0.9374999999999870104, 1.000000000000000000 ),
 .UNSPECIFIED. ) ;
#16332 = CARTESIAN_POINT ( 'NONE',  ( 2.892866454678787531E-17, -0.01771653543307086590, 0.1574803149606299191 ) ) ;
#16333 = CARTESIAN_POINT ( 'NONE',  ( 0.6971942568897626646, -0.07405724077823297447, 0.9498031495525356416 ) ) ;
#16334 = ( BOUNDED_CURVE ( )  B_SPLINE_CURVE ( 2, ( #11146, #32001, #46594, #13774, #25989, #22144, #11852, #33438, #33676 ),
 .UNSPECIFIED., .F., .T. ) 
 B_SPLINE_CURVE_WITH_KNOTS ( ( 3, 2, 2, 2, 3 ),
 ( 0.4299999999999999933, 0.4324999999999999956, 0.4349999999999999978, 0.4375000000000000000, 0.4400000000000000022 ),
 .UNSPECIFIED. ) 
 CURVE ( )  GEOMETRIC_REPRESENTATION_ITEM ( )  RATIONAL_B_SPLINE_CURVE ( ( 1.000000000000000000, 0.9238795325112869605, 1.000000000000000000, 0.9238795325112869605, 1.000000000000000000, 0.9238795325112869605, 1.000000000000000000, 0.9238795325112869605, 1.000000000000000000 ) ) 
 REPRESENTATION_ITEM ( '' )  ) ;
#16335 = VECTOR ( 'NONE', #5464, 39.37007874015748143 ) ;
#16336 = CARTESIAN_POINT ( 'NONE',  ( 0.06244181591614397786, 0.2594434330345316564, -0.05069326177275422507 ) ) ;
#16337 = CARTESIAN_POINT ( 'NONE',  ( 1.054774247047244540, 0.07405724077823318263, 1.919291338528913871 ) ) ;
#16338 = AXIS2_PLACEMENT_3D ( 'NONE', #18775, #23085, #33662 ) ;
#16339 = AXIS2_PLACEMENT_3D ( 'NONE', #4463, #30413, #22949 ) ;
#16340 = DIRECTION ( 'NONE',  ( 0.000000000000000000, 0.000000000000000000, -1.000000000000000000 ) ) ;
#16341 = CARTESIAN_POINT ( 'NONE',  ( 3.284318927891251994E-17, -0.4680118109698582773, 0.1787899950787401882 ) ) ;
#16342 = DIRECTION ( 'NONE',  ( 0.000000000000000000, 0.000000000000000000, 1.000000000000000000 ) ) ;
#16343 = CARTESIAN_POINT ( 'NONE',  ( 0.07405724077823318263, -1.444881889710016631, 0.1787899950787401604 ) ) ;
#16344 = CARTESIAN_POINT ( 'NONE',  ( 0.6971942568897626646, -0.07405724077823297447, 0.3248031495525359746 ) ) ;
#16345 = CARTESIAN_POINT ( 'NONE',  ( -0.8019270111902717657, -0.1787899950787401604, 1.860236220418677089 ) ) ;
#16346 = EDGE_LOOP ( 'NONE', ( #1404, #24613, #27905, #25913 ) ) ;
#16347 = CARTESIAN_POINT ( 'NONE',  ( -0.9500414927467378812, 0.1787899950787401604, 1.294291338528912982 ) ) ;
#16348 = CYLINDRICAL_SURFACE ( 'NONE', #31463, 0.1574803149606299191 ) ;
#16349 = CARTESIAN_POINT ( 'NONE',  ( -1.054774247047244096, 0.000000000000000000, 1.281988188922614125 ) ) ;
#16350 = EDGE_CURVE ( 'NONE', #40003, #13381, #18382, .T. ) ;
#16351 = CARTESIAN_POINT ( 'NONE',  ( -0.1545411696117860445, -0.09842519685039370636, -0.08990488994085453489 ) ) ;
#16352 = CARTESIAN_POINT ( 'NONE',  ( -1.033464566929133799, 0.000000000000000000, 0.9547244094488189781 ) ) ;
#16353 = CARTESIAN_POINT ( 'NONE',  ( 0.7495606340400177148, 0.1264236179284866091, 0.6323818897100157432 ) ) ;
#16354 = CARTESIAN_POINT ( 'NONE',  ( -0.9500414927467377701, -0.1787899950787401604, 0.5265748030958428139 ) ) ;
#16355 = CARTESIAN_POINT ( 'NONE',  ( -0.6971942568897626646, -0.07405724077823297447, 0.8316929133320636325 ) ) ;
#16356 = CARTESIAN_POINT ( 'NONE',  ( 0.1898890638025254318, -0.07836638817768155907, -0.1758005714383412132 ) ) ;
#16357 = FACE_OUTER_BOUND ( 'NONE', #14325, .T. ) ;
#16358 = ADVANCED_FACE ( 'NONE', ( #2079 ), #30412, .F. ) ;
#16359 = VERTEX_POINT ( 'NONE', #23191 ) ;
#16360 = EDGE_LOOP ( 'NONE', ( #12277, #45868, #39608, #39557 ) ) ;
#16361 = CARTESIAN_POINT ( 'NONE',  ( -0.9873396505805591694, -0.1113553986120547346, 0.3592519685039369803 ) ) ;
#16362 = ADVANCED_FACE ( 'NONE', ( #1595 ), #27288, .T. ) ;
#16363 = CARTESIAN_POINT ( 'NONE',  ( -0.2092529681372728712, -0.09851385015114920429, 0.1092847636717405591 ) ) ;
#16364 = DIRECTION ( 'NONE',  ( 1.000000000000000000, 0.000000000000000000, 0.000000000000000000 ) ) ;
#16365 = ORIENTED_EDGE ( 'NONE', *, *, #26695, .F. ) ;
#16366 = CARTESIAN_POINT ( 'NONE',  ( -0.7495606340400177148, 0.1264236179284866091, 0.9867125983714331028 ) ) ;
#16367 = CARTESIAN_POINT ( 'NONE',  ( -0.7495606340400177148, -0.1264236179284866091, 0.2042322834108035723 ) ) ;
#16368 = CARTESIAN_POINT ( 'NONE',  ( 0.1787899950787401882, -1.650222393426088896, -2.189545951927503898E-17 ) ) ;
#16369 = ORIENTED_EDGE ( 'NONE', *, *, #9535, .T. ) ;
#16370 = CARTESIAN_POINT ( 'NONE',  ( -0.3690944881889761664, 0.1574803149606353592, 0.7480314960629921295 ) ) ;
#16371 = CARTESIAN_POINT ( 'NONE',  ( -0.1787899950787401604, -0.5147637794737950356, -0.07405724077823318263 ) ) ;
#16372 = DIRECTION ( 'NONE',  ( 0.000000000000000000, -1.000000000000000000, 0.000000000000000000 ) ) ;
#16373 = CARTESIAN_POINT ( 'NONE',  ( 0.8759842519685039353, -0.1787899950787401882, 1.350885826717889815 ) ) ;
#16374 = CARTESIAN_POINT ( 'NONE',  ( -0.07267052686971341158, 0.2535370473722451390, -0.3104511204117335610 ) ) ;
#16375 = CARTESIAN_POINT ( 'NONE',  ( 0.000000000000000000, 0.000000000000000000, -0.4921259842519685179 ) ) ;
#16377 = EDGE_CURVE ( 'NONE', #17177, #22261, #34697, .T. ) ;
#16376 = CARTESIAN_POINT ( 'NONE',  ( 0.07405724077823318263, -0.2145669290800947537, -0.1787899950787401604 ) ) ;
#16378 = CARTESIAN_POINT ( 'NONE',  ( 0.7185039370078714072, 0.06523048226347728795, 1.877460629921259727 ) ) ;
#16379 = MECHANICAL_DESIGN_GEOMETRIC_PRESENTATION_REPRESENTATION (  '', ( #3365 ), #43888 ) ;
#16380 = CARTESIAN_POINT ( 'NONE',  ( -0.1264236179284866091, 0.1066673703534383871, 0.1264236179284866091 ) ) ;
#16381 = CARTESIAN_POINT ( 'NONE',  ( -0.07405724077823318263, -1.779527559001355952, -0.1787899950787401604 ) ) ;
#16382 = PRODUCT_CONTEXT ( 'NONE', #41312, 'mechanical' ) ;
#16383 = CARTESIAN_POINT ( 'NONE',  ( -1.033464566929134687, 0.06523048226347956391, 1.734744094380662904 ) ) ;
#16384 = CARTESIAN_POINT ( 'NONE',  ( 0.8019270111902717657, 0.1787899950787401604, 0.4281496062454490659 ) ) ;
#16385 = DIMENSIONAL_EXPONENTS ( 1.000000000000000000, 0.000000000000000000, 0.000000000000000000, 0.000000000000000000, 0.000000000000000000, 0.000000000000000000, 0.000000000000000000 ) ;
#16386 = CARTESIAN_POINT ( 'NONE',  ( -0.6971942568897648851, 0.07405724077823318263, 0.7529527558517473684 ) ) ;
#16388 = CARTESIAN_POINT ( 'NONE',  ( 2.892866454678787531E-17, 0.1003937007874015908, 0.1574803149606299191 ) ) ;
#16387 = CARTESIAN_POINT ( 'NONE',  ( -0.1574803149606300301, -0.8174212598425197873, -0.06523048226347956391 ) ) ;
#16389 = CARTESIAN_POINT ( 'NONE',  ( -0.1270800023317771588, -1.531539872575170991, 0.1270800023317771588 ) ) ;
#16390 = CARTESIAN_POINT ( 'NONE',  ( 2.892866454678787531E-17, -0.04724409438066189126, 0.1574803149606299191 ) ) ;
#16391 = CARTESIAN_POINT ( 'NONE',  ( 0.06523048226347956391, -0.4778543306011345249, 0.1574803149606297803 ) ) ;
#16392 = CARTESIAN_POINT ( 'NONE',  ( 0.1264236179284866091, -0.3794291338045042705, 0.1264236179284866091 ) ) ;
#16393 = DIRECTION ( 'NONE',  ( 0.000000000000000000, 1.000000000000000000, 0.000000000000000000 ) ) ;
#16394 = CARTESIAN_POINT ( 'NONE',  ( 0.7495606340400177148, 0.1264236179284866091, 1.459153543253322693 ) ) ;
#16395 = CARTESIAN_POINT ( 'NONE',  ( 0.8019270111902716547, -0.1787899950787401604, 1.781496062938362934 ) ) ;
#16396 = CARTESIAN_POINT ( 'NONE',  ( 0.8759842519685039353, 0.1787899950787401882, 0.4650590550643464716 ) ) ;
#16397 = DIRECTION ( 'NONE',  ( 0.000000000000000000, 0.000000000000000000, 1.000000000000000000 ) ) ;
#16398 = CARTESIAN_POINT ( 'NONE',  ( -0.7185039370078739607, 1.928577636452523993E-17, 0.5314960628845992741 ) ) ;
#16399 = CARTESIAN_POINT ( 'NONE',  ( 0.000000000000000000, 0.000000000000000000, 0.000000000000000000 ) ) ;
#16400 = CARTESIAN_POINT ( 'NONE',  ( 0.07405724077823318263, 0.06102362210100767403, -0.1787899950787401604 ) ) ;
#16401 = CARTESIAN_POINT ( 'NONE',  ( 0.8019270111902717657, -0.1787899950787401604, 0.4822834645131655606 ) ) ;
#16402 = FACE_OUTER_BOUND ( 'NONE', #41874, .T. ) ;
#16403 = DIRECTION ( 'NONE',  ( 0.000000000000000000, 1.000000000000000000, 0.000000000000000000 ) ) ;
#16404 = CARTESIAN_POINT ( 'NONE',  ( 0.8759842519685039353, 0.1574803149606299191, 0.2165354330708661457 ) ) ;
#16405 = CARTESIAN_POINT ( 'NONE',  ( 0.9412147342319837628, 0.1574803149606300301, 0.8341535431995593664 ) ) ;
#16406 = ORIENTED_EDGE ( 'NONE', *, *, #40234, .F. ) ;
#16407 = CARTESIAN_POINT ( 'NONE',  ( -0.7185039370078746268, 0.06523048226347956391, 0.8046259841444418637 ) ) ;
#16408 = CARTESIAN_POINT ( 'NONE',  ( 0.6971942568897648851, -0.07405724077823297447, 1.072834645615528659 ) ) ;
#16409 = ORIENTED_EDGE ( 'NONE', *, *, #11275, .T. ) ;
#16410 = EDGE_LOOP ( 'NONE', ( #32697, #31577, #41167, #40348 ) ) ;
#16411 = CARTESIAN_POINT ( 'NONE',  ( -0.8107537697050253289, -0.1574803149606297803, 0.4995078739082208230 ) ) ;
#16412 = CARTESIAN_POINT ( 'NONE',  ( -0.7646288533564489232, 0.1113553986120547346, 1.284448818897637956 ) ) ;
#16413 = EDGE_CURVE ( 'NONE', #19150, #17741, #26056, .T. ) ;
#16414 = CARTESIAN_POINT ( 'NONE',  ( -0.9412147342319837628, 0.1574803149606300301, 1.149114173120819427 ) ) ;
#16415 = DIRECTION ( 'NONE',  ( 0.000000000000000000, 1.000000000000000000, 0.000000000000000000 ) ) ;
#16416 = CARTESIAN_POINT ( 'NONE',  ( 1.002407869896990045, -0.1264236179284866091, 0.1796259841982051075 ) ) ;
#16417 = CARTESIAN_POINT ( 'NONE',  ( 0.8759842519685039353, 0.1574803149606299191, 1.427165354223181248 ) ) ;
#16418 = ORIENTED_EDGE ( 'NONE', *, *, #33149, .F. ) ;
#16419 = ORIENTED_EDGE ( 'NONE', *, *, #259, .T. ) ;
#16420 = EDGE_CURVE ( 'NONE', #7386, #9117, #9976, .T. ) ;
#16421 = LINE ( 'NONE', #45616, #42810 ) ;
#16422 = CIRCLE ( 'NONE', #28678, 0.09842519685039370636 ) ;
#16423 = EDGE_CURVE ( 'NONE', #21725, #30249, #44960, .T. ) ;
#16424 = CARTESIAN_POINT ( 'NONE',  ( -0.6971942568897648851, 0.07405724077823318263, 1.574803149552536530 ) ) ;
#16425 = CARTESIAN_POINT ( 'NONE',  ( -0.1113553986120547346, -0.1801181101286933040, -0.1113553986120547346 ) ) ;
#16426 = ORIENTED_EDGE ( 'NONE', *, *, #14951, .T. ) ;
#16427 = EDGE_CURVE ( 'NONE', #183, #7776, #9283, .T. ) ;
#16428 = CARTESIAN_POINT ( 'NONE',  ( -0.9412147342319837628, 0.1574803149606300301, 0.2436023620971973780 ) ) ;
#16429 = CARTESIAN_POINT ( 'NONE',  ( -0.6195511811023656223, 0.000000000000000000, -1.186023622047243986 ) ) ;
#16430 = CARTESIAN_POINT ( 'NONE',  ( 0.8107537697050254399, 0.1574803149606300301, 0.8784448817822366751 ) ) ;
#16431 = CARTESIAN_POINT ( 'NONE',  ( 0.1787899950787401604, -1.214690897363096989, -0.07405724077823318263 ) ) ;
#16432 = ORIENTED_EDGE ( 'NONE', *, *, #33471, .F. ) ;
#16433 = CARTESIAN_POINT ( 'NONE',  ( -1.094772975963752103E-17, -0.01033464561552785432, -0.1787899950787401882 ) ) ;
#16434 = EDGE_LOOP ( 'NONE', ( #14755, #1539, #32756, #17283 ) ) ;
#16435 = CARTESIAN_POINT ( 'NONE',  ( -0.7646288533564489232, -0.1113553986120547346, 1.402559055010582645 ) ) ;
#16436 = CARTESIAN_POINT ( 'NONE',  ( -0.9412147342319837628, -0.1574803149606297803, 1.459153543307085688 ) ) ;
#16437 = CARTESIAN_POINT ( 'NONE',  ( 0.8759842519685039353, -0.1574803149606299191, 1.889763779527559251 ) ) ;
#16438 = AXIS2_PLACEMENT_3D ( 'NONE', #6140, #9767, #20767 ) ;
#16439 = AXIS2_PLACEMENT_3D ( 'NONE', #24455, #37767, #12139 ) ;
#16440 = AXIS2_PLACEMENT_3D ( 'NONE', #37952, #5336, #41744 ) ;
#16441 = CARTESIAN_POINT ( 'NONE',  ( -0.1787899950787401604, -0.5541338582139530011, 0.07405724077823318263 ) ) ;
#16442 = CARTESIAN_POINT ( 'NONE',  ( -1.054774247047244096, 0.000000000000000000, 0.2239173227808822775 ) ) ;
#16443 = CARTESIAN_POINT ( 'NONE',  ( -0.8759842519685039353, 0.1574803149606299191, 1.003937007874015741 ) ) ;
#16444 = CARTESIAN_POINT ( 'NONE',  ( -0.1797182628040039365, -1.221500502496431162, 0.000000000000000000 ) ) ;
#16445 = FACE_OUTER_BOUND ( 'NONE', #35101, .T. ) ;
#16446 = CARTESIAN_POINT ( 'NONE',  ( 1.002407869896990045, -0.1264236179284866091, 1.006397637741511808 ) ) ;
#16447 = DIRECTION ( 'NONE',  ( -1.000000000000000000, 0.000000000000000000, 0.000000000000000000 ) ) ;
#16448 = CARTESIAN_POINT ( 'NONE',  ( 0.9412147342319837628, -0.1574803149606297803, 1.616633858267715551 ) ) ;
#16450 = DIRECTION ( 'NONE',  ( 0.000000000000000000, 1.000000000000000000, 0.000000000000000000 ) ) ;
#16449 = LINE ( 'NONE', #35368, #12959 ) ;
#16451 = DIRECTION ( 'NONE',  ( -1.000000000000000000, -5.372880794957870593E-15, 4.197754538034584604E-15 ) ) ;
#16452 = CYLINDRICAL_SURFACE ( 'NONE', #7727, 0.1574803149606299191 ) ;
#16453 = CARTESIAN_POINT ( 'NONE',  ( 0.8019270111902716547, -0.1787899950787401604, 1.033464566875371027 ) ) ;
#16454 = CARTESIAN_POINT ( 'NONE',  ( 0.9500414927467377701, -0.1787899950787401604, 1.870078740103715331 ) ) ;
#16455 = CARTESIAN_POINT ( 'NONE',  ( 0.9873396505805591694, -0.1113553986120547346, 0.3100393699712130080 ) ) ;
#16456 = ORIENTED_EDGE ( 'NONE', *, *, #8155, .F. ) ;
#16457 = CARTESIAN_POINT ( 'NONE',  ( 0.3649999999999999911, 0.1870078740157480324, 2.290185943287374283E-17 ) ) ;
#16458 = CARTESIAN_POINT ( 'NONE',  ( 0.1574803149606300301, -1.767224409341291658, -0.06523048226347956391 ) ) ;
#16459 = CARTESIAN_POINT ( 'NONE',  ( -0.9873396505805591694, 0.1113553986120547346, 0.2411417321759374011 ) ) ;
#16460 = CARTESIAN_POINT ( 'NONE',  ( 0.8759842519685039353, -0.1787899950787401882, 1.272145669237574772 ) ) ;
#16461 = DIRECTION ( 'NONE',  ( 0.000000000000000000, -0.2126700594528006805, 0.9771240687918512080 ) ) ;
#16462 = CARTESIAN_POINT ( 'NONE',  ( 0.1787899950787401604, 0.1397637795813224670, -0.07405724077823318263 ) ) ;
#16463 = CARTESIAN_POINT ( 'NONE',  ( -0.8759842519685039353, -0.1574803149606299191, 1.013779527451527551 ) ) ;
#16464 = ADVANCED_FACE ( 'NONE', ( #1358 ), #31432, .F. ) ;
#16465 = CARTESIAN_POINT ( 'NONE',  ( -0.9500414927467378812, 0.1787899950787401604, 0.5807086613635594752 ) ) ;
#16467 = CARTESIAN_POINT ( 'NONE',  ( 0.7185039370078739607, 1.928577636452523993E-17, 1.358267716427907779 ) ) ;
#16466 = VECTOR ( 'NONE', #23016, 39.37007874015748143 ) ;
#16468 = PLANE ( 'NONE',  #26881 ) ;
#16469 = ORIENTED_EDGE ( 'NONE', *, *, #23438, .F. ) ;
#16470 = DIRECTION ( 'NONE',  ( 1.822029033848725028E-16, 0.000000000000000000, 1.000000000000000000 ) ) ;
#16471 = ORIENTED_EDGE ( 'NONE', *, *, #13125, .F. ) ;
#16472 = CARTESIAN_POINT ( 'NONE',  ( -0.07405724077823318263, -1.587598425143086800, -0.1787899950787401604 ) ) ;
#16473 = AXIS2_PLACEMENT_3D ( 'NONE', #21237, #43514, #24376 ) ;
#16474 = CIRCLE ( 'NONE', #24143, 0.2559055118110236116 ) ;
#16475 = CARTESIAN_POINT ( 'NONE',  ( -0.9500414927467378812, -0.1787899950787401604, 1.786417322780882388 ) ) ;
#16476 = ORIENTED_EDGE ( 'NONE', *, *, #26756, .T. ) ;
#16477 = EDGE_CURVE ( 'NONE', #31750, #18573, #7681, .T. ) ;
#16478 = CARTESIAN_POINT ( 'NONE',  ( -0.9500414927467378812, 0.1787899950787401604, 0.6643700786863929730 ) ) ;
#16479 = EDGE_LOOP ( 'NONE', ( #42150, #27237, #15902 ) ) ;
#16480 = CARTESIAN_POINT ( 'NONE',  ( -0.2055371055870141295, 0.1768241869786838227, -0.3061783854717646802 ) ) ;
#16481 = DIRECTION ( 'NONE',  ( 0.000000000000000000, 0.000000000000000000, 1.000000000000000000 ) ) ;
#16482 = CARTESIAN_POINT ( 'NONE',  ( -0.1264236179284866091, -0.7299468028749075410, -0.1264236179284866091 ) ) ;
#16483 = CARTESIAN_POINT ( 'NONE',  ( 0.2021875001600378363, -0.08956021568874587835, -0.01555348493781427179 ) ) ;
#16484 = FACE_OUTER_BOUND ( 'NONE', #41476, .T. ) ;
#16485 = DIRECTION ( 'NONE',  ( 0.000000000000000000, 0.000000000000000000, 1.000000000000000000 ) ) ;
#16486 = CARTESIAN_POINT ( 'NONE',  ( -0.7185039370078739607, 1.928577636452523993E-17, 1.751968503829480106 ) ) ;
#16487 = CARTESIAN_POINT ( 'NONE',  ( -1.002407869896990045, 0.1264236179284866091, 0.5388779527021417826 ) ) ;
#16488 = CARTESIAN_POINT ( 'NONE',  ( -0.1787899950787401604, -1.824927117835538182, 0.07405724077823318263 ) ) ;
#16489 = CARTESIAN_POINT ( 'NONE',  ( -1.054774247047244540, -0.07405724077823318263, 1.599409448765134911 ) ) ;
#16490 = CARTESIAN_POINT ( 'NONE',  ( -0.1264236179284866091, -1.467027559001354398, -0.1264236179284866091 ) ) ;
#16491 = VERTEX_POINT ( 'NONE', #40372 ) ;
#16492 = EDGE_CURVE ( 'NONE', #22349, #35290, #8450, .T. ) ;
#16493 = CARTESIAN_POINT ( 'NONE',  ( -0.7185039370078739607, 1.928577636452523993E-17, 1.122047243986960652 ) ) ;
#16494 = ( BOUNDED_CURVE ( )  B_SPLINE_CURVE ( 2, ( #40848, #22669, #46050, #30141, #44682, #12134, #13258, #11900, #26521 ),
 .UNSPECIFIED., .F., .F. ) 
 B_SPLINE_CURVE_WITH_KNOTS ( ( 3, 2, 2, 2, 3 ),
 ( 0.6999999999999999556, 0.7025000000000000133, 0.7049999999999999600, 0.7075000000000000178, 0.7099999999999999645 ),
 .UNSPECIFIED. ) 
 CURVE ( )  GEOMETRIC_REPRESENTATION_ITEM ( )  RATIONAL_B_SPLINE_CURVE ( ( 1.000000000000000000, 0.9238795325112899581, 1.000000000000000000, 0.9238795325112869605, 1.000000000000000000, 0.9238795325112869605, 1.000000000000000000, 0.9238795325112799661, 1.000000000000000000 ) ) 
 REPRESENTATION_ITEM ( '' )  ) ;
#16495 = FACE_OUTER_BOUND ( 'NONE', #28689, .T. ) ;
#16496 = CARTESIAN_POINT ( 'NONE',  ( 0.1629747150817544565, -0.08009238079686641087, 0.1387239969760788449 ) ) ;
#16497 = CARTESIAN_POINT ( 'NONE',  ( -0.07444174185955065859, -0.7023075891106040913, 0.1797182628040039087 ) ) ;
#16498 = DIRECTION ( 'NONE',  ( 0.000000000000000000, 0.000000000000000000, -1.000000000000000000 ) ) ;
#16499 = CARTESIAN_POINT ( 'NONE',  ( -0.9412147342319837628, 0.1574803149606300301, 1.267224409341291436 ) ) ;
#16501 = CARTESIAN_POINT ( 'NONE',  ( 1.033464566929134687, -0.06523048226347956391, 1.769192913278299084 ) ) ;
#16500 = CARTESIAN_POINT ( 'NONE',  ( -0.1113553986120547346, -0.3868110236220472786, -0.1113553986120547346 ) ) ;
#16502 = VECTOR ( 'NONE', #34716, 39.37007874015748143 ) ;
#16503 = AXIS2_PLACEMENT_3D ( 'NONE', #7800, #19292, #37264 ) ;
#16504 = DIRECTION ( 'NONE',  ( 0.000000000000000000, 1.000000000000000000, 0.000000000000000000 ) ) ;
#16505 = ORIENTED_EDGE ( 'NONE', *, *, #44341, .T. ) ;
#16506 = CARTESIAN_POINT ( 'NONE',  ( 0.7185039370078739607, 0.000000000000000000, 4.498031496062992574 ) ) ;
#16507 = CARTESIAN_POINT ( 'NONE',  ( 1.033464566929134687, -0.06523048226347956391, 1.070374015748031038 ) ) ;
#16509 = CARTESIAN_POINT ( 'NONE',  ( -0.8938872902679191323, -0.1741726370573033755, 1.988501741345521712 ) ) ;
#16508 = CARTESIAN_POINT ( 'NONE',  ( -0.7185039370078714072, 0.06523048226347728795, 1.277066929026331232 ) ) ;
#16510 = CARTESIAN_POINT ( 'NONE',  ( 1.033464566929133799, 0.000000000000000000, 0.3149606298137326843 ) ) ;
#16512 = FACE_OUTER_BOUND ( 'NONE', #18994, .T. ) ;
#16511 = CARTESIAN_POINT ( 'NONE',  ( 0.9873396505805591694, -0.1113553986120547346, 0.5856299211523157133 ) ) ;
#16513 = CARTESIAN_POINT ( 'NONE',  ( 0.9873396505805591694, 0.1113553986120547346, 1.264763779420031486 ) ) ;
#16514 = CARTESIAN_POINT ( 'NONE',  ( -0.1642785720453234233, -0.08956005481713959215, -0.05376805096173911669 ) ) ;
#16515 = CARTESIAN_POINT ( 'NONE',  ( -0.1787899950787401882, -0.5123031495525355306, 0.000000000000000000 ) ) ;
#16516 = ORIENTED_EDGE ( 'NONE', *, *, #26901, .T. ) ;
#16517 = CARTESIAN_POINT ( 'NONE',  ( 0.7185039370078739607, 1.928577636452523993E-17, 0.8562992125984251190 ) ) ;
#16518 = CARTESIAN_POINT ( 'NONE',  ( 1.054774247047244540, -0.07405724077823318263, 0.8858267715997791836 ) ) ;
#16519 = ORIENTED_EDGE ( 'NONE', *, *, #43386, .F. ) ;
#16520 = DIRECTION ( 'NONE',  ( 1.000000000000000000, 0.000000000000000000, -1.822029033848725275E-16 ) ) ;
#16521 = DIRECTION ( 'NONE',  ( -1.000000000000000000, 0.000000000000000000, 0.000000000000000000 ) ) ;
#16522 = CARTESIAN_POINT ( 'NONE',  ( -1.094772975963752103E-17, -1.781988188922614347, -0.1787899950787401882 ) ) ;
#16523 = CARTESIAN_POINT ( 'NONE',  ( 0.07405724077823318263, -0.9773622046706458288, 0.1787899950787401604 ) ) ;
#16524 = CARTESIAN_POINT ( 'NONE',  ( -0.1574803149606300301, -1.289862204724410155, -0.06523048226347956391 ) ) ;
#16525 = CARTESIAN_POINT ( 'NONE',  ( 0.8107537697050253289, 0.1574803149606300301, 1.232775590443654812 ) ) ;
#16526 = CARTESIAN_POINT ( 'NONE',  ( 0.7646288533564489232, -0.1113553986120547346, 1.166338582569637961 ) ) ;
#16527 = EDGE_CURVE ( 'NONE', #31115, #3834, #7798, .T. ) ;
#16528 = ORIENTED_EDGE ( 'NONE', *, *, #35815, .F. ) ;
#16529 = ORIENTED_EDGE ( 'NONE', *, *, #16885, .F. ) ;
#16530 = CARTESIAN_POINT ( 'NONE',  ( -1.054774247047244540, 0.07405724077823318263, 1.840551181048599938 ) ) ;
#16531 = CARTESIAN_POINT ( 'NONE',  ( 1.054774247047244540, 0.07405724077823318263, 1.879921259788756016 ) ) ;
#16532 = ORIENTED_EDGE ( 'NONE', *, *, #37986, .F. ) ;
#16533 = CARTESIAN_POINT ( 'NONE',  ( 0.1574803149606300301, 0.004429133965794757564, -0.06523048226347956391 ) ) ;
#16534 = CARTESIAN_POINT ( 'NONE',  ( 1.054774247047244540, 0.07405724077823318263, 0.3838582676627718127 ) ) ;
#16535 = CARTESIAN_POINT ( 'NONE',  ( -0.8759842519685039353, -0.1787899950787401882, 1.390255905458047447 ) ) ;
#16536 = VECTOR ( 'NONE', #40409, 39.37007874015748143 ) ;
#16537 = CARTESIAN_POINT ( 'NONE',  ( 1.033464566929133799, 0.000000000000000000, 1.624015748031496287 ) ) ;
#16538 = EDGE_CURVE ( 'NONE', #8711, #3940, #5277, .T. ) ;
#16539 = CARTESIAN_POINT ( 'NONE',  ( -0.6971942568897626646, -0.07405724077823297447, 0.2854330708123783422 ) ) ;
#16540 = CARTESIAN_POINT ( 'NONE',  ( -0.2227678560577956990, 0.05525422739379964865, -0.1568179892043777002 ) ) ;
#16541 = CARTESIAN_POINT ( 'NONE',  ( -0.8759842519685039353, -0.1787899950787401882, 1.749507873961984483 ) ) ;
#16542 = CARTESIAN_POINT ( 'NONE',  ( -0.9500414927467378812, 0.1787899950787401604, 0.1131889763241892138 ) ) ;
#16543 = CARTESIAN_POINT ( 'NONE',  ( 0.03810507699822260341, -0.06563552548610589177, -0.2634293601846930399 ) ) ;
#16544 = CARTESIAN_POINT ( 'NONE',  ( -0.8759842519685039353, 0.1574803149606299191, 1.712598425196850238 ) ) ;
#16545 = CARTESIAN_POINT ( 'NONE',  ( 0.3302522695077432791, 4.466152701071653354E-17, 0.000000000000000000 ) ) ;
#16546 = CARTESIAN_POINT ( 'NONE',  ( 0.8759842519685039353, -0.1787899950787401882, 1.710137795221826851 ) ) ;
#16547 = CARTESIAN_POINT ( 'NONE',  ( 0.1576911482518127960, -0.09842519685039370636, -0.1232761894637649652 ) ) ;
#16548 = AXIS2_PLACEMENT_3D ( 'NONE', #13708, #42915, #10125 ) ;
#16549 = VERTEX_POINT ( 'NONE', #20234 ) ;
#16550 = CARTESIAN_POINT ( 'NONE',  ( -0.1264236179284866091, -1.063484251914740275, 0.1264236179284866091 ) ) ;
#16551 = EDGE_CURVE ( 'NONE', #9479, #14069, #41539, .T. ) ;
#16552 = CARTESIAN_POINT ( 'NONE',  ( -0.07405724077823318263, -1.267716535379307619, -0.1787899950787401604 ) ) ;
#16553 = FACE_OUTER_BOUND ( 'NONE', #1778, .T. ) ;
#16554 = DIRECTION ( 'NONE',  ( 0.000000000000000000, -0.6156614753256597350, -0.7880107536067207930 ) ) ;
#16555 = CARTESIAN_POINT ( 'NONE',  ( -0.9412147342319837628, -0.1574803149606297803, 0.7800196849318438153 ) ) ;
#16556 = CARTESIAN_POINT ( 'NONE',  ( 0.1574803149606299191, 0.03149606299212598381, -1.928577636452523993E-17 ) ) ;
#16557 = CIRCLE ( 'NONE', #8120, 0.2471922904502826812 ) ;
#16558 = CARTESIAN_POINT ( 'NONE',  ( 0.8019270111902717657, 0.1787899950787401604, 0.9399606298674970661 ) ) ;
#16559 = CARTESIAN_POINT ( 'NONE',  ( 0.1889095778402860304, 0.1864272366438185224, -0.04769437235510193968 ) ) ;
#16560 = CARTESIAN_POINT ( 'NONE',  ( 0.8759842519685039353, -0.1787899950787401882, 1.985728346402929168 ) ) ;
#16561 = EDGE_CURVE ( 'NONE', #35279, #21057, #13101, .T. ) ;
#16562 = ORIENTED_EDGE ( 'NONE', *, *, #7808, .F. ) ;
#16563 = CARTESIAN_POINT ( 'NONE',  ( 0.8759842519685039353, -0.1574803149606299191, 0.1968503937007874127 ) ) ;
#16564 = DIRECTION ( 'NONE',  ( 1.000000000000000000, 0.000000000000000000, -1.822029033848725275E-16 ) ) ;
#16565 = CARTESIAN_POINT ( 'NONE',  ( -0.1264236179284866091, -0.4434055117572598959, -0.1264236179284866091 ) ) ;
#16566 = CARTESIAN_POINT ( 'NONE',  ( 0.000000000000000000, 0.000000000000000000, -0.1045766232635885612 ) ) ;
#16567 = CARTESIAN_POINT ( 'NONE',  ( 3.284318927891251994E-17, -1.329232283410803239, 0.1787899950787401882 ) ) ;
#16568 = CARTESIAN_POINT ( 'NONE',  ( 0.6971942568897626646, 0.07405724077823318263, 0.3592519684501735977 ) ) ;
#16569 = CARTESIAN_POINT ( 'NONE',  ( -0.8759842519685039353, 0.000000000000000000, 0.000000000000000000 ) ) ;
#16570 = EDGE_CURVE ( 'NONE', #17791, #36844, #1542, .T. ) ;
#16571 = CARTESIAN_POINT ( 'NONE',  ( -0.6971942568897648851, 0.07405724077823318263, 1.850393700733638624 ) ) ;
#16572 = ORIENTED_EDGE ( 'NONE', *, *, #9036, .F. ) ;
#16573 = CARTESIAN_POINT ( 'NONE',  ( -0.8019270111902717657, 0.1787899950787401604, 1.417322834591906222 ) ) ;
#16574 = DIRECTION ( 'NONE',  ( 1.000000000000000000, 0.000000000000000000, 0.000000000000000000 ) ) ;
#16575 = CARTESIAN_POINT ( 'NONE',  ( 1.054774247047244540, -0.07405724077823318263, 1.402559055064346971 ) ) ;
#16576 = CARTESIAN_POINT ( 'NONE',  ( -0.1377952755905510474, 1.687505431895957955E-17, -0.2610569382242185488 ) ) ;
#16577 = CARTESIAN_POINT ( 'NONE',  ( 0.06523048226347956391, -1.225885826664126155, 0.1574803149606297803 ) ) ;
#16578 = CARTESIAN_POINT ( 'NONE',  ( -0.7495606340400177148, -0.1264236179284866091, 0.5634842519147401640 ) ) ;
#16579 = CARTESIAN_POINT ( 'NONE',  ( 0.8019270111902717657, 0.1787899950787401604, 0.07874015742655145200 ) ) ;
#16580 = CARTESIAN_POINT ( 'NONE',  ( -0.7495606340400177148, 0.1264236179284866091, 1.178641732229700922 ) ) ;
#16581 = CARTESIAN_POINT ( 'NONE',  ( 0.1441367711531681417, -0.09842284166182276028, -0.1062059330993350148 ) ) ;
#16582 = LINE ( 'NONE', #38373, #35415 ) ;
#16583 = CARTESIAN_POINT ( 'NONE',  ( 1.054774247047244096, 0.000000000000000000, 0.5782480314422993040 ) ) ;
#16584 = CARTESIAN_POINT ( 'NONE',  ( -0.7495606340400177148, 0.1264236179284866091, 0.5093503936470236138 ) ) ;
#16585 = ADVANCED_FACE ( 'NONE', ( #38454 ), #16657, .F. ) ;
#16586 = CARTESIAN_POINT ( 'NONE',  ( 0.000000000000000000, 0.000000000000000000, -0.3149606299212598381 ) ) ;
#16587 = DIRECTION ( 'NONE',  ( 0.6018150231520356108, -0.000000000000000000, -0.7986355100473022661 ) ) ;
#16588 = EDGE_LOOP ( 'NONE', ( #22013, #23169, #44740, #11334 ) ) ;
#16589 = DIRECTION ( 'NONE',  ( 1.822029033848725028E-16, 0.000000000000000000, 1.000000000000000000 ) ) ;
#16590 = CARTESIAN_POINT ( 'NONE',  ( -0.7646288533564489232, -0.1113553986120547346, 0.3100393700787401619 ) ) ;
#16591 = CARTESIAN_POINT ( 'NONE',  ( 1.054774247047244540, 0.07405724077823318263, 1.328740157426552049 ) ) ;
#16592 = CARTESIAN_POINT ( 'NONE',  ( 0.1098255079058281514, -0.09851384733571673380, 0.1889249215128767645 ) ) ;
#16593 = VERTEX_POINT ( 'NONE', #4906 ) ;
#16594 = CARTESIAN_POINT ( 'NONE',  ( -0.7646288533564489232, -0.1113553986120547346, 0.5462598425196850682 ) ) ;
#16595 = CARTESIAN_POINT ( 'NONE',  ( -0.8759842519685039353, -0.1787899950787401882, 1.001476377898992132 ) ) ;
#16596 = CARTESIAN_POINT ( 'NONE',  ( -1.054774247047244540, -0.07405724077823318263, 0.2165354330171024577 ) ) ;
#16597 = ORIENTED_EDGE ( 'NONE', *, *, #16561, .F. ) ;
#16598 = FACE_OUTER_BOUND ( 'NONE', #32707, .T. ) ;
#16599 = CARTESIAN_POINT ( 'NONE',  ( 0.1787899950787401604, -0.6131889763241887836, 0.07405724077823318263 ) ) ;
#16600 = ORIENTED_EDGE ( 'NONE', *, *, #1017, .F. ) ;
#16601 = CARTESIAN_POINT ( 'NONE',  ( 0.002317115957707514655, 0.1361028492807104251, 0.03985382897102638516 ) ) ;
#16602 = DIRECTION ( 'NONE',  ( 1.000000000000000000, 0.000000000000000000, -1.822029033848725275E-16 ) ) ;
#16603 = ( BOUNDED_CURVE ( )  B_SPLINE_CURVE ( 2, ( #46278, #27646, #16594, #13469, #38387, #2884, #35519, #17290, #42895 ),
 .UNSPECIFIED., .F., .T. ) 
 B_SPLINE_CURVE_WITH_KNOTS ( ( 3, 2, 2, 2, 3 ),
 ( 0.2700000000000000178, 0.2725000000000000200, 0.2750000000000000222, 0.2775000000000000244, 0.2800000000000000266 ),
 .UNSPECIFIED. ) 
 CURVE ( )  GEOMETRIC_REPRESENTATION_ITEM ( )  RATIONAL_B_SPLINE_CURVE ( ( 1.000000000000000000, 0.9238795325112869605, 1.000000000000000000, 0.9238795325112869605, 1.000000000000000000, 0.9238795325112869605, 1.000000000000000000, 0.9238795325112869605, 1.000000000000000000 ) ) 
 REPRESENTATION_ITEM ( '' )  ) ;
#16604 = CARTESIAN_POINT ( 'NONE',  ( -0.1787899950787401882, -0.8272637794737952577, 0.000000000000000000 ) ) ;
#16605 = DIRECTION ( 'NONE',  ( 0.000000000000000000, 0.000000000000000000, -1.000000000000000000 ) ) ;
#16606 = DIRECTION ( 'NONE',  ( 0.000000000000000000, 0.000000000000000000, 1.000000000000000000 ) ) ;
#16607 = CARTESIAN_POINT ( 'NONE',  ( 0.7495606340400177148, 0.1264236179284866091, 1.611712598371433103 ) ) ;
#16608 = CARTESIAN_POINT ( 'NONE',  ( -0.07405724077823318263, 0.03038784279438331778, 0.1787899950787401604 ) ) ;
#16609 = CARTESIAN_POINT ( 'NONE',  ( 0.07405724077823318263, -1.799212598371432659, 0.1787899950787401604 ) ) ;
#16610 = PRODUCT_CONTEXT ( 'NONE', #6132, 'mechanical' ) ;
#16611 = EDGE_CURVE ( 'NONE', #42642, #9764, #41785, .T. ) ;
#16612 = DIRECTION ( 'NONE',  ( 0.000000000000000000, -1.000000000000000000, 0.000000000000000000 ) ) ;
#16613 = AXIS2_PLACEMENT_3D ( 'NONE', #18982, #41469, #41231 ) ;
#16614 = CARTESIAN_POINT ( 'NONE',  ( -0.8019270111902716547, 0.1787899950787401604, 0.7480314960092282472 ) ) ;
#16616 = LINE ( 'NONE', #37950, #7795 ) ;
#16615 = CARTESIAN_POINT ( 'NONE',  ( -9.642888182262618425E-18, -0.8641732283464567121, -0.1574803149606299191 ) ) ;
#16617 = CARTESIAN_POINT ( 'NONE',  ( -0.07444174185955065859, -1.607819400134226528, 0.1797182628040039087 ) ) ;
#16618 = CARTESIAN_POINT ( 'NONE',  ( 1.002407869896990045, -0.1264236179284866091, 1.557578740103716441 ) ) ;
#16619 = CARTESIAN_POINT ( 'NONE',  ( 0.6971942568897648851, 0.07405724077823318263, 1.811023621993480548 ) ) ;
#16620 = CARTESIAN_POINT ( 'NONE',  ( 1.054774247047244096, 0.000000000000000000, 0.3764763778989925203 ) ) ;
#16621 = ADVANCED_FACE ( 'NONE', ( #30365 ), #37751, .T. ) ;
#16623 = EDGE_LOOP ( 'NONE', ( #11176, #44889, #39910, #2287 ) ) ;
#16622 = CARTESIAN_POINT ( 'NONE',  ( -0.7185039370078732945, -0.06523048226347920309, 0.1402559054042840370 ) ) ;
#16624 = CARTESIAN_POINT ( 'NONE',  ( -0.1574803149606299191, 0.5900595452500136950, -0.7440755677556079029 ) ) ;
#16625 = CARTESIAN_POINT ( 'NONE',  ( 0.07405724077823318263, 0.1003937008411650705, -0.1787899950787401604 ) ) ;
#16626 = CARTESIAN_POINT ( 'NONE',  ( 1.002407869896990045, 0.1264236179284866091, 0.3813976377415121966 ) ) ;
#16628 = CARTESIAN_POINT ( 'NONE',  ( 0.9873396505805591694, 0.1113553986120547346, 1.973425196742866206 ) ) ;
#16627 = CARTESIAN_POINT ( 'NONE',  ( 0.9500414927467377701, -0.1787899950787401604, 1.313976377898992132 ) ) ;
#16629 = CARTESIAN_POINT ( 'NONE',  ( -0.7646288533564489232, 0.1113553986120547346, 1.589566929026330566 ) ) ;
#16630 = CARTESIAN_POINT ( 'NONE',  ( -1.002407869896990045, 0.1264236179284866091, 1.444389763725763665 ) ) ;
#16631 = CARTESIAN_POINT ( 'NONE',  ( 0.8107537697050253289, -0.1574803149606297803, 0.7357283463491665065 ) ) ;
#16632 = ORIENTED_EDGE ( 'NONE', *, *, #7523, .T. ) ;
#16633 = DIRECTION ( 'NONE',  ( 1.822029033848725028E-16, 0.000000000000000000, 1.000000000000000000 ) ) ;
#16634 = CARTESIAN_POINT ( 'NONE',  ( 1.054774247047244096, 0.000000000000000000, 0.9719488188438739629 ) ) ;
#16635 = VERTEX_POINT ( 'NONE', #9472 ) ;
#16637 = ORIENTED_EDGE ( 'NONE', *, *, #35297, .T. ) ;
#16636 = CARTESIAN_POINT ( 'NONE',  ( 0.07405724077823318263, -1.316929133804503937, -0.1787899950787401604 ) ) ;
#16638 = CARTESIAN_POINT ( 'NONE',  ( -0.9873396505805591694, 0.1113553986120547346, 0.5167322833570401341 ) ) ;
#16639 = CYLINDRICAL_SURFACE ( 'NONE', #29490, 0.1574803149606299191 ) ;
#16640 = CARTESIAN_POINT ( 'NONE',  ( 0.8019270111902717657, -0.1787899950787401604, 1.663385826717890925 ) ) ;
#16641 = CARTESIAN_POINT ( 'NONE',  ( -0.9873396505805591694, 0.1113553986120547346, 1.392716535433070835 ) ) ;
#16642 = PLANE ( 'NONE',  #13628 ) ;
#16644 = LINE ( 'NONE', #6780, #10938 ) ;
#16643 = CARTESIAN_POINT ( 'NONE',  ( 0.2471922904502826812, 0.03219022224904102836, -0.1427165354330708902 ) ) ;
#16645 = CARTESIAN_POINT ( 'NONE',  ( 0.7495606340400177148, 0.1264236179284866091, 0.1993110235682838682 ) ) ;
#16646 = ADVANCED_FACE ( 'NONE', ( #5378 ), #19527, .T. ) ;
#16647 = CARTESIAN_POINT ( 'NONE',  ( 0.8759842519685039353, 0.1574803149606299191, 1.387795275483023616 ) ) ;
#16648 = VERTEX_POINT ( 'NONE', #26990 ) ;
#16649 = ORIENTED_EDGE ( 'NONE', *, *, #42061, .F. ) ;
#16650 = EDGE_CURVE ( 'NONE', #15531, #27462, #29185, .T. ) ;
#16651 = PLANE ( 'NONE',  #734 ) ;
#16652 = CARTESIAN_POINT ( 'NONE',  ( 0.7185039370078746268, -0.06523048226347956391, 0.5831692913385827515 ) ) ;
#16653 = CARTESIAN_POINT ( 'NONE',  ( 0.6971942568897648851, 0.07405724077823318263, 0.9498031495525356416 ) ) ;
#16654 = CARTESIAN_POINT ( 'NONE',  ( -0.8759842519685039353, 0.1787899950787401882, 1.646161417269070837 ) ) ;
#16655 = CARTESIAN_POINT ( 'NONE',  ( -0.1574803149606299191, -0.2145669290263310935, 0.000000000000000000 ) ) ;
#16656 = EDGE_LOOP ( 'NONE', ( #26265, #16945, #37441, #2261 ) ) ;
#16657 = CYLINDRICAL_SURFACE ( 'NONE', #43646, 0.09842519685039310962 ) ;
#16658 = DIRECTION ( 'NONE',  ( 1.000000000000000000, 0.000000000000000000, 0.000000000000000000 ) ) ;
#16659 = CARTESIAN_POINT ( 'NONE',  ( -0.1787899950787401604, -1.195005857993017839, 0.07405724077823318263 ) ) ;
#16660 = ORIENTED_EDGE ( 'NONE', *, *, #15497, .F. ) ;
#16661 = CARTESIAN_POINT ( 'NONE',  ( -1.094772975963752103E-17, -0.08907480309584270284, -0.1787899950787401882 ) ) ;
#16662 = EDGE_LOOP ( 'NONE', ( #13962, #3513, #20540, #37451 ) ) ;
#16663 = ORIENTED_EDGE ( 'NONE', *, *, #16611, .T. ) ;
#16664 = CARTESIAN_POINT ( 'NONE',  ( -0.2559055118110236116, 0.000000000000000000, -0.3149606299212598381 ) ) ;
#16665 = CARTESIAN_POINT ( 'NONE',  ( -0.7185039370078739607, 1.928577636452523993E-17, 0.9251968502861732668 ) ) ;
#16666 = CARTESIAN_POINT ( 'NONE',  ( 0.9873396505805591694, 0.1113553986120547346, 1.825787401574803237 ) ) ;
#16667 = CARTESIAN_POINT ( 'NONE',  ( -0.1787899950787401604, -0.5984251967966303098, -0.07405724077823318263 ) ) ;
#16668 = EDGE_CURVE ( 'NONE', #22426, #4083, #8923, .T. ) ;
#16669 = EDGE_CURVE ( 'NONE', #24988, #2951, #24317, .T. ) ;
#16670 = CARTESIAN_POINT ( 'NONE',  ( -0.8019270111902716547, -0.1787899950787401604, 0.2903543306548980185 ) ) ;
#16671 = CARTESIAN_POINT ( 'NONE',  ( -0.9873396505805591694, 0.1113553986120547346, 1.077755905511811108 ) ) ;
#16672 = VECTOR ( 'NONE', #29405, 39.37007874015748143 ) ;
#16673 = CARTESIAN_POINT ( 'NONE',  ( 0.07444174185955065859, -1.091087116669658963, 0.1797182628040039087 ) ) ;
#16674 = DIRECTION ( 'NONE',  ( -1.000000000000000000, 0.000000000000000000, 0.000000000000000000 ) ) ;
#16675 = CARTESIAN_POINT ( 'NONE',  ( 0.7495606340400177148, 0.1264236179284866091, 1.026082677111590513 ) ) ;
#16676 = CARTESIAN_POINT ( 'NONE',  ( 0.7495606340400177148, -0.1264236179284866091, 1.385334645615527549 ) ) ;
#16677 = CARTESIAN_POINT ( 'NONE',  ( 0.8759842519685039353, 0.1787899950787401882, 0.2288385826234019815 ) ) ;
#16678 = EDGE_CURVE ( 'NONE', #28106, #39448, #39846, .T. ) ;
#16679 = EDGE_CURVE ( 'NONE', #5551, #30540, #24257, .T. ) ;
#16680 = CARTESIAN_POINT ( 'NONE',  ( 0.7185039370078739607, 1.928577636452523993E-17, 0.2263779527559055260 ) ) ;
#16681 = CARTESIAN_POINT ( 'NONE',  ( 0.9873396505805591694, 0.1113553986120547346, 1.550196850393700920 ) ) ;
#16683 = CARTESIAN_POINT ( 'NONE',  ( -0.8702779046212122394, 0.1576667313500946244, 1.978454084305184990 ) ) ;
#16682 = CARTESIAN_POINT ( 'NONE',  ( 0.7878339515481005417, 0.1343209511212810070, 1.980178066860823760 ) ) ;
#16684 = CARTESIAN_POINT ( 'NONE',  ( 0.7646288533564489232, -0.1113553986120547346, 1.441929133750740277 ) ) ;
#16685 = LINE ( 'NONE', #37532, #16741 ) ;
#16686 = CARTESIAN_POINT ( 'NONE',  ( 1.033464566929134687, -0.06523048226347956391, 1.660925196850393526 ) ) ;
#16687 = CARTESIAN_POINT ( 'NONE',  ( 1.054774247047244540, 0.07405724077823318263, 0.9694881889226145688 ) ) ;
#16688 = CARTESIAN_POINT ( 'NONE',  ( 0.7495606340400177148, 0.1264236179284866091, 1.970964566875370139 ) ) ;
#16689 = CARTESIAN_POINT ( 'NONE',  ( -0.7495606340400177148, -0.1264236179284866091, 1.149114173174582643 ) ) ;
#16690 = CARTESIAN_POINT ( 'NONE',  ( 0.7185039370078746268, -0.06523048226347956391, 0.3371062991050715607 ) ) ;
#16691 = ORIENTED_EDGE ( 'NONE', *, *, #36095, .F. ) ;
#16692 = CARTESIAN_POINT ( 'NONE',  ( 0.9998624034419133499, 0.1095613300894844738, 0.03936950506162378849 ) ) ;
#16693 = CARTESIAN_POINT ( 'NONE',  ( 0.06523048226347956391, -1.698326771546016190, 0.1574803149606297803 ) ) ;
#16694 = CARTESIAN_POINT ( 'NONE',  ( -0.7646288533564489232, -0.1113553986120547346, 0.3001968502861740440 ) ) ;
#16695 = CARTESIAN_POINT ( 'NONE',  ( 1.002407869896990045, -0.1264236179284866091, 1.277066929080094448 ) ) ;
#16696 = PLANE ( 'NONE',  #40974 ) ;
#16697 = DIMENSIONAL_EXPONENTS ( 1.000000000000000000, 0.000000000000000000, 0.000000000000000000, 0.000000000000000000, 0.000000000000000000, 0.000000000000000000, 0.000000000000000000 ) ;
#16698 = CARTESIAN_POINT ( 'NONE',  ( -0.1264236179284866091, 0.07332677170730689253, -0.1264236179284866091 ) ) ;
#16699 = DIRECTION ( 'NONE',  ( 0.000000000000000000, -1.000000000000000000, 0.000000000000000000 ) ) ;
#16700 = CARTESIAN_POINT ( 'NONE',  ( 0.7646288533564489232, 0.1113553986120547346, 0.2608267716535432879 ) ) ;
#16701 = CARTESIAN_POINT ( 'NONE',  ( 0.5314960629921260393, 0.000000000000000000, 4.498031496062992574 ) ) ;
#16702 = CARTESIAN_POINT ( 'NONE',  ( -0.1787899950787401882, -1.698326771599779628, 0.000000000000000000 ) ) ;
#16703 = CARTESIAN_POINT ( 'NONE',  ( -0.9873396505805591694, 0.1113553986120547346, 0.05413385826771653642 ) ) ;
#16704 = ORIENTED_EDGE ( 'NONE', *, *, #39706, .F. ) ;
#16705 = CARTESIAN_POINT ( 'NONE',  ( -1.054774247047244096, 0.000000000000000000, 0.6963582676627716461 ) ) ;
#16706 = EDGE_LOOP ( 'NONE', ( #32041, #31812, #25869, #23374, #4745, #6319, #16869, #3085, #13810, #44738, #16287, #20065, #40168, #34887, #40260, #39914, #22819, #22118, #7803, #45440, #45032, #2186, #3949, #23769, #18762, #18815, #29500, #14292, #7067, #9672, #33945, #40936, #19522, #15412, #53, #43341, #1797, #34391, #16456, #32105, #13746, #33062, #42586, #17056, #34501, #2082, #23596, #32796, #31794, #28538, #44756, #22598, #8444, #36212, #25010, #23022, #9274, #39847, #23876, #29190, #24322, #9465, #17925, #12166, #952, #26092, #22035, #17519, #26130, #29234, #15401, #6774, #37636, #36608, #29049, #12614, #24888, #47460, #16987, #43441, #39537, #42776, #43125, #25257, #43861, #29432, #13349, #10355, #37155, #36029, #32592, #169, #26095, #12639, #34025, #29773, #1724, #13427, #24145, #35025, #28941, #3496 ) ) ;
#16707 = AXIS2_PLACEMENT_3D ( 'NONE', #33553, #670, #2108 ) ;
#16708 = CARTESIAN_POINT ( 'NONE',  ( 0.004457209083872700622, 0.04679503328990077676, -0.1377943176258828173 ) ) ;
#16709 = CARTESIAN_POINT ( 'NONE',  ( 0.07405724077823318263, -0.6585885351583735670, -0.1787899950787401604 ) ) ;
#16710 = ORIENTED_EDGE ( 'NONE', *, *, #15840, .T. ) ;
#16711 = CARTESIAN_POINT ( 'NONE',  ( 0.1920494157074515706, -0.08956033323250511824, 0.08002985433875355048 ) ) ;
#16712 = DIRECTION ( 'NONE',  ( 1.000000000000000000, 0.000000000000000000, 0.000000000000000000 ) ) ;
#16713 = VERTEX_POINT ( 'NONE', #32228 ) ;
#16714 = FACE_OUTER_BOUND ( 'NONE', #533, .T. ) ;
#16715 = FACE_OUTER_BOUND ( 'NONE', #43871, .T. ) ;
#16716 = AXIS2_PLACEMENT_3D ( 'NONE', #32349, #39029, #43088 ) ;
#16717 = CARTESIAN_POINT ( 'NONE',  ( -0.7495606340400177148, 0.1264236179284866091, 0.5487204723871811352 ) ) ;
#16718 = CARTESIAN_POINT ( 'NONE',  ( 0.7185039370078739607, 0.000000000000000000, 4.498031496062992574 ) ) ;
#16719 = VERTEX_POINT ( 'NONE', #24087 ) ;
#16720 = CARTESIAN_POINT ( 'NONE',  ( -0.7495606340400177148, -0.1264236179284866091, 1.705216535379307174 ) ) ;
#16721 = CARTESIAN_POINT ( 'NONE',  ( -1.094772975963752103E-17, -1.550688976324188895, -0.1787899950787401882 ) ) ;
#16722 = LINE ( 'NONE', #42564, #12688 ) ;
#16723 = EDGE_CURVE ( 'NONE', #15186, #2951, #19164, .T. ) ;
#16724 = DIRECTION ( 'NONE',  ( 1.000000000000000000, -0.000000000000000000, 0.000000000000000000 ) ) ;
#16725 = CARTESIAN_POINT ( 'NONE',  ( 3.301370929368692659E-17, -0.6998469591893444752, 0.1797182628040039365 ) ) ;
#16726 = DIRECTION ( 'NONE',  ( 0.000000000000000000, 0.000000000000000000, 1.000000000000000000 ) ) ;
#16727 = CARTESIAN_POINT ( 'NONE',  ( -0.7185039370078746268, 0.06523048226347956391, 1.198326771546015967 ) ) ;
#16728 = ADVANCED_FACE ( 'NONE', ( #13522 ), #39614, .T. ) ;
#16730 = CARTESIAN_POINT ( 'NONE',  ( -0.04902506021456321667, -0.09842519685039372024, 0.1521997253933253247 ) ) ;
#16729 = CARTESIAN_POINT ( 'NONE',  ( 0.1113553986120547346, -0.4458661417322834497, 0.1113553986120547346 ) ) ;
#16731 = DIRECTION ( 'NONE',  ( -1.267059173938974432E-30, -3.652049423109077687E-16, 1.000000000000000000 ) ) ;
#16732 = ORIENTED_EDGE ( 'NONE', *, *, #43208, .F. ) ;
#16733 = EDGE_CURVE ( 'NONE', #39408, #32565, #36796, .T. ) ;
#16734 = LINE ( 'NONE', #27794, #9333 ) ;
#16735 = CARTESIAN_POINT ( 'NONE',  ( 1.033464566929133799, 0.000000000000000000, 1.072834645669291431 ) ) ;
#16737 = CARTESIAN_POINT ( 'NONE',  ( -0.9498231833118063738, -0.1609423499385754242, 1.989542384547356324 ) ) ;
#16736 = CARTESIAN_POINT ( 'NONE',  ( 0.8759842519685039353, 0.000000000000000000, 4.498031496062992574 ) ) ;
#16738 = LINE ( 'NONE', #12695, #2885 ) ;
#16740 = DIRECTION ( 'NONE',  ( 1.000000000000000000, -3.469446951953626022E-15, -0.000000000000000000 ) ) ;
#16739 = CARTESIAN_POINT ( 'NONE',  ( 0.7646288533564489232, 0.1113553986120547346, 0.1820866141732283561 ) ) ;
#16741 = VECTOR ( 'NONE', #30388, 39.37007874015748143 ) ;
#16742 = CARTESIAN_POINT ( 'NONE',  ( 0.8107537697050254399, 0.1574803149606300301, 0.6028543306011346914 ) ) ;
#16743 = CARTESIAN_POINT ( 'NONE',  ( 0.07405724077823318263, -0.6181102361667089040, 0.1787899950787401604 ) ) ;
#16744 = ORIENTED_EDGE ( 'NONE', *, *, #20661, .T. ) ;
#16745 = CARTESIAN_POINT ( 'NONE',  ( 0.7646288533564489232, 0.1113553986120547346, 1.166338582677165281 ) ) ;
#16746 = CARTESIAN_POINT ( 'NONE',  ( 0.8019270111902717657, 0.1787899950787401604, 0.8218503936470251681 ) ) ;
#16747 = ORIENTED_EDGE ( 'NONE', *, *, #16315, .T. ) ;
#16748 = CARTESIAN_POINT ( 'NONE',  ( 0.9412147342319837628, -0.1574803149606297803, 1.459153543307085688 ) ) ;
#16749 = DIRECTION ( 'NONE',  ( 1.000000000000000000, 0.000000000000000000, 0.000000000000000000 ) ) ;
#16750 = CARTESIAN_POINT ( 'NONE',  ( 0.1787899950787401882, -1.791830708607653699, -2.189545951927503898E-17 ) ) ;
#16751 = CARTESIAN_POINT ( 'NONE',  ( -0.1264236179284866091, -1.033956692859621995, -0.1264236179284866091 ) ) ;
#16753 = AXIS2_PLACEMENT_3D ( 'NONE', #22710, #32818, #43803 ) ;
#16752 = CARTESIAN_POINT ( 'NONE',  ( 0.1574803149606300301, -1.422736220472442081, -0.06523048226347956391 ) ) ;
#16754 = CARTESIAN_POINT ( 'NONE',  ( 0.7646288533564489232, 0.1113553986120547346, 1.274606299105070839 ) ) ;
#16755 = CARTESIAN_POINT ( 'NONE',  ( 0.1645805237892203066, 0.08067386790044665801, -0.1414080254031222506 ) ) ;
#16756 = EDGE_LOOP ( 'NONE', ( #20238, #13861, #20365, #22271 ) ) ;
#16757 = CARTESIAN_POINT ( 'NONE',  ( -1.002407869896990045, 0.1264236179284866091, 1.882381889710015743 ) ) ;
#16758 = CARTESIAN_POINT ( 'NONE',  ( 0.8019270111902717657, -0.1787899950787401604, 1.865157480261195877 ) ) ;
#16759 = EDGE_LOOP ( 'NONE', ( #22536, #4186 ) ) ;
#16760 = DIRECTION ( 'NONE',  ( 1.822029033848725028E-16, 0.000000000000000000, 1.000000000000000000 ) ) ;
#16761 = CARTESIAN_POINT ( 'NONE',  ( -1.002407869896990045, -0.1264236179284866091, 1.552657480261196765 ) ) ;
#16762 = CARTESIAN_POINT ( 'NONE',  ( -0.4330708661417356775, 0.000000000000000000, 1.186023622047243986 ) ) ;
#16763 = CARTESIAN_POINT ( 'NONE',  ( -0.8759842519685039353, 0.1787899950787401882, 0.2337598424659216578 ) ) ;
#16764 = LINE ( 'NONE', #38571, #42841 ) ;
#16765 = CARTESIAN_POINT ( 'NONE',  ( -0.7495606340400177148, 0.1264236179284866091, 1.774114173174582643 ) ) ;
#16766 = CARTESIAN_POINT ( 'NONE',  ( -0.9412147342319837628, 0.1574803149606300301, 1.670767716535433545 ) ) ;
#16767 = CYLINDRICAL_SURFACE ( 'NONE', #23621, 0.1574803149606299191 ) ;
#16768 = CARTESIAN_POINT ( 'NONE',  ( -0.1264236179284866091, -0.2968759367331759713, -0.1264236179284866091 ) ) ;
#16769 = CARTESIAN_POINT ( 'NONE',  ( 0.6971942568897648851, -0.07405724077823297447, 1.742125984198204858 ) ) ;
#16770 = CARTESIAN_POINT ( 'NONE',  ( 0.1917573881879755804, -0.09842519685039370636, 0.09087608798953976386 ) ) ;
#16771 = CARTESIAN_POINT ( 'NONE',  ( -0.8759842519685039353, -0.1574803149606299191, 0.7381889762704251234 ) ) ;
#16772 = ( BOUNDED_CURVE ( )  B_SPLINE_CURVE ( 2, ( #12846, #27239, #5386, #20711, #20005, #27000, #42280, #9480, #1551 ),
 .UNSPECIFIED., .F., .T. ) 
 B_SPLINE_CURVE_WITH_KNOTS ( ( 3, 2, 2, 2, 3 ),
 ( 0.8599999999999999867, 0.8625000000000000444, 0.8649999999999999911, 0.8675000000000000488, 0.8699999999999999956 ),
 .UNSPECIFIED. ) 
 CURVE ( )  GEOMETRIC_REPRESENTATION_ITEM ( )  RATIONAL_B_SPLINE_CURVE ( ( 1.000000000000000000, 0.9238795325112869605, 1.000000000000000000, 0.9238795325112869605, 1.000000000000000000, 0.9238795325112869605, 1.000000000000000000, 0.9238795325112829637, 1.000000000000000000 ) ) 
 REPRESENTATION_ITEM ( '' )  ) ;
#16773 = AXIS2_PLACEMENT_3D ( 'NONE', #35777, #31487, #34852 ) ;
#16774 = ORIENTED_EDGE ( 'NONE', *, *, #12788, .F. ) ;
#16775 = CIRCLE ( 'NONE', #14383, 0.1864803149606299171 ) ;
#16776 = CARTESIAN_POINT ( 'NONE',  ( -0.8019270111902716547, 0.1787899950787401604, 1.299212598371434435 ) ) ;
#16777 = ORIENTED_EDGE ( 'NONE', *, *, #37506, .T. ) ;
#16778 = B_SPLINE_CURVE_WITH_KNOTS ( 'NONE', 3,
 ( #22494, #37114, #30437, #40918, #11488, #36888, #45228, #40454, #37836, #18895, #33794, #44757, #15808, #7639, #44522, #4994, #666, #15321, #1152 ),
 .UNSPECIFIED., .F., .F.,
 ( 4, 2, 1, 1, 2, 2, 2, 1, 2, 2, 4 ),
 ( 0.000000000000000000, 0.1250000000000000278, 0.1875000000000001110, 0.2187500000000001388, 0.2343750000000006661, 0.2500000000000011657, 0.3750000000000031086, 0.4375000000000041078, 0.4687500000000042744, 0.5000000000000044409, 1.000000000000000000 ),
 .UNSPECIFIED. ) ;
#16779 = CARTESIAN_POINT ( 'NONE',  ( -0.1787899950787401604, -1.257874015694269376, 0.07405724077823318263 ) ) ;
#16780 = ADVANCED_FACE ( 'NONE', ( #17349 ), #36039, .F. ) ;
#16781 = CARTESIAN_POINT ( 'NONE',  ( -1.033464566929133799, 0.000000000000000000, 1.377952755797984263 ) ) ;
#16782 = CARTESIAN_POINT ( 'NONE',  ( 0.8019270111902717657, 0.1787899950787401604, 0.3887795275052913224 ) ) ;
#16783 = CARTESIAN_POINT ( 'NONE',  ( -0.1797182628040039087, -0.4365595576145414047, -0.07444174185955065859 ) ) ;
#16784 = CARTESIAN_POINT ( 'NONE',  ( -0.7185039370078739607, 1.928577636452523993E-17, 0.8464566928058583350 ) ) ;
#16785 = CARTESIAN_POINT ( 'NONE',  ( -0.7646288533564489232, 0.1113553986120547346, 0.6938976377952755792 ) ) ;
#16786 = CARTESIAN_POINT ( 'NONE',  ( 0.1574803149606300301, -0.005413385826771673418, -0.06523048226347956391 ) ) ;
#16787 = ADVANCED_FACE ( 'NONE', ( #47050 ), #46572, .T. ) ;
#16788 = CARTESIAN_POINT ( 'NONE',  ( 0.6971942568897648851, -0.07405724077823297447, 0.9891732282926934960 ) ) ;
#16789 = CARTESIAN_POINT ( 'NONE',  ( 1.002407869896990045, -0.1264236179284866091, 1.990649606245448844 ) ) ;
#16790 = CARTESIAN_POINT ( 'NONE',  ( -0.8075642815980649258, 0.1651804164989427171, 0.03937007874015843040 ) ) ;
#16791 = CARTESIAN_POINT ( 'NONE',  ( 3.284318927891251994E-17, -0.6254921259304881964, 0.1787899950787401882 ) ) ;
#16792 = CARTESIAN_POINT ( 'NONE',  ( -0.1787899950787401604, -1.459645669237573884, -0.07405724077823318263 ) ) ;
#16793 = CARTESIAN_POINT ( 'NONE',  ( 1.054774247047244540, -0.07405724077823318263, 0.3395669290800945039 ) ) ;
#16794 = AXIS2_PLACEMENT_3D ( 'NONE', #4563, #19673, #33857 ) ;
#16795 = CARTESIAN_POINT ( 'NONE',  ( -1.054774247047244540, -0.07405724077823318263, 1.948818897584033927 ) ) ;
#16796 = VERTEX_POINT ( 'NONE', #31520 ) ;
#16797 = EDGE_LOOP ( 'NONE', ( #5315, #546, #6445, #25308 ) ) ;
#16798 = CARTESIAN_POINT ( 'NONE',  ( 0.6971942568897648851, -0.07405724077823297447, 1.387795275536786610 ) ) ;
#16799 = CARTESIAN_POINT ( 'NONE',  ( -0.7185039370078739607, 0.000000000000000000, -2.869337061179095023E-17 ) ) ;
#16800 = CARTESIAN_POINT ( 'NONE',  ( -0.6971942568897626646, 0.07405724077823318263, 0.6348425196312760255 ) ) ;
#16801 = CARTESIAN_POINT ( 'NONE',  ( 0.8019270111902717657, 0.1787899950787401604, 0.1181102361667090567 ) ) ;
#16802 = CARTESIAN_POINT ( 'NONE',  ( 0.1349619066862741967, -0.09842519684088384124, -0.1172652914709395727 ) ) ;
#16803 = CARTESIAN_POINT ( 'NONE',  ( 0.8019270111902716547, 0.1787899950787401604, 0.5511811023084406402 ) ) ;
#16804 = CARTESIAN_POINT ( 'NONE',  ( -1.054774247047244096, 0.000000000000000000, 0.5733267715997795166 ) ) ;
#16805 = EDGE_CURVE ( 'NONE', #10984, #1283, #36816, .T. ) ;
#16806 = CYLINDRICAL_SURFACE ( 'NONE', #20009, 0.1574803149606299191 ) ;
#16807 = ORIENTED_EDGE ( 'NONE', *, *, #30075, .T. ) ;
#16808 = VERTEX_POINT ( 'NONE', #12345 ) ;
#16809 = CARTESIAN_POINT ( 'NONE',  ( -1.033464566929134687, -0.06523048226347956391, 0.2829724409448821643 ) ) ;
#16810 = CIRCLE ( 'NONE', #10720, 0.1574803149606299191 ) ;
#16811 = CARTESIAN_POINT ( 'NONE',  ( 0.7495606340400177148, 0.1264236179284866091, 1.380413385773007873 ) ) ;
#16812 = CARTESIAN_POINT ( 'NONE',  ( 0.1917907757321275775, -0.09851384566401279186, 0.09088981981130157817 ) ) ;
#16813 = CARTESIAN_POINT ( 'NONE',  ( 0.3849708276051176936, 4.766607801171850497E-17, 0.000000000000000000 ) ) ;
#16814 = VERTEX_POINT ( 'NONE', #15466 ) ;
#16815 = CARTESIAN_POINT ( 'NONE',  ( -0.8019270111902717657, 0.1787899950787401604, 0.9448818897100165204 ) ) ;
#16816 = CARTESIAN_POINT ( 'NONE',  ( -0.1264236179284866091, -1.625616094213490292, 0.1264236179284866091 ) ) ;
#16817 = ORIENTED_EDGE ( 'NONE', *, *, #20169, .T. ) ;
#16818 = CARTESIAN_POINT ( 'NONE',  ( -1.033464566929133799, 0.000000000000000000, 1.929133858160188897 ) ) ;
#16819 = CARTESIAN_POINT ( 'NONE',  ( -0.1787899950787401882, -0.5910433070328504623, 0.000000000000000000 ) ) ;
#16820 = CARTESIAN_POINT ( 'NONE',  ( 1.002407869896990045, 0.1264236179284866091, 1.444389763725763665 ) ) ;
#16821 = ADVANCED_FACE ( 'NONE', ( #11632 ), #30566, .T. ) ;
#16822 = DIRECTION ( 'NONE',  ( 0.000000000000000000, -1.000000000000000000, 0.000000000000000000 ) ) ;
#16823 = CARTESIAN_POINT ( 'NONE',  ( -0.1264236179284866091, -0.7042322834108031282, 0.1264236179284866091 ) ) ;
#16824 = EDGE_CURVE ( 'NONE', #2521, #6124, #32841, .T. ) ;
#16825 = AXIS2_PLACEMENT_3D ( 'NONE', #45905, #42065, #16699 ) ;
#16826 = CARTESIAN_POINT ( 'NONE',  ( 0.7185039370078746268, -0.06523048226347956391, 0.1796259841444415029 ) ) ;
#16827 = LINE ( 'NONE', #41081, #40758 ) ;
#16828 = CARTESIAN_POINT ( 'NONE',  ( 0.07405724077823318263, 0.05007288216446208196, -0.1787899950787401604 ) ) ;
#16829 = CARTESIAN_POINT ( 'NONE',  ( 0.1787899950787401882, 0.05364173233722811102, -2.189545951927503898E-17 ) ) ;
#16830 = APPLICATION_PROTOCOL_DEFINITION ( 'draft international standard', 'automotive_design', 1998, #41312 ) ;
#16831 = DIRECTION ( 'NONE',  ( 1.000000000000000000, 0.000000000000000000, -1.822029033848725275E-16 ) ) ;
#16832 = EDGE_CURVE ( 'NONE', #19538, #45189, #15941, .T. ) ;
#16833 = VECTOR ( 'NONE', #8141, 39.37007874015748143 ) ;
#16834 = CARTESIAN_POINT ( 'NONE',  ( -1.002407869896990045, -0.1264236179284866091, 0.8095472440407244230 ) ) ;
#16836 = CARTESIAN_POINT ( 'NONE',  ( -1.033464566929133799, 0.000000000000000000, 1.377952755797984263 ) ) ;
#16835 = CARTESIAN_POINT ( 'NONE',  ( 0.1574803149606299191, -0.9527559055118109965, -1.928577636452523993E-17 ) ) ;
#16837 = CARTESIAN_POINT ( 'NONE',  ( -0.1797182628040039365, -1.536461132417690667, 0.000000000000000000 ) ) ;
#16838 = CARTESIAN_POINT ( 'NONE',  ( -9.642888182262618425E-18, -0.06692913375074074911, -0.1574803149606299191 ) ) ;
#16839 = CARTESIAN_POINT ( 'NONE',  ( 0.6971942568897637749, 2.189545951927499583E-17, 1.542814960576157413 ) ) ;
#16841 = CARTESIAN_POINT ( 'NONE',  ( 0.2559055118110236116, 0.1222388761248534295, -0.2994676661288905861 ) ) ;
#16840 = CARTESIAN_POINT ( 'NONE',  ( 1.002407869896990045, 0.1264236179284866091, 1.956200787347811110 ) ) ;
#16842 = CARTESIAN_POINT ( 'NONE',  ( 0.8759842519685039353, -0.1787899950787401882, 0.4060039369541102450 ) ) ;
#16843 = VERTEX_POINT ( 'NONE', #45128 ) ;
#16844 = DIRECTION ( 'NONE',  ( 0.000000000000000000, 0.000000000000000000, 1.000000000000000000 ) ) ;
#16845 = CARTESIAN_POINT ( 'NONE',  ( -0.7108038343253642033, 0.06841996760810098444, 0.03937007874015843040 ) ) ;
#16846 = FACE_OUTER_BOUND ( 'NONE', #10358, .T. ) ;
#16847 = CARTESIAN_POINT ( 'NONE',  ( -0.07405724077823318263, 0.1053149606836847191, -0.1787899950787401604 ) ) ;
#16848 = CARTESIAN_POINT ( 'NONE',  ( -0.7185039370078739607, 1.928577636452523993E-17, 1.240157480207432883 ) ) ;
#16849 = CARTESIAN_POINT ( 'NONE',  ( 0.1264236179284866091, -0.05462598419820496182, -0.1264236179284866091 ) ) ;
#16850 = CARTESIAN_POINT ( 'NONE',  ( 1.054774247047244540, 0.07405724077823318263, 0.4576771653005669016 ) ) ;
#16851 = CARTESIAN_POINT ( 'NONE',  ( -0.1787899950787401604, -0.9084645668753701386, -0.07405724077823318263 ) ) ;
#16852 = CARTESIAN_POINT ( 'NONE',  ( 0.7821658433489714346, -0.1347180231840020004, 0.03936951888585819848 ) ) ;
#16853 = FACE_OUTER_BOUND ( 'NONE', #7979, .T. ) ;
#16854 = CARTESIAN_POINT ( 'NONE',  ( -0.8759842519685039353, 0.1787899950787401882, 1.409940944828126153 ) ) ;
#16855 = EDGE_LOOP ( 'NONE', ( #22122, #18904, #35570, #41652 ) ) ;
#16856 = CARTESIAN_POINT ( 'NONE',  ( 1.002407869896990045, -0.1264236179284866091, 1.085137795221826629 ) ) ;
#16859 = VERTEX_POINT ( 'NONE', #8249 ) ;
#16858 = CARTESIAN_POINT ( 'NONE',  ( -0.07405724077823318263, -1.336614173174582865, 0.1787899950787401604 ) ) ;
#16857 = CARTESIAN_POINT ( 'NONE',  ( -0.06523048226347956391, -1.073326771546015301, 0.1574803149606297803 ) ) ;
#16860 = CARTESIAN_POINT ( 'NONE',  ( 1.002407869896990045, -0.1264236179284866091, 1.710137795221826851 ) ) ;
#16861 = CARTESIAN_POINT ( 'NONE',  ( -0.9873396505805591694, 0.1113553986120547346, 1.353346456692913424 ) ) ;
#16862 = CYLINDRICAL_SURFACE ( 'NONE', #24343, 0.1574803149606299191 ) ;
#16864 = CARTESIAN_POINT ( 'NONE',  ( -0.7018081390872378256, -0.006340216279131547818, 0.03937007874015843734 ) ) ;
#16863 = DIRECTION ( 'NONE',  ( -5.464378949326941559E-15, -1.000000000000000000, 0.000000000000000000 ) ) ;
#16865 = CARTESIAN_POINT ( 'NONE',  ( 0.8019270111902716547, 0.1787899950787401604, 0.1968503936470238636 ) ) ;
#16866 = UNCERTAINTY_MEASURE_WITH_UNIT (LENGTH_MEASURE( 1.000000000000000082E-05 ), #6683, 'distance_accuracy_value', 'NONE') ;
#16867 = CARTESIAN_POINT ( 'NONE',  ( 0.7646288533564489232, -0.1113553986120547346, 1.441929133750740277 ) ) ;
#16868 = ORIENTED_EDGE ( 'NONE', *, *, #37161, .T. ) ;
#16869 = ORIENTED_EDGE ( 'NONE', *, *, #9610, .F. ) ;
#16870 = AXIS2_PLACEMENT_3D ( 'NONE', #13709, #33314, #37108 ) ;
#16871 = DIRECTION ( 'NONE',  ( 0.000000000000000000, -1.000000000000000000, -0.000000000000000000 ) ) ;
#16872 = ORIENTED_EDGE ( 'NONE', *, *, #39267, .F. ) ;
#16873 = CARTESIAN_POINT ( 'NONE',  ( -0.7495606340400177148, 0.1264236179284866091, 1.769192913332062966 ) ) ;
#16874 = EDGE_LOOP ( 'NONE', ( #32104, #34969, #17418, #27305, #15254, #35581, #20165, #17161, #47367, #17665, #25576, #25312, #34183, #26948, #20213, #19024, #28161, #34635, #1014, #17616, #11557, #23909, #6763, #10036, #11937, #19811, #11780, #37742, #14107, #25508, #46164, #19939, #41688, #46405, #34474, #21843, #38216, #18533, #45127, #22241, #40368, #20783, #33350, #6230, #24832, #28216, #8263, #32628, #38509, #22343, #7914, #44916, #8309, #9163, #44971, #4452, #16227, #29071, #19496, #16660, #8100, #6288, #11532, #22272, #17385, #59, #17246, #40377, #23302, #6364, #3481, #14469, #23140, #46183, #9152, #36467, #3601, #30516, #34394, #4515, #14712, #8234, #30211, #42493, #28651, #22389, #2553, #20762, #23359, #45254, #14030, #2916, #34260, #9562, #10485, #39993, #2296, #33646, #17563, #34402, #18473, #17886 ) ) ;
#16875 = AXIS2_PLACEMENT_3D ( 'NONE', #43061, #10265, #26312 ) ;
#16876 = AXIS2_PLACEMENT_3D ( 'NONE', #39376, #2255, #31982 ) ;
#16877 = ( BOUNDED_CURVE ( )  B_SPLINE_CURVE ( 2, ( #46262, #20628, #35274, #2410, #23684, #20079, #12687, #30903, #12447 ),
 .UNSPECIFIED., .F., .F. ) 
 B_SPLINE_CURVE_WITH_KNOTS ( ( 3, 2, 2, 2, 3 ),
 ( 0.8000000000000000444, 0.8024999999999999911, 0.8050000000000000488, 0.8074999999999999956, 0.8100000000000000533 ),
 .UNSPECIFIED. ) 
 CURVE ( )  GEOMETRIC_REPRESENTATION_ITEM ( )  RATIONAL_B_SPLINE_CURVE ( ( 1.000000000000000000, 0.9238795325112869605, 1.000000000000000000, 0.9238795325112869605, 1.000000000000000000, 0.9238795325112869605, 1.000000000000000000, 0.9238795325112829637, 1.000000000000000000 ) ) 
 REPRESENTATION_ITEM ( '' )  ) ;
#16878 = CARTESIAN_POINT ( 'NONE',  ( -0.2471922904502826812, 0.07845432542752767135, -0.07637674237069251582 ) ) ;
#16879 = CARTESIAN_POINT ( 'NONE',  ( 0.1574803149606299191, 3.616083068348484413E-17, -0.2952755905511810774 ) ) ;
#16880 = CARTESIAN_POINT ( 'NONE',  ( 0.7185039370078739607, 1.928577636452523993E-17, 1.633858267609007875 ) ) ;
#16881 = CARTESIAN_POINT ( 'NONE',  ( 0.1787899950787401604, -1.180242078465460143, 0.07405724077823318263 ) ) ;
#16882 = ORIENTED_EDGE ( 'NONE', *, *, #25095, .F. ) ;
#16883 = CARTESIAN_POINT ( 'NONE',  ( -0.1264236179284866091, -0.1235236219934805202, -0.1264236179284866091 ) ) ;
#16884 = ORIENTED_EDGE ( 'NONE', *, *, #15612, .F. ) ;
#16885 = EDGE_CURVE ( 'NONE', #39837, #29015, #6148, .T. ) ;
#16886 = ORIENTED_EDGE ( 'NONE', *, *, #27034, .T. ) ;
#16887 = CARTESIAN_POINT ( 'NONE',  ( 0.6971942568897648851, -0.07405724077823297447, 1.107283464513165949 ) ) ;
#16888 = CARTESIAN_POINT ( 'NONE',  ( 0.8070866141732283561, -0.0009842519685049383633, -0.7574803149606299524 ) ) ;
#16889 = EDGE_CURVE ( 'NONE', #42069, #12184, #27003, .T. ) ;
#16890 = CARTESIAN_POINT ( 'NONE',  ( 1.033464566929134687, 0.06523048226347956391, 1.902066929133858775 ) ) ;
#16891 = CARTESIAN_POINT ( 'NONE',  ( 0.07405724077823318263, -0.5688976377415115859, -0.1787899950787401604 ) ) ;
#16892 = ORIENTED_EDGE ( 'NONE', *, *, #32223, .F. ) ;
#16893 = ( BOUNDED_CURVE ( )  B_SPLINE_CURVE ( 2, ( #7178, #43826, #43107, #14852, #32118, #10555, #6456, #11260, #33080 ),
 .UNSPECIFIED., .F., .T. ) 
 B_SPLINE_CURVE_WITH_KNOTS ( ( 3, 2, 2, 2, 3 ),
 ( 0.6999999999999999556, 0.7025000000000000133, 0.7049999999999999600, 0.7075000000000000178, 0.7099999999999999645 ),
 .UNSPECIFIED. ) 
 CURVE ( )  GEOMETRIC_REPRESENTATION_ITEM ( )  RATIONAL_B_SPLINE_CURVE ( ( 1.000000000000000000, 0.9238795325112899581, 1.000000000000000000, 0.9238795325112869605, 1.000000000000000000, 0.9238795325112869605, 1.000000000000000000, 0.9238795325112799661, 1.000000000000000000 ) ) 
 REPRESENTATION_ITEM ( '' )  ) ;
#16894 = VECTOR ( 'NONE', #30390, 39.37007874015748854 ) ;
#16895 = CARTESIAN_POINT ( 'NONE',  ( -0.8019270111902716547, 0.1787899950787401604, 0.3149606298674962890 ) ) ;
#16896 = CARTESIAN_POINT ( 'NONE',  ( -1.033464566929134687, 0.06523048226347956391, 1.035925196850394192 ) ) ;
#16897 = PRODUCT_RELATED_PRODUCT_CATEGORY ( 'part', '', ( #24326 ) ) ;
#16898 = CARTESIAN_POINT ( 'NONE',  ( 0.8759842519685039353, 0.000000000000000000, 4.498031496062992574 ) ) ;
#16900 = CARTESIAN_POINT ( 'NONE',  ( -0.7118405396259548379, 0.02030376831657693462, 1.982893094199861483 ) ) ;
#16899 = CARTESIAN_POINT ( 'NONE',  ( 0.1270800023317771588, -1.196894203283832780, -0.1270800023317771588 ) ) ;
#16901 = CARTESIAN_POINT ( 'NONE',  ( -0.1677835123531180861, 0.1986243762397535695, -0.03618545512905874811 ) ) ;
#16902 = CARTESIAN_POINT ( 'NONE',  ( 0.9500414927467378812, -0.1787899950787401604, 1.003937007820251193 ) ) ;
#16903 = CARTESIAN_POINT ( 'NONE',  ( 0.9500414927467377701, -0.1787899950787401604, 1.510826771599780294 ) ) ;
#16904 = CARTESIAN_POINT ( 'NONE',  ( 0.6971942568897637749, 2.189545951927499583E-17, 0.1993110235682838682 ) ) ;
#16905 = CIRCLE ( 'NONE', #43683, 0.09842519685039370636 ) ;
#16906 = CARTESIAN_POINT ( 'NONE',  ( 0.2395294000716133853, 0.1968503937007874127, 0.4921259842519685179 ) ) ;
#16907 = CARTESIAN_POINT ( 'NONE',  ( 1.033464566929133799, 0.000000000000000000, 1.663385826771653697 ) ) ;
#16909 = CARTESIAN_POINT ( 'NONE',  ( 0.9412147342319837628, -0.1574803149606297803, 1.528051180994836056 ) ) ;
#16908 = DIRECTION ( 'NONE',  ( 0.000000000000000000, 0.000000000000000000, -1.000000000000000000 ) ) ;
#16910 = VECTOR ( 'NONE', #442, 39.37007874015748854 ) ;
#16911 = CARTESIAN_POINT ( 'NONE',  ( 0.7185039370078739607, 1.928577636452523993E-17, 0.7677165353255432922 ) ) ;
#16912 = CARTESIAN_POINT ( 'NONE',  ( -0.7646288533564489232, -0.1113553986120547346, 0.6938976376877481478 ) ) ;
#16914 = CARTESIAN_POINT ( 'NONE',  ( 0.1574803149606299191, 1.928577636452524610E-17, -0.1574803149606298636 ) ) ;
#16913 = CARTESIAN_POINT ( 'NONE',  ( 0.6971942568897637749, 2.189545951927499583E-17, 1.026082677111590513 ) ) ;
#16915 = CARTESIAN_POINT ( 'NONE',  ( 1.054774247047244540, -0.07405724077823318263, 1.914370078686394860 ) ) ;
#16916 = CARTESIAN_POINT ( 'NONE',  ( 1.033464566929134687, -0.06523048226347956391, 0.3124999998924728462 ) ) ;
#16917 = ORIENTED_EDGE ( 'NONE', *, *, #11475, .T. ) ;
#16918 = DIRECTION ( 'NONE',  ( 1.822029033848725028E-16, 0.000000000000000000, 1.000000000000000000 ) ) ;
#16919 = CARTESIAN_POINT ( 'NONE',  ( -0.8759842519685039353, 0.1574803149606299191, 0.2854330707586145710 ) ) ;
#16920 = CARTESIAN_POINT ( 'NONE',  ( 1.054774247047244096, 0.000000000000000000, 1.360728346402929168 ) ) ;
#16922 = CARTESIAN_POINT ( 'NONE',  ( 0.7646288533564489232, -0.1113553986120547346, 0.06397637784522892945 ) ) ;
#16921 = CARTESIAN_POINT ( 'NONE',  ( -0.5314960629921260393, 0.000000000000000000, 4.842519685039370358 ) ) ;
#16923 = CARTESIAN_POINT ( 'NONE',  ( 0.1787899950787401882, 0.1373031496600628232, -2.189545951927503898E-17 ) ) ;
#16924 = CARTESIAN_POINT ( 'NONE',  ( -0.1377952755905511584, 0.1564960629921283985, -0.9074803149606294195 ) ) ;
#16925 = EDGE_LOOP ( 'NONE', ( #44590, #6018, #10333, #36513 ) ) ;
#16926 = CARTESIAN_POINT ( 'NONE',  ( 0.9873396505805591694, -0.1113553986120547346, 1.294291338475149544 ) ) ;
#16927 = CARTESIAN_POINT ( 'NONE',  ( -0.7185039370078739607, 1.928577636452523993E-17, 0.1082677165354330728 ) ) ;
#16928 = EDGE_LOOP ( 'NONE', ( #19914, #43553, #46441, #31283 ) ) ;
#16929 = CARTESIAN_POINT ( 'NONE',  ( -0.8019270111902716547, 0.1787899950787401604, 1.412401574749386990 ) ) ;
#16931 = CARTESIAN_POINT ( 'NONE',  ( -0.1264236179284866091, -1.693405511757259951, 0.1264236179284866091 ) ) ;
#16930 = CARTESIAN_POINT ( 'NONE',  ( -0.1113553986120547346, -0.4064960628845984414, 0.1113553986120547346 ) ) ;
#16932 = CARTESIAN_POINT ( 'NONE',  ( -1.002407869896990045, 0.1264236179284866091, 1.016240157426551161 ) ) ;
#16933 = CARTESIAN_POINT ( 'NONE',  ( -0.6971942568897637749, 2.189545951927499583E-17, 1.931594488135212728 ) ) ;
#16934 = EDGE_LOOP ( 'NONE', ( #2866, #26929, #20964, #11120 ) ) ;
#16935 = EDGE_CURVE ( 'NONE', #36616, #3517, #25456, .T. ) ;
#16936 = CARTESIAN_POINT ( 'NONE',  ( -0.7495606340400177148, 0.1264236179284866091, 0.7111220471903307860 ) ) ;
#16937 = VECTOR ( 'NONE', #5465, 39.37007874015748143 ) ;
#16938 = CARTESIAN_POINT ( 'NONE',  ( 0.1561172342761355525, 0.1239648558221263380, -0.04236179190153568225 ) ) ;
#16939 = DIRECTION ( 'NONE',  ( 8.659560562354332584E-17, 0.7071067811865965336, -0.7071067811864983899 ) ) ;
#16940 = CARTESIAN_POINT ( 'NONE',  ( 0.1264236179284866091, -0.6708916847646714254, 0.1264236179284866091 ) ) ;
#16941 = VERTEX_POINT ( 'NONE', #1049 ) ;
#16942 = CARTESIAN_POINT ( 'NONE',  ( 0.1614456555785303005, -0.08956047347222421962, -0.1130746612548063079 ) ) ;
#16943 = CARTESIAN_POINT ( 'NONE',  ( -0.9412147342319837628, -0.1574803149606297803, 0.6619094487113718062 ) ) ;
#16944 = EDGE_CURVE ( 'NONE', #4710, #31350, #37968, .T. ) ;
#16945 = ORIENTED_EDGE ( 'NONE', *, *, #29891, .F. ) ;
#16946 = AXIS2_PLACEMENT_3D ( 'NONE', #20301, #31588, #23914 ) ;
#16947 = VECTOR ( 'NONE', #18686, 39.37007874015748143 ) ;
#16949 = CARTESIAN_POINT ( 'NONE',  ( -0.1476377952755905387, 0.07021257666615011994, -0.1553045758542774268 ) ) ;
#16948 = AXIS2_PLACEMENT_3D ( 'NONE', #31307, #30847, #2044 ) ;
#16950 = CARTESIAN_POINT ( 'NONE',  ( -1.002407869896990045, -0.1264236179284866091, 0.5684055117572598403 ) ) ;
#16951 = CARTESIAN_POINT ( 'NONE',  ( 0.000000000000000000, 0.000000000000000000, -0.4921259842519685179 ) ) ;
#16952 = EDGE_LOOP ( 'NONE', ( #7636, #24781, #7887, #15369 ) ) ;
#16953 = CARTESIAN_POINT ( 'NONE',  ( -1.054774247047244540, -0.07405724077823318263, 1.638779527505292766 ) ) ;
#16954 = CARTESIAN_POINT ( 'NONE',  ( -0.2559055241377596879, 0.07349206531156367295, -0.3089908134149170760 ) ) ;
#16955 = FACE_OUTER_BOUND ( 'NONE', #6600, .T. ) ;
#16956 = CARTESIAN_POINT ( 'NONE',  ( 0.8759842519685039353, -0.1574803149606299191, 0.5905511811023621549 ) ) ;
#16957 = CARTESIAN_POINT ( 'NONE',  ( 1.033464566929133799, 0.000000000000000000, 0.6299212597349921339 ) ) ;
#16958 = CARTESIAN_POINT ( 'NONE',  ( -1.033464566929133799, 0.000000000000000000, 1.181102362097196989 ) ) ;
#16960 = DIRECTION ( 'NONE',  ( -1.000000000000000000, 3.469446951953614189E-15, 0.000000000000000000 ) ) ;
#16959 = CARTESIAN_POINT ( 'NONE',  ( 2.892866454678787531E-17, -0.4901574803149605919, 0.1574803149606299191 ) ) ;
#16961 = LINE ( 'NONE', #1866, #42191 ) ;
#16962 = ORIENTED_EDGE ( 'NONE', *, *, #23720, .F. ) ;
#16963 = CARTESIAN_POINT ( 'NONE',  ( 1.033464566929134687, 0.06523048226347956391, 1.577263779420032153 ) ) ;
#16964 = CARTESIAN_POINT ( 'NONE',  ( 1.033464566929134687, 0.06523048226347956391, 1.154035433070866423 ) ) ;
#16965 = CARTESIAN_POINT ( 'NONE',  ( 0.1574803149606299191, 0.08070866152484981737, -1.928577636452523993E-17 ) ) ;
#16967 = CARTESIAN_POINT ( 'NONE',  ( 0.4509871776442260227, -3.032960542342102697E-32, 0.09842519685039370636 ) ) ;
#16966 = CARTESIAN_POINT ( 'NONE',  ( 1.033464566929133799, 0.000000000000000000, 0.3248031496062992463 ) ) ;
#16968 = DIRECTION ( 'NONE',  ( 0.000000000000000000, 0.000000000000000000, 1.000000000000000000 ) ) ;
#16969 = CARTESIAN_POINT ( 'NONE',  ( 0.06523048226347956391, -0.5959645668216069225, 0.1574803149606297803 ) ) ;
#16970 = VECTOR ( 'NONE', #5052, 39.37007874015748143 ) ;
#16972 = CARTESIAN_POINT ( 'NONE',  ( 0.1574803149606300023, 2.123129472280982366, -1.759219038810944324 ) ) ;
#16971 = DIRECTION ( 'NONE',  ( 0.000000000000000000, 0.000000000000000000, -1.000000000000000000 ) ) ;
#16973 = CARTESIAN_POINT ( 'NONE',  ( 0.2383973256948878072, 0.3740157480314960647, 1.112073044918586717 ) ) ;
#16974 = CARTESIAN_POINT ( 'NONE',  ( 0.07405724077823318263, -0.4999999999462365619, 0.1787899950787401604 ) ) ;
#16975 = ORIENTED_EDGE ( 'NONE', *, *, #8633, .T. ) ;
#16976 = VECTOR ( 'NONE', #24266, 39.37007874015748854 ) ;
#16978 = DIRECTION ( 'NONE',  ( 0.000000000000000000, 0.6156614753256639538, 0.7880107536067174623 ) ) ;
#16977 = AXIS2_PLACEMENT_3D ( 'NONE', #38672, #15933, #30800 ) ;
#16979 = CARTESIAN_POINT ( 'NONE',  ( 0.8759842519685039353, -0.1787899950787401882, 0.8784448818360000022 ) ) ;
#16980 = CARTESIAN_POINT ( 'NONE',  ( -0.4338976377952755703, -2.656856766417909227E-17, 0.000000000000000000 ) ) ;
#16981 = DIRECTION ( 'NONE',  ( 1.000000000000000000, 0.000000000000000000, -1.822029033848725275E-16 ) ) ;
#16982 = CARTESIAN_POINT ( 'NONE',  ( -0.07444174185955065859, 0.1244640644327026091, 0.1797182628040039087 ) ) ;
#16983 = CARTESIAN_POINT ( 'NONE',  ( -0.1787899950787401604, -1.065944881836000224, 0.07405724077823318263 ) ) ;
#16984 = CARTESIAN_POINT ( 'NONE',  ( 0.1574803149606300301, -1.343996062992125706, -0.06523048226347956391 ) ) ;
#16985 = CARTESIAN_POINT ( 'NONE',  ( 0.8107537697050253289, 0.1574803149606300301, 1.272145669183810668 ) ) ;
#16986 = CARTESIAN_POINT ( 'NONE',  ( -0.9412147342319837628, 0.1574803149606300301, 1.395177165354331672 ) ) ;
#16987 = ORIENTED_EDGE ( 'NONE', *, *, #18710, .F. ) ;
#16988 = CARTESIAN_POINT ( 'NONE',  ( -1.002407869896990045, -0.1264236179284866091, 1.990649606245448844 ) ) ;
#16989 = CARTESIAN_POINT ( 'NONE',  ( 0.7185039370078739607, 0.000000000000000000, 4.498031496062992574 ) ) ;
#16990 = ORIENTED_EDGE ( 'NONE', *, *, #24562, .F. ) ;
#16991 = CARTESIAN_POINT ( 'NONE',  ( 0.9412147342319837628, -0.1574803149606297803, 0.5536417322834641386 ) ) ;
#16992 = CARTESIAN_POINT ( 'NONE',  ( -0.6971942568897648851, -0.07405724077823297447, 1.540354330654897685 ) ) ;
#16993 = DIRECTION ( 'NONE',  ( 0.000000000000000000, -0.7880107536067201268, 0.6156614753256606232 ) ) ;
#16994 = EDGE_CURVE ( 'NONE', #17869, #26907, #32986, .T. ) ;
#16995 = CARTESIAN_POINT ( 'NONE',  ( -1.054774247047244540, -0.07405724077823318263, 0.9645669290800953366 ) ) ;
#16996 = CARTESIAN_POINT ( 'NONE',  ( -0.6971942568897626646, -0.07405724077823297447, 0.1673228345919059168 ) ) ;
#16997 = EDGE_CURVE ( 'NONE', #18349, #20105, #30377, .T. ) ;
#16998 = DIRECTION ( 'NONE',  ( 0.000000000000000000, 0.000000000000000000, -1.000000000000000000 ) ) ;
#16999 = CARTESIAN_POINT ( 'NONE',  ( -1.002407869896990045, -0.1264236179284866091, 1.833169291284818758 ) ) ;
#17000 = CARTESIAN_POINT ( 'NONE',  ( 1.033464566929133799, 1.928577636452524610E-17, 4.498031496062992574 ) ) ;
#17001 = DIRECTION ( 'NONE',  ( 0.000000000000000000, 0.000000000000000000, -1.000000000000000000 ) ) ;
#17002 = CARTESIAN_POINT ( 'NONE',  ( -1.033464566929133799, 0.000000000000000000, 1.702755905511810885 ) ) ;
#17003 = CARTESIAN_POINT ( 'NONE',  ( 0.2559055118110236116, -4.594920972184172978E-16, -0.02740704184215071032 ) ) ;
#17004 = CARTESIAN_POINT ( 'NONE',  ( 0.1264236179284866091, -0.2279782989379003921, -0.1264236179284866091 ) ) ;
#17005 = CARTESIAN_POINT ( 'NONE',  ( 0.07326958550568327122, -0.09842519685039370636, 0.2080556247247394019 ) ) ;
#17006 = CARTESIAN_POINT ( 'NONE',  ( -1.033464566929133799, 0.000000000000000000, 0.7480314959554645871 ) ) ;
#17007 = CARTESIAN_POINT ( 'NONE',  ( -0.7646288533564489232, 0.1113553986120547346, 0.05413385816018952829 ) ) ;
#17008 = EDGE_CURVE ( 'NONE', #40254, #10382, #3870, .T. ) ;
#17009 = EDGE_CURVE ( 'NONE', #31513, #3955, #9199, .T. ) ;
#17010 = VECTOR ( 'NONE', #31845, 39.37007874015748854 ) ;
#17011 = ORIENTED_EDGE ( 'NONE', *, *, #16413, .F. ) ;
#17012 = CARTESIAN_POINT ( 'NONE',  ( -1.002407869896990045, 0.1264236179284866091, 1.252460629867496067 ) ) ;
#17013 = VERTEX_POINT ( 'NONE', #5603 ) ;
#17014 = AXIS2_PLACEMENT_3D ( 'NONE', #24963, #13697, #38860 ) ;
#17015 = VECTOR ( 'NONE', #42466, 39.37007874015748854 ) ;
#17016 = CARTESIAN_POINT ( 'NONE',  ( -1.094772975963752103E-17, -1.152066929080094448, -0.1787899950787401882 ) ) ;
#17017 = FACE_OUTER_BOUND ( 'NONE', #45799, .T. ) ;
#17018 = CARTESIAN_POINT ( 'NONE',  ( -0.07444174185955065859, -0.5595910536775339228, -0.1797182628040039087 ) ) ;
#17019 = CARTESIAN_POINT ( 'NONE',  ( -1.284448818897637956, 0.000000000000000000, 1.181102362204724310 ) ) ;
#17020 = CARTESIAN_POINT ( 'NONE',  ( -0.7646288533564489232, -0.1113553986120547346, 0.7726377951680629685 ) ) ;
#17021 = CARTESIAN_POINT ( 'NONE',  ( -0.7185039370078739607, 1.928577636452523993E-17, 0.7381889763779527769 ) ) ;
#17022 = CARTESIAN_POINT ( 'NONE',  ( -0.1574803149606300301, 0.04872047244094490637, -0.06523048226347956391 ) ) ;
#17023 = CARTESIAN_POINT ( 'NONE',  ( 0.9500414927467378812, 0.1787899950787401604, 0.9350393700249758355 ) ) ;
#17024 = CARTESIAN_POINT ( 'NONE',  ( 0.01990234270466926386, -0.2840036093443640275, -0.08759220388353182452 ) ) ;
#17026 = FILL_AREA_STYLE_COLOUR ( '', #46055 ) ;
#17025 = CARTESIAN_POINT ( 'NONE',  ( 0.1476377952755906220, -0.9875035750853327077, -1.463737590216208861 ) ) ;
#17027 = CARTESIAN_POINT ( 'NONE',  ( 0.7185039370078739607, 1.928577636452523993E-17, 0.1771653542231816925 ) ) ;
#17028 = ORIENTED_EDGE ( 'NONE', *, *, #44668, .F. ) ;
#17029 = CARTESIAN_POINT ( 'NONE',  ( 0.7185039370078746268, 0.06523048226347956391, 0.1845472440944883052 ) ) ;
#17030 = CARTESIAN_POINT ( 'NONE',  ( 0.9873396505805591694, -0.1113553986120547346, 1.845472440837354178 ) ) ;
#17031 = CARTESIAN_POINT ( 'NONE',  ( -1.033464566929134687, -0.06523048226347956391, 1.188484251968505268 ) ) ;
#17032 = CARTESIAN_POINT ( 'NONE',  ( 3.284318927891251994E-17, -0.6648622046706456068, 0.1787899950787401882 ) ) ;
#17033 = CARTESIAN_POINT ( 'NONE',  ( 0.1787899950787401604, -1.361220472387181690, 0.07405724077823318263 ) ) ;
#17034 = VECTOR ( 'NONE', #37194, 39.37007874015748143 ) ;
#17035 = CARTESIAN_POINT ( 'NONE',  ( -0.6971942568897637749, 2.189545951927499583E-17, 1.970964566875370139 ) ) ;
#17036 = ORIENTED_EDGE ( 'NONE', *, *, #40135, .T. ) ;
#17037 = CARTESIAN_POINT ( 'NONE',  ( -1.054774247047244096, 0.000000000000000000, 1.523129921206078707 ) ) ;
#17038 = CARTESIAN_POINT ( 'NONE',  ( 1.054774247047244540, -0.07405724077823318263, 1.441929133804504604 ) ) ;
#17039 = DIRECTION ( 'NONE',  ( -1.000000000000000000, 0.000000000000000000, 0.000000000000000000 ) ) ;
#17040 = AXIS2_PLACEMENT_3D ( 'NONE', #40111, #29866, #22382 ) ;
#17041 = CARTESIAN_POINT ( 'NONE',  ( 1.033464566929133799, 1.928577636452524610E-17, 4.498031496062992574 ) ) ;
#17042 = CARTESIAN_POINT ( 'NONE',  ( 0.6971942568897648851, -0.07405724077823297447, 0.5610236219934807700 ) ) ;
#17043 = CARTESIAN_POINT ( 'NONE',  ( -1.002407869896990045, -0.1264236179284866091, 0.6077755904974173617 ) ) ;
#17044 = LINE ( 'NONE', #12994, #21519 ) ;
#17045 = EDGE_CURVE ( 'NONE', #41784, #3252, #20211, .T. ) ;
#17046 = ORIENTED_EDGE ( 'NONE', *, *, #27476, .F. ) ;
#17047 = CARTESIAN_POINT ( 'NONE',  ( -0.8019270111902717657, 0.1787899950787401604, 1.496062992072220821 ) ) ;
#17048 = CONICAL_SURFACE ( 'NONE', #43821, 0.1377952755905510474, 0.9599310885968920237 ) ;
#17049 = CARTESIAN_POINT ( 'NONE',  ( -1.033464566929134687, -0.06523048226347956391, 0.5191929133858269596 ) ) ;
#17050 = CARTESIAN_POINT ( 'NONE',  ( 1.054774247047244540, 0.07405724077823318263, 1.289370078686393750 ) ) ;
#17051 = CARTESIAN_POINT ( 'NONE',  ( -0.2379425218648307250, -0.09851385171600395008, 0.03197312892090157371 ) ) ;
#17052 = ORIENTED_EDGE ( 'NONE', *, *, #14563, .F. ) ;
#17053 = ADVANCED_FACE ( 'NONE', ( #15940 ), #13051, .T. ) ;
#17054 = CARTESIAN_POINT ( 'NONE',  ( -0.8759842519685039353, 0.000000000000000000, 0.000000000000000000 ) ) ;
#17055 = CARTESIAN_POINT ( 'NONE',  ( -0.9500414927467378812, 0.1787899950787401604, 1.018700787347811110 ) ) ;
#17056 = ORIENTED_EDGE ( 'NONE', *, *, #6978, .F. ) ;
#17057 = CARTESIAN_POINT ( 'NONE',  ( 0.1264236179284866091, -0.5270669290800944484, -0.1264236179284866091 ) ) ;
#17058 = CARTESIAN_POINT ( 'NONE',  ( 0.7185039370078739607, 1.928577636452523993E-17, 0.5019685039370078705 ) ) ;
#17059 = ORIENTED_EDGE ( 'NONE', *, *, #29711, .F. ) ;
#17060 = CARTESIAN_POINT ( 'NONE',  ( -0.1787899950787401882, -0.7878937007336378473, 0.000000000000000000 ) ) ;
#17061 = CIRCLE ( 'NONE', #32419, 0.08090551181102362266 ) ;
#17062 = CARTESIAN_POINT ( 'NONE',  ( 0.7646288533564489232, -0.1113553986120547346, 0.1820866140657015630 ) ) ;
#17063 = CARTESIAN_POINT ( 'NONE',  ( 0.1620125769266285432, -0.1593973085597378270, -5.302411703423666122E-08 ) ) ;
#17064 = ORIENTED_EDGE ( 'NONE', *, *, #25015, .T. ) ;
#17065 = AXIS2_PLACEMENT_3D ( 'NONE', #2843, #39736, #46944 ) ;
#17066 = CARTESIAN_POINT ( 'NONE',  ( -0.1787899950787401882, 0.06237603177076121719, 0.000000000000000000 ) ) ;
#17067 = CARTESIAN_POINT ( 'NONE',  ( -0.1264236179284866091, 0.03887795280966901967, 0.1264236179284866091 ) ) ;
#17068 = ITEM_DEFINED_TRANSFORMATION ( 'NONE', 'NONE', #36984,  #20860 ) ;
#17069 = CARTESIAN_POINT ( 'NONE',  ( 0.04918729031099923488, -0.09842519685039373412, 0.1567634384477433751 ) ) ;
#17070 = CLOSED_SHELL ( 'NONE', ( #37706, #9757, #13070, #13486, #45875, #21654, #30436, #23277, #4691, #3983, #37501, #14068, #44174, #32110, #23556, #35510, #2318, #26697, #19483, #20289, #8604, #14144, #6368, #19372, #9969, #45786, #5756, #20935, #35023, #7416 ) ) ;
#17071 = CARTESIAN_POINT ( 'NONE',  ( -1.054774247047244540, 0.07405724077823318263, 0.8562992125446617919 ) ) ;
#17073 = LINE ( 'NONE', #12798, #1671 ) ;
#17072 = CARTESIAN_POINT ( 'NONE',  ( -0.1574803149606299191, -0.8937007874015748810, 0.000000000000000000 ) ) ;
#17075 = CARTESIAN_POINT ( 'NONE',  ( -0.7680718972492022178, -0.1324197970153654924, 1.986028192752562482 ) ) ;
#17074 = CARTESIAN_POINT ( 'NONE',  ( 0.1270800023317771588, -1.797287904071236397, 0.1270800023317771588 ) ) ;
#17076 = CARTESIAN_POINT ( 'NONE',  ( 0.7495606340400177148, -0.1264236179284866091, 1.547736220418677089 ) ) ;
#17078 = CARTESIAN_POINT ( 'NONE',  ( -0.7646288533564489232, -0.1113553986120547346, 1.806102362204724532 ) ) ;
#17077 = CARTESIAN_POINT ( 'NONE',  ( 1.054774247047244096, 0.000000000000000000, 1.990649606245448844 ) ) ;
#17079 = CARTESIAN_POINT ( 'NONE',  ( 1.054774247047244096, 0.000000000000000000, 0.3371062991588349989 ) ) ;
#17080 = ORIENTED_EDGE ( 'NONE', *, *, #11323, .F. ) ;
#17082 = ORIENTED_EDGE ( 'NONE', *, *, #23019, .F. ) ;
#17081 = CARTESIAN_POINT ( 'NONE',  ( -0.1351206911654056209, -0.09842519685039369248, -0.2074211034487065675 ) ) ;
#17083 = CARTESIAN_POINT ( 'NONE',  ( -0.3980944881889753040, 0.4370297686271547022, 0.6367018223237037589 ) ) ;
#17084 = DIRECTION ( 'NONE',  ( 0.000000000000000000, 1.000000000000000000, 0.000000000000000000 ) ) ;
#17086 = CARTESIAN_POINT ( 'NONE',  ( -0.1264236179284866091, -0.1678149605761578844, -0.1264236179284866091 ) ) ;
#17085 = CARTESIAN_POINT ( 'NONE',  ( 0.06523048226347956391, -0.8961614172153083979, -0.1574803149606300301 ) ) ;
#17087 = CARTESIAN_POINT ( 'NONE',  ( 1.054774247047244540, 0.07405724077823318263, 0.5757874015210394658 ) ) ;
#17088 = CARTESIAN_POINT ( 'NONE',  ( -0.1787899950787401882, -0.8666338582139527791, 0.000000000000000000 ) ) ;
#17089 = CARTESIAN_POINT ( 'NONE',  ( 0.7938769800658418418, -0.1410816750883244208, 0.03937005840330796980 ) ) ;
#17090 = LINE ( 'NONE', #2700, #38462 ) ;
#17091 = CARTESIAN_POINT ( 'NONE',  ( -0.9500414927467378812, 0.1787899950787401604, 1.446850393647023614 ) ) ;
#17092 = ORIENTED_EDGE ( 'NONE', *, *, #20351, .T. ) ;
#17093 = CARTESIAN_POINT ( 'NONE',  ( -0.2927220607601823121, -0.1026043301529236951, -1.008602447134615776 ) ) ;
#17094 = CARTESIAN_POINT ( 'NONE',  ( 0.6971942568897648851, 0.07405724077823318263, 1.028543307032851795 ) ) ;
#17095 = ORIENTED_EDGE ( 'NONE', *, *, #16209, .T. ) ;
#17096 = CARTESIAN_POINT ( 'NONE',  ( -0.1113553986120547346, -1.075787401467275695, 0.1113553986120547346 ) ) ;
#17097 = DIRECTION ( 'NONE',  ( 0.000000000000000000, 0.000000000000000000, 1.000000000000000000 ) ) ;
#17098 = CARTESIAN_POINT ( 'NONE',  ( -0.9412147342319837628, -0.1574803149606297803, 1.419783464566930276 ) ) ;
#17099 = CARTESIAN_POINT ( 'NONE',  ( -0.6971942568897626646, 0.07405724077823318263, 0.9055118109698585549 ) ) ;
#17100 = CARTESIAN_POINT ( 'NONE',  ( 0.9412147342319837628, -0.1574803149606297803, 1.803641732175937706 ) ) ;
#17101 = CARTESIAN_POINT ( 'NONE',  ( -0.2471922904502826812, -0.09842519685039370636, 0.1427165354330708902 ) ) ;
#17102 = CARTESIAN_POINT ( 'NONE',  ( 1.054774247047244540, 0.07405724077823318263, 0.1476377952218269340 ) ) ;
#17103 = CARTESIAN_POINT ( 'NONE',  ( -1.002407869896990045, 0.1264236179284866091, 0.1451771653005673179 ) ) ;
#17104 = CARTESIAN_POINT ( 'NONE',  ( 1.033464566929134687, -0.06523048226347956391, 1.611712598317668999 ) ) ;
#17105 = EDGE_LOOP ( 'NONE', ( #45774, #3554, #20980, #9574 ) ) ;
#17106 = ADVANCED_FACE ( 'NONE', ( #27212 ), #20452, .T. ) ;
#17107 = CARTESIAN_POINT ( 'NONE',  ( -0.1787899950787401882, 0.1126968504474643862, 0.000000000000000000 ) ) ;
#17108 = CARTESIAN_POINT ( 'NONE',  ( 1.033464566929134687, -0.06523048226347956391, 0.5979330708661413363 ) ) ;
#17109 = EDGE_LOOP ( 'NONE', ( #38678, #32027, #29051, #5843 ) ) ;
#17110 = CARTESIAN_POINT ( 'NONE',  ( -0.8019270111902716547, -0.1787899950787401604, 1.663385826717890925 ) ) ;
#17111 = AXIS2_PLACEMENT_3D ( 'NONE', #19605, #34952, #16726 ) ;
#17112 = VERTEX_POINT ( 'NONE', #42249 ) ;
#17113 = ADVANCED_FACE ( 'NONE', ( #41517 ), #34379, .F. ) ;
#17114 = CARTESIAN_POINT ( 'NONE',  ( -0.2471922904502826812, 0.07885719401822635644, -0.07558487950069482653 ) ) ;
#17115 = CARTESIAN_POINT ( 'NONE',  ( -0.7185039370078746268, -0.06523048226347956391, 0.7800196850393691372 ) ) ;
#17116 = CARTESIAN_POINT ( 'NONE',  ( -1.094772975963752103E-17, -1.089198771378844466, -0.1787899950787401882 ) ) ;
#17117 = COLOUR_RGB ( '', 0.66274510, 0.83137255, 0.94901961) ;
#17118 = ORIENTED_EDGE ( 'NONE', *, *, #2162, .T. ) ;
#17119 = CARTESIAN_POINT ( 'NONE',  ( 0.07405724077823318263, -0.1850393700249766959, 0.1787899950787401604 ) ) ;
#17120 = ORIENTED_EDGE ( 'NONE', *, *, #15990, .T. ) ;
#17121 = VERTEX_POINT ( 'NONE', #19743 ) ;
#17122 = CARTESIAN_POINT ( 'NONE',  ( 0.002794899975992053229, -0.1377744224360938075, -0.03695826049548953801 ) ) ;
#17123 = CARTESIAN_POINT ( 'NONE',  ( -0.1574803149606299191, 0.000000000000000000, -0.1183602362204724257 ) ) ;
#17124 = CARTESIAN_POINT ( 'NONE',  ( 0.7185039370078739607, 1.928577636452523993E-17, 1.840551181102362266 ) ) ;
#17125 = CARTESIAN_POINT ( 'NONE',  ( -0.07444174185955065859, -0.2298666442287148337, 0.1797182628040039087 ) ) ;
#17126 = CARTESIAN_POINT ( 'NONE',  ( 0.07405724077823318263, -0.8051181101824581576, -0.1787899950787401604 ) ) ;
#17127 = EDGE_CURVE ( 'NONE', #37845, #22837, #35265, .T. ) ;
#17128 = CARTESIAN_POINT ( 'NONE',  ( -0.6971942568897637749, 2.189545951927499583E-17, 0.3617125983714334359 ) ) ;
#17129 = CARTESIAN_POINT ( 'NONE',  ( -0.7185039370078746268, 0.06523048226347956391, 1.090059055118109965 ) ) ;
#17130 = CARTESIAN_POINT ( 'NONE',  ( -0.1270800023317771588, -1.147681604858635795, -0.1270800023317771588 ) ) ;
#17131 = CARTESIAN_POINT ( 'NONE',  ( -0.06200172126964421937, 0.2596975217971581040, -0.05114647357131848343 ) ) ;
#17132 = CARTESIAN_POINT ( 'NONE',  ( 0.8759842519685039353, 0.1787899950787401882, 1.021161417269070837 ) ) ;
#17133 = CARTESIAN_POINT ( 'NONE',  ( 0.6971942568897648851, -0.07405724077823297447, 1.461614173174583753 ) ) ;
#17134 = CARTESIAN_POINT ( 'NONE',  ( 1.054774247047244540, -0.07405724077823318263, 0.2165354330171024577 ) ) ;
#17135 = LINE ( 'NONE', #28415, #5487 ) ;
#17136 = CARTESIAN_POINT ( 'NONE',  ( 0.1574803149606299191, 1.928577636452524610E-17, -0.04012007874015743186 ) ) ;
#17137 = CARTESIAN_POINT ( 'NONE',  ( 0.5660731898098425585, 4.766607801171850497E-17, 0.000000000000000000 ) ) ;
#17138 = CARTESIAN_POINT ( 'NONE',  ( -0.1574803149606299191, -0.7263779526483780113, 0.000000000000000000 ) ) ;
#17139 = CARTESIAN_POINT ( 'NONE',  ( -1.033464566929134687, 0.06523048226347956391, 1.695374015640504828 ) ) ;
#17140 = CARTESIAN_POINT ( 'NONE',  ( -0.07405724077823318263, 0.04625984257344856188, 0.1787899950787401604 ) ) ;
#17141 = CARTESIAN_POINT ( 'NONE',  ( 1.033464566929133799, 0.000000000000000000, 1.663385826771653697 ) ) ;
#17143 = CARTESIAN_POINT ( 'NONE',  ( -1.033464566929133799, 0.000000000000000000, 1.938976377952756014 ) ) ;
#17142 = CARTESIAN_POINT ( 'NONE',  ( 1.002407869896990045, 0.1264236179284866091, 1.129429133804503937 ) ) ;
#17144 = CYLINDRICAL_SURFACE ( 'NONE', #44200, 0.1574803149606299191 ) ;
#17145 = CARTESIAN_POINT ( 'NONE',  ( -0.8019270111902717657, -0.1787899950787401604, 1.151574803095843036 ) ) ;
#17146 = CARTESIAN_POINT ( 'NONE',  ( 0.9412147342319837628, 0.1574803149606300301, 0.4404527557979849850 ) ) ;
#17147 = ORIENTED_EDGE ( 'NONE', *, *, #10785, .T. ) ;
#17148 = AXIS2_PLACEMENT_3D ( 'NONE', #31181, #42400, #3090 ) ;
#17149 = EDGE_CURVE ( 'NONE', #2, #45855, #17564, .T. ) ;
#17150 = CARTESIAN_POINT ( 'NONE',  ( 0.5415383587465882886, 4.466152701071653354E-17, 0.000000000000000000 ) ) ;
#17151 = EDGE_CURVE ( 'NONE', #22900, #20097, #13536, .T. ) ;
#17152 = CARTESIAN_POINT ( 'NONE',  ( -0.7185039370078739607, 1.928577636452523993E-17, 0.2952755904436539236 ) ) ;
#17153 = ORIENTED_EDGE ( 'NONE', *, *, #22284, .T. ) ;
#17154 = CARTESIAN_POINT ( 'NONE',  ( 0.9500414927467378812, 0.1787899950787401604, 1.289370078686393750 ) ) ;
#17156 = FACE_OUTER_BOUND ( 'NONE', #17109, .T. ) ;
#17155 = DIRECTION ( 'NONE',  ( 1.000000000000000000, 0.000000000000000000, -4.336808689942015271E-16 ) ) ;
#17157 = CARTESIAN_POINT ( 'NONE',  ( 0.07405724077823318263, -0.01279527553678768380, -0.1787899950787401604 ) ) ;
#17158 = FACE_OUTER_BOUND ( 'NONE', #47183, .T. ) ;
#17159 = ( BOUNDED_CURVE ( )  B_SPLINE_CURVE ( 2, ( #18491, #14912, #7466, #25708, #7241, #22086, #32669, #32906, #25216 ),
 .UNSPECIFIED., .F., .T. ) 
 B_SPLINE_CURVE_WITH_KNOTS ( ( 3, 2, 2, 2, 3 ),
 ( 0.4600000000000000200, 0.4625000000000000222, 0.4650000000000000244, 0.4675000000000000266, 0.4699999999999999734 ),
 .UNSPECIFIED. ) 
 CURVE ( )  GEOMETRIC_REPRESENTATION_ITEM ( )  RATIONAL_B_SPLINE_CURVE ( ( 1.000000000000000000, 0.9238795325112869605, 1.000000000000000000, 0.9238795325112869605, 1.000000000000000000, 0.9238795325112869605, 1.000000000000000000, 0.9238795325112849621, 1.000000000000000000 ) ) 
 REPRESENTATION_ITEM ( '' )  ) ;
#17160 = EDGE_CURVE ( 'NONE', #42416, #47237, #708, .T. ) ;
#17161 = ORIENTED_EDGE ( 'NONE', *, *, #12877, .F. ) ;
#17162 = DIRECTION ( 'NONE',  ( 0.000000000000000000, 0.000000000000000000, 1.000000000000000000 ) ) ;
#17163 = CARTESIAN_POINT ( 'NONE',  ( -0.7185039370078746268, 0.06523048226347956391, 0.2140748030420794590 ) ) ;
#17164 = ORIENTED_EDGE ( 'NONE', *, *, #22775, .F. ) ;
#17165 = ORIENTED_EDGE ( 'NONE', *, *, #9702, .T. ) ;
#17166 = CARTESIAN_POINT ( 'NONE',  ( -0.9500414927467377701, 0.1787899950787401604, 1.368110236166710125 ) ) ;
#17167 = CARTESIAN_POINT ( 'NONE',  ( 0.1787899950787401604, -1.759842519631276581, 0.07405724077823318263 ) ) ;
#17168 = CARTESIAN_POINT ( 'NONE',  ( -0.7185039370078739607, 1.928577636452523993E-17, 0.02952755905511811330 ) ) ;
#17169 = EDGE_LOOP ( 'NONE', ( #17654, #24845, #45475, #10936 ) ) ;
#17170 = CARTESIAN_POINT ( 'NONE',  ( -1.054774247047244540, 0.07405724077823318263, 1.087598425143086578 ) ) ;
#17171 = EDGE_CURVE ( 'NONE', #39764, #7863, #26719, .T. ) ;
#17172 = CARTESIAN_POINT ( 'NONE',  ( -0.6971942568897626646, -0.07405724077823297447, 0.7185039369541108556 ) ) ;
#17173 = EDGE_CURVE ( 'NONE', #9764, #23901, #14591, .T. ) ;
#17174 = AXIS2_PLACEMENT_3D ( 'NONE', #25330, #39918, #3515 ) ;
#17175 = CARTESIAN_POINT ( 'NONE',  ( 0.008639645916121835995, 0.06621452963738141961, -0.1377924362075181319 ) ) ;
#17176 = CARTESIAN_POINT ( 'NONE',  ( 0.1264236179284866091, -0.7004192438197893722, -0.1264236179284866091 ) ) ;
#17177 = VERTEX_POINT ( 'NONE', #29595 ) ;
#17178 = CARTESIAN_POINT ( 'NONE',  ( -1.033464566929133799, 0.000000000000000000, 0.04921259842519685318 ) ) ;
#17179 = CARTESIAN_POINT ( 'NONE',  ( -0.8759842519685039353, -0.1574803149606299191, 0.6594488187901103027 ) ) ;
#17180 = VECTOR ( 'NONE', #28795, 39.37007874015748143 ) ;
#17181 = ORIENTED_EDGE ( 'NONE', *, *, #16492, .F. ) ;
#17182 = ( BOUNDED_CURVE ( )  B_SPLINE_CURVE ( 2, ( #26488, #41050, #11389, #8248, #4395, #22874, #12103, #567, #22638 ),
 .UNSPECIFIED., .F., .T. ) 
 B_SPLINE_CURVE_WITH_KNOTS ( ( 3, 2, 2, 2, 3 ),
 ( 0.6999999999999999556, 0.7025000000000000133, 0.7049999999999999600, 0.7075000000000000178, 0.7099999999999999645 ),
 .UNSPECIFIED. ) 
 CURVE ( )  GEOMETRIC_REPRESENTATION_ITEM ( )  RATIONAL_B_SPLINE_CURVE ( ( 1.000000000000000000, 0.9238795325112899581, 1.000000000000000000, 0.9238795325112869605, 1.000000000000000000, 0.9238795325112869605, 1.000000000000000000, 0.9238795325112869605, 1.000000000000000000 ) ) 
 REPRESENTATION_ITEM ( '' )  ) ;
#17183 = CARTESIAN_POINT ( 'NONE',  ( -0.8019270111902717657, 0.1787899950787401604, 0.7037401574265510495 ) ) ;
#17184 = CARTESIAN_POINT ( 'NONE',  ( 0.06523048226347956391, -0.0004921259842519827002, -0.1574803149606300301 ) ) ;
#17185 = ORIENTED_EDGE ( 'NONE', *, *, #5153, .F. ) ;
#17186 = VECTOR ( 'NONE', #9688, 39.37007874015748143 ) ;
#17187 = CARTESIAN_POINT ( 'NONE',  ( -0.7495606340400177148, 0.1264236179284866091, 1.656003936954110412 ) ) ;
#17188 = DIRECTION ( 'NONE',  ( 0.000000000000000000, 0.000000000000000000, -1.000000000000000000 ) ) ;
#17189 = FILL_AREA_STYLE ('',( #20543 ) ) ;
#17190 = CYLINDRICAL_SURFACE ( 'NONE', #22365, 0.1968503937007874405 ) ;
#17191 = CARTESIAN_POINT ( 'NONE',  ( 0.8107537697050253289, 0.1574803149606300301, 0.6126968503937006982 ) ) ;
#17192 = CARTESIAN_POINT ( 'NONE',  ( -1.100456976456230270E-17, -0.6801619198192657700, -0.1797182628040039365 ) ) ;
#17194 = CARTESIAN_POINT ( 'NONE',  ( 0.000000000000000000, -0.09842519685039370636, 0.000000000000000000 ) ) ;
#17193 = CARTESIAN_POINT ( 'NONE',  ( -0.1574803149606297803, -0.6550196850393706915, 0.06523048226347956391 ) ) ;
#17195 = DIRECTION ( 'NONE',  ( 0.000000000000000000, 0.000000000000000000, -1.000000000000000000 ) ) ;
#17196 = VERTEX_POINT ( 'NONE', #37416 ) ;
#17197 = EDGE_CURVE ( 'NONE', #10582, #3955, #2481, .T. ) ;
#17198 = CIRCLE ( 'NONE', #5771, 0.1574803149606299191 ) ;
#17199 = CARTESIAN_POINT ( 'NONE',  ( 0.8107537697050254399, 0.1574803149606300301, 1.587106299105070839 ) ) ;
#17200 = CARTESIAN_POINT ( 'NONE',  ( 0.8107537697050253289, -0.1574803149606297803, 1.296751968503936370 ) ) ;
#17201 = CYLINDRICAL_SURFACE ( 'NONE', #15691, 0.009842519685039371677 ) ;
#17203 = CARTESIAN_POINT ( 'NONE',  ( -0.7185039370078746268, -0.06523048226347956391, 1.331200787401575436 ) ) ;
#17202 = CARTESIAN_POINT ( 'NONE',  ( 0.3690944881889771101, 0.1864803149606328037, 0.7480314960629921295 ) ) ;
#17204 = CARTESIAN_POINT ( 'NONE',  ( 0.8759842519685039353, 0.000000000000000000, 4.498031496062992574 ) ) ;
#17206 = FACE_OUTER_BOUND ( 'NONE', #12713, .T. ) ;
#17205 = CARTESIAN_POINT ( 'NONE',  ( 1.002407869896990045, 0.1264236179284866091, 0.7357283464029290565 ) ) ;
#17207 = CARTESIAN_POINT ( 'NONE',  ( -0.1611263444889494134, -0.08956074569868537061, -0.06449846707264046686 ) ) ;
#17209 = AXIS2_PLACEMENT_3D ( 'NONE', #313, #33654, #14962 ) ;
#17208 = CARTESIAN_POINT ( 'NONE',  ( -0.1787899950787401604, -0.6673228345919050009, 0.07405724077823318263 ) ) ;
#17210 = ORIENTED_EDGE ( 'NONE', *, *, #46039, .T. ) ;
#17211 = EDGE_CURVE ( 'NONE', #37199, #18156, #12017, .T. ) ;
#17212 = CARTESIAN_POINT ( 'NONE',  ( -0.9412147342319837628, -0.1574803149606297803, 1.065452755905511806 ) ) ;
#17213 = CIRCLE ( 'NONE', #7263, 0.09842519685039370636 ) ;
#17214 = CIRCLE ( 'NONE', #42469, 0.2559055118110236116 ) ;
#17215 = CARTESIAN_POINT ( 'NONE',  ( 0.003062405574111899762, 0.1000190445539651529, -0.1023525292013673232 ) ) ;
#17216 = CARTESIAN_POINT ( 'NONE',  ( 0.7495606340400177148, 0.1264236179284866091, 0.9030511810485984947 ) ) ;
#17217 = CARTESIAN_POINT ( 'NONE',  ( 1.033464566929134687, -0.06523048226347956391, 1.464074803149607140 ) ) ;
#17218 = CARTESIAN_POINT ( 'NONE',  ( 0.7185039370078739607, 1.928577636452523993E-17, 0.6889763778452283605 ) ) ;
#17219 = CARTESIAN_POINT ( 'NONE',  ( -0.07405724077823318263, -1.804133858213953889, 0.1787899950787401604 ) ) ;
#17220 = CARTESIAN_POINT ( 'NONE',  ( -0.1787899950787401604, -1.105314960576158301, 0.07405724077823318263 ) ) ;
#17221 = CARTESIAN_POINT ( 'NONE',  ( 0.1113553986120547346, -1.302165354330708791, -0.1113553986120547346 ) ) ;
#17222 = CARTESIAN_POINT ( 'NONE',  ( 0.8107537697050253289, -0.1574803149606297803, 1.208169291231056430 ) ) ;
#17223 = CARTESIAN_POINT ( 'NONE',  ( -1.033464566929131356, 0.06523048226348168721, 1.390255905511812218 ) ) ;
#17224 = UNCERTAINTY_MEASURE_WITH_UNIT (LENGTH_MEASURE( 1.000000000000000082E-05 ), #18094, 'distance_accuracy_value', 'NONE') ;
#17225 = CARTESIAN_POINT ( 'NONE',  ( -0.9500414927467378812, 0.1787899950787401604, 1.845472440891119392 ) ) ;
#17226 = CARTESIAN_POINT ( 'NONE',  ( -1.033464566929133799, 0.000000000000000000, 0.8267716534357796299 ) ) ;
#17227 = VERTEX_POINT ( 'NONE', #22100 ) ;
#17228 = CARTESIAN_POINT ( 'NONE',  ( -1.054774247047244540, 0.07405724077823318263, 1.879921259788756016 ) ) ;
#17229 = CARTESIAN_POINT ( 'NONE',  ( -1.054774247047244540, 0.07405724077823318263, 1.481299212544662680 ) ) ;
#17230 = DIRECTION ( 'NONE',  ( 0.000000000000000000, 0.000000000000000000, 1.000000000000000000 ) ) ;
#17231 = CARTESIAN_POINT ( 'NONE',  ( -0.8759842519685039353, 0.1787899950787401882, 0.9768700786863937502 ) ) ;
#17232 = CARTESIAN_POINT ( 'NONE',  ( -0.2471922904502826257, 0.07319706521783654607, 0.08615678709745397401 ) ) ;
#17233 = CARTESIAN_POINT ( 'NONE',  ( -0.8019270111902717657, -0.1787899950787401604, 1.825787401521040243 ) ) ;
#17234 = CARTESIAN_POINT ( 'NONE',  ( -0.2272550450522833887, 0.05212746764704522667, 0.1542273094305053049 ) ) ;
#17235 = CARTESIAN_POINT ( 'NONE',  ( -0.7185039370078739607, 1.928577636452523993E-17, 1.919291338582677309 ) ) ;
#17236 = CARTESIAN_POINT ( 'NONE',  ( 0.000000000000000000, 1.205361022782826802E-17, -0.09842519685039370636 ) ) ;
#17237 = CARTESIAN_POINT ( 'NONE',  ( 0.07405724077823318263, -0.3042578264969555413, -0.1787899950787401604 ) ) ;
#17238 = CARTESIAN_POINT ( 'NONE',  ( 0.03196316912850031416, -0.09842519685039370636, -0.1894554451039858478 ) ) ;
#17239 = DIRECTION ( 'NONE',  ( 0.5735764363510417185, 0.6455006197386566891, -0.5043203561029927506 ) ) ;
#17240 = LINE ( 'NONE', #31876, #47139 ) ;
#17241 = AXIS2_PLACEMENT_3D ( 'NONE', #30220, #18905, #45245 ) ;
#17242 = CIRCLE ( 'NONE', #44009, 0.02900000000000001882 ) ;
#17243 = EDGE_LOOP ( 'NONE', ( #6370, #1048, #31339, #16135 ) ) ;
#17244 = CONICAL_SURFACE ( 'NONE', #34094, 0.1787899950787401049, 1.047197551196598297 ) ;
#17245 = CARTESIAN_POINT ( 'NONE',  ( -0.8759842519685039353, -0.1787899950787401882, 1.237696850339937038 ) ) ;
#17246 = ORIENTED_EDGE ( 'NONE', *, *, #39211, .F. ) ;
#17247 = AXIS2_PLACEMENT_3D ( 'NONE', #41305, #8030, #26511 ) ;
#17248 = CARTESIAN_POINT ( 'NONE',  ( -0.1787899950787401604, -1.188976377898991688, -0.07405724077823318263 ) ) ;
#17249 = CARTESIAN_POINT ( 'NONE',  ( -1.094772975963752103E-17, -1.270177165300566902, -0.1787899950787401882 ) ) ;
#17250 = CARTESIAN_POINT ( 'NONE',  ( -0.1797182628040039087, -0.4710083765121794164, 0.07444174185955065859 ) ) ;
#17251 = LINE ( 'NONE', #24919, #40787 ) ;
#17252 = CARTESIAN_POINT ( 'NONE',  ( -0.9873396505805591694, -0.1113553986120547346, 0.7923228346456693272 ) ) ;
#17253 = CARTESIAN_POINT ( 'NONE',  ( 0.1113553986120547346, 0.03641732283464567399, -0.1113553986120547346 ) ) ;
#17254 = EDGE_CURVE ( 'NONE', #34930, #35290, #36726, .T. ) ;
#17255 = CARTESIAN_POINT ( 'NONE',  ( 0.9873396505805591694, 0.1113553986120547346, 0.8415354330708662012 ) ) ;
#17256 = CARTESIAN_POINT ( 'NONE',  ( -0.9873396505805591694, 0.1113553986120547346, 1.077755905511811108 ) ) ;
#17257 = EDGE_CURVE ( 'NONE', #34984, #23841, #40996, .T. ) ;
#17259 = CARTESIAN_POINT ( 'NONE',  ( 1.928577636452524610E-17, -0.09842519685039370636, -0.1574803149606299191 ) ) ;
#17258 = CARTESIAN_POINT ( 'NONE',  ( 0.1595947434767874262, 0.2033521641548338144, -0.03294411891277416321 ) ) ;
#17260 = CARTESIAN_POINT ( 'NONE',  ( 0.8759842519685039353, 0.1574803149606299191, 0.1673228345381423399 ) ) ;
#17261 = EDGE_CURVE ( 'NONE', #15306, #1625, #18431, .T. ) ;
#17262 = ORIENTED_EDGE ( 'NONE', *, *, #36755, .F. ) ;
#17263 = AXIS2_PLACEMENT_3D ( 'NONE', #37794, #26316, #11691 ) ;
#17264 = ADVANCED_FACE ( 'NONE', ( #11335 ), #7480, .F. ) ;
#17265 = EDGE_LOOP ( 'NONE', ( #2468, #33953, #43339, #20477 ) ) ;
#17266 = DIRECTION ( 'NONE',  ( -1.000000000000000000, 0.000000000000000000, 0.000000000000000000 ) ) ;
#17267 = CARTESIAN_POINT ( 'NONE',  ( 0.07405724077823318263, -0.5688976377415115859, -0.1787899950787401604 ) ) ;
#17268 = CARTESIAN_POINT ( 'NONE',  ( 0.1787899950787401604, -1.316929133804503937, -0.07405724077823318263 ) ) ;
#17269 = CARTESIAN_POINT ( 'NONE',  ( -0.9500414927467378812, 0.1787899950787401604, 1.879921259788756016 ) ) ;
#17270 = ORIENTED_EDGE ( 'NONE', *, *, #8101, .F. ) ;
#17271 = CARTESIAN_POINT ( 'NONE',  ( -0.9500414927467378812, 0.1787899950787401604, 1.451771653489543290 ) ) ;
#17272 = CARTESIAN_POINT ( 'NONE',  ( 0.6971942568897637749, 2.189545951927499583E-17, 1.503444881836000002 ) ) ;
#17273 = VERTEX_POINT ( 'NONE', #512 ) ;
#17274 = CIRCLE ( 'NONE', #23414, 0.6872114956789353579 ) ;
#17275 = AXIS2_PLACEMENT_3D ( 'NONE', #43283, #28952, #10482 ) ;
#17276 = CARTESIAN_POINT ( 'NONE',  ( -0.8019270111902717657, -0.1787899950787401604, 0.6840551180564720113 ) ) ;
#17277 = CARTESIAN_POINT ( 'NONE',  ( 0.6971942568897637749, 2.189545951927499583E-17, 0.1648622046706460786 ) ) ;
#17278 = CARTESIAN_POINT ( 'NONE',  ( 0.1635870200194612933, -0.09842519684036495076, -0.07221633666346874425 ) ) ;
#17279 = CARTESIAN_POINT ( 'NONE',  ( 1.002407869896990045, -0.1264236179284866091, 0.5733267715997795166 ) ) ;
#17280 = CARTESIAN_POINT ( 'NONE',  ( -1.002407869896990045, -0.1264236179284866091, 0.4896653542769449086 ) ) ;
#17281 = CARTESIAN_POINT ( 'NONE',  ( 0.8759842519685039353, 0.000000000000000000, 4.498031496062992574 ) ) ;
#17282 = CARTESIAN_POINT ( 'NONE',  ( 0.1574803149606299746, 0.3740157480314960647, 0.9783464566929134243 ) ) ;
#17283 = ORIENTED_EDGE ( 'NONE', *, *, #7959, .F. ) ;
#17284 = CARTESIAN_POINT ( 'NONE',  ( -0.8759842519685039353, 0.1787899950787401882, 1.414862204670645829 ) ) ;
#17285 = CARTESIAN_POINT ( 'NONE',  ( -0.7646288533564489232, 0.1113553986120547346, 1.481299212598425230 ) ) ;
#17286 = CARTESIAN_POINT ( 'NONE',  ( -0.8759842519685039353, -0.1574803149606299191, 0.4330708661417322913 ) ) ;
#17287 = CARTESIAN_POINT ( 'NONE',  ( 1.002407869896990045, 0.1264236179284866091, 1.291830708607653477 ) ) ;
#17288 = CARTESIAN_POINT ( 'NONE',  ( -0.002277221062301980261, -0.09851385079347381446, 0.2245454195424968769 ) ) ;
#17289 = ORIENTED_EDGE ( 'NONE', *, *, #3089, .T. ) ;
#17290 = CARTESIAN_POINT ( 'NONE',  ( -1.033464566929134687, -0.06523048226347956391, 0.5585629921259840369 ) ) ;
#17291 = SHAPE_REPRESENTATION ( 'Side Bracket', ( #20860 ), #46110 ) ;
#17292 = CARTESIAN_POINT ( 'NONE',  ( 0.1787899950787401604, -1.726501920985144656, -0.07405724077823318263 ) ) ;
#17293 = ORIENTED_EDGE ( 'NONE', *, *, #33374, .F. ) ;
#17294 = CARTESIAN_POINT ( 'NONE',  ( -0.1264236179284866091, -0.5959645668753701386, -0.1264236179284866091 ) ) ;
#17295 = CARTESIAN_POINT ( 'NONE',  ( 0.1574803149606299191, 0.4666052258408008302, -0.7025346432751023995 ) ) ;
#17296 = ORIENTED_EDGE ( 'NONE', *, *, #34682, .T. ) ;
#17297 = CARTESIAN_POINT ( 'NONE',  ( 1.002407869896990045, -0.1264236179284866091, 1.434547244040724534 ) ) ;
#17298 = CARTESIAN_POINT ( 'NONE',  ( 0.1787899950787401604, -0.6919291338045056028, 0.07405724077823318263 ) ) ;
#17299 = CARTESIAN_POINT ( 'NONE',  ( -0.5314960629921260393, 1.928577636452522761E-17, 5.000000000000000000 ) ) ;
#17300 = CARTESIAN_POINT ( 'NONE',  ( 0.1641609508005656415, -0.1617434695452283633, -1.990205904980697972E-06 ) ) ;
#17301 = CARTESIAN_POINT ( 'NONE',  ( 0.8019270111902717657, -0.1787899950787401604, 1.663385826717890925 ) ) ;
#17302 = CARTESIAN_POINT ( 'NONE',  ( 0.9500414927467378812, 0.1787899950787401604, 0.3444881889226146243 ) ) ;
#17303 = CARTESIAN_POINT ( 'NONE',  ( -0.1787899950787401882, 0.02300595303060378252, 0.000000000000000000 ) ) ;
#17304 = CARTESIAN_POINT ( 'NONE',  ( 0.1787899950787401604, 0.05118110241596821736, 0.07405724077823318263 ) ) ;
#17305 = LINE ( 'NONE', #24975, #39460 ) ;
#17306 = CARTESIAN_POINT ( 'NONE',  ( 0.9873396505805591694, 0.1113553986120547346, 0.5561023620971968784 ) ) ;
#17307 = CARTESIAN_POINT ( 'NONE',  ( 1.002407869896990045, -0.1264236179284866091, 0.4896653542769449086 ) ) ;
#17308 = EDGE_CURVE ( 'NONE', #41232, #43350, #34507, .T. ) ;
#17309 = CARTESIAN_POINT ( 'NONE',  ( -0.8019270111902716547, 0.1787899950787401604, 0.8267716534895444003 ) ) ;
#17311 = CARTESIAN_POINT ( 'NONE',  ( 0.4620708661417369245, 1.354170115732555191, -0.4197102375732078561 ) ) ;
#17310 = CARTESIAN_POINT ( 'NONE',  ( -0.1574803149606300301, -0.8961614173228339419, -0.06523048226347956391 ) ) ;
#17312 = CARTESIAN_POINT ( 'NONE',  ( 0.1797182628040039365, -1.674256408008242047, -2.200913952912460540E-17 ) ) ;
#17313 = CARTESIAN_POINT ( 'NONE',  ( -0.1787899950787401604, -0.3917322834108032947, 0.07405724077823318263 ) ) ;
#17314 = CARTESIAN_POINT ( 'NONE',  ( 0.8019270111902717657, -0.1787899950787401604, 1.747047244040724312 ) ) ;
#17316 = CARTESIAN_POINT ( 'NONE',  ( 0.1636082376785381876, 0.1608670784834268785, 1.645031862152206036E-07 ) ) ;
#17315 = CARTESIAN_POINT ( 'NONE',  ( 0.1854001451104992926, 0.08095196624128539464, -0.1783922471787993125 ) ) ;
#17317 = CARTESIAN_POINT ( 'NONE',  ( 0.8759842519685039353, -0.1787899950787401882, 0.4453740156942677664 ) ) ;
#17318 = ORIENTED_EDGE ( 'NONE', *, *, #28485, .T. ) ;
#17319 = ADVANCED_FACE ( 'NONE', ( #30280 ), #41, .T. ) ;
#17320 = CARTESIAN_POINT ( 'NONE',  ( -7.957671378281915615E-17, 0.1564960629921311464, -0.3937007874015748254 ) ) ;
#17321 = CARTESIAN_POINT ( 'NONE',  ( 0.1738065908861024245, -0.1951474930446358835, -0.3118411609178733390 ) ) ;
#17322 = CARTESIAN_POINT ( 'NONE',  ( 0.07405724077823318263, -0.05708661411946481384, -0.1787899950787401604 ) ) ;
#17323 = CARTESIAN_POINT ( 'NONE',  ( 0.9500414927467378812, 0.1787899950787401604, 0.6594488188438737408 ) ) ;
#17324 = CARTESIAN_POINT ( 'NONE',  ( 0.07405724077823318263, -0.9183070865604088251, -0.1787899950787401604 ) ) ;
#17325 = CARTESIAN_POINT ( 'NONE',  ( 0.8182746624668372215, -0.1508186042162177609, 0.03937399344056087547 ) ) ;
#17326 = CARTESIAN_POINT ( 'NONE',  ( -1.033464566929133799, 0.000000000000000000, 0.6397637795275591399 ) ) ;
#17327 = CARTESIAN_POINT ( 'NONE',  ( 0.7646288533564489232, 0.1113553986120547346, 1.156496062884598608 ) ) ;
#17328 = CARTESIAN_POINT ( 'NONE',  ( -0.6971942568897637749, 2.189545951927499583E-17, 1.459153543253322693 ) ) ;
#17329 = ORIENTED_EDGE ( 'NONE', *, *, #2117, .T. ) ;
#17330 = CARTESIAN_POINT ( 'NONE',  ( 0.7185039370078732945, -0.06523048226347920309, 0.1500984251968504879 ) ) ;
#17331 = CARTESIAN_POINT ( 'NONE',  ( 1.054774247047244540, -0.07405724077823318263, 1.205708661363558365 ) ) ;
#17333 = ORIENTED_EDGE ( 'NONE', *, *, #29161, .F. ) ;
#17332 = CARTESIAN_POINT ( 'NONE',  ( 2.892866454678787531E-17, -1.149606299105070839, 0.1574803149606299191 ) ) ;
#17334 = CARTESIAN_POINT ( 'NONE',  ( -0.9873396505805591694, 0.1113553986120547346, 0.7135826770578268530 ) ) ;
#17335 = CARTESIAN_POINT ( 'NONE',  ( 0.8019270111902717657, -0.1787899950787401604, 1.899606299158834943 ) ) ;
#17336 = CARTESIAN_POINT ( 'NONE',  ( -0.9412147342319837628, 0.1574803149606300301, 1.395177165354331672 ) ) ;
#17337 = CARTESIAN_POINT ( 'NONE',  ( -0.8019270111902717657, 0.1787899950787401604, 0.9399606298674970661 ) ) ;
#17338 = CARTESIAN_POINT ( 'NONE',  ( 0.5555748031496123840, 1.332209862199691397, -0.06082000038405670217 ) ) ;
#17339 = CYLINDRICAL_SURFACE ( 'NONE', #42301, 0.1968503937007874127 ) ;
#17340 = CARTESIAN_POINT ( 'NONE',  ( 0.6971942568897626646, -0.07405724077823297447, 0.1673228345919059168 ) ) ;
#17341 = CARTESIAN_POINT ( 'NONE',  ( 0.7646288533564489232, 0.1113553986120547346, 1.628937007766488199 ) ) ;
#17342 = ORIENTED_EDGE ( 'NONE', *, *, #29606, .T. ) ;
#17343 = CARTESIAN_POINT ( 'NONE',  ( 0.1264236179284866091, 0.1274606299750234428, 0.1264236179284866091 ) ) ;
#17344 = CARTESIAN_POINT ( 'NONE',  ( 0.2559055118110236116, -0.1477471161312047254, -0.1122047244094488277 ) ) ;
#17345 = VERTEX_POINT ( 'NONE', #11567 ) ;
#17346 = CARTESIAN_POINT ( 'NONE',  ( 1.033464566929133799, 1.928577636452524610E-17, 4.498031496062992574 ) ) ;
#17347 = CARTESIAN_POINT ( 'NONE',  ( 0.6971942568897626646, -0.07405724077823297447, 0.7578740156942689321 ) ) ;
#17348 = CARTESIAN_POINT ( 'NONE',  ( -1.054774247047244540, 0.07405724077823318263, 1.638779527505292766 ) ) ;
#17349 = FACE_OUTER_BOUND ( 'NONE', #41906, .T. ) ;
#17350 = DIRECTION ( 'NONE',  ( 2.943801717310645197E-16, -1.000000000000000000, -2.197428715927220134E-15 ) ) ;
#17351 = CARTESIAN_POINT ( 'NONE',  ( -0.1787899950787401882, -1.197466487914277566, 0.000000000000000000 ) ) ;
#17352 = ORIENTED_EDGE ( 'NONE', *, *, #20386, .F. ) ;
#17353 = CARTESIAN_POINT ( 'NONE',  ( -0.1787899950787401604, -0.1161417322297011862, 0.07405724077823318263 ) ) ;
#17354 = EDGE_LOOP ( 'NONE', ( #20613, #7567, #39217, #45326 ) ) ;
#17355 = CARTESIAN_POINT ( 'NONE',  ( -0.8759842519685039353, -0.1574803149606299191, 1.210629921152315047 ) ) ;
#17356 = DIRECTION ( 'NONE',  ( 0.000000000000000000, 0.000000000000000000, 1.000000000000000000 ) ) ;
#17357 = AXIS2_PLACEMENT_3D ( 'NONE', #27332, #22989, #1644 ) ;
#17358 = CARTESIAN_POINT ( 'NONE',  ( 0.8759842519685039353, -0.1574803149606299191, 1.929133858267716661 ) ) ;
#17359 = ORIENTED_EDGE ( 'NONE', *, *, #33751, .F. ) ;
#17360 = EDGE_CURVE ( 'NONE', #29380, #36821, #33627, .T. ) ;
#17361 = CARTESIAN_POINT ( 'NONE',  ( -1.033464566929133799, 0.000000000000000000, 0.2066929133858267931 ) ) ;
#17362 = CARTESIAN_POINT ( 'NONE',  ( 0.7495606340400177148, -0.1264236179284866091, 1.464074803095842370 ) ) ;
#17363 = CARTESIAN_POINT ( 'NONE',  ( 0.8759842519685039353, 0.1787899950787401882, 0.1500984251430870220 ) ) ;
#17364 = DIRECTION ( 'NONE',  ( 8.659560562354332584E-17, 0.7071067811865965336, -0.7071067811864983899 ) ) ;
#17365 = ADVANCED_FACE ( 'NONE', ( #742 ), #33777, .F. ) ;
#17367 = CARTESIAN_POINT ( 'NONE',  ( -1.033464566929133799, 0.000000000000000000, 1.112204724409448842 ) ) ;
#17366 = CARTESIAN_POINT ( 'NONE',  ( 0.3690944881889784424, 0.1864803149606333310, -0.7480314960629921295 ) ) ;
#17368 = CARTESIAN_POINT ( 'NONE',  ( 0.9873396505805591694, 0.1113553986120547346, 0.6742125983176693316 ) ) ;
#17369 = CARTESIAN_POINT ( 'NONE',  ( -0.9873396505805591694, 0.1113553986120547346, 1.697834645561763889 ) ) ;
#17370 = CARTESIAN_POINT ( 'NONE',  ( 0.1787899950787401604, 0.02165354336085011100, -0.07405724077823318263 ) ) ;
#17371 = CARTESIAN_POINT ( 'NONE',  ( 1.002407869896990045, 0.1264236179284866091, 0.1058070865604098382 ) ) ;
#17372 = CYLINDRICAL_SURFACE ( 'NONE', #19973, 0.009842519685039274532 ) ;
#17374 = CARTESIAN_POINT ( 'NONE',  ( -0.7185039370078739607, 1.928577636452523993E-17, 1.830708661309795149 ) ) ;
#17373 = CARTESIAN_POINT ( 'NONE',  ( 1.054774247047244096, 0.000000000000000000, 1.163877952702141672 ) ) ;
#17375 = DIRECTION ( 'NONE',  ( -1.000000000000000000, 0.000000000000000000, 0.000000000000000000 ) ) ;
#17376 = CARTESIAN_POINT ( 'NONE',  ( 0.9873396505805591694, -0.1113553986120547346, 0.4675196849318432601 ) ) ;
#17377 = EDGE_LOOP ( 'NONE', ( #15518, #29698, #27038, #22237 ) ) ;
#17378 = CARTESIAN_POINT ( 'NONE',  ( 1.033121824622407647, 0.02587047616005715145, 0.03936947535289492955 ) ) ;
#17379 = CARTESIAN_POINT ( 'NONE',  ( -0.9412147342319837628, -0.1574803149606297803, 0.4650590550105836440 ) ) ;
#17380 = ORIENTED_EDGE ( 'NONE', *, *, #38350, .F. ) ;
#17381 = CARTESIAN_POINT ( 'NONE',  ( 1.054774247047244540, -0.07405724077823318263, 1.476377952702141449 ) ) ;
#17383 = CARTESIAN_POINT ( 'NONE',  ( -0.7185039370078746268, -0.06523048226347956391, 0.2189960628845991353 ) ) ;
#17382 = CARTESIAN_POINT ( 'NONE',  ( -1.033464566929133799, 0.000000000000000000, 0.9153543307086614567 ) ) ;
#17384 = CARTESIAN_POINT ( 'NONE',  ( 0.1787899950787401604, -0.09645669285962235606, -0.07405724077823318263 ) ) ;
#17385 = ORIENTED_EDGE ( 'NONE', *, *, #2963, .F. ) ;
#17386 = AXIS2_PLACEMENT_3D ( 'NONE', #14028, #9254, #44182 ) ;
#17387 = CARTESIAN_POINT ( 'NONE',  ( 0.1571284080983731402, -0.02678626661708362333, -0.1404155760989511115 ) ) ;
#17388 = ORIENTED_EDGE ( 'NONE', *, *, #21147, .F. ) ;
#17389 = CARTESIAN_POINT ( 'NONE',  ( 0.7185039370078739607, 1.928577636452523993E-17, 0.5019685039370078705 ) ) ;
#17390 = ORIENTED_EDGE ( 'NONE', *, *, #43700, .T. ) ;
#17391 = CARTESIAN_POINT ( 'NONE',  ( 0.6971942568897626646, -0.07405724077823297447, 0.3641732282926931630 ) ) ;
#17392 = VERTEX_POINT ( 'NONE', #19444 ) ;
#17393 = CARTESIAN_POINT ( 'NONE',  ( -0.9500414927467377701, -0.1787899950787401604, 1.353346456639149986 ) ) ;
#17394 = CARTESIAN_POINT ( 'NONE',  ( 0.07405724077823318263, -1.646653543253324026, 0.1787899950787401604 ) ) ;
#17395 = CARTESIAN_POINT ( 'NONE',  ( -0.8759842519685039353, 0.1787899950787401882, 0.9424212597887559051 ) ) ;
#17396 = CARTESIAN_POINT ( 'NONE',  ( -1.054774247047244540, -0.07405724077823318263, 1.948818897584033927 ) ) ;
#17397 = CARTESIAN_POINT ( 'NONE',  ( -0.8759842519685039353, 0.1787899950787401882, 1.094980314906866203 ) ) ;
#17398 = CARTESIAN_POINT ( 'NONE',  ( -1.002407869896990045, 0.1264236179284866091, 0.7012795275052913224 ) ) ;
#17399 = EDGE_CURVE ( 'NONE', #36803, #33940, #20152, .T. ) ;
#17400 = CARTESIAN_POINT ( 'NONE',  ( -0.2066929133858267931, 0.3171096708378827178, -3.631137952917390166 ) ) ;
#17401 = CARTESIAN_POINT ( 'NONE',  ( -0.1787899950787401604, -0.6831948343709717264, 0.07405724077823318263 ) ) ;
#17402 = ORIENTED_EDGE ( 'NONE', *, *, #36692, .T. ) ;
#17403 = CARTESIAN_POINT ( 'NONE',  ( -0.01513468283956021648, -0.08956185498306418191, 0.1527452548388714693 ) ) ;
#17404 = DIRECTION ( 'NONE',  ( 1.000000000000000000, 0.000000000000000000, -2.392722035830075028E-16 ) ) ;
#17406 = ORIENTED_EDGE ( 'NONE', *, *, #3376, .F. ) ;
#17405 = B_SPLINE_CURVE_WITH_KNOTS ( 'NONE', 3,
 ( #7059, #29156, #36772, #39873, #21686 ),
 .UNSPECIFIED., .F., .F.,
 ( 4, 1, 4 ),
 ( 0.000000000000000000, 0.002020725942163689639, 0.004041451884327379278 ),
 .UNSPECIFIED. ) ;
#17407 = ORIENTED_EDGE ( 'NONE', *, *, #35349, .T. ) ;
#17408 = CARTESIAN_POINT ( 'NONE',  ( -1.033464566929134687, -0.06523048226347956391, 0.3518700786326304231 ) ) ;
#17409 = CARTESIAN_POINT ( 'NONE',  ( -0.1574803149606299191, 1.174718201258053485, -3.430321324600322352 ) ) ;
#17410 = CARTESIAN_POINT ( 'NONE',  ( -0.7495606340400177148, -0.1264236179284866091, 0.5979330708123780092 ) ) ;
#17411 = LINE ( 'NONE', #16718, #31502 ) ;
#17412 = EDGE_LOOP ( 'NONE', ( #25328, #41077 ) ) ;
#17413 = DIRECTION ( 'NONE',  ( 0.000000000000000000, -1.000000000000000000, 0.000000000000000000 ) ) ;
#17414 = CARTESIAN_POINT ( 'NONE',  ( -1.002407869896990045, 0.1264236179284866091, 1.646161417269070837 ) ) ;
#17415 = DIRECTION ( 'NONE',  ( -0.000000000000000000, 1.000000000000000000, -0.000000000000000000 ) ) ;
#17416 = EDGE_CURVE ( 'NONE', #38075, #33479, #23350, .T. ) ;
#17417 = LINE ( 'NONE', #40156, #3458 ) ;
#17418 = ORIENTED_EDGE ( 'NONE', *, *, #17793, .F. ) ;
#17419 = CARTESIAN_POINT ( 'NONE',  ( 0.7185039370078746268, 0.06523048226347956391, 0.5782480314960627421 ) ) ;
#17420 = CARTESIAN_POINT ( 'NONE',  ( -0.07444174185955065859, -0.8991579828113921424, 0.1797182628040039087 ) ) ;
#17421 = DIRECTION ( 'NONE',  ( 0.000000000000000000, 0.000000000000000000, -1.000000000000000000 ) ) ;
#17422 = CARTESIAN_POINT ( 'NONE',  ( -0.7646288533564489232, 0.1113553986120547346, 1.353346456585388102 ) ) ;
#17423 = CARTESIAN_POINT ( 'NONE',  ( 0.7495606340400177148, -0.1264236179284866091, 0.6815944881352126172 ) ) ;
#17424 = CARTESIAN_POINT ( 'NONE',  ( -0.1113553986120547346, -0.5738188976377952555, 0.1113553986120547346 ) ) ;
#17425 = CARTESIAN_POINT ( 'NONE',  ( 0.8107537697050254399, 0.1574803149606300301, 1.626476377845228916 ) ) ;
#17426 = CARTESIAN_POINT ( 'NONE',  ( 0.000000000000000000, 1.205361022782826802E-17, -0.09842519685039370636 ) ) ;
#17427 = ADVANCED_FACE ( 'NONE', ( #1940 ), #16348, .T. ) ;
#17428 = CARTESIAN_POINT ( 'NONE',  ( 1.033464566929134687, -0.06523048226347956391, 1.267224409448818978 ) ) ;
#17429 = CARTESIAN_POINT ( 'NONE',  ( -9.642888182262618425E-18, 0.09055118120988918384, -0.1574803149606299191 ) ) ;
#17431 = ( LENGTH_UNIT ( ) NAMED_UNIT ( * ) SI_UNIT ( $, .METRE. ) ) ;
#17430 = CYLINDRICAL_SURFACE ( 'NONE', #39668, 0.09842519685039370636 ) ;
#17432 = FACE_OUTER_BOUND ( 'NONE', #19328, .T. ) ;
#17433 = CARTESIAN_POINT ( 'NONE',  ( -9.642888182262618425E-18, -0.6574803148531023211, -0.1574803149606299191 ) ) ;
#17434 = ( BOUNDED_CURVE ( )  B_SPLINE_CURVE ( 2, ( #20377, #39292, #32126, #35016, #24691, #38831, #46246, #17031, #31902 ),
 .UNSPECIFIED., .F., .T. ) 
 B_SPLINE_CURVE_WITH_KNOTS ( ( 3, 2, 2, 2, 3 ),
 ( 0.5899999999999999689, 0.5925000000000000266, 0.5949999999999999734, 0.5975000000000000311, 0.5999999999999999778 ),
 .UNSPECIFIED. ) 
 CURVE ( )  GEOMETRIC_REPRESENTATION_ITEM ( )  RATIONAL_B_SPLINE_CURVE ( ( 1.000000000000000000, 0.9238795325112869605, 1.000000000000000000, 0.9238795325112869605, 1.000000000000000000, 0.9238795325112869605, 1.000000000000000000, 0.9238795325112869605, 1.000000000000000000 ) ) 
 REPRESENTATION_ITEM ( '' )  ) ;
#17436 = DIRECTION ( 'NONE',  ( -1.000000000000000000, 0.000000000000000000, 0.000000000000000000 ) ) ;
#17435 = CARTESIAN_POINT ( 'NONE',  ( 0.6971942568897648851, -0.07405724077823297447, 0.7135826771115916234 ) ) ;
#17437 = CARTESIAN_POINT ( 'NONE',  ( -0.1264236179284866091, -0.6353346456155275490, -0.1264236179284866091 ) ) ;
#17438 = CARTESIAN_POINT ( 'NONE',  ( 0.03901279071809810040, 0.3740157480314960647, 1.057384721142220263 ) ) ;
#17439 = ORIENTED_EDGE ( 'NONE', *, *, #20241, .T. ) ;
#17440 = FACE_OUTER_BOUND ( 'NONE', #126, .T. ) ;
#17441 = CARTESIAN_POINT ( 'NONE',  ( 0.1618465483937462923, 0.06719994080174256090, -0.1405161193130588237 ) ) ;
#17442 = CARTESIAN_POINT ( 'NONE',  ( 0.8759842519685039353, 0.1787899950787401882, 0.8981299212060788184 ) ) ;
#17443 = DIRECTION ( 'NONE',  ( 0.000000000000000000, 0.000000000000000000, 1.000000000000000000 ) ) ;
#17444 = LINE ( 'NONE', #6414, #32749 ) ;
#17445 = CARTESIAN_POINT ( 'NONE',  ( -0.1797182628040039365, 0.03834201718860799635, 0.000000000000000000 ) ) ;
#17446 = CARTESIAN_POINT ( 'NONE',  ( 0.1787899950787401882, -1.088090551127338657, -2.189545951927503898E-17 ) ) ;
#17447 = CARTESIAN_POINT ( 'NONE',  ( -0.1574803149606299191, -1.523622047244094446, 0.000000000000000000 ) ) ;
#17448 = LINE ( 'NONE', #28749, #33706 ) ;
#17449 = AXIS2_PLACEMENT_3D ( 'NONE', #44992, #23692, #26830 ) ;
#17450 = CARTESIAN_POINT ( 'NONE',  ( -0.8019270111902717657, 0.1787899950787401604, 0.07381889758403178958 ) ) ;
#17451 = EDGE_LOOP ( 'NONE', ( #22452, #37391, #7447, #42501 ) ) ;
#17452 = CARTESIAN_POINT ( 'NONE',  ( 0.7495606340400177148, -0.1264236179284866091, 1.941437007820252081 ) ) ;
#17453 = ORIENTED_EDGE ( 'NONE', *, *, #14956, .T. ) ;
#17454 = CARTESIAN_POINT ( 'NONE',  ( -0.6971942568897637749, 2.189545951927499583E-17, 1.975885826717889815 ) ) ;
#17455 = CARTESIAN_POINT ( 'NONE',  ( -1.002407869896990045, -0.1264236179284866091, 1.040846456639149764 ) ) ;
#17456 = VECTOR ( 'NONE', #45783, 39.37007874015748143 ) ;
#17457 = CARTESIAN_POINT ( 'NONE',  ( -0.8759842519685039353, -0.1787899950787401882, 0.2140748030958428971 ) ) ;
#17458 = ( BOUNDED_CURVE ( )  B_SPLINE_CURVE ( 2, ( #15952, #12114, #34167, #16183, #37977, #8974, #19280, #811, #26501 ),
 .UNSPECIFIED., .F., .T. ) 
 B_SPLINE_CURVE_WITH_KNOTS ( ( 3, 2, 2, 2, 3 ),
 ( 0.2300000000000000100, 0.2325000000000000122, 0.2349999999999999867, 0.2374999999999999889, 0.2399999999999999911 ),
 .UNSPECIFIED. ) 
 CURVE ( )  GEOMETRIC_REPRESENTATION_ITEM ( )  RATIONAL_B_SPLINE_CURVE ( ( 1.000000000000000000, 0.9238795325112869605, 1.000000000000000000, 0.9238795325112869605, 1.000000000000000000, 0.9238795325112869605, 1.000000000000000000, 0.9238795325112869605, 1.000000000000000000 ) ) 
 REPRESENTATION_ITEM ( '' )  ) ;
#17459 = CARTESIAN_POINT ( 'NONE',  ( -0.7185039370078746268, -0.06523048226347956391, 0.6619094488188971281 ) ) ;
#17460 = CARTESIAN_POINT ( 'NONE',  ( -1.002407869896990045, 0.1264236179284866091, 1.961122047190330786 ) ) ;
#17461 = CARTESIAN_POINT ( 'NONE',  ( -0.7185039370078739607, 1.928577636452523993E-17, 1.879921259842519676 ) ) ;
#17462 = CARTESIAN_POINT ( 'NONE',  ( -0.1586641775163213364, 2.177585298233989164, -3.731703755406937439 ) ) ;
#17463 = CARTESIAN_POINT ( 'NONE',  ( 0.1787899950787401882, -0.3116397162607351112, -2.189545951927503898E-17 ) ) ;
#17464 = ITEM_DEFINED_TRANSFORMATION ( 'NONE', 'NONE', #19356,  #20860 ) ;
#17465 = LINE ( 'NONE', #32099, #14967 ) ;
#17466 = CARTESIAN_POINT ( 'NONE',  ( 0.000000000000000000, 0.1102362204724409434, 0.000000000000000000 ) ) ;
#17467 = CARTESIAN_POINT ( 'NONE',  ( -1.054774247047244096, 0.000000000000000000, 0.1402559054580474474 ) ) ;
#17468 = ORIENTED_EDGE ( 'NONE', *, *, #10842, .T. ) ;
#17469 = EDGE_CURVE ( 'NONE', #33274, #20413, #39872, .T. ) ;
#17470 = CARTESIAN_POINT ( 'NONE',  ( -1.054774247047244096, 0.000000000000000000, 1.286909448765133801 ) ) ;
#17471 = ORIENTED_EDGE ( 'NONE', *, *, #14530, .T. ) ;
#17472 = CARTESIAN_POINT ( 'NONE',  ( -1.094772975963752103E-17, -1.235728346402928945, -0.1787899950787401882 ) ) ;
#17473 = CARTESIAN_POINT ( 'NONE',  ( -0.07405724077823318263, -1.449803149552535642, 0.1787899950787401604 ) ) ;
#17474 = AXIS2_PLACEMENT_3D ( 'NONE', #15987, #1569, #30609 ) ;
#17475 = CARTESIAN_POINT ( 'NONE',  ( -0.1184675242425147629, -0.5708661417322835607, 1.713085361781126803 ) ) ;
#17476 = ( NAMED_UNIT ( * ) PLANE_ANGLE_UNIT ( ) SI_UNIT ( $, .RADIAN. ) ) ;
#17477 = CARTESIAN_POINT ( 'NONE',  ( 0.8759842519685039353, -0.1574803149606299191, 0.3149606299212598381 ) ) ;
#17478 = CARTESIAN_POINT ( 'NONE',  ( 0.1270800023317771588, -0.4587052269058803367, 0.1270800023317771588 ) ) ;
#17479 = DIRECTION ( 'NONE',  ( 0.000000000000000000, 0.000000000000000000, -1.000000000000000000 ) ) ;
#17480 = CARTESIAN_POINT ( 'NONE',  ( -0.7185039370078746268, 0.06523048226347956391, 0.7357283464566919395 ) ) ;
#17481 = CARTESIAN_POINT ( 'NONE',  ( -0.1574803149606297803, -0.1825787401574804625, 0.06523048226347956391 ) ) ;
#17482 = CARTESIAN_POINT ( 'NONE',  ( 0.9412147342319837628, -0.1574803149606297803, 1.764271653435779630 ) ) ;
#17483 = ORIENTED_EDGE ( 'NONE', *, *, #18969, .T. ) ;
#17484 = CARTESIAN_POINT ( 'NONE',  ( 0.8107537697050234415, -0.1574803149606297803, 0.2239173227271187561 ) ) ;
#17485 = CARTESIAN_POINT ( 'NONE',  ( 1.033464566929133799, 0.000000000000000000, 0.7578740157480314821 ) ) ;
#17487 = CARTESIAN_POINT ( 'NONE',  ( 0.03889724126169821078, -0.2730368995492337691, -0.06846571731931765104 ) ) ;
#17486 = CIRCLE ( 'NONE', #38911, 0.09842519685039370636 ) ;
#17488 = CARTESIAN_POINT ( 'NONE',  ( -0.4240551181102362177, 0.2559055118110236116, 0.000000000000000000 ) ) ;
#17489 = EDGE_CURVE ( 'NONE', #15059, #1067, #838, .T. ) ;
#17491 = CARTESIAN_POINT ( 'NONE',  ( -0.8759842519685039353, 0.000000000000000000, 0.000000000000000000 ) ) ;
#17490 = CARTESIAN_POINT ( 'NONE',  ( -0.9873396505805591694, -0.1113553986120547346, 0.4773622047244094890 ) ) ;
#17492 = CARTESIAN_POINT ( 'NONE',  ( 1.033464566929133799, 0.000000000000000000, 0.2362204723334177248 ) ) ;
#17493 = VERTEX_POINT ( 'NONE', #41701 ) ;
#17494 = CARTESIAN_POINT ( 'NONE',  ( 0.000000000000000000, 0.000000000000000000, -0.02633646578327370619 ) ) ;
#17495 = CARTESIAN_POINT ( 'NONE',  ( -0.7330379983016587220, 0.1099100077093767003, 0.03937007874015843040 ) ) ;
#17496 = CARTESIAN_POINT ( 'NONE',  ( -0.1264236179284866091, -0.5221456692375747721, -0.1264236179284866091 ) ) ;
#17497 = CARTESIAN_POINT ( 'NONE',  ( -0.1574803149606297803, -1.009350393700786608, 0.06523048226347956391 ) ) ;
#17498 = CARTESIAN_POINT ( 'NONE',  ( 0.7185039370078746268, 0.06523048226347956391, 0.8833661416247557963 ) ) ;
#17499 = CARTESIAN_POINT ( 'NONE',  ( 0.4151545546392377273, 0.09842519685039370636, 0.000000000000000000 ) ) ;
#17500 = CARTESIAN_POINT ( 'NONE',  ( -0.6971942568897637749, 2.189545951927499583E-17, 0.3567913385289137596 ) ) ;
#17501 = ORIENTED_EDGE ( 'NONE', *, *, #26383, .T. ) ;
#17502 = EDGE_LOOP ( 'NONE', ( #26926, #27649, #41815 ) ) ;
#17503 = CARTESIAN_POINT ( 'NONE',  ( -1.002407869896990045, 0.1264236179284866091, 1.409940944828126153 ) ) ;
#17504 = CARTESIAN_POINT ( 'NONE',  ( 0.8019270111902717657, 0.1787899950787401604, 1.574803149552536530 ) ) ;
#17505 = CARTESIAN_POINT ( 'NONE',  ( -0.8107537697050254399, -0.1574803149606297803, 0.9030511811023625990 ) ) ;
#17506 = CARTESIAN_POINT ( 'NONE',  ( 2.892866454678787531E-17, -1.267716535325543070, 0.1574803149606299191 ) ) ;
#17507 = CARTESIAN_POINT ( 'NONE',  ( -0.6971942568897626646, -0.07405724077823297447, 0.6397637794737947026 ) ) ;
#17508 = CARTESIAN_POINT ( 'NONE',  ( -0.8759842519685039353, -0.1574803149606299191, 1.683070866034204638 ) ) ;
#17509 = CARTESIAN_POINT ( 'NONE',  ( 0.6971942568897637749, 2.189545951927499583E-17, 0.7160433070328504623 ) ) ;
#17510 = CARTESIAN_POINT ( 'NONE',  ( -0.6971942568897637749, 2.189545951927499583E-17, 0.6717519684501732646 ) ) ;
#17511 = CARTESIAN_POINT ( 'NONE',  ( 0.1925175471591499543, -0.07678538764768121083, 0.1742829424377221881 ) ) ;
#17512 = CARTESIAN_POINT ( 'NONE',  ( 0.8107537697050254399, 0.1574803149606300301, 1.075295275483024726 ) ) ;
#17513 = CARTESIAN_POINT ( 'NONE',  ( -0.1113553986120547346, -0.1407480313885360323, -0.1113553986120547346 ) ) ;
#17514 = CARTESIAN_POINT ( 'NONE',  ( -1.002407869896990045, 0.1264236179284866091, 1.370570866087968520 ) ) ;
#17515 = DIRECTION ( 'NONE',  ( 0.000000000000000000, 0.000000000000000000, 1.000000000000000000 ) ) ;
#17516 = CARTESIAN_POINT ( 'NONE',  ( -0.7646288533564489232, 0.1113553986120547346, 0.4970472440944882497 ) ) ;
#17517 = CARTESIAN_POINT ( 'NONE',  ( 0.6971942568897648851, 0.07405724077823318263, 1.264763779473795813 ) ) ;
#17518 = CARTESIAN_POINT ( 'NONE',  ( -0.1490661257827161357, -0.09851383790554034403, -0.1002053949427159502 ) ) ;
#17519 = ORIENTED_EDGE ( 'NONE', *, *, #46159, .F. ) ;
#17520 = EDGE_CURVE ( 'NONE', #14480, #8597, #21522, .T. ) ;
#17521 = CARTESIAN_POINT ( 'NONE',  ( 0.2395294000716134131, 3.218313930830148909E-16, -0.8759842519685039353 ) ) ;
#17522 = AXIS2_PLACEMENT_3D ( 'NONE', #14824, #40655, #25385 ) ;
#17523 = ADVANCED_FACE ( 'NONE', ( #12759 ), #12526, .T. ) ;
#17524 = VERTEX_POINT ( 'NONE', #34547 ) ;
#17525 = CARTESIAN_POINT ( 'NONE',  ( -0.07405724077823318263, -0.6771653542769455747, -0.1787899950787401604 ) ) ;
#17526 = AXIS2_PLACEMENT_3D ( 'NONE', #21095, #35733, #2176 ) ;
#17527 = ADVANCED_FACE ( 'NONE', ( #1698 ), #30969, .T. ) ;
#17528 = CARTESIAN_POINT ( 'NONE',  ( 0.9873396505805591694, -0.1113553986120547346, 0.3986220472440945017 ) ) ;
#17529 = ORIENTED_EDGE ( 'NONE', *, *, #3692, .F. ) ;
#17530 = CARTESIAN_POINT ( 'NONE',  ( 1.054774247047244096, 0.000000000000000000, 1.439468503883244210 ) ) ;
#17531 = DIRECTION ( 'NONE',  ( -1.000000000000000000, 0.000000000000000000, 0.000000000000000000 ) ) ;
#17532 = CARTESIAN_POINT ( 'NONE',  ( 0.1264236179284866091, -0.3056102361667090705, 0.1264236179284866091 ) ) ;
#17533 = CARTESIAN_POINT ( 'NONE',  ( 0.4736248074375464800, 1.798092712879862276, -3.826876940038421715 ) ) ;
#17534 = CARTESIAN_POINT ( 'NONE',  ( -0.1279527559055118058, -0.2216206741968047289, -0.3149606299212598381 ) ) ;
#17535 = CARTESIAN_POINT ( 'NONE',  ( 0.6971942568897648851, 0.07405724077823318263, 1.692913385773008539 ) ) ;
#17536 = CARTESIAN_POINT ( 'NONE',  ( 1.054774247047244540, -0.07405724077823318263, 0.2559055117572600624 ) ) ;
#17537 = CARTESIAN_POINT ( 'NONE',  ( -0.1264236179284866091, 0.02792721287312346923, 0.1264236179284866091 ) ) ;
#17538 = CARTESIAN_POINT ( 'NONE',  ( -0.1787899950787401604, -0.2391732282926934683, -0.07405724077823318263 ) ) ;
#17539 = CARTESIAN_POINT ( 'NONE',  ( 0.2559055118110236116, 0.000000000000000000, -0.3149606299212598381 ) ) ;
#17540 = CARTESIAN_POINT ( 'NONE',  ( -0.7185039370078739607, 1.928577636452523993E-17, 1.683070866141732402 ) ) ;
#17541 = CARTESIAN_POINT ( 'NONE',  ( 1.054774247047244540, -0.07405724077823318263, 0.5708661416785201226 ) ) ;
#17542 = CARTESIAN_POINT ( 'NONE',  ( -0.7495606340400177148, -0.1264236179284866091, 0.9571850393163149340 ) ) ;
#17543 = CIRCLE ( 'NONE', #38983, 0.3912448816427701037 ) ;
#17545 = FACE_OUTER_BOUND ( 'NONE', #37967, .T. ) ;
#17544 = CARTESIAN_POINT ( 'NONE',  ( -0.06523048226347956391, -0.8469488188976374010, 0.1574803149606297803 ) ) ;
#17546 = CARTESIAN_POINT ( 'NONE',  ( -1.100456976456230270E-17, -1.664413888323202695, -0.1797182628040039365 ) ) ;
#17547 = FACE_OUTER_BOUND ( 'NONE', #3851, .T. ) ;
#17548 = CARTESIAN_POINT ( 'NONE',  ( 1.002407869896990045, 0.1264236179284866091, 1.606791338528913426 ) ) ;
#17550 = CARTESIAN_POINT ( 'NONE',  ( 0.000000000000000000, 0.000000000000000000, 0.2952755905511810774 ) ) ;
#17549 = CARTESIAN_POINT ( 'NONE',  ( 0.1631888523360092158, 0.09129006187719292120, -0.1912159430412007366 ) ) ;
#17551 = EDGE_LOOP ( 'NONE', ( #35799, #16087 ) ) ;
#17552 = DIRECTION ( 'NONE',  ( 0.000000000000000000, 0.000000000000000000, -1.000000000000000000 ) ) ;
#17553 = CARTESIAN_POINT ( 'NONE',  ( 0.8107537697050253289, 0.1574803149606300301, 0.02214566929133862661 ) ) ;
#17554 = CARTESIAN_POINT ( 'NONE',  ( 0.3302522695077432791, 4.466152701071653354E-17, 0.000000000000000000 ) ) ;
#17555 = CARTESIAN_POINT ( 'NONE',  ( -0.1787899950787401604, -0.1604330708123782034, 0.07405724077823318263 ) ) ;
#17556 = CIRCLE ( 'NONE', #31334, 0.04921259842519688094 ) ;
#17557 = CARTESIAN_POINT ( 'NONE',  ( 0.1787899950787401604, -1.085629921206079374, 0.07405724077823318263 ) ) ;
#17558 = CARTESIAN_POINT ( 'NONE',  ( 0.6971942568897626646, -0.07405724077823297447, 0.08858267711159097113 ) ) ;
#17559 = FACE_BOUND ( 'NONE', #37076, .T. ) ;
#17560 = CARTESIAN_POINT ( 'NONE',  ( 0.6971942568897637749, 2.189545951927499583E-17, 0.5536417322297008115 ) ) ;
#17561 = CARTESIAN_POINT ( 'NONE',  ( -0.1377952755905510751, 1.687505431895958263E-17, -0.02633646578327370619 ) ) ;
#17562 = CARTESIAN_POINT ( 'NONE',  ( -0.6971942568897637749, 2.189545951927499583E-17, 1.419783464513165505 ) ) ;
#17563 = ORIENTED_EDGE ( 'NONE', *, *, #38952, .F. ) ;
#17564 = LINE ( 'NONE', #31731, #29951 ) ;
#17565 = CARTESIAN_POINT ( 'NONE',  ( 0.6971942568897637749, 2.189545951927499583E-17, 1.188484251914740275 ) ) ;
#17566 = CARTESIAN_POINT ( 'NONE',  ( -0.8759842519685039353, 0.1574803149606299191, 0.6791338581601890079 ) ) ;
#17567 = CARTESIAN_POINT ( 'NONE',  ( 0.9500414927467378812, 0.1787899950787401604, 1.840551181048599938 ) ) ;
#17568 = CARTESIAN_POINT ( 'NONE',  ( -1.033464566929133799, 0.000000000000000000, 1.348425196850393748 ) ) ;
#17569 = CARTESIAN_POINT ( 'NONE',  ( -0.8019270111902717657, -0.1787899950787401604, 0.9547244093950547628 ) ) ;
#17570 = CARTESIAN_POINT ( 'NONE',  ( 0.1377952755905510196, 1.687505431895957030E-17, -0.1828167807439035619 ) ) ;
#17571 = DIRECTION ( 'NONE',  ( -1.000000000000000000, 0.000000000000000000, 0.000000000000000000 ) ) ;
#17572 = CARTESIAN_POINT ( 'NONE',  ( 0.9500414927467377701, 0.1787899950787401604, 0.2312992125446618197 ) ) ;
#17573 = CARTESIAN_POINT ( 'NONE',  ( -0.8019270111902716547, 0.1787899950787401604, 0.1131889763241894220 ) ) ;
#17574 = CARTESIAN_POINT ( 'NONE',  ( -1.002407869896990045, 0.1264236179284866091, 0.5388779527021417826 ) ) ;
#17575 = CARTESIAN_POINT ( 'NONE',  ( 0.7185039370078746268, -0.06523048226347956391, 1.518208661309795149 ) ) ;
#17576 = ORIENTED_EDGE ( 'NONE', *, *, #6034, .T. ) ;
#17577 = ( BOUNDED_CURVE ( )  B_SPLINE_CURVE ( 2, ( #30885, #23908, #23197, #41597, #45445, #4965, #12667, #12428, #27292 ),
 .UNSPECIFIED., .F., .T. ) 
 B_SPLINE_CURVE_WITH_KNOTS ( ( 3, 2, 2, 2, 3 ),
 ( 0.2300000000000000100, 0.2325000000000000122, 0.2349999999999999867, 0.2374999999999999889, 0.2399999999999999911 ),
 .UNSPECIFIED. ) 
 CURVE ( )  GEOMETRIC_REPRESENTATION_ITEM ( )  RATIONAL_B_SPLINE_CURVE ( ( 1.000000000000000000, 0.9238795325112869605, 1.000000000000000000, 0.9238795325112869605, 1.000000000000000000, 0.9238795325112869605, 1.000000000000000000, 0.9238795325112869605, 1.000000000000000000 ) ) 
 REPRESENTATION_ITEM ( '' )  ) ;
#17578 = CARTESIAN_POINT ( 'NONE',  ( -0.1264236179284866091, -0.07923228341080333637, 0.1264236179284866091 ) ) ;
#17579 = CARTESIAN_POINT ( 'NONE',  ( 0.9873396505805591694, 0.1113553986120547346, 1.776574803042078488 ) ) ;
#17580 = CARTESIAN_POINT ( 'NONE',  ( 0.8759842519685039353, 0.1787899950787401882, 0.8243110235682834519 ) ) ;
#17581 = CARTESIAN_POINT ( 'NONE',  ( -0.7495606340400177148, -0.1264236179284866091, 1.739665354276945131 ) ) ;
#17582 = EDGE_CURVE ( 'NONE', #31513, #27525, #31896, .T. ) ;
#17583 = EDGE_CURVE ( 'NONE', #26517, #17013, #43685, .T. ) ;
#17584 = CARTESIAN_POINT ( 'NONE',  ( -0.2471922904502827922, 0.06732389326667123641, -0.09794877975412334681 ) ) ;
#17585 = AXIS2_PLACEMENT_3D ( 'NONE', #34086, #26658, #11800 ) ;
#17586 = CYLINDRICAL_SURFACE ( 'NONE', #37433, 0.1377952755905512694 ) ;
#17587 = CARTESIAN_POINT ( 'NONE',  ( -1.094772975963752103E-17, -1.286049165079631962, -0.1787899950787401882 ) ) ;
#17588 = ORIENTED_EDGE ( 'NONE', *, *, #13812, .F. ) ;
#17589 = CARTESIAN_POINT ( 'NONE',  ( 0.07405724077823318263, -0.06692913380450424277, 0.1787899950787401604 ) ) ;
#17590 = EDGE_CURVE ( 'NONE', #1000, #37016, #25158, .T. ) ;
#17591 = ORIENTED_EDGE ( 'NONE', *, *, #26379, .F. ) ;
#17592 = CARTESIAN_POINT ( 'NONE',  ( 0.7495606340400177148, -0.1264236179284866091, 1.109744094434425232 ) ) ;
#17593 = EDGE_CURVE ( 'NONE', #42069, #10600, #26409, .T. ) ;
#17594 = AXIS2_PLACEMENT_3D ( 'NONE', #7967, #4344, #19221 ) ;
#17595 = CARTESIAN_POINT ( 'NONE',  ( -0.2471920270788468266, -0.07566776403313510424, 0.08167830084061132589 ) ) ;
#17596 = CARTESIAN_POINT ( 'NONE',  ( 0.9500414927467378812, 0.1787899950787401604, 0.06889763774151215492 ) ) ;
#17597 = CARTESIAN_POINT ( 'NONE',  ( -0.07405724077823318263, -1.494094488135213394, 0.1787899950787401604 ) ) ;
#17598 = CARTESIAN_POINT ( 'NONE',  ( -1.094772975963752103E-17, -0.7239173227808818334, -0.1787899950787401882 ) ) ;
#17599 = CARTESIAN_POINT ( 'NONE',  ( -0.7495606340400177148, -0.1264236179284866091, 0.4847440944344252323 ) ) ;
#17600 = CARTESIAN_POINT ( 'NONE',  ( -0.7124824329870323991, -0.03455856718743761241, 1.983908545787091082 ) ) ;
#17601 = CARTESIAN_POINT ( 'NONE',  ( -0.09631076833422043404, 0.2398891842387853301, -0.03294411891277443383 ) ) ;
#17602 = CARTESIAN_POINT ( 'NONE',  ( 0.7495606340400177148, 0.1264236179284866091, 1.532972440891118060 ) ) ;
#17603 = CARTESIAN_POINT ( 'NONE',  ( 0.8759842519685039353, 0.1574803149606299191, 1.673228346456693050 ) ) ;
#17604 = DIRECTION ( 'NONE',  ( -1.020425574104001164E-16, 1.020425574104001164E-16, -1.000000000000000000 ) ) ;
#17606 = CARTESIAN_POINT ( 'NONE',  ( -0.8759842491179902213, 0.1574803149606299191, 1.978346456692913646 ) ) ;
#17605 = CARTESIAN_POINT ( 'NONE',  ( 2.700008691033534577E-17, 0.1102362204724409434, 0.2204724409448818867 ) ) ;
#17607 = DIRECTION ( 'NONE',  ( 0.000000000000000000, -8.240357684727058740E-16, 1.000000000000000000 ) ) ;
#17608 = CARTESIAN_POINT ( 'NONE',  ( 0.1574803149606300301, -0.7878937006798749643, 0.06523048226347956391 ) ) ;
#17609 = CARTESIAN_POINT ( 'NONE',  ( -1.033464566929134687, 0.06523048226347956391, 1.774114173120818316 ) ) ;
#17610 = CARTESIAN_POINT ( 'NONE',  ( 0.07405724077823318263, -0.01279527553678768380, -0.1787899950787401604 ) ) ;
#17611 = CARTESIAN_POINT ( 'NONE',  ( 0.7495606340400177148, 0.1264236179284866091, 0.1943897637257641919 ) ) ;
#17612 = CARTESIAN_POINT ( 'NONE',  ( 0.7032143776996268025, -0.01662162624712908501, 0.03937554043527696085 ) ) ;
#17614 = CARTESIAN_POINT ( 'NONE',  ( -0.9412147342319837628, 0.1574803149606300301, 1.818405511703497845 ) ) ;
#17613 = CARTESIAN_POINT ( 'NONE',  ( 1.002407869896990045, -0.1264236179284866091, 1.198326771599779628 ) ) ;
#17615 = CARTESIAN_POINT ( 'NONE',  ( 0.9873396505805591694, -0.1113553986120547346, 0.5462598424121581919 ) ) ;
#17616 = ORIENTED_EDGE ( 'NONE', *, *, #29850, .F. ) ;
#17617 = CARTESIAN_POINT ( 'NONE',  ( -1.054774247047244540, -0.07405724077823318263, 1.048228346402930944 ) ) ;
#17618 = LINE ( 'NONE', #39642, #36035 ) ;
#17619 = CARTESIAN_POINT ( 'NONE',  ( 0.8940612688331117663, 0.1724986514511060165, 0.03937022261624964492 ) ) ;
#17620 = CARTESIAN_POINT ( 'NONE',  ( -0.7185039370078739607, 1.928577636452523993E-17, 0.4527559054042842868 ) ) ;
#17621 = AXIS2_PLACEMENT_3D ( 'NONE', #28129, #675, #22744 ) ;
#17622 = CARTESIAN_POINT ( 'NONE',  ( 1.054774247047244540, 0.07405724077823318263, 1.520669291284818758 ) ) ;
#17624 = CARTESIAN_POINT ( 'NONE',  ( -0.8107537697050254399, 0.1574803149606300301, 0.2878937006798746312 ) ) ;
#17623 = CARTESIAN_POINT ( 'NONE',  ( -0.7185039370078746268, 0.06523048226347977208, 0.1058070866141732902 ) ) ;
#17625 = DIMENSIONAL_EXPONENTS ( 1.000000000000000000, 0.000000000000000000, 0.000000000000000000, 0.000000000000000000, 0.000000000000000000, 0.000000000000000000, 0.000000000000000000 ) ;
#17627 = CIRCLE ( 'NONE', #46690, 0.2362204724409449064 ) ;
#17626 = CARTESIAN_POINT ( 'NONE',  ( 0.1787899950787401882, -0.05954724404072461036, -2.189545951927503898E-17 ) ) ;
#17628 = ORIENTED_EDGE ( 'NONE', *, *, #46027, .T. ) ;
#17629 = CARTESIAN_POINT ( 'NONE',  ( 0.7646288533564489232, 0.1113553986120547346, 0.4478346455617645550 ) ) ;
#17630 = ORIENTED_EDGE ( 'NONE', *, *, #24843, .T. ) ;
#17631 = CARTESIAN_POINT ( 'NONE',  ( 0.7185039370078766252, -0.06523048226348168721, 1.281988188868851353 ) ) ;
#17632 = CARTESIAN_POINT ( 'NONE',  ( 1.033464566929133799, 0.000000000000000000, 1.112204724409448842 ) ) ;
#17633 = CARTESIAN_POINT ( 'NONE',  ( 0.6971942568897626646, -0.07405724077823297447, 0.6397637794737947026 ) ) ;
#17634 = ORIENTED_EDGE ( 'NONE', *, *, #20766, .T. ) ;
#17635 = CARTESIAN_POINT ( 'NONE',  ( -1.002407869896990045, -0.1264236179284866091, 1.355807086560409491 ) ) ;
#17636 = CARTESIAN_POINT ( 'NONE',  ( -0.1787899950787401604, -1.735236220418678643, 0.07405724077823318263 ) ) ;
#17637 = CARTESIAN_POINT ( 'NONE',  ( -0.8019270111902717657, 0.1787899950787401604, 1.062992125930488418 ) ) ;
#17638 = CARTESIAN_POINT ( 'NONE',  ( -0.9412147342319837628, 0.1574803149606300301, 0.09596456692913378494 ) ) ;
#17639 = CARTESIAN_POINT ( 'NONE',  ( -1.002407869896990045, -0.1264236179284866091, 1.119586614119464585 ) ) ;
#17640 = CARTESIAN_POINT ( 'NONE',  ( -0.6971942568897637749, 2.189545951927499583E-17, 0.8341535432533228045 ) ) ;
#17641 = EDGE_CURVE ( 'NONE', #44955, #15275, #40738, .T. ) ;
#17642 = CARTESIAN_POINT ( 'NONE',  ( -1.002407869896990045, 0.1264236179284866091, 0.1894685038832444879 ) ) ;
#17643 = CARTESIAN_POINT ( 'NONE',  ( 0.2698848154395015464, 0.09842519685039370636, 1.205361022782828805E-17 ) ) ;
#17644 = CARTESIAN_POINT ( 'NONE',  ( 0.000000000000000000, 0.09842519685039370636, 0.000000000000000000 ) ) ;
#17645 = CARTESIAN_POINT ( 'NONE',  ( 0.1264236179284866091, -0.8578995587804193468, -0.1264236179284866091 ) ) ;
#17646 = ORIENTED_EDGE ( 'NONE', *, *, #36036, .F. ) ;
#17647 = CARTESIAN_POINT ( 'NONE',  ( -0.1429330575240212731, -0.08956165177108092734, 0.08068231488144075869 ) ) ;
#17648 = CARTESIAN_POINT ( 'NONE',  ( -0.8070866141732283561, 0.000000000000000000, 0.8559055118110230342 ) ) ;
#17649 = ORIENTED_EDGE ( 'NONE', *, *, #38353, .T. ) ;
#17650 = CARTESIAN_POINT ( 'NONE',  ( 1.033464566929134687, 0.06523048226347956391, 0.7603346456692923194 ) ) ;
#17651 = ADVANCED_FACE ( 'NONE', ( #8887 ), #15420, .T. ) ;
#17652 = CARTESIAN_POINT ( 'NONE',  ( -1.002407869896990045, 0.1264236179284866091, 0.5782480314422993040 ) ) ;
#17653 = CARTESIAN_POINT ( 'NONE',  ( 0.8107537697050254399, 0.1574803149606300301, 1.350885826664126821 ) ) ;
#17654 = ORIENTED_EDGE ( 'NONE', *, *, #5795, .F. ) ;
#17655 = CARTESIAN_POINT ( 'NONE',  ( -0.9500414927467377701, -0.1787899950787401604, 1.751968503883245987 ) ) ;
#17656 = VECTOR ( 'NONE', #33472, 39.37007874015748143 ) ;
#17657 = CARTESIAN_POINT ( 'NONE',  ( 0.000000000000000000, 0.000000000000000000, -0.1377952755905511861 ) ) ;
#17658 = CARTESIAN_POINT ( 'NONE',  ( -0.9873396505805591694, -0.1113553986120547346, 0.1919291337507405548 ) ) ;
#17659 = CARTESIAN_POINT ( 'NONE',  ( 0.1270800023317771588, -0.7736658568271397307, 0.1270800023317771588 ) ) ;
#17660 = CARTESIAN_POINT ( 'NONE',  ( 0.2471922904502826257, 0.08342621139837362587, 0.06611980121264769694 ) ) ;
#17661 = CARTESIAN_POINT ( 'NONE',  ( -0.9873396505805591694, -0.1113553986120547346, 1.412401574695621997 ) ) ;
#17662 = CARTESIAN_POINT ( 'NONE',  ( 0.8759842519685039353, -0.1787899950787401882, 0.8439960629383622681 ) ) ;
#17663 = CARTESIAN_POINT ( 'NONE',  ( 0.1574803149606300301, -0.5959645669291335768, -0.06523048226347956391 ) ) ;
#17664 = CARTESIAN_POINT ( 'NONE',  ( -0.1596048934580996670, 0.1255079988737376195, -0.03370813687491143462 ) ) ;
#17665 = ORIENTED_EDGE ( 'NONE', *, *, #5461, .F. ) ;
#17666 = CARTESIAN_POINT ( 'NONE',  ( 0.7646288533564489232, 0.1113553986120547346, 0.1722440943806619884 ) ) ;
#17667 = CARTESIAN_POINT ( 'NONE',  ( 0.9873396505805591694, -0.1113553986120547346, 1.304133858267716661 ) ) ;
#17669 = CARTESIAN_POINT ( 'NONE',  ( -0.1377952755905511861, 0.1574803149606320007, 0.8070866141732283561 ) ) ;
#17668 = CARTESIAN_POINT ( 'NONE',  ( 0.8151215678306394929, -0.1614990644632125771, 1.987062530839091901 ) ) ;
#17670 = CARTESIAN_POINT ( 'NONE',  ( -0.3980944881889745268, 0.6449983665207583705, -0.7480314960629921295 ) ) ;
#17672 = DIRECTION ( 'NONE',  ( 0.000000000000000000, 0.000000000000000000, 1.000000000000000000 ) ) ;
#17671 = CARTESIAN_POINT ( 'NONE',  ( 0.6971942568897637749, 2.189545951927499583E-17, 0.5930118109698583329 ) ) ;
#17673 = ORIENTED_EDGE ( 'NONE', *, *, #27123, .T. ) ;
#17674 = LINE ( 'NONE', #14567, #33737 ) ;
#17675 = DIRECTION ( 'NONE',  ( 0.000000000000000000, 0.000000000000000000, 1.000000000000000000 ) ) ;
#17676 = CARTESIAN_POINT ( 'NONE',  ( 0.8759842519685039353, -0.1787899950787401882, 0.9178149605761574126 ) ) ;
#17677 = CARTESIAN_POINT ( 'NONE',  ( 0.8107537697050254399, 0.1574803149606300301, 1.478838582677165059 ) ) ;
#17678 = CARTESIAN_POINT ( 'NONE',  ( 0.9873396505805591694, -0.1113553986120547346, 0.7037401573727875004 ) ) ;
#17679 = CARTESIAN_POINT ( 'NONE',  ( -0.1270800023317771588, 0.03342075734608830617, -0.1270800023317771588 ) ) ;
#17680 = CARTESIAN_POINT ( 'NONE',  ( -0.1787899950787401604, -1.070866141678519456, -0.07405724077823318263 ) ) ;
#17681 = CARTESIAN_POINT ( 'NONE',  ( 0.1113553986120547346, -1.499015748031496065, -0.1113553986120547346 ) ) ;
#17682 = FACE_OUTER_BOUND ( 'NONE', #33318, .T. ) ;
#17683 = AXIS2_PLACEMENT_3D ( 'NONE', #25649, #12150, #40224 ) ;
#17684 = CARTESIAN_POINT ( 'NONE',  ( -0.7495606340400177148, 0.1264236179284866091, 0.03690944876513417572 ) ) ;
#17685 = EDGE_LOOP ( 'NONE', ( #16562, #35863, #14651, #32540 ) ) ;
#17686 = CARTESIAN_POINT ( 'NONE',  ( 0.9500414927467378812, -0.1787899950787401604, 1.948818897584033927 ) ) ;
#17687 = ORIENTED_EDGE ( 'NONE', *, *, #29207, .F. ) ;
#17688 = CARTESIAN_POINT ( 'NONE',  ( -0.7495606340400177148, 0.1264236179284866091, 1.970964566875370139 ) ) ;
#17689 = AXIS2_PLACEMENT_3D ( 'NONE', #38464, #17356, #31531 ) ;
#17690 = AXIS2_PLACEMENT_3D ( 'NONE', #5659, #5896, #23413 ) ;
#17691 = CARTESIAN_POINT ( 'NONE',  ( -0.8019270111902717657, -0.1787899950787401604, 1.545275590497416696 ) ) ;
#17692 = CARTESIAN_POINT ( 'NONE',  ( 0.6971942568897648851, 0.07405724077823318263, 0.8710629920722218200 ) ) ;
#17693 = CARTESIAN_POINT ( 'NONE',  ( -0.6971942568897648851, 0.07405724077823318263, 0.8267716534895444003 ) ) ;
#17694 = VECTOR ( 'NONE', #9069, 39.37007874015748854 ) ;
#17695 = CARTESIAN_POINT ( 'NONE',  ( -0.6971942568897626646, -0.07405724077823297447, 0.3641732282926931630 ) ) ;
#17696 = EDGE_CURVE ( 'NONE', #15659, #46267, #22790, .T. ) ;
#17697 = CARTESIAN_POINT ( 'NONE',  ( -0.9412147342319837628, -0.1574803149606297803, 0.6717519685039375910 ) ) ;
#17698 = CARTESIAN_POINT ( 'NONE',  ( -0.7495606340400177148, -0.1264236179284866091, 1.941437007820252081 ) ) ;
#17699 = CARTESIAN_POINT ( 'NONE',  ( -0.9873396505805591694, 0.1113553986120547346, 1.471456692913385877 ) ) ;
#17700 = CARTESIAN_POINT ( 'NONE',  ( -1.033464566929134687, 0.06523048226347956391, 1.941437007874014187 ) ) ;
#17701 = CARTESIAN_POINT ( 'NONE',  ( 0.2559054503028028726, 0.07924707884460499563, -0.05308369988359751268 ) ) ;
#17702 = CARTESIAN_POINT ( 'NONE',  ( -0.1787899950787401882, -0.2919546768906559064, 0.000000000000000000 ) ) ;
#17703 = LINE ( 'NONE', #10777, #4984 ) ;
#17704 = DIRECTION ( 'NONE',  ( 0.000000000000000000, 1.000000000000000000, 0.000000000000000000 ) ) ;
#17705 = CARTESIAN_POINT ( 'NONE',  ( -0.7495606340400177148, -0.1264236179284866091, 0.08612204719033110523 ) ) ;
#17706 = ORIENTED_EDGE ( 'NONE', *, *, #1541, .T. ) ;
#17707 = CARTESIAN_POINT ( 'NONE',  ( -1.002407869896990045, -0.1264236179284866091, 1.281988188922614125 ) ) ;
#17708 = ORIENTED_EDGE ( 'NONE', *, *, #46159, .T. ) ;
#17709 = CARTESIAN_POINT ( 'NONE',  ( -0.1787899950787401604, -1.223425196796630532, 0.07405724077823318263 ) ) ;
#17710 = CARTESIAN_POINT ( 'NONE',  ( -0.1787899950787401882, -1.378444881836000002, 0.000000000000000000 ) ) ;
#17711 = ( BOUNDED_CURVE ( )  B_SPLINE_CURVE ( 2, ( #35665, #10748, #39467, #43301, #38999, #3040, #39690, #32317, #13600 ),
 .UNSPECIFIED., .F., .T. ) 
 B_SPLINE_CURVE_WITH_KNOTS ( ( 3, 2, 2, 2, 3 ),
 ( 0.8699999999999999956, 0.8725000000000000533, 0.8750000000000000000, 0.8774999999999999467, 0.8800000000000000044 ),
 .UNSPECIFIED. ) 
 CURVE ( )  GEOMETRIC_REPRESENTATION_ITEM ( )  RATIONAL_B_SPLINE_CURVE ( ( 1.000000000000000000, 0.9238795325112869605, 1.000000000000000000, 0.9238795325112869605, 1.000000000000000000, 0.9238795325112869605, 1.000000000000000000, 0.9238795325112869605, 1.000000000000000000 ) ) 
 REPRESENTATION_ITEM ( '' )  ) ;
#17712 = CARTESIAN_POINT ( 'NONE',  ( -0.7646288533564489232, -0.1113553986120547346, 1.363188976270427455 ) ) ;
#17713 = SHAPE_REPRESENTATION_RELATIONSHIP ( 'NONE' , 'NONE' ,  #1042, #12440 ) ;
#17714 = CARTESIAN_POINT ( 'NONE',  ( 0.07444174185955046430, -0.6432524710003691970, -0.1797182628040039087 ) ) ;
#17715 = DIRECTION ( 'NONE',  ( 0.000000000000000000, 0.000000000000000000, 1.000000000000000000 ) ) ;
#17716 = CARTESIAN_POINT ( 'NONE',  ( -0.9873396505805591694, 0.1113553986120547346, 0.9891732282389291697 ) ) ;
#17717 = CARTESIAN_POINT ( 'NONE',  ( -0.9873396505805591694, -0.1113553986120547346, 0.6742125984251968740 ) ) ;
#17718 = CARTESIAN_POINT ( 'NONE',  ( 0.8759842519685039353, 0.1787899950787401882, 0.3912401574265515491 ) ) ;
#17719 = CARTESIAN_POINT ( 'NONE',  ( 0.1574803149606299191, -0.1653543307086614012, -1.928577636452523993E-17 ) ) ;
#17720 = CONICAL_SURFACE ( 'NONE', #20050, 0.1003937007874010356, 0.7853981633978647237 ) ;
#17721 = VECTOR ( 'NONE', #35391, 39.37007874015748143 ) ;
#17722 = CARTESIAN_POINT ( 'NONE',  ( 0.7646288533564489232, 0.1113553986120547346, 1.786417322727117840 ) ) ;
#17723 = DIRECTION ( 'NONE',  ( -1.000000000000000000, 0.000000000000000000, 1.144917494144692682E-16 ) ) ;
#17724 = CARTESIAN_POINT ( 'NONE',  ( 0.8759842519685039353, 0.1574803149606299191, 0.8464566929133857665 ) ) ;
#17725 = CONICAL_SURFACE ( 'NONE', #36855, 0.2471922904502826812, 0.5235987755982992597 ) ;
#17726 = CARTESIAN_POINT ( 'NONE',  ( 0.05712600390865848338, -0.2625125185280174911, -0.05471869868084958122 ) ) ;
#17727 = CARTESIAN_POINT ( 'NONE',  ( -0.9412147342319837628, 0.1574803149606300301, 1.080216535433071501 ) ) ;
#17728 = CARTESIAN_POINT ( 'NONE',  ( 0.6195511811023610704, 0.6102362204724403050, 0.5167322834645649010 ) ) ;
#17729 = CARTESIAN_POINT ( 'NONE',  ( 0.7185039370078739607, 1.928577636452523993E-17, 0.2559055117034968463 ) ) ;
#17730 = CARTESIAN_POINT ( 'NONE',  ( 0.07405724077823318263, -0.06692913380450424277, 0.1787899950787401604 ) ) ;
#17731 = DIRECTION ( 'NONE',  ( 0.000000000000000000, 0.000000000000000000, 1.000000000000000000 ) ) ;
#17732 = CARTESIAN_POINT ( 'NONE',  ( 0.1113553986120547346, -1.459645669183811112, 0.1113553986120547346 ) ) ;
#17733 = CARTESIAN_POINT ( 'NONE',  ( 0.1787899950787401604, -0.5738188975840317063, -0.07405724077823318263 ) ) ;
#17734 = CARTESIAN_POINT ( 'NONE',  ( -0.1113553986120547346, -1.085629921259842590, 0.1113553986120547346 ) ) ;
#17736 = ( BOUNDED_CURVE ( )  B_SPLINE_CURVE ( 2, ( #26071, #11226, #410, #15060, #44253, #30177, #7845, #33514, #15287 ),
 .UNSPECIFIED., .F., .T. ) 
 B_SPLINE_CURVE_WITH_KNOTS ( ( 3, 2, 2, 2, 3 ),
 ( 0.1600000000000000033, 0.1625000000000000056, 0.1650000000000000078, 0.1675000000000000100, 0.1700000000000000122 ),
 .UNSPECIFIED. ) 
 CURVE ( )  GEOMETRIC_REPRESENTATION_ITEM ( )  RATIONAL_B_SPLINE_CURVE ( ( 1.000000000000000000, 0.9238795325112869605, 1.000000000000000000, 0.9238795325112869605, 1.000000000000000000, 0.9238795325112869605, 1.000000000000000000, 0.9238795325112869605, 1.000000000000000000 ) ) 
 REPRESENTATION_ITEM ( '' )  ) ;
#17735 = CARTESIAN_POINT ( 'NONE',  ( 0.9873396505805591694, -0.1113553986120547346, 1.018700787294047228 ) ) ;
#17737 = DIRECTION ( 'NONE',  ( -1.000000000000000000, 0.000000000000000000, 0.000000000000000000 ) ) ;
#17738 = CARTESIAN_POINT ( 'NONE',  ( -0.9500414927467378812, 0.1787899950787401604, 0.3838582676627718127 ) ) ;
#17739 = ORIENTED_EDGE ( 'NONE', *, *, #46961, .T. ) ;
#17740 = EDGE_LOOP ( 'NONE', ( #10872, #31700, #5131, #35749 ) ) ;
#17741 = VERTEX_POINT ( 'NONE', #30721 ) ;
#17742 = CARTESIAN_POINT ( 'NONE',  ( -1.054774247047244540, -0.07405724077823318263, 1.638779527505292988 ) ) ;
#17743 = ORIENTED_EDGE ( 'NONE', *, *, #8653, .F. ) ;
#17744 = EDGE_CURVE ( 'NONE', #46310, #42055, #30107, .T. ) ;
#17745 = CARTESIAN_POINT ( 'NONE',  ( 1.054774247047244540, 0.07405724077823318263, 1.604330708607653921 ) ) ;
#17746 = ORIENTED_EDGE ( 'NONE', *, *, #70, .T. ) ;
#17747 = CARTESIAN_POINT ( 'NONE',  ( -1.002407869896990045, -0.1264236179284866091, 0.6520669290800944484 ) ) ;
#17748 = CARTESIAN_POINT ( 'NONE',  ( 0.8759842519685039353, -0.1787899950787401882, 0.2140748030958428971 ) ) ;
#17749 = CARTESIAN_POINT ( 'NONE',  ( -1.033464566929134687, -0.06523048226347956391, 0.4699803148531029873 ) ) ;
#17750 = CARTESIAN_POINT ( 'NONE',  ( 0.8759842519685039353, 0.1787899950787401882, 0.7062007873478109987 ) ) ;
#17751 = CARTESIAN_POINT ( 'NONE',  ( -0.6971942568897637749, 2.189545951927499583E-17, 0.7504921259304880854 ) ) ;
#17752 = AXIS2_PLACEMENT_3D ( 'NONE', #12028, #4805, #26653 ) ;
#17753 = CARTESIAN_POINT ( 'NONE',  ( 0.1465245066989980804, -0.09658349877441907427, 0.2008369897434355567 ) ) ;
#17754 = VECTOR ( 'NONE', #2806, 39.37007874015748854 ) ;
#17755 = EDGE_CURVE ( 'NONE', #31929, #2197, #45291, .T. ) ;
#17756 = CARTESIAN_POINT ( 'NONE',  ( 0.7185039370078746268, 0.06523048226347956391, 1.080216535325543958 ) ) ;
#17757 = CARTESIAN_POINT ( 'NONE',  ( -0.1574803149606300301, -0.2563976376877486474, -0.06523048226347956391 ) ) ;
#17758 = CARTESIAN_POINT ( 'NONE',  ( -0.9500414927467378812, -0.1787899950787401604, 1.437007873961985371 ) ) ;
#17759 = CARTESIAN_POINT ( 'NONE',  ( -0.8759842519685039353, -0.1574803149606299191, 0.3937007874015748254 ) ) ;
#17760 = CARTESIAN_POINT ( 'NONE',  ( 0.8759842519685039353, 0.1787899950787401882, 1.532972440891118060 ) ) ;
#17761 = CARTESIAN_POINT ( 'NONE',  ( -0.9873396505805591694, -0.1113553986120547346, 1.579724409448818978 ) ) ;
#17762 = ORIENTED_EDGE ( 'NONE', *, *, #14189, .T. ) ;
#17763 = AXIS2_PLACEMENT_3D ( 'NONE', #28912, #43476, #41047 ) ;
#17764 = ORIENTED_EDGE ( 'NONE', *, *, #10121, .T. ) ;
#17765 = CARTESIAN_POINT ( 'NONE',  ( 1.033464566929133799, 0.000000000000000000, 0.4822834645669291653 ) ) ;
#17766 = VERTEX_POINT ( 'NONE', #31187 ) ;
#17767 = CARTESIAN_POINT ( 'NONE',  ( 0.6971942568897648851, 0.07405724077823318263, 1.456692913332062744 ) ) ;
#17768 = CARTESIAN_POINT ( 'NONE',  ( 0.6195511811023612925, 0.6102362204724401940, 0.9891732283464566011 ) ) ;
#17769 = CARTESIAN_POINT ( 'NONE',  ( -0.1264236179284866091, -0.3548228345919058890, 0.1264236179284866091 ) ) ;
#17770 = CARTESIAN_POINT ( 'NONE',  ( 0.07405724077823318263, -0.8789370078202529690, -0.1787899950787401604 ) ) ;
#17771 = DIRECTION ( 'NONE',  ( 0.000000000000000000, -1.000000000000000000, 0.000000000000000000 ) ) ;
#17772 = CARTESIAN_POINT ( 'NONE',  ( -1.033464566929133799, 0.000000000000000000, 0.9842519683964094934 ) ) ;
#17773 = ( NAMED_UNIT ( * ) SI_UNIT ( $, .STERADIAN. ) SOLID_ANGLE_UNIT ( ) ) ;
#17774 = CARTESIAN_POINT ( 'NONE',  ( 0.7495606340400177148, -0.1264236179284866091, 1.660925196796630088 ) ) ;
#17775 = CARTESIAN_POINT ( 'NONE',  ( 1.002407869896990045, -0.1264236179284866091, 0.3715551180564728440 ) ) ;
#17776 = CARTESIAN_POINT ( 'NONE',  ( -1.094772975963752103E-17, -0.1836869603552232222, -0.1787899950787401882 ) ) ;
#17777 = DIRECTION ( 'NONE',  ( 0.000000000000000000, 0.000000000000000000, -1.000000000000000000 ) ) ;
#17778 = CARTESIAN_POINT ( 'NONE',  ( 0.7185039370078739607, 1.928577636452523993E-17, 0.5708661416247566844 ) ) ;
#17779 = CARTESIAN_POINT ( 'NONE',  ( 0.7495606340400177148, 0.1264236179284866091, 0.6668307086076534773 ) ) ;
#17780 = AXIS2_PLACEMENT_3D ( 'NONE', #38305, #23940, #27078 ) ;
#17781 = CARTESIAN_POINT ( 'NONE',  ( -0.7495606340400177148, -0.1264236179284866091, 1.035925196796629866 ) ) ;
#17783 = CARTESIAN_POINT ( 'NONE',  ( -0.4338976377952755703, 0.2559055118110236116, 3.133938659235350488E-17 ) ) ;
#17782 = CARTESIAN_POINT ( 'NONE',  ( -0.8959059128496592583, 0.1723076359399909885, 0.03937007874015844427 ) ) ;
#17785 = CARTESIAN_POINT ( 'NONE',  ( -0.8875170849661903061, -0.1744992477839313050, 1.988385192983781025 ) ) ;
#17784 = CARTESIAN_POINT ( 'NONE',  ( -0.07444174185955065859, -1.701323337142099934, -0.1797182628040039087 ) ) ;
#17786 = CARTESIAN_POINT ( 'NONE',  ( 0.07405724077823318263, -0.4458661416785199560, -0.1787899950787401604 ) ) ;
#17787 = FACE_OUTER_BOUND ( 'NONE', #22358, .T. ) ;
#17788 = CARTESIAN_POINT ( 'NONE',  ( 0.8759842519685039353, -0.1787899950787401882, 1.670767716481669440 ) ) ;
#17790 = CARTESIAN_POINT ( 'NONE',  ( 0.1624141299556661477, 0.1597555635152225761, 1.164103944325189621E-06 ) ) ;
#17789 = CARTESIAN_POINT ( 'NONE',  ( 0.2272550450523252441, 0.05212746764700336433, -0.1542273094304812131 ) ) ;
#17791 = VERTEX_POINT ( 'NONE', #12971 ) ;
#17792 = VECTOR ( 'NONE', #31728, 39.37007874015748854 ) ;
#17793 = EDGE_CURVE ( 'NONE', #11128, #23920, #42162, .T. ) ;
#17794 = CARTESIAN_POINT ( 'NONE',  ( 0.9873396505805591694, -0.1113553986120547346, 1.333661417215306955 ) ) ;
#17795 = CARTESIAN_POINT ( 'NONE',  ( 0.07405724077823318263, -0.07185039364702387743, 0.1787899950787401604 ) ) ;
#17796 = CARTESIAN_POINT ( 'NONE',  ( -0.9500414927467378812, -0.1787899950787401604, 0.4133858267178901480 ) ) ;
#17797 = CARTESIAN_POINT ( 'NONE',  ( 0.8019270111902717657, -0.1787899950787401604, 0.5610236219934807700 ) ) ;
#17798 = CARTESIAN_POINT ( 'NONE',  ( -0.1264236179284866091, -1.029035433017102319, -0.1264236179284866091 ) ) ;
#17799 = CARTESIAN_POINT ( 'NONE',  ( 0.7495606340400177148, -0.1264236179284866091, 0.05167322829269323931 ) ) ;
#17800 = CARTESIAN_POINT ( 'NONE',  ( 0.4208034506101054895, 4.466152701071653354E-17, 0.000000000000000000 ) ) ;
#17801 = CARTESIAN_POINT ( 'NONE',  ( -1.054774247047244096, 0.000000000000000000, 1.636318897584031484 ) ) ;
#17802 = ORIENTED_EDGE ( 'NONE', *, *, #42714, .F. ) ;
#17803 = VECTOR ( 'NONE', #852, 39.37007874015748143 ) ;
#17804 = CARTESIAN_POINT ( 'NONE',  ( -0.3094378032379023757, -0.02221465895966925203, -0.7097682129517437488 ) ) ;
#17805 = EDGE_CURVE ( 'NONE', #13679, #44149, #43585, .T. ) ;
#17806 = CARTESIAN_POINT ( 'NONE',  ( 0.7495606340400177148, -0.1264236179284866091, 1.114665354276944909 ) ) ;
#17807 = CARTESIAN_POINT ( 'NONE',  ( -0.7646288533564489232, 0.1113553986120547346, 0.6840551180027086842 ) ) ;
#17808 = CARTESIAN_POINT ( 'NONE',  ( 0.9412147342319837628, -0.1574803149606297803, 1.498523622047243764 ) ) ;
#17809 = CARTESIAN_POINT ( 'NONE',  ( 1.054774247047244540, -0.07405724077823318263, 1.870078740103715331 ) ) ;
#17810 = CARTESIAN_POINT ( 'NONE',  ( -0.7185039370078746268, -0.06523048226347956391, 0.5831692913385827515 ) ) ;
#17811 = CARTESIAN_POINT ( 'NONE',  ( -0.6971942568897637749, 2.189545951927499583E-17, 0.9079724408911180600 ) ) ;
#17812 = DIRECTION ( 'NONE',  ( 1.831190596606011519E-15, -0.7880107536067199048, 0.6156614753256609562 ) ) ;
#17813 = CARTESIAN_POINT ( 'NONE',  ( -0.05473415491935922084, -0.2638934531858492805, -0.05654496252297270403 ) ) ;
#17814 = CARTESIAN_POINT ( 'NONE',  ( 1.054774247047244096, 0.000000000000000000, 0.3026574802611972648 ) ) ;
#17815 = CARTESIAN_POINT ( 'NONE',  ( -1.054774247047244096, 0.000000000000000000, 0.2189960629383626012 ) ) ;
#17816 = UNCERTAINTY_MEASURE_WITH_UNIT (LENGTH_MEASURE( 1.000000000000000082E-05 ), #28286, 'distance_accuracy_value', 'NONE') ;
#17817 = CARTESIAN_POINT ( 'NONE',  ( -0.8019270111902717657, 0.1787899950787401604, 0.7431102361667091261 ) ) ;
#17818 = CARTESIAN_POINT ( 'NONE',  ( 0.7646288533564489232, -0.1113553986120547346, 1.560039369971212508 ) ) ;
#17819 = ORIENTED_EDGE ( 'NONE', *, *, #11248, .T. ) ;
#17820 = CARTESIAN_POINT ( 'NONE',  ( 0.07405724077823318263, -0.05708661411946481384, -0.1787899950787401604 ) ) ;
#17821 = EDGE_LOOP ( 'NONE', ( #46949, #41887, #36288, #17453 ) ) ;
#17822 = CARTESIAN_POINT ( 'NONE',  ( 1.054774247047244096, 0.000000000000000000, 0.8538385826234016207 ) ) ;
#17823 = CARTESIAN_POINT ( 'NONE',  ( -1.054774247047244096, 0.000000000000000000, 1.872539370024976391 ) ) ;
#17824 = CARTESIAN_POINT ( 'NONE',  ( 0.9500414927467378812, -0.1787899950787401604, 1.943897637741510254 ) ) ;
#17825 = ORIENTED_EDGE ( 'NONE', *, *, #42405, .T. ) ;
#17826 = CARTESIAN_POINT ( 'NONE',  ( -0.2471922904502827090, 0.08082342248659966921, -0.07163232281567466497 ) ) ;
#17827 = CYLINDRICAL_SURFACE ( 'NONE', #11450, 0.09842519685039310962 ) ;
#17828 = CARTESIAN_POINT ( 'NONE',  ( 0.1787899950787401604, -1.372171212323726852, -0.07405724077823318263 ) ) ;
#17829 = ORIENTED_EDGE ( 'NONE', *, *, #35815, .T. ) ;
#17830 = CARTESIAN_POINT ( 'NONE',  ( -0.1787899950787401604, -0.2736220471903310081, 0.07405724077823318263 ) ) ;
#17831 = ORIENTED_EDGE ( 'NONE', *, *, #23981, .F. ) ;
#17832 = CARTESIAN_POINT ( 'NONE',  ( 1.054774247047244540, 0.07405724077823318263, 1.048228346402928723 ) ) ;
#17833 = ( GEOMETRIC_REPRESENTATION_CONTEXT ( 3 ) GLOBAL_UNCERTAINTY_ASSIGNED_CONTEXT ( ( #32214 ) ) GLOBAL_UNIT_ASSIGNED_CONTEXT ( ( #35928, #17476, #2381 ) ) REPRESENTATION_CONTEXT ( 'NONE', 'WORKASPACE' ) ) ;
#17834 = CIRCLE ( 'NONE', #27026, 0.2460629921259842590 ) ;
#17835 = CARTESIAN_POINT ( 'NONE',  ( -0.5314960629921260393, 0.000000000000000000, 4.498031496062992574 ) ) ;
#17836 = CARTESIAN_POINT ( 'NONE',  ( -0.2471920410536367907, -0.09140649424435846881, 0.04498895533817294512 ) ) ;
#17837 = CARTESIAN_POINT ( 'NONE',  ( 0.9412147342319837628, 0.1574803149606300301, 1.946358267716538082 ) ) ;
#17838 = AXIS2_PLACEMENT_3D ( 'NONE', #4918, #19542, #34190 ) ;
#17839 = CARTESIAN_POINT ( 'NONE',  ( -0.1787899950787401604, -1.617125984198204414, 0.07405724077823318263 ) ) ;
#17840 = CARTESIAN_POINT ( 'NONE',  ( -0.6971942568897648851, 0.07405724077823318263, 0.4773622046706456068 ) ) ;
#17841 = FACE_OUTER_BOUND ( 'NONE', #25390, .T. ) ;
#17842 = CARTESIAN_POINT ( 'NONE',  ( 0.6971942568897637749, 2.189545951927499583E-17, 1.188484251914740275 ) ) ;
#17843 = CARTESIAN_POINT ( 'NONE',  ( 1.054774247047244540, 0.07405724077823318263, 1.481299212544662902 ) ) ;
#17844 = EDGE_CURVE ( 'NONE', #5685, #4833, #39986, .T. ) ;
#17845 = CARTESIAN_POINT ( 'NONE',  ( 0.7646288533564489232, 0.1113553986120547346, 1.717519685039369914 ) ) ;
#17846 = CARTESIAN_POINT ( 'NONE',  ( -0.9412147342319837628, 0.1574803149606300301, 1.001476377952755348 ) ) ;
#17847 = FACE_OUTER_BOUND ( 'NONE', #36870, .T. ) ;
#17848 = CARTESIAN_POINT ( 'NONE',  ( -1.033464566929134687, -0.06523048226347956391, 1.729822834538142784 ) ) ;
#17849 = CARTESIAN_POINT ( 'NONE',  ( 0.6971942568897626646, -0.07405724077823297447, 0.2411417322297011168 ) ) ;
#17850 = ( BOUNDED_CURVE ( )  B_SPLINE_CURVE ( 2, ( #13935, #28579, #43144, #10352, #5557, #31219, #45796, #13003, #35046 ),
 .UNSPECIFIED., .F., .T. ) 
 B_SPLINE_CURVE_WITH_KNOTS ( ( 3, 2, 2, 2, 3 ),
 ( 0.3099999999999999978, 0.3125000000000000000, 0.3150000000000000022, 0.3175000000000000044, 0.3200000000000000067 ),
 .UNSPECIFIED. ) 
 CURVE ( )  GEOMETRIC_REPRESENTATION_ITEM ( )  RATIONAL_B_SPLINE_CURVE ( ( 1.000000000000000000, 0.9238795325112869605, 1.000000000000000000, 0.9238795325112869605, 1.000000000000000000, 0.9238795325112869605, 1.000000000000000000, 0.9238795325112869605, 1.000000000000000000 ) ) 
 REPRESENTATION_ITEM ( '' )  ) ;
#17851 = EDGE_CURVE ( 'NONE', #36580, #29380, #16893, .T. ) ;
#17852 = COLOUR_RGB ( '', 0.72549020, 0.75294118, 0.79215686) ;
#17854 = DIRECTION ( 'NONE',  ( 1.000000000000000000, 0.000000000000000000, 0.000000000000000000 ) ) ;
#17853 = CARTESIAN_POINT ( 'NONE',  ( 0.6971942568897648851, 0.07405724077823318263, 1.062992125930488418 ) ) ;
#17855 = DIRECTION ( 'NONE',  ( -1.000000000000000000, 0.000000000000000000, 0.000000000000000000 ) ) ;
#17856 = CARTESIAN_POINT ( 'NONE',  ( 0.7185039370078746268, 0.06523048226347956391, 0.4502952754830242266 ) ) ;
#17857 = ORIENTED_EDGE ( 'NONE', *, *, #3076, .T. ) ;
#17858 = DIRECTION ( 'NONE',  ( 0.000000000000000000, 0.000000000000000000, -1.000000000000000000 ) ) ;
#17859 = EDGE_CURVE ( 'NONE', #17892, #37198, #21806, .T. ) ;
#17860 = CARTESIAN_POINT ( 'NONE',  ( -0.9412147342319837628, 0.1574803149606300301, 1.897145669183811778 ) ) ;
#17861 = CARTESIAN_POINT ( 'NONE',  ( 2.892866454678787531E-17, -1.031496062884598386, 0.1574803149606299191 ) ) ;
#17862 = CARTESIAN_POINT ( 'NONE',  ( -0.7646288533564489232, -0.1113553986120547346, 0.3789370077664886427 ) ) ;
#17863 = CARTESIAN_POINT ( 'NONE',  ( 0.6971942568897648851, 0.07405724077823318263, 1.417322834591906222 ) ) ;
#17864 = EDGE_CURVE ( 'NONE', #13286, #24988, #21073, .T. ) ;
#17865 = DIRECTION ( 'NONE',  ( -0.000000000000000000, 0.000000000000000000, -1.000000000000000000 ) ) ;
#17866 = CARTESIAN_POINT ( 'NONE',  ( -1.094772975963752103E-17, -0.08907480309584270284, -0.1787899950787401882 ) ) ;
#17867 = ORIENTED_EDGE ( 'NONE', *, *, #8880, .F. ) ;
#17868 = CARTESIAN_POINT ( 'NONE',  ( 0.1619971594100464152, -0.06735705997062264860, -0.1405166210180647801 ) ) ;
#17869 = VERTEX_POINT ( 'NONE', #21554 ) ;
#17870 = CARTESIAN_POINT ( 'NONE',  ( -0.8070866141732283561, 0.000000000000000000, 0.7574803149606299524 ) ) ;
#17871 = CARTESIAN_POINT ( 'NONE',  ( 0.1435836963516304854, -0.09660391682274863112, -0.2025327002555687705 ) ) ;
#17872 = CARTESIAN_POINT ( 'NONE',  ( 0.8759842519685039353, 0.1787899950787401882, 0.5487204723871811352 ) ) ;
#17873 = ORIENTED_EDGE ( 'NONE', *, *, #33087, .T. ) ;
#17874 = CARTESIAN_POINT ( 'NONE',  ( -0.1574803149606299191, 0.06102362215477106361, 0.000000000000000000 ) ) ;
#17875 = CARTESIAN_POINT ( 'NONE',  ( -0.7495606340400177148, -0.1264236179284866091, 1.075295275536787276 ) ) ;
#17876 = CARTESIAN_POINT ( 'NONE',  ( -0.9412147342319837628, 0.1574803149606300301, 0.1747047244094488694 ) ) ;
#17877 = VERTEX_POINT ( 'NONE', #13895 ) ;
#17878 = CARTESIAN_POINT ( 'NONE',  ( -0.7495606340400177148, -0.1264236179284866091, 1.149114173174582643 ) ) ;
#17879 = CARTESIAN_POINT ( 'NONE',  ( -0.8019270111902717657, -0.1787899950787401604, 0.2509842519147403861 ) ) ;
#17880 = FACE_OUTER_BOUND ( 'NONE', #39784, .T. ) ;
#17881 = FACE_OUTER_BOUND ( 'NONE', #43686, .T. ) ;
#17882 = CARTESIAN_POINT ( 'NONE',  ( -1.094772975963752103E-17, -0.7742381414575847387, -0.1787899950787401882 ) ) ;
#17883 = ORIENTED_EDGE ( 'NONE', *, *, #41559, .T. ) ;
#17884 = CARTESIAN_POINT ( 'NONE',  ( -0.1007914167158820845, -0.08956157794326476129, 0.1244328764867059095 ) ) ;
#17885 = VERTEX_POINT ( 'NONE', #36191 ) ;
#17886 = ORIENTED_EDGE ( 'NONE', *, *, #47, .F. ) ;
#17887 = DIRECTION ( 'NONE',  ( -1.000000000000000000, 0.000000000000000000, 0.000000000000000000 ) ) ;
#17888 = AXIS2_PLACEMENT_3D ( 'NONE', #40222, #13899, #21313 ) ;
#17889 = CARTESIAN_POINT ( 'NONE',  ( 0.2362204724409448231, 0.000000000000000000, 1.186023622047243986 ) ) ;
#17890 = CARTESIAN_POINT ( 'NONE',  ( -1.054774247047244540, -0.07405724077823318263, 0.6102362204186774219 ) ) ;
#17891 = FACE_OUTER_BOUND ( 'NONE', #4668, .T. ) ;
#17892 = VERTEX_POINT ( 'NONE', #6693 ) ;
#17893 = CARTESIAN_POINT ( 'NONE',  ( -1.054774247047244540, -0.07405724077823318263, 1.796259842465920853 ) ) ;
#17894 = ORIENTED_EDGE ( 'NONE', *, *, #18187, .F. ) ;
#17895 = FACE_OUTER_BOUND ( 'NONE', #5252, .T. ) ;
#17896 = CARTESIAN_POINT ( 'NONE',  ( -0.6971942568897626646, -0.07405724077823297447, 0.04921259837143338728 ) ) ;
#17897 = ORIENTED_EDGE ( 'NONE', *, *, #11878, .T. ) ;
#17898 = CARTESIAN_POINT ( 'NONE',  ( 0.07444174185955046430, -0.8794729434413131042, -0.1797182628040039087 ) ) ;
#17899 = CARTESIAN_POINT ( 'NONE',  ( -2.680625843783058887E-15, -0.2954942322624074524, -0.2921040715117803055 ) ) ;
#17900 = CARTESIAN_POINT ( 'NONE',  ( -0.7185039370078746268, 0.06523048226347956391, 1.434547243986962428 ) ) ;
#17901 = CARTESIAN_POINT ( 'NONE',  ( 1.002407869896990045, -0.1264236179284866091, 0.8095472440407244230 ) ) ;
#17902 = CARTESIAN_POINT ( 'NONE',  ( -0.08069314021478943277, 0.1221948107111021781, -0.1379473356501541015 ) ) ;
#17903 = ORIENTED_EDGE ( 'NONE', *, *, #12189, .F. ) ;
#17904 = PLANE ( 'NONE',  #43713 ) ;
#17905 = CARTESIAN_POINT ( 'NONE',  ( 0.8759842519685039353, -0.1574803149606299191, 1.181102362204724310 ) ) ;
#17906 = CARTESIAN_POINT ( 'NONE',  ( 0.7753512748119036901, -0.1383705155101382922, 1.986206650002734886 ) ) ;
#17907 = CARTESIAN_POINT ( 'NONE',  ( 0.7646288533564489232, -0.1113553986120547346, 1.845472440944881942 ) ) ;
#17908 = EDGE_CURVE ( 'NONE', #35268, #15333, #45208, .T. ) ;
#17910 = FACE_OUTER_BOUND ( 'NONE', #14421, .T. ) ;
#17909 = CARTESIAN_POINT ( 'NONE',  ( 1.002407869896990045, 0.1264236179284866091, 0.6963582676627716461 ) ) ;
#17911 = CARTESIAN_POINT ( 'NONE',  ( -0.1787899950787401882, -0.6304133857730078727, 0.000000000000000000 ) ) ;
#17912 = CARTESIAN_POINT ( 'NONE',  ( 0.000000000000000000, 0.000000000000000000, -0.2219368594840610276 ) ) ;
#17913 = ORIENTED_EDGE ( 'NONE', *, *, #20556, .F. ) ;
#17914 = CARTESIAN_POINT ( 'NONE',  ( 0.1606807218934673820, 0.07955615087644739292, 0.1377952558084805934 ) ) ;
#17915 = CARTESIAN_POINT ( 'NONE',  ( 0.1564216623530368111, -8.910440797025414093E-13, -0.1403857474672218497 ) ) ;
#17916 = CARTESIAN_POINT ( 'NONE',  ( 1.054774247047244096, 0.000000000000000000, 1.045767716481669440 ) ) ;
#17917 = EDGE_CURVE ( 'NONE', #12524, #47303, #32253, .T. ) ;
#17918 = FACE_OUTER_BOUND ( 'NONE', #44080, .T. ) ;
#17919 = CARTESIAN_POINT ( 'NONE',  ( -0.1787899950787401604, -1.262795275536788386, 0.07405724077823318263 ) ) ;
#17920 = CARTESIAN_POINT ( 'NONE',  ( -0.1113553986120547346, -1.518700787401574770, 0.1113553986120547346 ) ) ;
#17921 = DIRECTION ( 'NONE',  ( 0.000000000000000000, -1.000000000000000000, 0.000000000000000000 ) ) ;
#17922 = CARTESIAN_POINT ( 'NONE',  ( -0.6971942568897626646, -0.07405724077823297447, 0.1230314960092287191 ) ) ;
#17923 = ORIENTED_EDGE ( 'NONE', *, *, #1026, .F. ) ;
#17924 = CARTESIAN_POINT ( 'NONE',  ( 0.6971942568897648851, 0.07405724077823318263, 1.934055118056471567 ) ) ;
#17925 = ORIENTED_EDGE ( 'NONE', *, *, #1132, .F. ) ;
#17926 = CARTESIAN_POINT ( 'NONE',  ( -0.9500414927467377701, -0.1787899950787401604, 1.909448818843873186 ) ) ;
#17927 = CARTESIAN_POINT ( 'NONE',  ( -0.9500414927467378812, -0.1787899950787401604, 1.707677165300566235 ) ) ;
#17928 = CARTESIAN_POINT ( 'NONE',  ( 0.6971942568897637749, 2.189545951927499583E-17, 0.8735236219934803259 ) ) ;
#17929 = CARTESIAN_POINT ( 'NONE',  ( -0.2471922904502825424, 0.07573437638786091608, 0.08155181604443949295 ) ) ;
#17930 = CARTESIAN_POINT ( 'NONE',  ( -0.6971942568897648851, 0.07405724077823318263, 1.894685039316315489 ) ) ;
#17931 = CARTESIAN_POINT ( 'NONE',  ( 0.7185039370078739607, 1.928577636452523993E-17, 0.3051181102362204856 ) ) ;
#17932 = CARTESIAN_POINT ( 'NONE',  ( -0.9873396505805591694, -0.1113553986120547346, 1.894685039370078927 ) ) ;
#17933 = DIRECTION ( 'NONE',  ( -1.000000000000000000, 0.000000000000000000, 0.000000000000000000 ) ) ;
#17934 = CARTESIAN_POINT ( 'NONE',  ( 0.1264236179284866091, -0.3460885351583728453, -0.1264236179284866091 ) ) ;
#17935 = CARTESIAN_POINT ( 'NONE',  ( -0.04622344188396850656, -0.09842519685039370636, 0.1526493060429974513 ) ) ;
#17936 = CARTESIAN_POINT ( 'NONE',  ( -0.7185039370078739607, 1.928577636452523993E-17, 1.318897637687747926 ) ) ;
#17937 = CARTESIAN_POINT ( 'NONE',  ( -0.8759842519685039353, -0.1787899950787401882, 0.1697834645131655606 ) ) ;
#17938 = ORIENTED_EDGE ( 'NONE', *, *, #40917, .F. ) ;
#17939 = CARTESIAN_POINT ( 'NONE',  ( -0.8759842519685039353, 0.1787899950787401882, 1.414862204670645829 ) ) ;
#17940 = ORIENTED_EDGE ( 'NONE', *, *, #26036, .T. ) ;
#17941 = CARTESIAN_POINT ( 'NONE',  ( -0.07405724077823318263, -1.139763779473794925, 0.1787899950787401604 ) ) ;
#17942 = CARTESIAN_POINT ( 'NONE',  ( -0.1787899950787401604, -1.336614173174582865, 0.07405724077823318263 ) ) ;
#17943 = FACE_OUTER_BOUND ( 'NONE', #21695, .T. ) ;
#17944 = DIRECTION ( 'NONE',  ( 1.000000000000000000, 0.000000000000000000, 0.000000000000000000 ) ) ;
#17945 = CARTESIAN_POINT ( 'NONE',  ( 0.9873396505805591694, 0.1113553986120547346, 0.3297244094488189226 ) ) ;
#17946 = AXIS2_PLACEMENT_3D ( 'NONE', #43625, #18697, #29319 ) ;
#17947 = CARTESIAN_POINT ( 'NONE',  ( 0.1184675242425352465, 0.3740157480314960647, 2.185526306663015728 ) ) ;
#17948 = CARTESIAN_POINT ( 'NONE',  ( -0.7646288533564489232, 0.1113553986120547346, 0.9596456691838111119 ) ) ;
#17949 = CARTESIAN_POINT ( 'NONE',  ( 0.7495606340400177148, -0.1264236179284866091, 0.4847440944344252323 ) ) ;
#17950 = CARTESIAN_POINT ( 'NONE',  ( -9.642888182262618425E-18, -0.07677165354330708902, -0.1574803149606299191 ) ) ;
#17951 = CIRCLE ( 'NONE', #40106, 0.1003937007874011050 ) ;
#17952 = VECTOR ( 'NONE', #39988, 39.37007874015748143 ) ;
#17953 = CARTESIAN_POINT ( 'NONE',  ( 1.033464566929134687, -0.06523048226347956391, 1.887303149498773092 ) ) ;
#17954 = ORIENTED_EDGE ( 'NONE', *, *, #42714, .T. ) ;
#17955 = CARTESIAN_POINT ( 'NONE',  ( -0.5314960629921260393, 0.000000000000000000, 4.842519685039370358 ) ) ;
#17956 = CARTESIAN_POINT ( 'NONE',  ( 0.8107537697050253289, -0.1574803149606297803, 0.7849409448818904789 ) ) ;
#17957 = CARTESIAN_POINT ( 'NONE',  ( 0.1643970000112103258, -0.08114886790928133031, -0.1405539621936140182 ) ) ;
#17958 = CARTESIAN_POINT ( 'NONE',  ( -0.9873396505805591694, -0.1113553986120547346, 1.609251968396409493 ) ) ;
#17959 = EDGE_CURVE ( 'NONE', #6423, #954, #3905, .T. ) ;
#17960 = CARTESIAN_POINT ( 'NONE',  ( -0.8759842519685039353, -0.1574803149606299191, 0.4724409448818898127 ) ) ;
#17961 = CARTESIAN_POINT ( 'NONE',  ( 0.7185039370078746268, 0.06523048226347956391, 0.1353346455617644717 ) ) ;
#17962 = VERTEX_POINT ( 'NONE', #25410 ) ;
#17963 = CARTESIAN_POINT ( 'NONE',  ( 0.1787899950787401882, -0.05954724404072461036, -2.189545951927503898E-17 ) ) ;
#17964 = EDGE_CURVE ( 'NONE', #3817, #42967, #27700, .T. ) ;
#17965 = CARTESIAN_POINT ( 'NONE',  ( 0.8759842519685039353, 0.000000000000000000, 4.498031496062992574 ) ) ;
#17966 = CARTESIAN_POINT ( 'NONE',  ( 1.033464566929133799, 0.000000000000000000, 1.850393700679873854 ) ) ;
#17967 = CARTESIAN_POINT ( 'NONE',  ( -0.1574803149606299191, -1.592519684931842372, 0.000000000000000000 ) ) ;
#17968 = CARTESIAN_POINT ( 'NONE',  ( -0.07405724077823318263, -0.7854330708123791194, 0.1787899950787401604 ) ) ;
#17969 = CARTESIAN_POINT ( 'NONE',  ( -0.7646288533564489232, -0.1113553986120547346, 0.1427165353255439029 ) ) ;
#17970 = CARTESIAN_POINT ( 'NONE',  ( 0.06523048226347956391, -0.9995078740157482544, 0.1574803149606297803 ) ) ;
#17971 = CARTESIAN_POINT ( 'NONE',  ( 1.033464566929133799, 0.000000000000000000, 1.023622047136567126 ) ) ;
#17972 = DIRECTION ( 'NONE',  ( 0.000000000000000000, 0.000000000000000000, 1.000000000000000000 ) ) ;
#17973 = ORIENTED_EDGE ( 'NONE', *, *, #10359, .F. ) ;
#17974 = EDGE_LOOP ( 'NONE', ( #20574, #25857, #12572, #41783 ) ) ;
#17975 = ORIENTED_EDGE ( 'NONE', *, *, #24552, .T. ) ;
#17976 = CARTESIAN_POINT ( 'NONE',  ( -1.054774247047244096, 0.000000000000000000, 1.641240157426551161 ) ) ;
#17977 = VERTEX_POINT ( 'NONE', #40219 ) ;
#17978 = CARTESIAN_POINT ( 'NONE',  ( 1.054774247047244096, 0.000000000000000000, 1.562499999946236118 ) ) ;
#17979 = ORIENTED_EDGE ( 'NONE', *, *, #23177, .T. ) ;
#17980 = CARTESIAN_POINT ( 'NONE',  ( -0.7495606340400177148, -0.1264236179284866091, 0.8390748030958424808 ) ) ;
#17981 = CARTESIAN_POINT ( 'NONE',  ( 0.9500414927467378812, 0.1787899950787401604, 0.2312992125446618197 ) ) ;
#17982 = LINE ( 'NONE', #14405, #38863 ) ;
#17983 = CARTESIAN_POINT ( 'NONE',  ( 0.7495606340400177148, 0.1264236179284866091, 0.7111220471903307860 ) ) ;
#17984 = CARTESIAN_POINT ( 'NONE',  ( -0.9500414927467377701, -0.1787899950787401604, 0.6446850393163160442 ) ) ;
#17985 = DIRECTION ( 'NONE',  ( 0.000000000000000000, 0.000000000000000000, -1.000000000000000000 ) ) ;
#17986 = CARTESIAN_POINT ( 'NONE',  ( 0.9412147342319837628, 0.1574803149606300301, 1.070374015640503496 ) ) ;
#17987 = CARTESIAN_POINT ( 'NONE',  ( -0.06523048226347956391, -0.1678149605223941132, 0.1574803149606297803 ) ) ;
#17988 = CARTESIAN_POINT ( 'NONE',  ( -0.7646288533564489232, -0.1113553986120547346, 1.914370078632629868 ) ) ;
#17989 = ORIENTED_EDGE ( 'NONE', *, *, #39035, .T. ) ;
#17990 = AXIS2_PLACEMENT_3D ( 'NONE', #24374, #17404, #2084 ) ;
#17991 = CARTESIAN_POINT ( 'NONE',  ( -0.7646288533564489232, -0.1113553986120547346, 0.4675196850393700809 ) ) ;
#17992 = CARTESIAN_POINT ( 'NONE',  ( 1.002407869896990045, -0.1264236179284866091, 1.439468503883244210 ) ) ;
#17993 = DIRECTION ( 'NONE',  ( 0.000000000000000000, 0.2432573283306646017, -0.9699617890481188054 ) ) ;
#17994 = VECTOR ( 'NONE', #28709, 39.37007874015748143 ) ;
#17995 = ORIENTED_EDGE ( 'NONE', *, *, #47026, .F. ) ;
#17996 = ADVANCED_FACE ( 'NONE', ( #25644 ), #28539, .T. ) ;
#17997 = ( BOUNDED_CURVE ( )  B_SPLINE_CURVE ( 2, ( #42578, #13840, #17907, #20787, #32558, #14330, #46423, #35432, #43055 ),
 .UNSPECIFIED., .F., .T. ) 
 B_SPLINE_CURVE_WITH_KNOTS ( ( 3, 2, 2, 2, 3 ),
 ( 0.9300000000000000488, 0.9324999999999999956, 0.9350000000000000533, 0.9375000000000000000, 0.9399999999999999467 ),
 .UNSPECIFIED. ) 
 CURVE ( )  GEOMETRIC_REPRESENTATION_ITEM ( )  RATIONAL_B_SPLINE_CURVE ( ( 1.000000000000000000, 0.9238795325112869605, 1.000000000000000000, 0.9238795325112869605, 1.000000000000000000, 0.9238795325112869605, 1.000000000000000000, 0.9238795325112829637, 1.000000000000000000 ) ) 
 REPRESENTATION_ITEM ( '' )  ) ;
#17998 = EDGE_LOOP ( 'NONE', ( #3307, #47300 ) ) ;
#17999 = CARTESIAN_POINT ( 'NONE',  ( 0.1264236179284866091, -0.6845472440407243120, -0.1264236179284866091 ) ) ;
#18000 = EDGE_LOOP ( 'NONE', ( #40259, #36438, #22743, #25164, #10477, #8132 ) ) ;
#18001 = CARTESIAN_POINT ( 'NONE',  ( 0.4811709046783464450, 0.09842519685039370636, 1.205361022782828805E-17 ) ) ;
#18002 = CARTESIAN_POINT ( 'NONE',  ( -0.1787899950787401604, -0.4015748030958427028, -0.07405724077823318263 ) ) ;
#18003 = CARTESIAN_POINT ( 'NONE',  ( 0.07405724077823318263, -0.9576771653005667906, -0.1787899950787401604 ) ) ;
#18004 = CARTESIAN_POINT ( 'NONE',  ( 1.033464566929134687, 0.06523048226347956391, 1.035925196850394192 ) ) ;
#18005 = CARTESIAN_POINT ( 'NONE',  ( 0.8019270111902717657, -0.1787899950787401604, 0.3641732282926931630 ) ) ;
#18006 = CARTESIAN_POINT ( 'NONE',  ( -0.1797182628040039365, -0.1191382977720218533, 0.000000000000000000 ) ) ;
#18007 = ADVANCED_FACE ( 'NONE', ( #7409 ), #20726, .F. ) ;
#18008 = CARTESIAN_POINT ( 'NONE',  ( 0.1787899950787401882, -0.1147893225599474487, -2.189545951927503898E-17 ) ) ;
#18009 = CARTESIAN_POINT ( 'NONE',  ( -0.07405724077823318263, -0.2834645668753703052, -0.1787899950787401604 ) ) ;
#18010 = CARTESIAN_POINT ( 'NONE',  ( -0.1264236179284866091, -0.08907480309584270284, -0.1264236179284866091 ) ) ;
#18011 = CARTESIAN_POINT ( 'NONE',  ( 0.2471911249972296165, -0.08424752482839464873, -0.06442904123614238976 ) ) ;
#18012 = CARTESIAN_POINT ( 'NONE',  ( 0.7495606340400177148, -0.1264236179284866091, 0.6373031495525354195 ) ) ;
#18013 = ( BOUNDED_CURVE ( )  B_SPLINE_CURVE ( 2, ( #40788, #770, #11832, #15429, #26692, #30079, #26457, #8449, #23080 ),
 .UNSPECIFIED., .F., .T. ) 
 B_SPLINE_CURVE_WITH_KNOTS ( ( 3, 2, 2, 2, 3 ),
 ( 0.8000000000000000444, 0.8024999999999999911, 0.8050000000000000488, 0.8074999999999999956, 0.8100000000000000533 ),
 .UNSPECIFIED. ) 
 CURVE ( )  GEOMETRIC_REPRESENTATION_ITEM ( )  RATIONAL_B_SPLINE_CURVE ( ( 1.000000000000000000, 0.9238795325112869605, 1.000000000000000000, 0.9238795325112869605, 1.000000000000000000, 0.9238795325112869605, 1.000000000000000000, 0.9238795325112869605, 1.000000000000000000 ) ) 
 REPRESENTATION_ITEM ( '' )  ) ;
#18014 = CARTESIAN_POINT ( 'NONE',  ( -0.8019270111902716547, 0.1787899950787401604, 0.9842519684501743749 ) ) ;
#18015 = EDGE_CURVE ( 'NONE', #18496, #33336, #46006, .T. ) ;
#18017 = DIRECTION ( 'NONE',  ( 0.5735764363510447161, 0.8191520442889925757, 0.000000000000000000 ) ) ;
#18016 = CARTESIAN_POINT ( 'NONE',  ( -0.9538951735880809579, 0.1509809590367724719, 0.03937007874015843040 ) ) ;
#18018 = CARTESIAN_POINT ( 'NONE',  ( 0.1797182628040039087, -1.676717037929501775, 0.07444174185955046430 ) ) ;
#18019 = AXIS2_PLACEMENT_3D ( 'NONE', #30195, #22716, #9051 ) ;
#18020 = VECTOR ( 'NONE', #19469, 39.37007874015748854 ) ;
#18021 = ( BOUNDED_CURVE ( )  B_SPLINE_CURVE ( 2, ( #10703, #17631, #14043, #21454, #38958, #32275, #16926, #28690, #43259 ),
 .UNSPECIFIED., .F., .F. ) 
 B_SPLINE_CURVE_WITH_KNOTS ( ( 3, 2, 2, 2, 3 ),
 ( 0.6300000000000000044, 0.6324999999999999512, 0.6350000000000000089, 0.6374999999999999556, 0.6400000000000000133 ),
 .UNSPECIFIED. ) 
 CURVE ( )  GEOMETRIC_REPRESENTATION_ITEM ( )  RATIONAL_B_SPLINE_CURVE ( ( 1.000000000000000000, 0.9238795325112899581, 1.000000000000000000, 0.9238795325112869605, 1.000000000000000000, 0.9238795325112869605, 1.000000000000000000, 0.9238795325112869605, 1.000000000000000000 ) ) 
 REPRESENTATION_ITEM ( '' )  ) ;
#18022 = CARTESIAN_POINT ( 'NONE',  ( 3.284318927891251994E-17, -0.4630905511273386010, 0.1787899950787401882 ) ) ;
#18023 = CARTESIAN_POINT ( 'NONE',  ( 0.000000000000000000, 0.000000000000000000, 0.000000000000000000 ) ) ;
#18024 = CARTESIAN_POINT ( 'NONE',  ( 1.002407869896990045, 0.1264236179284866091, 1.724901574749385880 ) ) ;
#18025 = CARTESIAN_POINT ( 'NONE',  ( 0.7185039370078739607, 1.928577636452523993E-17, 1.289370078740157632 ) ) ;
#18026 = VECTOR ( 'NONE', #45936, 39.37007874015748143 ) ;
#18027 = AXIS2_PLACEMENT_3D ( 'NONE', #27231, #45862, #23383 ) ;
#18028 = ORIENTED_EDGE ( 'NONE', *, *, #5365, .F. ) ;
#18029 = EDGE_CURVE ( 'NONE', #27462, #15531, #10043, .T. ) ;
#18030 = CARTESIAN_POINT ( 'NONE',  ( 1.033464566929134687, -0.06523048226347956391, 1.336122047136566904 ) ) ;
#18031 = CARTESIAN_POINT ( 'NONE',  ( -0.07405724077823318263, -0.05216535427694517224, -0.1787899950787401604 ) ) ;
#18032 = CARTESIAN_POINT ( 'NONE',  ( -0.7495606340400177148, -0.1264236179284866091, 0.4453740156942677664 ) ) ;
#18033 = CARTESIAN_POINT ( 'NONE',  ( 0.9500414927467378812, 0.1787899950787401604, 0.5413385826234012876 ) ) ;
#18034 = CARTESIAN_POINT ( 'NONE',  ( 3.284318927891251994E-17, -1.093011810969858333, 0.1787899950787401882 ) ) ;
#18035 = CARTESIAN_POINT ( 'NONE',  ( 0.8759842519685039353, 0.1787899950787401882, 0.07627952750529173875 ) ) ;
#18036 = CARTESIAN_POINT ( 'NONE',  ( 1.033464566929134687, 0.06523048226347956391, 1.104822834538142340 ) ) ;
#18037 = CARTESIAN_POINT ( 'NONE',  ( -0.6971942568897637749, 2.189545951927499583E-17, 1.656003936954110412 ) ) ;
#18038 = ORIENTED_EDGE ( 'NONE', *, *, #21423, .F. ) ;
#18039 = CARTESIAN_POINT ( 'NONE',  ( -0.8019270111902717657, -0.1787899950787401604, 1.195866141678520345 ) ) ;
#18040 = CARTESIAN_POINT ( 'NONE',  ( -0.2833820772873882343, -0.1260390447071882414, -0.9865535077132553399 ) ) ;
#18041 = CARTESIAN_POINT ( 'NONE',  ( 0.9500414927467378812, 0.1787899950787401604, 1.136811023568283119 ) ) ;
#18042 = CARTESIAN_POINT ( 'NONE',  ( -9.642888182262618425E-18, -1.129921259734992134, -0.1574803149606299191 ) ) ;
#18043 = CARTESIAN_POINT ( 'NONE',  ( 1.002407869896990045, -0.1264236179284866091, 1.749507873961984483 ) ) ;
#18044 = CARTESIAN_POINT ( 'NONE',  ( -0.8107537697050253289, -0.1574803149606297803, 0.5880905511811019837 ) ) ;
#18045 = CARTESIAN_POINT ( 'NONE',  ( -0.6971942568897637749, 2.189545951927499583E-17, 0.9473425196312755814 ) ) ;
#18046 = CARTESIAN_POINT ( 'NONE',  ( -7.957671378281915615E-17, 0.1574803149606340824, -0.2933070866141737065 ) ) ;
#18047 = CARTESIAN_POINT ( 'NONE',  ( 0.8759842519685039353, 0.1787899950787401882, 0.3518700786863940833 ) ) ;
#18048 = CARTESIAN_POINT ( 'NONE',  ( -1.054774247047244540, -0.07405724077823318263, 0.2952755904974176948 ) ) ;
#18049 = CARTESIAN_POINT ( 'NONE',  ( -0.8019270111902717657, 0.1787899950787401604, 0.7824803149068669805 ) ) ;
#18050 = CARTESIAN_POINT ( 'NONE',  ( 0.7185039370078746268, 0.06523048226347956391, 1.631397637687747926 ) ) ;
#18051 = ORIENTED_EDGE ( 'NONE', *, *, #11008, .F. ) ;
#18052 = CARTESIAN_POINT ( 'NONE',  ( 0.1787899950787401604, -0.02755905506434671789, 0.07405724077823318263 ) ) ;
#18053 = CARTESIAN_POINT ( 'NONE',  ( 1.054774247047244540, 0.07405724077823318263, 0.7775590550643479704 ) ) ;
#18054 = CARTESIAN_POINT ( 'NONE',  ( 0.9500414927467377701, 0.1787899950787401604, 1.097440944828127041 ) ) ;
#18055 = CARTESIAN_POINT ( 'NONE',  ( -0.7495606340400177148, 0.1264236179284866091, 1.808562992072220377 ) ) ;
#18056 = CIRCLE ( 'NONE', #24198, 0.3100393700787401619 ) ;
#18057 = CARTESIAN_POINT ( 'NONE',  ( 1.002407869896990045, -0.1264236179284866091, 1.906988188922614125 ) ) ;
#18058 = VERTEX_POINT ( 'NONE', #14607 ) ;
#18059 = CARTESIAN_POINT ( 'NONE',  ( 0.8107537697050254399, -0.1574803149606297803, 1.601870078632630756 ) ) ;
#18060 = CARTESIAN_POINT ( 'NONE',  ( -0.07405724077823318263, -1.347564913111128471, 0.1787899950787401604 ) ) ;
#18061 = VERTEX_POINT ( 'NONE', #25870 ) ;
#18062 = CARTESIAN_POINT ( 'NONE',  ( 0.1264236179284866091, -0.2121062991588350544, -0.1264236179284866091 ) ) ;
#18063 = AXIS2_PLACEMENT_3D ( 'NONE', #43091, #10295, #42614 ) ;
#18064 = ORIENTED_EDGE ( 'NONE', *, *, #41719, .F. ) ;
#18065 = CARTESIAN_POINT ( 'NONE',  ( 1.054774247047244540, 0.07405724077823318263, 1.126968503883244654 ) ) ;
#18066 = EDGE_CURVE ( 'NONE', #1531, #1638, #38036, .T. ) ;
#18067 = CARTESIAN_POINT ( 'NONE',  ( -0.01585547164981878157, 0.3740157480314960647, 1.025733466389939785 ) ) ;
#18068 = CARTESIAN_POINT ( 'NONE',  ( 0.000000000000000000, 3.616083068348478250E-17, 0.2952755905511806334 ) ) ;
#18069 = CARTESIAN_POINT ( 'NONE',  ( 0.8107537697050253289, -0.1574803149606297803, 1.966043307086614567 ) ) ;
#18070 = ADVANCED_FACE ( 'NONE', ( #44990 ), #16184, .F. ) ;
#18071 = CARTESIAN_POINT ( 'NONE',  ( 3.284318927891251994E-17, -1.649114173174582643, 0.1787899950787401882 ) ) ;
#18072 = CARTESIAN_POINT ( 'NONE',  ( -0.07405724077823318263, -0.7066929133320629663, 0.1787899950787401604 ) ) ;
#18073 = CARTESIAN_POINT ( 'NONE',  ( -1.054774247047244540, -0.07405724077823318263, 0.5364173227808820554 ) ) ;
#18074 = DIRECTION ( 'NONE',  ( 0.000000000000000000, -1.000000000000000000, 0.000000000000000000 ) ) ;
#18075 = CARTESIAN_POINT ( 'NONE',  ( 0.07444174185955065859, -1.287937510370446903, 0.1797182628040039087 ) ) ;
#18076 = DIRECTION ( 'NONE',  ( 0.000000000000000000, 1.000000000000000000, 0.000000000000000000 ) ) ;
#18077 = CARTESIAN_POINT ( 'NONE',  ( 0.9500414927467378812, 0.1787899950787401604, 1.294291338528912982 ) ) ;
#18078 = CARTESIAN_POINT ( 'NONE',  ( 1.054774247047244540, 0.07405724077823318263, 1.638779527505292766 ) ) ;
#18079 = AXIS2_PLACEMENT_3D ( 'NONE', #36077, #14752, #9974 ) ;
#18080 = CARTESIAN_POINT ( 'NONE',  ( -1.033464566929134687, 0.06523048226347956391, 1.902066929133858553 ) ) ;
#18081 = ADVANCED_FACE ( 'NONE', ( #26109 ), #8350, .F. ) ;
#18082 = DIRECTION ( 'NONE',  ( 1.000000000000000000, 0.000000000000000000, -1.822029033848725275E-16 ) ) ;
#18083 = DIRECTION ( 'NONE',  ( 0.000000000000000000, 0.000000000000000000, 1.000000000000000000 ) ) ;
#18084 = CARTESIAN_POINT ( 'NONE',  ( 0.06523048226347956391, -0.7780511809948342794, -0.1574803149606300301 ) ) ;
#18085 = CARTESIAN_POINT ( 'NONE',  ( -0.7185039370078746268, 0.06523048226347956391, 1.749507873908222155 ) ) ;
#18086 = CARTESIAN_POINT ( 'NONE',  ( 0.6971942568897626646, 0.07405724077823318263, 0.1574803149068664809 ) ) ;
#18087 = CARTESIAN_POINT ( 'NONE',  ( 0.7023349083174097451, 0.03108062574093124059, 0.03937019779350070525 ) ) ;
#18089 = DIRECTION ( 'NONE',  ( 1.000000000000000000, 0.000000000000000000, -1.822029033848725275E-16 ) ) ;
#18088 = CARTESIAN_POINT ( 'NONE',  ( 0.7495606340400177148, 0.1264236179284866091, 1.178641732229700922 ) ) ;
#18090 = CARTESIAN_POINT ( 'NONE',  ( 0.9412147342319837628, -0.1574803149606297803, 1.222933070866141669 ) ) ;
#18091 = CARTESIAN_POINT ( 'NONE',  ( -1.054774247047244540, -0.07405724077823318263, 1.161417322780881278 ) ) ;
#18092 = CARTESIAN_POINT ( 'NONE',  ( 0.9412147342319837628, 0.1574803149606300301, 0.5191929132782994172 ) ) ;
#18093 = ORIENTED_EDGE ( 'NONE', *, *, #24893, .T. ) ;
#18094 = ( CONVERSION_BASED_UNIT ( 'INCH', #24580 ) LENGTH_UNIT ( ) NAMED_UNIT ( #9023 ) ) ;
#18095 = CARTESIAN_POINT ( 'NONE',  ( 0.8663930385888580776, 0.1748445346236966735, 0.03937198857582425993 ) ) ;
#18096 = CARTESIAN_POINT ( 'NONE',  ( 1.033464566929134687, -0.06523048226347956391, 0.2829724409448821643 ) ) ;
#18097 = DIRECTION ( 'NONE',  ( 0.000000000000000000, -0.1045284632676499459, 0.9945218953682736229 ) ) ;
#18098 = CARTESIAN_POINT ( 'NONE',  ( -0.9873396505805591694, 0.1113553986120547346, 0.3986220471365669038 ) ) ;
#18099 = ORIENTED_EDGE ( 'NONE', *, *, #3053, .F. ) ;
#18100 = CARTESIAN_POINT ( 'NONE',  ( 0.9500414927467378812, -0.1787899950787401604, 1.510826771599780294 ) ) ;
#18101 = CARTESIAN_POINT ( 'NONE',  ( -1.033464566929134687, -0.06523048226347956391, 1.099901574695623108 ) ) ;
#18103 = CARTESIAN_POINT ( 'NONE',  ( 0.8759842519685039353, 0.1574803149606299191, 1.909448818897637956 ) ) ;
#18102 = CARTESIAN_POINT ( 'NONE',  ( -0.1377952755905511861, 0.1564960629921283985, -0.8070866141732283561 ) ) ;
#18104 = CARTESIAN_POINT ( 'NONE',  ( -0.7495606340400177148, -0.1264236179284866091, 0.04675196845017354913 ) ) ;
#18105 = CARTESIAN_POINT ( 'NONE',  ( -0.1264236179284866091, 0.03395669296714932950, -0.1264236179284866091 ) ) ;
#18106 = ORIENTED_EDGE ( 'NONE', *, *, #3686, .T. ) ;
#18107 = LINE ( 'NONE', #14041, #42831 ) ;
#18108 = ORIENTED_EDGE ( 'NONE', *, *, #777, .T. ) ;
#18109 = DIRECTION ( 'NONE',  ( 0.000000000000000000, 0.000000000000000000, -1.000000000000000000 ) ) ;
#18110 = CYLINDRICAL_SURFACE ( 'NONE', #46004, 0.1574803149606299191 ) ;
#18111 = ORIENTED_EDGE ( 'NONE', *, *, #18516, .T. ) ;
#18112 = CARTESIAN_POINT ( 'NONE',  ( 1.054774247047244096, 0.000000000000000000, 0.6176181101824566033 ) ) ;
#18113 = VERTEX_POINT ( 'NONE', #19130 ) ;
#18114 = CARTESIAN_POINT ( 'NONE',  ( 0.06523048226347956391, 0.07332677176107038619, 0.1574803149606297803 ) ) ;
#18115 = CARTESIAN_POINT ( 'NONE',  ( -0.6971942568897648851, 0.07405724077823318263, 1.067913385773007651 ) ) ;
#18116 = VERTEX_POINT ( 'NONE', #4746 ) ;
#18117 = CARTESIAN_POINT ( 'NONE',  ( -0.6971942568897637749, 2.189545951927499583E-17, 1.065452755851747924 ) ) ;
#18118 = CARTESIAN_POINT ( 'NONE',  ( -1.054774247047244540, -0.07405724077823318263, 0.8513779527021426707 ) ) ;
#18119 = CARTESIAN_POINT ( 'NONE',  ( 1.033464566929134687, -0.06523048226347956391, 1.818405511811023167 ) ) ;
#18120 = CARTESIAN_POINT ( 'NONE',  ( 0.1787899950787401604, -0.8209901099615228848, -0.07405724077823318263 ) ) ;
#18121 = VERTEX_POINT ( 'NONE', #30667 ) ;
#18122 = CARTESIAN_POINT ( 'NONE',  ( -0.06523048226347956391, -0.01033464556176428781, 0.1574803149606297803 ) ) ;
#18123 = CARTESIAN_POINT ( 'NONE',  ( 0.7439266621721258854, 0.1207772627896461087, 0.03937008034557057390 ) ) ;
#18124 = ORIENTED_EDGE ( 'NONE', *, *, #45815, .F. ) ;
#18125 = CARTESIAN_POINT ( 'NONE',  ( -0.8759842519685039353, -0.1574803149606299191, 1.732283464566929165 ) ) ;
#18126 = ADVANCED_FACE ( 'NONE', ( #40684 ), #12200, .T. ) ;
#18127 = DIRECTION ( 'NONE',  ( 1.000000000000000000, 0.000000000000000000, 0.000000000000000000 ) ) ;
#18128 = CARTESIAN_POINT ( 'NONE',  ( -0.8759842519685039353, 0.1787899950787401882, 0.7406496062454487328 ) ) ;
#18129 = ADVANCED_FACE ( 'NONE', ( #44283 ), #26595, .T. ) ;
#18130 = EDGE_CURVE ( 'NONE', #26779, #43256, #16778, .T. ) ;
#18131 = CARTESIAN_POINT ( 'NONE',  ( -1.054774247047244096, 0.000000000000000000, 1.838090551127338657 ) ) ;
#18132 = ORIENTED_EDGE ( 'NONE', *, *, #16320, .T. ) ;
#18133 = ( BOUNDED_CURVE ( )  B_SPLINE_CURVE ( 2, ( #25929, #7699, #22313, #40277, #18718, #15151, #37172, #969, #23034 ),
 .UNSPECIFIED., .F., .F. ) 
 B_SPLINE_CURVE_WITH_KNOTS ( ( 3, 2, 2, 2, 3 ),
 ( 0.5500000000000000444, 0.5524999999999999911, 0.5550000000000000488, 0.5574999999999999956, 0.5600000000000000533 ),
 .UNSPECIFIED. ) 
 CURVE ( )  GEOMETRIC_REPRESENTATION_ITEM ( )  RATIONAL_B_SPLINE_CURVE ( ( 1.000000000000000000, 0.9238795325112869605, 1.000000000000000000, 0.9238795325112869605, 1.000000000000000000, 0.9238795325112869605, 1.000000000000000000, 0.9238795325112869605, 1.000000000000000000 ) ) 
 REPRESENTATION_ITEM ( '' )  ) ;
#18134 = ( NAMED_UNIT ( * ) SI_UNIT ( $, .STERADIAN. ) SOLID_ANGLE_UNIT ( ) ) ;
#18135 = CARTESIAN_POINT ( 'NONE',  ( 0.7185039370078746268, -0.06523048226347956391, 0.7012795275590552047 ) ) ;
#18137 = CARTESIAN_POINT ( 'NONE',  ( -0.7382059478614877435, 0.08697056858538719515, 1.981492242426230899 ) ) ;
#18136 = CARTESIAN_POINT ( 'NONE',  ( -1.100456976456230270E-17, -0.8770123135200531550, -0.1797182628040039365 ) ) ;
#18138 = CARTESIAN_POINT ( 'NONE',  ( 0.1089815878294855545, -0.2325720113810400280, -0.3144321013757211958 ) ) ;
#18139 = CARTESIAN_POINT ( 'NONE',  ( -0.8759842519685039353, 0.1574803149606299191, 1.348425196742866206 ) ) ;
#18140 = CARTESIAN_POINT ( 'NONE',  ( 0.9500414927467378812, -0.1787899950787401604, 0.8070866141194653620 ) ) ;
#18141 = CARTESIAN_POINT ( 'NONE',  ( 1.054774247047244540, 0.07405724077823318263, 1.363188976324188673 ) ) ;
#18142 = CARTESIAN_POINT ( 'NONE',  ( 2.892866454678787531E-17, -0.6082677165354331006, 0.1574803149606299191 ) ) ;
#18143 = CARTESIAN_POINT ( 'NONE',  ( 0.3547871005709968273, 0.09842519685039370636, 0.000000000000000000 ) ) ;
#18144 = CARTESIAN_POINT ( 'NONE',  ( 2.892866454678787531E-17, 0.02165354330708661734, 0.1574803149606299191 ) ) ;
#18145 = CARTESIAN_POINT ( 'NONE',  ( 0.8759842519685039353, 0.1574803149606299191, 1.240157480314960647 ) ) ;
#18147 = CARTESIAN_POINT ( 'NONE',  ( 0.8759842519685039353, -0.1574803149606299191, 1.564960629813732185 ) ) ;
#18146 = CARTESIAN_POINT ( 'NONE',  ( 0.9972096056529755614, -0.1313310934784522044, 1.990530892258217222 ) ) ;
#18148 = CARTESIAN_POINT ( 'NONE',  ( 0.8107537697050254399, -0.1574803149606297803, 1.719980314853102321 ) ) ;
#18149 = CARTESIAN_POINT ( 'NONE',  ( 0.1574803149606300301, -0.6304133857192448787, 0.06523048226347956391 ) ) ;
#18150 = ORIENTED_EDGE ( 'NONE', *, *, #14949, .T. ) ;
#18151 = AXIS2_PLACEMENT_3D ( 'NONE', #42814, #21271, #35896 ) ;
#18153 = CARTESIAN_POINT ( 'NONE',  ( 0.1574803149606299191, 0.1473293504822035527, -0.9532488779249704836 ) ) ;
#18152 = CARTESIAN_POINT ( 'NONE',  ( 0.7495606340400177148, 0.1264236179284866091, 0.6668307086076534773 ) ) ;
#18154 = CARTESIAN_POINT ( 'NONE',  ( -0.07405724077823318263, -0.6771653542769455747, -0.1787899950787401604 ) ) ;
#18155 = DIRECTION ( 'NONE',  ( -3.469446951953614583E-15, -1.000000000000000000, -1.751623080406021339E-46 ) ) ;
#18156 = VERTEX_POINT ( 'NONE', #41147 ) ;
#18157 = CARTESIAN_POINT ( 'NONE',  ( 0.8107537697050254399, -0.1574803149606297803, 0.6176181101286931652 ) ) ;
#18158 = LINE ( 'NONE', #33276, #39710 ) ;
#18159 = CARTESIAN_POINT ( 'NONE',  ( 1.054774247047244096, 0.000000000000000000, 1.006397637741511808 ) ) ;
#18160 = DIRECTION ( 'NONE',  ( -1.000000000000000000, 0.000000000000000000, 0.000000000000000000 ) ) ;
#18161 = CARTESIAN_POINT ( 'NONE',  ( -0.1787899950787401604, -1.144685039316316599, 0.07405724077823318263 ) ) ;
#18162 = CARTESIAN_POINT ( 'NONE',  ( -0.1574803149606300301, -1.447342519685039797, -0.06523048226347956391 ) ) ;
#18163 = DIRECTION ( 'NONE',  ( 0.000000000000000000, -1.000000000000000000, 0.000000000000000000 ) ) ;
#18164 = CARTESIAN_POINT ( 'NONE',  ( -0.9500414927467378812, -0.1787899950787401604, 0.09350393695411057804 ) ) ;
#18165 = EDGE_LOOP ( 'NONE', ( #18038, #43370, #37348, #38385 ) ) ;
#18166 = CARTESIAN_POINT ( 'NONE',  ( 0.7185039370078746268, 0.06523048226347956391, 1.759350393700788162 ) ) ;
#18167 = ORIENTED_EDGE ( 'NONE', *, *, #31349, .T. ) ;
#18169 = CARTESIAN_POINT ( 'NONE',  ( -0.1264236179284866091, -1.427657480261196987, -0.1264236179284866091 ) ) ;
#18168 = CARTESIAN_POINT ( 'NONE',  ( -0.1113553986120547346, -0.3277559054042838982, 0.1113553986120547346 ) ) ;
#18170 = CARTESIAN_POINT ( 'NONE',  ( -0.1476377952755905387, -0.4075443641102559078, -0.9311509272141712534 ) ) ;
#18171 = CARTESIAN_POINT ( 'NONE',  ( -1.002407869896990045, 0.1264236179284866091, 1.641240157426551161 ) ) ;
#18172 = CARTESIAN_POINT ( 'NONE',  ( -1.002407869896990045, -0.1264236179284866091, 1.119586614119464585 ) ) ;
#18173 = CARTESIAN_POINT ( 'NONE',  ( -0.8019270111902717657, 0.1787899950787401604, 0.4330708660879683536 ) ) ;
#18174 = CARTESIAN_POINT ( 'NONE',  ( -0.7185039370078766252, -0.06523048226348168721, 1.793799212490897688 ) ) ;
#18175 = CARTESIAN_POINT ( 'NONE',  ( 0.1564216623530370054, 0.01359171937779157097, 0.1403857474671354466 ) ) ;
#18176 = CARTESIAN_POINT ( 'NONE',  ( 0.06218625040858925118, 0.08128102204192401425, -0.2495298224528492981 ) ) ;
#18177 = CARTESIAN_POINT ( 'NONE',  ( 0.6195511811023636239, 1.354170115732554747, -0.4197102375732078561 ) ) ;
#18178 = CARTESIAN_POINT ( 'NONE',  ( 0.07405724077823318263, -0.4765019209851441007, 0.1787899950787401604 ) ) ;
#18179 = CARTESIAN_POINT ( 'NONE',  ( -0.1729392868700769803, -0.09842519685039370636, -0.02639094656065850072 ) ) ;
#18180 = DIRECTION ( 'NONE',  ( 0.6018150231520440485, 0.000000000000000000, 0.7986355100472960489 ) ) ;
#18181 = LINE ( 'NONE', #36410, #14174 ) ;
#18182 = CIRCLE ( 'NONE', #45688, 0.09842519685039370636 ) ;
#18183 = CARTESIAN_POINT ( 'NONE',  ( -1.002407869896990045, -0.1264236179284866091, 0.3321850393163153226 ) ) ;
#18184 = EDGE_CURVE ( 'NONE', #39665, #39149, #4655, .T. ) ;
#18185 = VERTEX_POINT ( 'NONE', #22254 ) ;
#18186 = EDGE_LOOP ( 'NONE', ( #26826, #10784 ) ) ;
#18187 = EDGE_CURVE ( 'NONE', #23245, #45939, #45975, .T. ) ;
#18188 = CARTESIAN_POINT ( 'NONE',  ( -0.8759842519685039353, -0.1787899950787401882, 1.434547244040724534 ) ) ;
#18189 = ORIENTED_EDGE ( 'NONE', *, *, #29340, .F. ) ;
#18190 = EDGE_CURVE ( 'NONE', #19819, #9918, #28418, .T. ) ;
#18191 = CARTESIAN_POINT ( 'NONE',  ( 0.1787899950787401604, -1.203740157426551383, -0.07405724077823318263 ) ) ;
#18192 = CARTESIAN_POINT ( 'NONE',  ( -0.1787899950787401604, -1.420275590497418250, -0.07405724077823318263 ) ) ;
#18193 = PRESENTATION_STYLE_ASSIGNMENT (( #10788 ) ) ;
#18194 = DIRECTION ( 'NONE',  ( -0.9999965023344152826, -0.002644866525196000462, 7.000000000000001727E-15 ) ) ;
#18195 = CARTESIAN_POINT ( 'NONE',  ( 0.9873396505805591694, -0.1113553986120547346, 0.3986220472440945017 ) ) ;
#18196 = CARTESIAN_POINT ( 'NONE',  ( -0.1797182628040039365, -0.6309493213940688960, 0.000000000000000000 ) ) ;
#18197 = CARTESIAN_POINT ( 'NONE',  ( 0.2559055118110236116, -4.594920972184172978E-16, -0.02740704184215071032 ) ) ;
#18198 = CARTESIAN_POINT ( 'NONE',  ( -0.9873396505805591694, -0.1113553986120547346, 0.9005905510735748853 ) ) ;
#18199 = CARTESIAN_POINT ( 'NONE',  ( 0.6971942568897626646, 0.07405724077823318263, 0.4773622046706456068 ) ) ;
#18200 = CARTESIAN_POINT ( 'NONE',  ( -9.642888182262618425E-18, -0.1161417322834645688, -0.1574803149606299191 ) ) ;
#18201 = CARTESIAN_POINT ( 'NONE',  ( 0.9412147342319837628, -0.1574803149606297803, 1.803641732175937484 ) ) ;
#18202 = VERTEX_POINT ( 'NONE', #912 ) ;
#18203 = DIRECTION ( 'NONE',  ( -0.000000000000000000, -0.000000000000000000, -1.000000000000000000 ) ) ;
#18204 = CARTESIAN_POINT ( 'NONE',  ( 0.8759842519685039353, -0.1574803149606299191, 0.8267716535433071723 ) ) ;
#18205 = CARTESIAN_POINT ( 'NONE',  ( -0.1574803149606299191, -0.06692913385826770867, 0.000000000000000000 ) ) ;
#18207 = DIRECTION ( 'NONE',  ( -1.000000000000000000, 0.000000000000000000, 0.000000000000000000 ) ) ;
#18206 = DIRECTION ( 'NONE',  ( -1.000000000000000000, 0.000000000000000000, 0.000000000000000000 ) ) ;
#18208 = CARTESIAN_POINT ( 'NONE',  ( 0.9873396505805591694, -0.1113553986120547346, 0.7923228346456693272 ) ) ;
#18209 = ORIENTED_EDGE ( 'NONE', *, *, #10423, .T. ) ;
#18210 = ORIENTED_EDGE ( 'NONE', *, *, #33520, .T. ) ;
#18211 = DIRECTION ( 'NONE',  ( -1.000000000000000000, 0.000000000000000000, 0.000000000000000000 ) ) ;
#18212 = CARTESIAN_POINT ( 'NONE',  ( -0.1787899950787401604, -1.533464566875370805, 0.07405724077823318263 ) ) ;
#18213 = CARTESIAN_POINT ( 'NONE',  ( 0.06523048226347956391, -1.526082677057828629, -0.1574803149606300301 ) ) ;
#18214 = CARTESIAN_POINT ( 'NONE',  ( -0.07405724077823318263, -0.7214566928596228834, -0.1787899950787401604 ) ) ;
#18215 = CARTESIAN_POINT ( 'NONE',  ( -0.8759842519685039353, 0.1574803149606299191, 0.1673228345381423399 ) ) ;
#18217 = VECTOR ( 'NONE', #21826, 39.37007874015748143 ) ;
#18216 = CARTESIAN_POINT ( 'NONE',  ( -9.642888182262618425E-18, -0.9822834645669291653, -0.1574803149606299191 ) ) ;
#18218 = CARTESIAN_POINT ( 'NONE',  ( 0.8107537697050253289, -0.1574803149606297803, 1.011318897530268712 ) ) ;
#18219 = CARTESIAN_POINT ( 'NONE',  ( -0.8019270111902717657, -0.1787899950787401604, 0.3641732282926931630 ) ) ;
#18220 = ORIENTED_EDGE ( 'NONE', *, *, #4160, .T. ) ;
#18221 = VERTEX_POINT ( 'NONE', #30212 ) ;
#18222 = EDGE_LOOP ( 'NONE', ( #33127, #14097, #31290, #38921 ) ) ;
#18223 = CARTESIAN_POINT ( 'NONE',  ( -1.002407869896990045, 0.1264236179284866091, 1.646161417269070837 ) ) ;
#18224 = ORIENTED_EDGE ( 'NONE', *, *, #6091, .F. ) ;
#18225 = CARTESIAN_POINT ( 'NONE',  ( 0.9500414927467378812, -0.1787899950787401604, 1.594488188922613237 ) ) ;
#18226 = ORIENTED_EDGE ( 'NONE', *, *, #11343, .T. ) ;
#18227 = CARTESIAN_POINT ( 'NONE',  ( -0.8019270111902717657, 0.1787899950787401604, 0.8267716534895444003 ) ) ;
#18228 = CARTESIAN_POINT ( 'NONE',  ( -1.002407869896990045, -0.1264236179284866091, 0.7258858267178898149 ) ) ;
#18229 = LINE ( 'NONE', #14408, #12380 ) ;
#18230 = DIRECTION ( 'NONE',  ( 1.000000000000000000, 0.000000000000000000, 0.000000000000000000 ) ) ;
#18231 = CARTESIAN_POINT ( 'NONE',  ( -1.002407869896990045, 0.1264236179284866091, 1.528051181048598384 ) ) ;
#18232 = CARTESIAN_POINT ( 'NONE',  ( -0.9412147342319837628, -0.1574803149606297803, 1.961122047136568014 ) ) ;
#18233 = ORIENTED_EDGE ( 'NONE', *, *, #27301, .T. ) ;
#18234 = CARTESIAN_POINT ( 'NONE',  ( 1.033464566929133799, 0.000000000000000000, 0.9842519683964094934 ) ) ;
#18235 = CARTESIAN_POINT ( 'NONE',  ( 0.6971942568897637749, 2.189545951927499583E-17, 1.503444881836000002 ) ) ;
#18236 = CARTESIAN_POINT ( 'NONE',  ( 0.1577183631698106381, -0.09851384455655413930, -0.1232999193531017779 ) ) ;
#18237 = CARTESIAN_POINT ( 'NONE',  ( 0.000000000000000000, 0.000000000000000000, -0.05390369169704170571 ) ) ;
#18238 = ORIENTED_EDGE ( 'NONE', *, *, #12367, .F. ) ;
#18239 = EDGE_CURVE ( 'NONE', #2020, #7195, #11975, .T. ) ;
#18240 = CIRCLE ( 'NONE', #16707, 0.7874015748031496509 ) ;
#18241 = VERTEX_POINT ( 'NONE', #2564 ) ;
#18242 = VERTEX_POINT ( 'NONE', #9784 ) ;
#18243 = EDGE_CURVE ( 'NONE', #28708, #45599, #34532, .T. ) ;
#18244 = LINE ( 'NONE', #6982, #46036 ) ;
#18245 = CIRCLE ( 'NONE', #25124, 0.09842519685039370636 ) ;
#18246 = CARTESIAN_POINT ( 'NONE',  ( 0.1787899950787401604, -0.3818897637257640532, 0.07405724077823318263 ) ) ;
#18247 = CARTESIAN_POINT ( 'NONE',  ( -0.1787899950787401604, -0.9084645668753701386, -0.07405724077823318263 ) ) ;
#18248 = DIRECTION ( 'NONE',  ( 4.272009658007763174E-15, -0.6156614753256599570, -0.7880107536067207930 ) ) ;
#18249 = LINE ( 'NONE', #14659, #267 ) ;
#18250 = CARTESIAN_POINT ( 'NONE',  ( 0.8019270111902717657, 0.1787899950787401604, 1.766732283410803461 ) ) ;
#18251 = CARTESIAN_POINT ( 'NONE',  ( 0.7185039370078746268, 0.06523048226347956391, 0.3026574803149607029 ) ) ;
#18252 = CARTESIAN_POINT ( 'NONE',  ( 0.07444174185955065859, -0.2249453843861952684, 0.1797182628040039087 ) ) ;
#18253 = CARTESIAN_POINT ( 'NONE',  ( 3.284318927891251994E-17, -0.08526176350482933541, 0.1787899950787401882 ) ) ;
#18254 = CARTESIAN_POINT ( 'NONE',  ( -0.1787899950787401882, -0.2367125983714334636, 0.000000000000000000 ) ) ;
#18255 = CARTESIAN_POINT ( 'NONE',  ( 0.1787899950787401604, -0.06200787396198446239, -0.07405724077823318263 ) ) ;
#18256 = DIRECTION ( 'NONE',  ( -0.000000000000000000, 0.9771240687918548717, 0.2126700594527834720 ) ) ;
#18257 = CARTESIAN_POINT ( 'NONE',  ( 1.002407869896990045, -0.1264236179284866091, 0.6077755904974173617 ) ) ;
#18258 = CARTESIAN_POINT ( 'NONE',  ( -0.8206535098617165902, 0.1696709502983688167, 0.03937007874015842346 ) ) ;
#18259 = CARTESIAN_POINT ( 'NONE',  ( 0.1574803149606300023, 0.06245656531175268478, -0.1492449156640648089 ) ) ;
#18260 = CARTESIAN_POINT ( 'NONE',  ( -0.9412147342319837628, 0.1574803149606300301, 1.306594488081449290 ) ) ;
#18261 = CARTESIAN_POINT ( 'NONE',  ( 0.6971942568897648851, -0.07405724077823297447, 1.742125984198204858 ) ) ;
#18263 = CARTESIAN_POINT ( 'NONE',  ( 0.9873396505805591694, 0.1113553986120547346, 0.1230314959554651699 ) ) ;
#18262 = CARTESIAN_POINT ( 'NONE',  ( -0.1435836963511328279, -0.09660391682274867275, 0.2025327002559215717 ) ) ;
#18264 = CARTESIAN_POINT ( 'NONE',  ( 0.8759842519685039353, -0.1787899950787401882, 0.4847440944344252323 ) ) ;
#18265 = ORIENTED_EDGE ( 'NONE', *, *, #47268, .T. ) ;
#18266 = CARTESIAN_POINT ( 'NONE',  ( 0.4934383202099732468, -0.08090551181102362266, 1.098083891755157578E-17 ) ) ;
#18267 = CARTESIAN_POINT ( 'NONE',  ( -0.1574803149606299191, 1.928577636452524610E-17, -0.3149606299212598381 ) ) ;
#18268 = CARTESIAN_POINT ( 'NONE',  ( -0.07405724077823318263, -0.2736220471903310081, 0.1787899950787401604 ) ) ;
#18270 = CARTESIAN_POINT ( 'NONE',  ( 0.1618536817989107979, 0.08807120157702044705, 0.1284887221114194289 ) ) ;
#18269 = CARTESIAN_POINT ( 'NONE',  ( -0.6971942568897637749, 2.189545951927499583E-17, 0.4010826771115905687 ) ) ;
#18271 = EDGE_CURVE ( 'NONE', #18481, #3331, #29825, .T. ) ;
#18272 = CARTESIAN_POINT ( 'NONE',  ( -0.1787899950787401604, -1.026574803095842370, -0.07405724077823318263 ) ) ;
#18273 = CARTESIAN_POINT ( 'NONE',  ( 0.8759842519685039353, -0.1787899950787401882, 0.09596456687537047170 ) ) ;
#18274 = CARTESIAN_POINT ( 'NONE',  ( 1.284448818897637956, -0.3937007874015748254, -1.181102362204724310 ) ) ;
#18275 = VECTOR ( 'NONE', #39631, 39.37007874015748143 ) ;
#18276 = CARTESIAN_POINT ( 'NONE',  ( -0.7495606340400177148, 0.1264236179284866091, 1.651082677111590513 ) ) ;
#18277 = ORIENTED_EDGE ( 'NONE', *, *, #10353, .T. ) ;
#18278 = CARTESIAN_POINT ( 'NONE',  ( -0.6971942568897648851, -0.07405724077823297447, 1.112204724355684959 ) ) ;
#18279 = CARTESIAN_POINT ( 'NONE',  ( 1.033464566929133799, 0.000000000000000000, 1.033464566929133799 ) ) ;
#18280 = AXIS2_PLACEMENT_3D ( 'NONE', #31606, #28237, #13598 ) ;
#18281 = CARTESIAN_POINT ( 'NONE',  ( 0.6971942568897637749, 2.189545951927499583E-17, 1.149114173174582643 ) ) ;
#18282 = CARTESIAN_POINT ( 'NONE',  ( 1.002407869896990045, -0.1264236179284866091, 1.867618110182456714 ) ) ;
#18283 = CARTESIAN_POINT ( 'NONE',  ( -1.033464566929134687, -0.06523048226347956391, 0.6373031496062994128 ) ) ;
#18284 = CARTESIAN_POINT ( 'NONE',  ( -0.9500414927467378812, -0.1787899950787401604, 1.117125984198206412 ) ) ;
#18285 = CARTESIAN_POINT ( 'NONE',  ( 0.1594510458733990610, 0.09722652869638431783, -0.1125335630252820018 ) ) ;
#18286 = CARTESIAN_POINT ( 'NONE',  ( -0.1541343738003721486, -0.2065047100573886574, -0.03112915705354596732 ) ) ;
#18287 = CARTESIAN_POINT ( 'NONE',  ( 0.6971942568897637749, 2.189545951927499583E-17, 0.2829724408911185041 ) ) ;
#18288 = CARTESIAN_POINT ( 'NONE',  ( -0.8759842519685039353, 0.1787899950787401882, 0.3075787401037169411 ) ) ;
#18289 = PRODUCT_DEFINITION_CONTEXT ( 'detailed design', #37634, 'design' ) ;
#18290 = CARTESIAN_POINT ( 'NONE',  ( -1.054774247047244096, 0.000000000000000000, 0.7308070865604093802 ) ) ;
#18291 = ORIENTED_EDGE ( 'NONE', *, *, #25596, .T. ) ;
#18292 = CIRCLE ( 'NONE', #26718, 0.1003937007874010356 ) ;
#18293 = CARTESIAN_POINT ( 'NONE',  ( -1.094772975963752103E-17, 0.06348425202226751218, -0.1787899950787401882 ) ) ;
#18294 = CARTESIAN_POINT ( 'NONE',  ( 0.6971942568897626646, -0.07405724077823297447, 0.7185039369541108556 ) ) ;
#18295 = CARTESIAN_POINT ( 'NONE',  ( 0.8019270111902716547, -0.1787899950787401604, 1.038385826717890259 ) ) ;
#18296 = CARTESIAN_POINT ( 'NONE',  ( -0.7495606340400177148, 0.1264236179284866091, 1.926673228292693052 ) ) ;
#18297 = CARTESIAN_POINT ( 'NONE',  ( 1.002407869896990045, 0.1264236179284866091, 1.956200787347811110 ) ) ;
#18298 = EDGE_CURVE ( 'NONE', #32711, #37242, #13869, .T. ) ;
#18299 = ORIENTED_EDGE ( 'NONE', *, *, #20943, .F. ) ;
#18300 = EDGE_CURVE ( 'NONE', #41049, #46340, #20551, .T. ) ;
#18301 = CARTESIAN_POINT ( 'NONE',  ( 0.1264236179284866091, -1.261442865867033580, 0.1264236179284866091 ) ) ;
#18302 = ORIENTED_EDGE ( 'NONE', *, *, #10183, .T. ) ;
#18303 = CARTESIAN_POINT ( 'NONE',  ( -0.1787899950787401604, -0.3523622046706461619, 0.07405724077823318263 ) ) ;
#18304 = CARTESIAN_POINT ( 'NONE',  ( -0.1574803149606299191, 0.5323553679591567223, -0.7566348232351032266 ) ) ;
#18305 = ORIENTED_EDGE ( 'NONE', *, *, #40646, .F. ) ;
#18306 = CARTESIAN_POINT ( 'NONE',  ( 1.054774247047244096, 0.000000000000000000, 1.163877952702141672 ) ) ;
#18307 = EDGE_CURVE ( 'NONE', #40880, #19150, #31604, .T. ) ;
#18308 = CARTESIAN_POINT ( 'NONE',  ( 0.2559055118110236116, 0.1477471161312027548, -0.3149606299212598381 ) ) ;
#18309 = CARTESIAN_POINT ( 'NONE',  ( 0.1574803149606299746, -0.9875035750853327077, -1.463737590216208861 ) ) ;
#18310 = ( BOUNDED_CURVE ( )  B_SPLINE_CURVE ( 2, ( #37641, #35006, #4795, #42154, #19422, #15858, #23984, #30481, #45040 ),
 .UNSPECIFIED., .F., .F. ) 
 B_SPLINE_CURVE_WITH_KNOTS ( ( 3, 2, 2, 2, 3 ),
 ( 0.6400000000000000133, 0.6424999999999999600, 0.6450000000000000178, 0.6474999999999999645, 0.6500000000000000222 ),
 .UNSPECIFIED. ) 
 CURVE ( )  GEOMETRIC_REPRESENTATION_ITEM ( )  RATIONAL_B_SPLINE_CURVE ( ( 1.000000000000000000, 0.9238795325112869605, 1.000000000000000000, 0.9238795325112869605, 1.000000000000000000, 0.9238795325112869605, 1.000000000000000000, 0.9238795325112869605, 1.000000000000000000 ) ) 
 REPRESENTATION_ITEM ( '' )  ) ;
#18311 = CARTESIAN_POINT ( 'NONE',  ( 1.002407869896990045, 0.1264236179284866091, 1.523129921206078707 ) ) ;
#18312 = CARTESIAN_POINT ( 'NONE',  ( 1.054774247047244540, 0.07405724077823318263, 0.02460629915883492599 ) ) ;
#18313 = CARTESIAN_POINT ( 'NONE',  ( -0.07405724077823318263, -1.690944881836001334, 0.1787899950787401604 ) ) ;
#18314 = CARTESIAN_POINT ( 'NONE',  ( 0.1787899950787401604, -1.631889763725764553, -0.07405724077823318263 ) ) ;
#18315 = CIRCLE ( 'NONE', #45074, 0.1864803149606299448 ) ;
#18316 = CARTESIAN_POINT ( 'NONE',  ( -0.6971942568897637749, 2.189545951927499583E-17, 0.5585629920722204877 ) ) ;
#18317 = DIRECTION ( 'NONE',  ( -1.000000000000000000, 0.000000000000000000, 7.155734338404321376E-15 ) ) ;
#18319 = CARTESIAN_POINT ( 'NONE',  ( -0.7098384388722608351, -0.01069464109018706914, 1.983455518814613017 ) ) ;
#18318 = CARTESIAN_POINT ( 'NONE',  ( 0.1797182628040039365, -1.319925699346824688, -2.200913952912460540E-17 ) ) ;
#18320 = DIRECTION ( 'NONE',  ( -5.159318851433079625E-16, -0.6156614753256609562, -0.7880107536067197938 ) ) ;
#18321 = CARTESIAN_POINT ( 'NONE',  ( 0.8759842519685039353, 0.1787899950787401882, 1.218011810969858111 ) ) ;
#18322 = VECTOR ( 'NONE', #27027, 39.37007874015748143 ) ;
#18323 = CARTESIAN_POINT ( 'NONE',  ( 0.8019270111902716547, -0.1787899950787401604, 1.742125984198204858 ) ) ;
#18324 = CARTESIAN_POINT ( 'NONE',  ( 0.8107537697050254399, 0.1574803149606300301, 1.508366141624757129 ) ) ;
#18325 = CARTESIAN_POINT ( 'NONE',  ( 0.1574803149606300023, 1.126631386849004990, -3.440787370833234160 ) ) ;
#18326 = LINE ( 'NONE', #85, #16672 ) ;
#18327 = DIRECTION ( 'NONE',  ( 1.822029033848725028E-16, 0.000000000000000000, 1.000000000000000000 ) ) ;
#18328 = CARTESIAN_POINT ( 'NONE',  ( -0.9873396505805591694, -0.1113553986120547346, 1.934055118110236338 ) ) ;
#18329 = DIRECTION ( 'NONE',  ( -1.000000000000000000, 0.000000000000000000, 0.000000000000000000 ) ) ;
#18330 = CARTESIAN_POINT ( 'NONE',  ( 1.054774247047244540, 0.07405724077823318263, 0.1427165353793072855 ) ) ;
#18331 = LINE ( 'NONE', #29640, #23898 ) ;
#18332 = DIRECTION ( 'NONE',  ( 0.000000000000000000, 0.000000000000000000, -1.000000000000000000 ) ) ;
#18333 = CARTESIAN_POINT ( 'NONE',  ( 1.181102362204724310, -0.3937007874015748254, -0.9842519685039370358 ) ) ;
#18334 = CARTESIAN_POINT ( 'NONE',  ( -0.9500414927467378812, 0.1787899950787401604, 1.171259842465921741 ) ) ;
#18335 = CARTESIAN_POINT ( 'NONE',  ( 0.8759842519685039353, 0.1574803149606299191, 0.7185039369003465293 ) ) ;
#18336 = ORIENTED_EDGE ( 'NONE', *, *, #4698, .F. ) ;
#18337 = CARTESIAN_POINT ( 'NONE',  ( -0.7185039370078714072, 0.06523048226347728795, 1.129429133858268708 ) ) ;
#18338 = CARTESIAN_POINT ( 'NONE',  ( -0.8107537697050253289, 0.1574803149606300301, 0.4060039369003469734 ) ) ;
#18339 = CARTESIAN_POINT ( 'NONE',  ( 7.155189876034614158E-05, 0.006740216713035995962, 0.1377954718200116446 ) ) ;
#18340 = CARTESIAN_POINT ( 'NONE',  ( 1.054774247047244096, 0.000000000000000000, 1.478838582623401399 ) ) ;
#18342 = CARTESIAN_POINT ( 'NONE',  ( -0.1377952755905511861, 0.1574803149606320007, -0.8070866141732283561 ) ) ;
#18341 = DIRECTION ( 'NONE',  ( 1.822029033848725028E-16, 0.000000000000000000, 1.000000000000000000 ) ) ;
#18343 = CARTESIAN_POINT ( 'NONE',  ( 0.07405724077823318263, -0.2096456692375751329, -0.1787899950787401604 ) ) ;
#18344 = ORIENTED_EDGE ( 'NONE', *, *, #2264, .F. ) ;
#18345 = DIRECTION ( 'NONE',  ( -1.000000000000000000, 0.000000000000000000, 0.000000000000000000 ) ) ;
#18346 = AXIS2_PLACEMENT_3D ( 'NONE', #37405, #22563, #44823 ) ;
#18347 = CARTESIAN_POINT ( 'NONE',  ( 1.002407869896990045, 0.1264236179284866091, 0.6619094487651338010 ) ) ;
#18348 = EDGE_CURVE ( 'NONE', #12211, #25679, #44454, .T. ) ;
#18349 = VERTEX_POINT ( 'NONE', #38537 ) ;
#18350 = CARTESIAN_POINT ( 'NONE',  ( 0.1113553986120547346, 0.04625984262721204859, -0.1113553986120547346 ) ) ;
#18351 = CARTESIAN_POINT ( 'NONE',  ( -0.8019270111902717657, 0.1787899950787401604, 1.102362204670646495 ) ) ;
#18352 = ORIENTED_EDGE ( 'NONE', *, *, #2428, .T. ) ;
#18353 = CARTESIAN_POINT ( 'NONE',  ( 0.7185039370078714072, 0.06523048226347728795, 1.316437007766489531 ) ) ;
#18354 = CIRCLE ( 'NONE', #26027, 0.1013779527559055538 ) ;
#18355 = CARTESIAN_POINT ( 'NONE',  ( -0.8019270111902717657, 0.1787899950787401604, 0.7874015747493863238 ) ) ;
#18356 = EDGE_CURVE ( 'NONE', #20344, #39970, #5376, .T. ) ;
#18357 = CARTESIAN_POINT ( 'NONE',  ( -0.9500414927467378812, 0.1787899950787401604, 0.2706692912848194243 ) ) ;
#18358 = CARTESIAN_POINT ( 'NONE',  ( 0.000000000000000000, 0.1193342091828950846, -0.06889763779527559306 ) ) ;
#18359 = DIRECTION ( 'NONE',  ( 1.000000000000000000, 0.000000000000000000, 0.000000000000000000 ) ) ;
#18360 = CARTESIAN_POINT ( 'NONE',  ( 0.1264236179284866091, -0.8185294800402619364, -0.1264236179284866091 ) ) ;
#18361 = VERTEX_POINT ( 'NONE', #46185 ) ;
#18362 = AXIS2_PLACEMENT_3D ( 'NONE', #17870, #25309, #17162 ) ;
#18363 = CARTESIAN_POINT ( 'NONE',  ( -1.033464566929134687, -0.06523048226347956391, 0.8636811022546768690 ) ) ;
#18364 = ORIENTED_EDGE ( 'NONE', *, *, #40725, .F. ) ;
#18365 = FACE_OUTER_BOUND ( 'NONE', #43902, .T. ) ;
#18366 = CARTESIAN_POINT ( 'NONE',  ( -0.6971942568897637749, 2.189545951927499583E-17, 0.7898622046706456068 ) ) ;
#18367 = ORIENTED_EDGE ( 'NONE', *, *, #20066, .F. ) ;
#18368 = EDGE_CURVE ( 'NONE', #34914, #36844, #16734, .T. ) ;
#18369 = PRODUCT_DEFINITION ( 'UNKNOWN', '', #37747, #14462 ) ;
#18370 = CARTESIAN_POINT ( 'NONE',  ( -0.7495606340400177148, -0.1264236179284866091, 1.862696850339937038 ) ) ;
#18371 = CARTESIAN_POINT ( 'NONE',  ( 0.1787899950787401604, -0.4999999999462365619, 0.07405724077823318263 ) ) ;
#18372 = ORIENTED_EDGE ( 'NONE', *, *, #36382, .F. ) ;
#18373 = CARTESIAN_POINT ( 'NONE',  ( 1.033464566929134687, -0.06523048226347956391, 0.6766732283464570452 ) ) ;
#18374 = CARTESIAN_POINT ( 'NONE',  ( -0.1270800023317771588, -0.8228784552523366047, 0.1270800023317771588 ) ) ;
#18375 = CARTESIAN_POINT ( 'NONE',  ( 0.3551574803149606385, 8.783380181941220341E-34, 0.000000000000000000 ) ) ;
#18376 = CARTESIAN_POINT ( 'NONE',  ( -0.7646288533564489232, 0.1113553986120547346, 1.510826771546015523 ) ) ;
#18377 = CARTESIAN_POINT ( 'NONE',  ( 0.9500414927467378812, 0.1787899950787401604, 0.8218503936470251681 ) ) ;
#18378 = CARTESIAN_POINT ( 'NONE',  ( 0.8759842519685039353, 0.1574803149606299191, 0.1673228345381423399 ) ) ;
#18379 = CARTESIAN_POINT ( 'NONE',  ( 0.7185039370078739607, 1.928577636452523993E-17, 1.486220472440944906 ) ) ;
#18381 = DIRECTION ( 'NONE',  ( -0.5735764363510518216, -0.8191520442889876907, 0.000000000000000000 ) ) ;
#18380 = CARTESIAN_POINT ( 'NONE',  ( 0.9431103146933020875, -0.1634063081578735477, 1.989410936682964870 ) ) ;
#18382 = CIRCLE ( 'NONE', #45148, 0.1968503937007874127 ) ;
#18383 = CARTESIAN_POINT ( 'NONE',  ( 0.7646288533564489232, -0.1113553986120547346, 1.717519684931842594 ) ) ;
#18384 = CARTESIAN_POINT ( 'NONE',  ( -0.06523048226347956391, -0.6156496061916855167, -0.1574803149606300301 ) ) ;
#18385 = VERTEX_POINT ( 'NONE', #5467 ) ;
#18386 = CARTESIAN_POINT ( 'NONE',  ( 0.8019270111902716547, -0.1787899950787401604, 0.7578740156942688211 ) ) ;
#18387 = CARTESIAN_POINT ( 'NONE',  ( -0.1787899950787401882, -0.8272637794737952577, 0.000000000000000000 ) ) ;
#18388 = CARTESIAN_POINT ( 'NONE',  ( -0.7185039370078739607, 1.928577636452523993E-17, 0.3740157479239689664 ) ) ;
#18389 = ORIENTED_EDGE ( 'NONE', *, *, #25778, .T. ) ;
#18390 = B_SPLINE_CURVE_WITH_KNOTS ( 'NONE', 3,
 ( #33111, #10823, #11059, #28814, #7668, #25900, #25437, #33346, #14639, #26140, #7207, #32871, #21830, #36456 ),
 .UNSPECIFIED., .F., .F.,
 ( 4, 2, 2, 2, 2, 2, 4 ),
 ( 0.000000000000000000, 0.1249999999999997780, 0.2499999999999995559, 0.3749999999999993339, 0.4374999999999992228, 0.4999999999999991118, 1.000000000000000000 ),
 .UNSPECIFIED. ) ;
#18391 = CARTESIAN_POINT ( 'NONE',  ( 0.7185039370078739607, 0.000000000000000000, 4.498031496062992574 ) ) ;
#18392 = CARTESIAN_POINT ( 'NONE',  ( 1.054774247047244096, 0.000000000000000000, 0.9276574802611967652 ) ) ;
#18393 = ADVANCED_FACE ( 'NONE', ( #24394 ), #20082, .T. ) ;
#18394 = DIRECTION ( 'NONE',  ( -1.000000000000000000, 0.000000000000000000, 0.000000000000000000 ) ) ;
#18395 = CARTESIAN_POINT ( 'NONE',  ( 0.1113553986120547346, -1.626968503937007871, 0.1113553986120547346 ) ) ;
#18396 = DIRECTION ( 'NONE',  ( 1.000000000000000000, 0.000000000000000000, 0.000000000000000000 ) ) ;
#18397 = CARTESIAN_POINT ( 'NONE',  ( -0.1574803149606299191, 0.4954925676037022497, -0.4875697200146963950 ) ) ;
#18398 = CARTESIAN_POINT ( 'NONE',  ( -0.8759842519685039353, -0.1787899950787401882, 0.09104330703285078152 ) ) ;
#18399 = EDGE_CURVE ( 'NONE', #31524, #8209, #27072, .T. ) ;
#18400 = CARTESIAN_POINT ( 'NONE',  ( 0.06523048226347977208, 0.1028543307086613318, 0.1574803149606297803 ) ) ;
#18401 = CARTESIAN_POINT ( 'NONE',  ( -1.054774247047244540, 0.07405724077823318263, 1.678149606245448622 ) ) ;
#18402 = ORIENTED_EDGE ( 'NONE', *, *, #18930, .T. ) ;
#18403 = CARTESIAN_POINT ( 'NONE',  ( -0.6971942568897626646, -0.07405724077823297447, 0.4429133857730075952 ) ) ;
#18404 = CARTESIAN_POINT ( 'NONE',  ( -1.284448818897637956, -0.3937007874015748254, 1.181102362204724310 ) ) ;
#18405 = CARTESIAN_POINT ( 'NONE',  ( -1.054774247047244096, 0.000000000000000000, 1.995570866087968520 ) ) ;
#18406 = CARTESIAN_POINT ( 'NONE',  ( 0.7185039370078746268, 0.06523048226347956391, 0.3026574803149607029 ) ) ;
#18407 = CARTESIAN_POINT ( 'NONE',  ( 0.7495606340400177148, -0.1264236179284866091, 0.04675196845017354913 ) ) ;
#18408 = CYLINDRICAL_SURFACE ( 'NONE', #17522, 0.1003937007874011050 ) ;
#18409 = CARTESIAN_POINT ( 'NONE',  ( 0.1787899950787401882, -0.3903798737410496544, -2.189545951927503898E-17 ) ) ;
#18410 = CARTESIAN_POINT ( 'NONE',  ( -0.1674188814857066887, -0.09842519685039370636, 0.03545433526083362208 ) ) ;
#18411 = CARTESIAN_POINT ( 'NONE',  ( 0.3161444924769519216, 1.488499961090669288, -0.3513258257898460579 ) ) ;
#18412 = CIRCLE ( 'NONE', #32979, 0.2007874015748031815 ) ;
#18413 = AXIS2_PLACEMENT_3D ( 'NONE', #13284, #27915, #27687 ) ;
#18414 = CARTESIAN_POINT ( 'NONE',  ( -0.9500414927467378812, -0.1787899950787401604, 0.3690944881352128393 ) ) ;
#18415 = ( BOUNDED_CURVE ( )  B_SPLINE_CURVE ( 2, ( #24037, #27422, #41731, #38163, #5324, #41965, #19944, #16378, #9653 ),
 .UNSPECIFIED., .F., .F. ) 
 B_SPLINE_CURVE_WITH_KNOTS ( ( 3, 2, 2, 2, 3 ),
 ( 0.9399999999999999467, 0.9425000000000000044, 0.9449999999999999512, 0.9475000000000000089, 0.9499999999999999556 ),
 .UNSPECIFIED. ) 
 CURVE ( )  GEOMETRIC_REPRESENTATION_ITEM ( )  RATIONAL_B_SPLINE_CURVE ( ( 1.000000000000000000, 0.9238795325112899581, 1.000000000000000000, 0.9238795325112869605, 1.000000000000000000, 0.9238795325112869605, 1.000000000000000000, 0.9238795325112829637, 1.000000000000000000 ) ) 
 REPRESENTATION_ITEM ( '' )  ) ;
#18416 = ORIENTED_EDGE ( 'NONE', *, *, #21157, .F. ) ;
#18417 = CARTESIAN_POINT ( 'NONE',  ( -0.8759842519685039353, -0.1787899950787401882, 1.316437007820252081 ) ) ;
#18418 = EDGE_LOOP ( 'NONE', ( #42036, #37758, #15493, #12984 ) ) ;
#18419 = CARTESIAN_POINT ( 'NONE',  ( 0.1264236179284866091, -1.353838582623401621, -0.1264236179284866091 ) ) ;
#18420 = CARTESIAN_POINT ( 'NONE',  ( 0.7646288533564489232, -0.1113553986120547346, 0.3887795275590551491 ) ) ;
#18421 = CARTESIAN_POINT ( 'NONE',  ( 0.07444174185955065859, -0.5792760930476124059, 0.1797182628040039087 ) ) ;
#18422 = CARTESIAN_POINT ( 'NONE',  ( 0.1377952755905511861, 0.1574803149606299191, 0.9074803149606294195 ) ) ;
#18423 = CARTESIAN_POINT ( 'NONE',  ( -0.9412147342319837628, -0.1574803149606297803, 1.094980314853103653 ) ) ;
#18424 = CARTESIAN_POINT ( 'NONE',  ( -0.06523048226347956391, -0.3105314960629923515, -0.1574803149606300301 ) ) ;
#18425 = CARTESIAN_POINT ( 'NONE',  ( 0.9873396505805591694, 0.1113553986120547346, 1.934055118002708573 ) ) ;
#18426 = DIRECTION ( 'NONE',  ( 0.000000000000000000, 1.000000000000000000, 0.000000000000000000 ) ) ;
#18427 = CARTESIAN_POINT ( 'NONE',  ( 0.7646288533564489232, -0.1113553986120547346, 0.9793307086614173596 ) ) ;
#18428 = CARTESIAN_POINT ( 'NONE',  ( 0.5057057357416000487, 4.766607801171850497E-17, 0.000000000000000000 ) ) ;
#18429 = CARTESIAN_POINT ( 'NONE',  ( 0.1640396990260823695, -0.08075828909096639807, -0.1398798884322421388 ) ) ;
#18430 = DIRECTION ( 'NONE',  ( 0.000000000000000000, 0.000000000000000000, 1.000000000000000000 ) ) ;
#18431 = ( BOUNDED_CURVE ( )  B_SPLINE_CURVE ( 2, ( #4116, #8182, #21882, #985, #40295, #285, #32921, #18737, #33395 ),
 .UNSPECIFIED., .F., .F. ) 
 B_SPLINE_CURVE_WITH_KNOTS ( ( 3, 2, 2, 2, 3 ),
 ( 0.1600000000000000033, 0.1625000000000000056, 0.1650000000000000078, 0.1675000000000000100, 0.1700000000000000122 ),
 .UNSPECIFIED. ) 
 CURVE ( )  GEOMETRIC_REPRESENTATION_ITEM ( )  RATIONAL_B_SPLINE_CURVE ( ( 1.000000000000000000, 0.9238795325112869605, 1.000000000000000000, 0.9238795325112869605, 1.000000000000000000, 0.9238795325112869605, 1.000000000000000000, 0.9238795325112869605, 1.000000000000000000 ) ) 
 REPRESENTATION_ITEM ( '' )  ) ;
#18433 = CARTESIAN_POINT ( 'NONE',  ( 1.033464566929134687, -0.06523048226347956391, 1.542814960629921073 ) ) ;
#18432 = CARTESIAN_POINT ( 'NONE',  ( 0.2395294000716134131, 0.000000000000000000, 0.7086614173228350522 ) ) ;
#18434 = CARTESIAN_POINT ( 'NONE',  ( 0.1574803149606300023, 3.616083068348478250E-17, 0.2952755905511806334 ) ) ;
#18436 = CARTESIAN_POINT ( 'NONE',  ( -0.2896200801440090289, 0.1109568837733816149, 1.001682203372160851 ) ) ;
#18435 = AXIS2_PLACEMENT_3D ( 'NONE', #16701, #34441, #42542 ) ;
#18437 = ORIENTED_EDGE ( 'NONE', *, *, #31349, .F. ) ;
#18438 = EDGE_CURVE ( 'NONE', #28768, #7920, #4676, .T. ) ;
#18439 = CYLINDRICAL_SURFACE ( 'NONE', #46294, 0.1574803149606299191 ) ;
#18440 = CARTESIAN_POINT ( 'NONE',  ( 0.3547871005709968273, -3.032960542342102697E-32, 0.09842519685039370636 ) ) ;
#18441 = CARTESIAN_POINT ( 'NONE',  ( -0.1264236179284866091, -1.570374015694267600, 0.1264236179284866091 ) ) ;
#18442 = CARTESIAN_POINT ( 'NONE',  ( 0.1574803149606299191, -1.454724409341291436, -1.928577636452523993E-17 ) ) ;
#18443 = CARTESIAN_POINT ( 'NONE',  ( -0.1787899950787401604, -0.6722440944344262315, 0.07405724077823318263 ) ) ;
#18444 = CARTESIAN_POINT ( 'NONE',  ( -0.9412147342319837628, 0.1574803149606300301, 0.08612204713656734789 ) ) ;
#18445 = AXIS2_PLACEMENT_3D ( 'NONE', #46950, #18203, #28785 ) ;
#18446 = CARTESIAN_POINT ( 'NONE',  ( 0.1113553986120547346, -1.075787401574803015, 0.1113553986120547346 ) ) ;
#18447 = CARTESIAN_POINT ( 'NONE',  ( 0.9873396505805591694, 0.1113553986120547346, 0.9104330707586141269 ) ) ;
#18448 = ADVANCED_FACE ( 'NONE', ( #41620, #8829 ), #45702, .F. ) ;
#18449 = CARTESIAN_POINT ( 'NONE',  ( -0.8019270111902717657, 0.1787899950787401604, 0.3494094487651343006 ) ) ;
#18450 = VERTEX_POINT ( 'NONE', #12920 ) ;
#18451 = ORIENTED_EDGE ( 'NONE', *, *, #25927, .F. ) ;
#18452 = VERTEX_POINT ( 'NONE', #20784 ) ;
#18453 = CARTESIAN_POINT ( 'NONE',  ( -0.8759842519685039353, 0.1787899950787401882, 1.611712598371433103 ) ) ;
#18454 = EDGE_CURVE ( 'NONE', #35946, #24004, #36775, .T. ) ;
#18455 = CARTESIAN_POINT ( 'NONE',  ( 1.054774247047244540, 0.07405724077823318263, 1.683070866087970074 ) ) ;
#18456 = CARTESIAN_POINT ( 'NONE',  ( 0.1574803149606299191, -1.336614173120818760, -1.928577636452523993E-17 ) ) ;
#18457 = CARTESIAN_POINT ( 'NONE',  ( -0.7495606340400177148, 0.1264236179284866091, 0.8686023621509606496 ) ) ;
#18458 = CARTESIAN_POINT ( 'NONE',  ( 0.9500414927467378812, -0.1787899950787401604, 0.3346456692375748831 ) ) ;
#18459 = EDGE_CURVE ( 'NONE', #19657, #34936, #25096, .T. ) ;
#18460 = CARTESIAN_POINT ( 'NONE',  ( -0.7495606340400177148, -0.1264236179284866091, 1.306594488135212728 ) ) ;
#18461 = CARTESIAN_POINT ( 'NONE',  ( -1.002407869896990045, 0.1264236179284866091, 0.7357283464029290565 ) ) ;
#18462 = CARTESIAN_POINT ( 'NONE',  ( 0.1574803149606299191, -0.07677165343578011558, -1.928577636452523993E-17 ) ) ;
#18463 = DIRECTION ( 'NONE',  ( 0.000000000000000000, 1.000000000000000000, 0.000000000000000000 ) ) ;
#18464 = CARTESIAN_POINT ( 'NONE',  ( -0.7495606340400177148, 0.1264236179284866091, 1.656003936954110412 ) ) ;
#18465 = CARTESIAN_POINT ( 'NONE',  ( -0.7185039370078746268, -0.06523048226347956391, 1.911909448711371917 ) ) ;
#18466 = ORIENTED_EDGE ( 'NONE', *, *, #19582, .T. ) ;
#18467 = CARTESIAN_POINT ( 'NONE',  ( -0.7185039370078746268, 0.06523048226347956391, 1.601870078740158077 ) ) ;
#18468 = LINE ( 'NONE', #44100, #47325 ) ;
#18469 = CARTESIAN_POINT ( 'NONE',  ( 1.054774247047244096, 0.000000000000000000, 1.405019684985606476 ) ) ;
#18470 = LINE ( 'NONE', #40022, #13393 ) ;
#18471 = ORIENTED_EDGE ( 'NONE', *, *, #30605, .T. ) ;
#18472 = CIRCLE ( 'NONE', #14650, 0.1574803149606299191 ) ;
#18473 = ORIENTED_EDGE ( 'NONE', *, *, #9702, .F. ) ;
#18474 = ORIENTED_EDGE ( 'NONE', *, *, #24304, .F. ) ;
#18475 = AXIS2_PLACEMENT_3D ( 'NONE', #42338, #28220, #5689 ) ;
#18476 = VECTOR ( 'NONE', #44092, 39.37007874015748143 ) ;
#18477 = CIRCLE ( 'NONE', #7663, 0.09842519685039310962 ) ;
#18478 = DIRECTION ( 'NONE',  ( 0.000000000000000000, 0.7880107536067203489, -0.6156614753256602901 ) ) ;
#18479 = CARTESIAN_POINT ( 'NONE',  ( -0.1787899950787401882, -0.4384842519147402196, 0.000000000000000000 ) ) ;
#18480 = CARTESIAN_POINT ( 'NONE',  ( 0.1787899950787401604, -0.8887795275052913224, 0.07405724077823318263 ) ) ;
#18481 = VERTEX_POINT ( 'NONE', #36376 ) ;
#18482 = FILL_AREA_STYLE_COLOUR ( '', #17117 ) ;
#18483 = CARTESIAN_POINT ( 'NONE',  ( 1.002407869896990045, 0.1264236179284866091, 1.798720472387181024 ) ) ;
#18484 = CARTESIAN_POINT ( 'NONE',  ( -0.1270800023317771588, -0.2027997150948566696, -0.1270800023317771588 ) ) ;
#18485 = CARTESIAN_POINT ( 'NONE',  ( 0.1264236179284866091, -0.1098680627174277585, -0.1264236179284866091 ) ) ;
#18486 = CARTESIAN_POINT ( 'NONE',  ( -0.1264236179284866091, -0.07923228341080333637, 0.1264236179284866091 ) ) ;
#18487 = CARTESIAN_POINT ( 'NONE',  ( 1.002407869896990045, 0.1264236179284866091, 0.7750984251430865779 ) ) ;
#18488 = CYLINDRICAL_SURFACE ( 'NONE', #6269, 0.1574803149606299191 ) ;
#18489 = DIRECTION ( 'NONE',  ( -1.000000000000000000, 0.000000000000000000, 0.000000000000000000 ) ) ;
#18490 = CARTESIAN_POINT ( 'NONE',  ( -0.07405724077823318263, -0.4261811023084413064, 0.1787899950787401604 ) ) ;
#18491 = CARTESIAN_POINT ( 'NONE',  ( 1.033464566929133799, 0.000000000000000000, 0.9448818896562519720 ) ) ;
#18492 = CARTESIAN_POINT ( 'NONE',  ( 0.7495606340400177148, 0.1264236179284866091, 1.892224409395055096 ) ) ;
#18494 = DIRECTION ( 'NONE',  ( 1.000000000000000000, 0.000000000000000000, -0.000000000000000000 ) ) ;
#18493 = CARTESIAN_POINT ( 'NONE',  ( -0.2275913475554304233, -0.05179116514389500714, 0.1540331450897821919 ) ) ;
#18495 = CARTESIAN_POINT ( 'NONE',  ( 0.6971942568897637749, 2.189545951927499583E-17, 0.4749015747493858242 ) ) ;
#18496 = VERTEX_POINT ( 'NONE', #6400 ) ;
#18497 = CARTESIAN_POINT ( 'NONE',  ( 0.1559665883013663656, -0.1473510212940053188, 0.02037109575272184891 ) ) ;
#18498 = CARTESIAN_POINT ( 'NONE',  ( 0.07405724077823318263, -0.2145669290800947537, -0.1787899950787401604 ) ) ;
#18500 = CARTESIAN_POINT ( 'NONE',  ( 0.1579024634500834634, 0.1046578554684915313, 0.09958160468956725464 ) ) ;
#18499 = CARTESIAN_POINT ( 'NONE',  ( -1.054774247047244540, -0.07405724077823318263, 0.4183070865604097133 ) ) ;
#18501 = CARTESIAN_POINT ( 'NONE',  ( -0.1787899950787401604, -1.144685039316316599, -0.07405724077823318263 ) ) ;
#18502 = CARTESIAN_POINT ( 'NONE',  ( 1.002407869896990045, -0.1264236179284866091, 0.2189960629383626012 ) ) ;
#18503 = EDGE_CURVE ( 'NONE', #24526, #24301, #10186, .T. ) ;
#18504 = CARTESIAN_POINT ( 'NONE',  ( 0.9412147342319837628, 0.1574803149606300301, 0.05659448818897643008 ) ) ;
#18505 = AXIS2_PLACEMENT_3D ( 'NONE', #36386, #46901, #6409 ) ;
#18506 = CARTESIAN_POINT ( 'NONE',  ( -1.054774247047244096, 0.000000000000000000, 1.596948818843874074 ) ) ;
#18507 = ORIENTED_EDGE ( 'NONE', *, *, #28425, .F. ) ;
#18508 = CARTESIAN_POINT ( 'NONE',  ( -1.054774247047244540, -0.07405724077823318263, 1.126968503883244654 ) ) ;
#18509 = CARTESIAN_POINT ( 'NONE',  ( 1.002407869896990045, -0.1264236179284866091, 1.242618110182456714 ) ) ;
#18510 = CARTESIAN_POINT ( 'NONE',  ( 0.06523048226347956391, -1.171751968396410382, -0.1574803149606300301 ) ) ;
#18511 = AXIS2_PLACEMENT_3D ( 'NONE', #12783, #13700, #20648 ) ;
#18512 = CIRCLE ( 'NONE', #45280, 0.1377952755905511861 ) ;
#18513 = CARTESIAN_POINT ( 'NONE',  ( 0.6971942568897637749, 2.189545951927499583E-17, 1.931594488135212728 ) ) ;
#18514 = CARTESIAN_POINT ( 'NONE',  ( -0.8107537697050253289, 0.1574803149606300301, 0.6520669291338586637 ) ) ;
#18515 = CARTESIAN_POINT ( 'NONE',  ( -0.9500414927467378812, 0.1787899950787401604, 1.092519684985605810 ) ) ;
#18516 = EDGE_CURVE ( 'NONE', #39448, #36523, #3533, .T. ) ;
#18517 = CARTESIAN_POINT ( 'NONE',  ( 0.1600714537641983737, 0.09473400225496043936, -0.1168739604210893984 ) ) ;
#18518 = CARTESIAN_POINT ( 'NONE',  ( -0.1647197266561004347, -0.2003932537366667210, -0.03489849683095793548 ) ) ;
#18519 = CARTESIAN_POINT ( 'NONE',  ( 0.9500414927467377701, -0.1787899950787401604, 0.3346456692375752162 ) ) ;
#18520 = CARTESIAN_POINT ( 'NONE',  ( -1.002407869896990045, 0.1264236179284866091, 0.1845472440407248116 ) ) ;
#18521 = CARTESIAN_POINT ( 'NONE',  ( -1.054774247047244096, 0.000000000000000000, 0.8095472440407244230 ) ) ;
#18522 = EDGE_LOOP ( 'NONE', ( #37211, #45478, #25610 ) ) ;
#18523 = CARTESIAN_POINT ( 'NONE',  ( -1.094772975963752103E-17, -0.05462598419820496182, -0.1787899950787401882 ) ) ;
#18524 = CARTESIAN_POINT ( 'NONE',  ( 1.002407869896990045, -0.1264236179284866091, 1.124507873961984261 ) ) ;
#18525 = CARTESIAN_POINT ( 'NONE',  ( -1.002407869896990045, 0.1264236179284866091, 1.798720472387181024 ) ) ;
#18526 = ORIENTED_EDGE ( 'NONE', *, *, #12185, .F. ) ;
#18527 = CARTESIAN_POINT ( 'NONE',  ( 0.8019270111902717657, -0.1787899950787401604, 1.860236220418677089 ) ) ;
#18528 = DIRECTION ( 'NONE',  ( 0.5735764363510447161, 0.8191520442889925757, 0.000000000000000000 ) ) ;
#18529 = CARTESIAN_POINT ( 'NONE',  ( -0.1787899950787401604, -1.318037354056011079, -0.07405724077823318263 ) ) ;
#18530 = ORIENTED_EDGE ( 'NONE', *, *, #36916, .T. ) ;
#18531 = CARTESIAN_POINT ( 'NONE',  ( 0.1787899950787401604, -0.2933070865604095467, -0.07405724077823318263 ) ) ;
#18532 = DIRECTION ( 'NONE',  ( 0.6018150231520440485, 0.000000000000000000, 0.7986355100472960489 ) ) ;
#18533 = ORIENTED_EDGE ( 'NONE', *, *, #41559, .F. ) ;
#18534 = CARTESIAN_POINT ( 'NONE',  ( 0.6971942568897648851, 0.07405724077823318263, 1.220472440891118504 ) ) ;
#18535 = VECTOR ( 'NONE', #2164, 39.37007874015748143 ) ;
#18536 = DIRECTION ( 'NONE',  ( 0.000000000000000000, 0.000000000000000000, -1.000000000000000000 ) ) ;
#18537 = EDGE_CURVE ( 'NONE', #10815, #34169, #35661, .T. ) ;
#18538 = DIRECTION ( 'NONE',  ( 1.822029033848725028E-16, 0.000000000000000000, 1.000000000000000000 ) ) ;
#18539 = CARTESIAN_POINT ( 'NONE',  ( 1.054774247047244540, 0.07405724077823318263, 1.481299212544662680 ) ) ;
#18540 = CARTESIAN_POINT ( 'NONE',  ( 0.8759842519685039353, -0.1787899950787401882, 0.1304133857730082613 ) ) ;
#18541 = AXIS2_PLACEMENT_3D ( 'NONE', #33381, #14441, #29578 ) ;
#18542 = CARTESIAN_POINT ( 'NONE',  ( -0.07405724077823318263, -1.661417322780881500, -0.1787899950787401604 ) ) ;
#18543 = PRODUCT_CONTEXT ( 'NONE', #10140, 'mechanical' ) ;
#18544 = CARTESIAN_POINT ( 'NONE',  ( -0.7495606340400177148, -0.1264236179284866091, 0.4453740156942677664 ) ) ;
#18545 = CARTESIAN_POINT ( 'NONE',  ( 0.1476377952755906220, -0.4812165006432430059, -0.8611016091043821596 ) ) ;
#18546 = CARTESIAN_POINT ( 'NONE',  ( -0.1797182628040039087, -1.420811526118478829, -0.07444174185955065859 ) ) ;
#18547 = CARTESIAN_POINT ( 'NONE',  ( 1.002407869896990045, -0.1264236179284866091, 1.360728346402929168 ) ) ;
#18548 = CARTESIAN_POINT ( 'NONE',  ( 0.8019270111902716547, 0.1787899950787401604, 1.687992125930489307 ) ) ;
#18549 = DIRECTION ( 'NONE',  ( -0.000000000000000000, 1.000000000000000000, -0.000000000000000000 ) ) ;
#18550 = CARTESIAN_POINT ( 'NONE',  ( -0.09075913361134779755, 0.1299212598425197318, 0.1419506277346105627 ) ) ;
#18551 = DIRECTION ( 'NONE',  ( -1.000000000000000000, 0.000000000000000000, 0.000000000000000000 ) ) ;
#18552 = FACE_OUTER_BOUND ( 'NONE', #21727, .T. ) ;
#18553 = CARTESIAN_POINT ( 'NONE',  ( -0.9873396505805591694, -0.1113553986120547346, 1.028543307086614123 ) ) ;
#18554 = CARTESIAN_POINT ( 'NONE',  ( 0.8107537697050254399, 0.1574803149606300301, 0.7603346455617647770 ) ) ;
#18555 = CARTESIAN_POINT ( 'NONE',  ( 1.054774247047244540, -0.07405724077823318263, 0.2952755904974176393 ) ) ;
#18556 = EDGE_CURVE ( 'NONE', #3019, #25965, #10012, .T. ) ;
#18558 = CARTESIAN_POINT ( 'NONE',  ( -0.1377952755905511861, -1.331775896911328393E-15, -0.8070866141732283561 ) ) ;
#18557 = CARTESIAN_POINT ( 'NONE',  ( 0.7495606340400177148, -0.1264236179284866091, 1.267224409395055096 ) ) ;
#18559 = DIRECTION ( 'NONE',  ( 0.000000000000000000, 0.000000000000000000, 1.000000000000000000 ) ) ;
#18560 = DIRECTION ( 'NONE',  ( 0.000000000000000000, 0.000000000000000000, 1.000000000000000000 ) ) ;
#18561 = CARTESIAN_POINT ( 'NONE',  ( -1.054774247047244540, -0.07405724077823318263, 1.240157480261197431 ) ) ;
#18562 = CARTESIAN_POINT ( 'NONE',  ( 0.8107537697050253289, -0.1574803149606297803, 0.6569881888688503535 ) ) ;
#18563 = VERTEX_POINT ( 'NONE', #6872 ) ;
#18564 = CARTESIAN_POINT ( 'NONE',  ( -0.9873396505805591694, 0.1113553986120547346, 1.747047244094488194 ) ) ;
#18565 = CARTESIAN_POINT ( 'NONE',  ( 0.9781702082981658108, 0.1325945652753822701, 0.03936699474371046364 ) ) ;
#18566 = VERTEX_POINT ( 'NONE', #43298 ) ;
#18567 = CARTESIAN_POINT ( 'NONE',  ( 0.07444174185955065859, 0.1293853242752222577, 0.1797182628040039087 ) ) ;
#18568 = CARTESIAN_POINT ( 'NONE',  ( -0.1574803149606299191, -1.041338582569637738, 0.000000000000000000 ) ) ;
#18569 = CARTESIAN_POINT ( 'NONE',  ( -0.7185039370078739607, 1.928577636452523993E-17, 1.122047243986960652 ) ) ;
#18570 = CARTESIAN_POINT ( 'NONE',  ( 0.7495606340400177148, 0.1264236179284866091, 1.532972440891118060 ) ) ;
#18571 = CARTESIAN_POINT ( 'NONE',  ( -0.9412147342319837628, 0.1574803149606300301, 1.828248031496063630 ) ) ;
#18572 = CARTESIAN_POINT ( 'NONE',  ( 0.1787899950787401604, -0.2145669290800947537, -0.07405724077823318263 ) ) ;
#18573 = VERTEX_POINT ( 'NONE', #10975 ) ;
#18574 = AXIS2_PLACEMENT_3D ( 'NONE', #13293, #27922, #2712 ) ;
#18575 = CARTESIAN_POINT ( 'NONE',  ( -0.1113553986120547346, 0.09547244094488190058, 0.1113553986120547346 ) ) ;
#18576 = PRESENTATION_STYLE_ASSIGNMENT (( #30747 ) ) ;
#18577 = CARTESIAN_POINT ( 'NONE',  ( 0.7495606340400177148, 0.1264236179284866091, 0.6323818897100157432 ) ) ;
#18578 = ORIENTED_EDGE ( 'NONE', *, *, #44717, .F. ) ;
#18579 = CARTESIAN_POINT ( 'NONE',  ( 0.1574803149606300301, 0.1225393701862672879, -0.06523048226347956391 ) ) ;
#18580 = CARTESIAN_POINT ( 'NONE',  ( -0.9500414927467378812, 0.1787899950787401604, 1.097440944828127041 ) ) ;
#18581 = CARTESIAN_POINT ( 'NONE',  ( -0.1818270763433404713, 0.1905157801856738331, -0.3106979152243534159 ) ) ;
#18582 = CARTESIAN_POINT ( 'NONE',  ( -0.8019270111902717657, 0.1787899950787401604, 0.1574803149068664809 ) ) ;
#18583 = DIRECTION ( 'NONE',  ( 0.000000000000000000, 0.000000000000000000, -1.000000000000000000 ) ) ;
#18584 = ( BOUNDED_CURVE ( )  B_SPLINE_CURVE ( 2, ( #31738, #24764, #13510, #46794, #36019, #17808, #14226, #28868, #39362 ),
 .UNSPECIFIED., .F., .T. ) 
 B_SPLINE_CURVE_WITH_KNOTS ( ( 3, 2, 2, 2, 3 ),
 ( 0.7500000000000000000, 0.7524999999999999467, 0.7550000000000000044, 0.7574999999999999512, 0.7600000000000000089 ),
 .UNSPECIFIED. ) 
 CURVE ( )  GEOMETRIC_REPRESENTATION_ITEM ( )  RATIONAL_B_SPLINE_CURVE ( ( 1.000000000000000000, 0.9238795325112869605, 1.000000000000000000, 0.9238795325112869605, 1.000000000000000000, 0.9238795325112869605, 1.000000000000000000, 0.9238795325112869605, 1.000000000000000000 ) ) 
 REPRESENTATION_ITEM ( '' )  ) ;
#18585 = CARTESIAN_POINT ( 'NONE',  ( 0.9873396505805591694, -0.1113553986120547346, 1.648622047136566904 ) ) ;
#18586 = CARTESIAN_POINT ( 'NONE',  ( 0.1787899950787401604, -0.8259113698040420060, 0.07405724077823318263 ) ) ;
#18587 = ( GEOMETRIC_REPRESENTATION_CONTEXT ( 3 ) GLOBAL_UNCERTAINTY_ASSIGNED_CONTEXT ( ( #5727 ) ) GLOBAL_UNIT_ASSIGNED_CONTEXT ( ( #6167, #24630, #13839 ) ) REPRESENTATION_CONTEXT ( 'NONE', 'WORKASPACE' ) ) ;
#18588 = CARTESIAN_POINT ( 'NONE',  ( -0.1787899950787401882, 0.1176181102899840625, 0.000000000000000000 ) ) ;
#18589 = EDGE_LOOP ( 'NONE', ( #43145, #20933, #1937, #45909 ) ) ;
#18590 = EDGE_CURVE ( 'NONE', #23202, #43509, #21869, .T. ) ;
#18591 = CARTESIAN_POINT ( 'NONE',  ( -1.002407869896990045, 0.1264236179284866091, 0.7750984251430865779 ) ) ;
#18592 = PLANE ( 'NONE',  #43709 ) ;
#18593 = CARTESIAN_POINT ( 'NONE',  ( -0.6971942568897648851, -0.07405724077823297447, 1.860236220418677089 ) ) ;
#18594 = AXIS2_PLACEMENT_3D ( 'NONE', #14973, #3923, #15918 ) ;
#18595 = CARTESIAN_POINT ( 'NONE',  ( -0.7495606340400177148, -0.1264236179284866091, 0.05167322829269323931 ) ) ;
#18596 = CARTESIAN_POINT ( 'NONE',  ( -0.9412147342319837628, 0.1574803149606300301, 0.8439960629921254842 ) ) ;
#18597 = CARTESIAN_POINT ( 'NONE',  ( -0.07444174185955065859, -0.9778981402917082955, 0.1797182628040039087 ) ) ;
#18598 = CARTESIAN_POINT ( 'NONE',  ( 0.1171060910386464843, -0.2278812977170392440, -0.3148284977848750943 ) ) ;
#18599 = CARTESIAN_POINT ( 'NONE',  ( -0.9412147342319837628, 0.1574803149606300301, 1.503444881782235232 ) ) ;
#18600 = EDGE_CURVE ( 'NONE', #2019, #33940, #35337, .T. ) ;
#18601 = CARTESIAN_POINT ( 'NONE',  ( 0.8019270111902717657, -0.1787899950787401604, 0.8415354330171019859 ) ) ;
#18602 = ADVANCED_FACE ( 'NONE', ( #13836 ), #17904, .T. ) ;
#18603 = CARTESIAN_POINT ( 'NONE',  ( -1.054774247047244096, 0.000000000000000000, 1.562499999946236118 ) ) ;
#18604 = VECTOR ( 'NONE', #18863, 39.37007874015748854 ) ;
#18605 = CARTESIAN_POINT ( 'NONE',  ( -0.9873396505805591694, 0.1113553986120547346, 0.4478346456692913202 ) ) ;
#18606 = CARTESIAN_POINT ( 'NONE',  ( 0.9412147342319837628, 0.1574803149606300301, 1.355807086614173596 ) ) ;
#18608 = DIRECTION ( 'NONE',  ( 0.000000000000000000, 0.000000000000000000, -1.000000000000000000 ) ) ;
#18607 = CARTESIAN_POINT ( 'NONE',  ( 0.8499887760485748123, -0.1717780610005492925, 1.987730942720379090 ) ) ;
#18609 = CLOSED_SHELL ( 'NONE', ( #44137, #33806, #26315, #31454, #12907, #7575, #1235, #26590, #193, #10387, #6615, #28218, #44450, #6240, #21210, #9646, #19421, #24622, #39481, #44938, #20166, #3636, #4262, #23528, #32286, #42455, #12207, #24359, #40977, #41083, #39539, #36631, #2208, #44402, #7208, #44707, #15883, #20131, #1609, #43994, #3736, #18876, #13479, #5635 ) ) ;
#18610 = ADVANCED_FACE ( 'NONE', ( #43051 ), #24861, .T. ) ;
#18611 = CARTESIAN_POINT ( 'NONE',  ( 0.6971942568897648851, -0.07405724077823297447, 0.7529527558517473684 ) ) ;
#18612 = CARTESIAN_POINT ( 'NONE',  ( 0.07405724077823318263, -0.8149606298674965110, 0.1787899950787401604 ) ) ;
#18613 = ORIENTED_EDGE ( 'NONE', *, *, #46906, .T. ) ;
#18614 = CARTESIAN_POINT ( 'NONE',  ( 1.033464566929134687, 0.06523048226347956391, 0.9178149606299221830 ) ) ;
#18615 = CARTESIAN_POINT ( 'NONE',  ( 1.033464566929133799, 0.000000000000000000, 0.4035433070866141780 ) ) ;
#18616 = CARTESIAN_POINT ( 'NONE',  ( 1.054774247047244540, -0.07405724077823318263, 1.043307086560409269 ) ) ;
#18617 = EDGE_CURVE ( 'NONE', #6678, #30540, #46892, .T. ) ;
#18618 = CYLINDRICAL_SURFACE ( 'NONE', #17263, 0.2952755905511810774 ) ;
#18619 = CARTESIAN_POINT ( 'NONE',  ( 2.892866454678787531E-17, -1.671259842519685179, 0.1574803149606299191 ) ) ;
#18620 = CARTESIAN_POINT ( 'NONE',  ( 0.2066929133858268486, -0.2237541348899642901, -1.272196386806234925 ) ) ;
#18621 = CARTESIAN_POINT ( 'NONE',  ( -0.9500414927467378812, 0.1787899950787401604, 0.5019685038832442103 ) ) ;
#18622 = VERTEX_POINT ( 'NONE', #37282 ) ;
#18623 = FACE_OUTER_BOUND ( 'NONE', #16759, .T. ) ;
#18624 = CARTESIAN_POINT ( 'NONE',  ( -1.002407869896990045, -0.1264236179284866091, 0.2534448818360003908 ) ) ;
#18625 = ORIENTED_EDGE ( 'NONE', *, *, #22560, .F. ) ;
#18626 = CARTESIAN_POINT ( 'NONE',  ( 0.1113553986120547346, 0.1151574803149606335, -0.1113553986120547346 ) ) ;
#18627 = CARTESIAN_POINT ( 'NONE',  ( -0.8759842519685039353, 0.1787899950787401882, 1.724901574749385880 ) ) ;
#18628 = CARTESIAN_POINT ( 'NONE',  ( -0.6971942568897637749, 2.189545951927499583E-17, 0.8686023621509606496 ) ) ;
#18629 = CARTESIAN_POINT ( 'NONE',  ( -0.7495606340400177148, 0.1264236179284866091, 0.3174212597887562382 ) ) ;
#18630 = CARTESIAN_POINT ( 'NONE',  ( 0.06523048226347956391, -0.03001968493184305545, -0.1574803149606300301 ) ) ;
#18631 = CARTESIAN_POINT ( 'NONE',  ( 0.7646288533564489232, -0.1113553986120547346, 0.9793307086614173596 ) ) ;
#18632 = PLANE ( 'NONE',  #43266 ) ;
#18633 = CARTESIAN_POINT ( 'NONE',  ( 0.08443540605192632886, 0.09133345722616725837, -0.2366842664529266727 ) ) ;
#18634 = CARTESIAN_POINT ( 'NONE',  ( -0.2833779466431469163, 0.1260493684579870322, -0.9865437305733709694 ) ) ;
#18635 = CARTESIAN_POINT ( 'NONE',  ( -0.1264236179284866091, -0.3756160942134905700, -0.1264236179284866091 ) ) ;
#18636 = CARTESIAN_POINT ( 'NONE',  ( -0.1979409878709763870, -0.08955984950924253396, 0.1204397522454633829 ) ) ;
#18637 = CARTESIAN_POINT ( 'NONE',  ( -0.8759842519685039353, 0.1574803149606299191, 1.899606299105070839 ) ) ;
#18638 = CARTESIAN_POINT ( 'NONE',  ( 2.892866454678787531E-17, 0.03149606309965303358, 0.1574803149606299191 ) ) ;
#18639 = AXIS2_PLACEMENT_3D ( 'NONE', #40445, #37335, #26349 ) ;
#18640 = CARTESIAN_POINT ( 'NONE',  ( -0.8019270111902717657, -0.1787899950787401604, 0.2460629920722207375 ) ) ;
#18641 = ORIENTED_EDGE ( 'NONE', *, *, #42405, .F. ) ;
#18642 = ORIENTED_EDGE ( 'NONE', *, *, #31785, .F. ) ;
#18643 = CARTESIAN_POINT ( 'NONE',  ( -1.054774247047244096, 0.000000000000000000, 1.365649606245448844 ) ) ;
#18644 = EDGE_LOOP ( 'NONE', ( #5673, #12930, #38691, #13790 ) ) ;
#18645 = EDGE_CURVE ( 'NONE', #11192, #28460, #10483, .T. ) ;
#18646 = CARTESIAN_POINT ( 'NONE',  ( -0.1264236179284866091, -1.270177165300566902, -0.1264236179284866091 ) ) ;
#18647 = CARTESIAN_POINT ( 'NONE',  ( -1.094772975963752103E-17, -1.467027559001354398, -0.1787899950787401882 ) ) ;
#18648 = DIRECTION ( 'NONE',  ( 1.822029033848725028E-16, 0.000000000000000000, 1.000000000000000000 ) ) ;
#18649 = DIRECTION ( 'NONE',  ( 0.000000000000000000, -4.000000000000000311E-15, 1.000000000000000000 ) ) ;
#18650 = EDGE_CURVE ( 'NONE', #6014, #35175, #34461, .T. ) ;
#18651 = CARTESIAN_POINT ( 'NONE',  ( 0.7646288533564489232, 0.1113553986120547346, 0.4183070866141732624 ) ) ;
#18652 = DIRECTION ( 'NONE',  ( 0.000000000000000000, 0.000000000000000000, -1.000000000000000000 ) ) ;
#18653 = CARTESIAN_POINT ( 'NONE',  ( -0.9873396505805591694, -0.1113553986120547346, 1.018700787294047228 ) ) ;
#18654 = EDGE_CURVE ( 'NONE', #529, #43357, #22915, .T. ) ;
#18655 = LINE ( 'NONE', #13949, #28388 ) ;
#18656 = ( REPRESENTATION_RELATIONSHIP ('NONE','NONE', #9609, #1042 ) REPRESENTATION_RELATIONSHIP_WITH_TRANSFORMATION ( #10124 )SHAPE_REPRESENTATION_RELATIONSHIP( ) ) ;
#18657 = VERTEX_POINT ( 'NONE', #23156 ) ;
#18658 = CARTESIAN_POINT ( 'NONE',  ( 0.7185039370078739607, 0.000000000000000000, 4.498031496062992574 ) ) ;
#18659 = VERTEX_POINT ( 'NONE', #37057 ) ;
#18660 = DIRECTION ( 'NONE',  ( 0.000000000000000000, 1.000000000000000000, 0.000000000000000000 ) ) ;
#18661 = CARTESIAN_POINT ( 'NONE',  ( 0.7185039370078739607, 1.928577636452523993E-17, 0.8956692913385826404 ) ) ;
#18662 = CARTESIAN_POINT ( 'NONE',  ( -0.1574803149606297803, -0.5270669290263310103, 0.06523048226347956391 ) ) ;
#18663 = CARTESIAN_POINT ( 'NONE',  ( 0.7646288533564489232, -0.1113553986120547346, 1.530511811023621993 ) ) ;
#18664 = DIRECTION ( 'NONE',  ( 4.272009658007748186E-16, 0.7880107536067211260, -0.6156614753256594019 ) ) ;
#18665 = VECTOR ( 'NONE', #19840, 39.37007874015748143 ) ;
#18666 = CARTESIAN_POINT ( 'NONE',  ( -0.2741498948998221663, 0.1449524278970008850, 0.7917137902625999146 ) ) ;
#18667 = ORIENTED_EDGE ( 'NONE', *, *, #34172, .T. ) ;
#18668 = CARTESIAN_POINT ( 'NONE',  ( 0.9873396505805591694, 0.1113553986120547346, 1.894685039262551163 ) ) ;
#18669 = CARTESIAN_POINT ( 'NONE',  ( 0.7646288533564489232, -0.1113553986120547346, 1.373031496062992352 ) ) ;
#18670 = CARTESIAN_POINT ( 'NONE',  ( -1.094772975963752103E-17, -1.545767716481669218, -0.1787899950787401882 ) ) ;
#18671 = CARTESIAN_POINT ( 'NONE',  ( 0.1264236179284866091, -0.8174212597887557941, 0.1264236179284866091 ) ) ;
#18672 = CARTESIAN_POINT ( 'NONE',  ( -0.1113553986120547346, -1.134842519685039353, -0.1113553986120547346 ) ) ;
#18673 = CARTESIAN_POINT ( 'NONE',  ( 0.9412147342319837628, -0.1574803149606297803, 0.9768700786326298680 ) ) ;
#18674 = CARTESIAN_POINT ( 'NONE',  ( -0.7185039370078739607, 1.928577636452523993E-17, 0.4232283464566928832 ) ) ;
#18675 = UNCERTAINTY_MEASURE_WITH_UNIT (LENGTH_MEASURE( 1.000000000000000082E-05 ), #33257, 'distance_accuracy_value', 'NONE') ;
#18676 = ORIENTED_EDGE ( 'NONE', *, *, #19255, .F. ) ;
#18677 = ORIENTED_EDGE ( 'NONE', *, *, #40079, .T. ) ;
#18678 = CARTESIAN_POINT ( 'NONE',  ( -0.9500414927467378812, 0.1787899950787401604, 1.648622047190331230 ) ) ;
#18679 = CARTESIAN_POINT ( 'NONE',  ( 1.002407869896990045, -0.1264236179284866091, 1.715059055064346527 ) ) ;
#18680 = CARTESIAN_POINT ( 'NONE',  ( -0.1574803149606299191, -1.316929133750740055, 0.000000000000000000 ) ) ;
#18681 = CARTESIAN_POINT ( 'NONE',  ( -0.8019270111902717657, -0.1787899950787401604, 0.7234251967966300878 ) ) ;
#18682 = DIRECTION ( 'NONE',  ( 0.000000000000000000, 0.000000000000000000, 1.000000000000000000 ) ) ;
#18683 = CARTESIAN_POINT ( 'NONE',  ( 1.054774247047244096, 0.000000000000000000, 0.2632874015210397434 ) ) ;
#18684 = LINE ( 'NONE', #15349, #9817 ) ;
#18685 = CARTESIAN_POINT ( 'NONE',  ( -0.8759842519685039353, 0.1787899950787401882, 1.291830708607653477 ) ) ;
#18686 = DIRECTION ( 'NONE',  ( -1.000000000000000000, 0.000000000000000000, -0.000000000000000000 ) ) ;
#18687 = ( BOUNDED_CURVE ( )  B_SPLINE_CURVE ( 2, ( #47282, #15650, #34553, #27395, #30288, #19921, #34104, #41464, #12285 ),
 .UNSPECIFIED., .F., .T. ) 
 B_SPLINE_CURVE_WITH_KNOTS ( ( 3, 2, 2, 2, 3 ),
 ( 0.6600000000000000311, 0.6624999999999999778, 0.6650000000000000355, 0.6674999999999999822, 0.6700000000000000400 ),
 .UNSPECIFIED. ) 
 CURVE ( )  GEOMETRIC_REPRESENTATION_ITEM ( )  RATIONAL_B_SPLINE_CURVE ( ( 1.000000000000000000, 0.9238795325112869605, 1.000000000000000000, 0.9238795325112869605, 1.000000000000000000, 0.9238795325112869605, 1.000000000000000000, 0.9238795325112829637, 1.000000000000000000 ) ) 
 REPRESENTATION_ITEM ( '' )  ) ;
#18688 = CARTESIAN_POINT ( 'NONE',  ( 0.08400343811432031682, 0.09129006187721050436, 0.2369336632579849278 ) ) ;
#18689 = CARTESIAN_POINT ( 'NONE',  ( -0.8759842519685039353, -0.1787899950787401882, 1.513287401521039355 ) ) ;
#18690 = CARTESIAN_POINT ( 'NONE',  ( -0.7646288533564489232, 0.1113553986120547346, 1.865157480207432883 ) ) ;
#18691 = EDGE_LOOP ( 'NONE', ( #1867, #43742, #15572, #31815 ) ) ;
#18692 = DIRECTION ( 'NONE',  ( 0.000000000000000000, 0.7880107536067184615, -0.6156614753256628436 ) ) ;
#18693 = CARTESIAN_POINT ( 'NONE',  ( -0.8759842519685039353, 0.1574803149606299191, 1.594488188976378007 ) ) ;
#18694 = CARTESIAN_POINT ( 'NONE',  ( 0.3161444924769519216, 1.488499961090669288, -0.3513258257898460579 ) ) ;
#18695 = CARTESIAN_POINT ( 'NONE',  ( 0.8019270111902716547, 0.1787899950787401604, 1.417322834591906444 ) ) ;
#18696 = CARTESIAN_POINT ( 'NONE',  ( -0.2364432464758906005, -0.09842519685039370636, -0.06084591350176535296 ) ) ;
#18697 = DIRECTION ( 'NONE',  ( 1.822029033848725028E-16, 0.000000000000000000, 1.000000000000000000 ) ) ;
#18698 = CIRCLE ( 'NONE', #29581, 0.04921259842519682542 ) ;
#18699 = VERTEX_POINT ( 'NONE', #26768 ) ;
#18700 = AXIS2_PLACEMENT_3D ( 'NONE', #18325, #25766, #40336 ) ;
#18701 = EDGE_CURVE ( 'NONE', #22505, #33099, #29689, .T. ) ;
#18702 = CARTESIAN_POINT ( 'NONE',  ( 0.1787899950787401604, -0.9675196849856075865, -0.07405724077823318263 ) ) ;
#18703 = ( BOUNDED_CURVE ( )  B_SPLINE_CURVE ( 2, ( #22208, #19565, #11445, #26545, #4940, #34211, #44703, #41339, #37294 ),
 .UNSPECIFIED., .F., .T. ) 
 B_SPLINE_CURVE_WITH_KNOTS ( ( 3, 2, 2, 2, 3 ),
 ( 0.4199999999999999845, 0.4224999999999999867, 0.4249999999999999889, 0.4274999999999999911, 0.4299999999999999933 ),
 .UNSPECIFIED. ) 
 CURVE ( )  GEOMETRIC_REPRESENTATION_ITEM ( )  RATIONAL_B_SPLINE_CURVE ( ( 1.000000000000000000, 0.9238795325112869605, 1.000000000000000000, 0.9238795325112869605, 1.000000000000000000, 0.9238795325112869605, 1.000000000000000000, 0.9238795325112869605, 1.000000000000000000 ) ) 
 REPRESENTATION_ITEM ( '' )  ) ;
#18704 = CARTESIAN_POINT ( 'NONE',  ( -0.1787899950787401604, -0.4409448818359998357, -0.07405724077823318263 ) ) ;
#18705 = EDGE_CURVE ( 'NONE', #7195, #23068, #30020, .T. ) ;
#18706 = CARTESIAN_POINT ( 'NONE',  ( 0.07405724077823318263, -0.8937007873478103326, 0.1787899950787401604 ) ) ;
#18707 = DIRECTION ( 'NONE',  ( 1.000000000000000000, 5.372880794957870593E-15, -4.197754538034584604E-15 ) ) ;
#18708 = ( NAMED_UNIT ( * ) SI_UNIT ( $, .STERADIAN. ) SOLID_ANGLE_UNIT ( ) ) ;
#18709 = CARTESIAN_POINT ( 'NONE',  ( 0.1270800023317771588, -0.2224847544649354303, 0.1270800023317771588 ) ) ;
#18710 = EDGE_CURVE ( 'NONE', #42764, #16359, #7389, .T. ) ;
#18711 = CARTESIAN_POINT ( 'NONE',  ( -0.06523048226347956391, 0.1225393700787401341, -0.1574803149606300301 ) ) ;
#18712 = CARTESIAN_POINT ( 'NONE',  ( -0.07405724077823318263, -0.01279527553678766298, -0.1787899950787401604 ) ) ;
#18713 = CARTESIAN_POINT ( 'NONE',  ( 0.9412147342319837628, -0.1574803149606297803, 0.1500984250893234173 ) ) ;
#18714 = EDGE_CURVE ( 'NONE', #14452, #44955, #18477, .T. ) ;
#18715 = CARTESIAN_POINT ( 'NONE',  ( -0.7185039370078739607, 1.928577636452523993E-17, 0.8858267715460158565 ) ) ;
#18716 = CARTESIAN_POINT ( 'NONE',  ( 1.002407869896990045, 0.1264236179284866091, 0.7357283464029290565 ) ) ;
#18718 = CARTESIAN_POINT ( 'NONE',  ( 0.8759842519685039353, -0.1574803149606299191, 1.131889763672000004 ) ) ;
#18717 = CARTESIAN_POINT ( 'NONE',  ( -0.8823337881418780171, 0.1741736834747893703, 0.03937007874015843734 ) ) ;
#18720 = DIRECTION ( 'NONE',  ( 0.000000000000000000, -0.6156614753256604011, -0.7880107536067203489 ) ) ;
#18719 = CARTESIAN_POINT ( 'NONE',  ( 0.8070866141732283561, -0.3937007874015746034, -0.7574803149606299524 ) ) ;
#18721 = LINE ( 'NONE', #39577, #45233 ) ;
#18722 = CARTESIAN_POINT ( 'NONE',  ( 0.6971942568897648851, 0.07405724077823318263, 1.855314960576157635 ) ) ;
#18723 = CARTESIAN_POINT ( 'NONE',  ( 0.000000000000000000, 0.000000000000000000, -0.2952755905511806334 ) ) ;
#18724 = CARTESIAN_POINT ( 'NONE',  ( 0.9873396505805591694, -0.1113553986120547346, 0.08366141732283464971 ) ) ;
#18725 = CARTESIAN_POINT ( 'NONE',  ( 0.1574803149606299191, 0.3740157480314960647, 0.9783464566929134243 ) ) ;
#18727 = CARTESIAN_POINT ( 'NONE',  ( -0.07405724077823318263, -0.2490157479777327099, -0.1787899950787401604 ) ) ;
#18726 = CARTESIAN_POINT ( 'NONE',  ( -0.1113553986120547346, -0.9675196849318424830, -0.1113553986120547346 ) ) ;
#18728 = DIRECTION ( 'NONE',  ( 1.000000000000000000, 0.000000000000000000, -1.822029033848725275E-16 ) ) ;
#18729 = CARTESIAN_POINT ( 'NONE',  ( -0.1264236179284866091, -1.265255905458047225, -0.1264236179284866091 ) ) ;
#18730 = CARTESIAN_POINT ( 'NONE',  ( 0.6971942568897626646, 0.07405724077823318263, 0.1624015747493861295 ) ) ;
#18731 = LINE ( 'NONE', #507, #11688 ) ;
#18732 = CARTESIAN_POINT ( 'NONE',  ( 1.002407869896990045, 0.1264236179284866091, 0.5782480314422993040 ) ) ;
#18733 = CARTESIAN_POINT ( 'NONE',  ( -0.8759842519685039353, 0.1787899950787401882, 1.567421259788755794 ) ) ;
#18734 = VERTEX_POINT ( 'NONE', #44463 ) ;
#18735 = VECTOR ( 'NONE', #15133, 39.37007874015748143 ) ;
#18736 = CARTESIAN_POINT ( 'NONE',  ( -0.8759842519685039353, 0.1787899950787401882, 1.139271653489543290 ) ) ;
#18737 = CARTESIAN_POINT ( 'NONE',  ( -0.7185039370078746268, 0.06523048226347956391, 0.3420275590551182798 ) ) ;
#18738 = CARTESIAN_POINT ( 'NONE',  ( 0.7495606340400177148, -0.1264236179284866091, 1.311515747977732405 ) ) ;
#18739 = VECTOR ( 'NONE', #13139, 39.37007874015748854 ) ;
#18740 = CARTESIAN_POINT ( 'NONE',  ( 1.054774247047244540, -0.07405724077823318263, 0.06397637789899228433 ) ) ;
#18741 = CARTESIAN_POINT ( 'NONE',  ( -0.9500414927467378812, 0.1787899950787401604, 1.131889763725763665 ) ) ;
#18742 = CARTESIAN_POINT ( 'NONE',  ( -0.7185039370078739607, 1.928577636452523993E-17, 0.3740157479239689664 ) ) ;
#18743 = DIRECTION ( 'NONE',  ( 0.000000000000000000, -1.000000000000000000, 0.000000000000000000 ) ) ;
#18744 = CARTESIAN_POINT ( 'NONE',  ( 0.9500414927467377701, 0.1787899950787401604, 0.3887795275052913224 ) ) ;
#18745 = CARTESIAN_POINT ( 'NONE',  ( -0.8019270111902716547, 0.1787899950787401604, 0.1525590550643468324 ) ) ;
#18746 = CARTESIAN_POINT ( 'NONE',  ( -0.6971942568897626646, -0.07405724077823297447, 0.7135826771115916234 ) ) ;
#18747 = ORIENTED_EDGE ( 'NONE', *, *, #21262, .F. ) ;
#18748 = CARTESIAN_POINT ( 'NONE',  ( -0.8759842519685039353, 0.1574803149606299191, 1.358267716535433323 ) ) ;
#18749 = ORIENTED_EDGE ( 'NONE', *, *, #1026, .T. ) ;
#18750 = CARTESIAN_POINT ( 'NONE',  ( 1.054774247047244540, 0.07405724077823318263, 0.8956692912848198684 ) ) ;
#18751 = CARTESIAN_POINT ( 'NONE',  ( -0.8107537697050253289, 0.1574803149606300301, 0.1008858267716536417 ) ) ;
#18752 = CARTESIAN_POINT ( 'NONE',  ( 0.8759842519685039353, 0.1787899950787401882, 1.021161417269070837 ) ) ;
#18753 = CARTESIAN_POINT ( 'NONE',  ( -1.002407869896990045, -0.1264236179284866091, 1.906988188922614125 ) ) ;
#18754 = ORIENTED_EDGE ( 'NONE', *, *, #43762, .T. ) ;
#18755 = CARTESIAN_POINT ( 'NONE',  ( 0.8019270111902717657, -0.1787899950787401604, 1.899606299158834943 ) ) ;
#18756 = CARTESIAN_POINT ( 'NONE',  ( 0.3547871005709968273, 4.766607801171850497E-17, 0.000000000000000000 ) ) ;
#18757 = CARTESIAN_POINT ( 'NONE',  ( -0.1787899950787401604, -1.396777511536325234, -0.07405724077823318263 ) ) ;
#18758 = ORIENTED_EDGE ( 'NONE', *, *, #32814, .F. ) ;
#18759 = FACE_OUTER_BOUND ( 'NONE', #24238, .T. ) ;
#18760 = CARTESIAN_POINT ( 'NONE',  ( -1.094772975963752103E-17, -0.2465551180564728440, -0.1787899950787401882 ) ) ;
#18761 = CARTESIAN_POINT ( 'NONE',  ( -0.3100393700787401619, 0.000000000000000000, 0.7086614173228351632 ) ) ;
#18762 = ORIENTED_EDGE ( 'NONE', *, *, #18271, .F. ) ;
#18763 = CARTESIAN_POINT ( 'NONE',  ( 0.9500414927467378812, 0.1787899950787401604, 1.131889763725763665 ) ) ;
#18764 = CARTESIAN_POINT ( 'NONE',  ( -1.033464566929133799, 0.000000000000000000, 0.8267716534357796299 ) ) ;
#18765 = DIRECTION ( 'NONE',  ( -5.244653365444468611E-15, 0.2126700594527759225, -0.9771240687918565371 ) ) ;
#18766 = ADVANCED_FACE ( 'NONE', ( #4686 ), #14797, .T. ) ;
#18767 = DIRECTION ( 'NONE',  ( 1.000000000000000000, 0.000000000000000000, 0.000000000000000000 ) ) ;
#18768 = CARTESIAN_POINT ( 'NONE',  ( 0.7495606340400177148, -0.1264236179284866091, 0.2042322834108035723 ) ) ;
#18769 = AXIS2_PLACEMENT_3D ( 'NONE', #32588, #29494, #44038 ) ;
#18770 = EDGE_CURVE ( 'NONE', #23920, #758, #33020, .T. ) ;
#18771 = VECTOR ( 'NONE', #28223, 39.37007874015748143 ) ;
#18772 = AXIS2_PLACEMENT_3D ( 'NONE', #26279, #22416, #11888 ) ;
#18773 = CARTESIAN_POINT ( 'NONE',  ( -0.1787899950787401604, -1.695866141678520567, 0.07405724077823318263 ) ) ;
#18774 = CARTESIAN_POINT ( 'NONE',  ( 0.1787899950787401882, -1.752460629867496067, -2.189545951927503898E-17 ) ) ;
#18775 = CARTESIAN_POINT ( 'NONE',  ( 0.000000000000000000, 0.000000000000000000, 0.000000000000000000 ) ) ;
#18776 = EDGE_CURVE ( 'NONE', #7776, #24150, #36109, .T. ) ;
#18777 = CARTESIAN_POINT ( 'NONE',  ( -0.7495606340400177148, 0.1264236179284866091, 0.5930118109698583329 ) ) ;
#18778 = ( LENGTH_UNIT ( ) NAMED_UNIT ( * ) SI_UNIT ( $, .METRE. ) ) ;
#18779 = CARTESIAN_POINT ( 'NONE',  ( -0.1270800023317771588, -1.344531998559423069, -0.1270800023317771588 ) ) ;
#18780 = CARTESIAN_POINT ( 'NONE',  ( -0.3980944881889761366, 0.1864803149606355237, -0.7480314960629921295 ) ) ;
#18781 = CARTESIAN_POINT ( 'NONE',  ( 0.6971942568897637749, 2.189545951927499583E-17, 1.424704724355685181 ) ) ;
#18782 = CARTESIAN_POINT ( 'NONE',  ( 0.7495606340400177148, 0.1264236179284866091, 1.690452755851748146 ) ) ;
#18783 = CYLINDRICAL_SURFACE ( 'NONE', #9223, 0.09842519685039310962 ) ;
#18785 = CARTESIAN_POINT ( 'NONE',  ( -0.7760757061066729801, 0.1264651649003885048, 1.980451458961573596 ) ) ;
#18784 = DIRECTION ( 'NONE',  ( -7.047314121155773299E-15, 0.000000000000000000, 1.000000000000000000 ) ) ;
#18786 = DIRECTION ( 'NONE',  ( -0.000000000000000000, 0.2432573283306645462, -0.9699617890481188054 ) ) ;
#18787 = CARTESIAN_POINT ( 'NONE',  ( -0.1787899950787401604, 0.1496062992663619862, -0.07405724077823318263 ) ) ;
#18788 = DIRECTION ( 'NONE',  ( 0.000000000000000000, -1.000000000000000000, 0.000000000000000000 ) ) ;
#18789 = CARTESIAN_POINT ( 'NONE',  ( 1.054774247047244096, 0.000000000000000000, 0.2583661416785200671 ) ) ;
#18790 = PLANE ( 'NONE',  #4714 ) ;
#18791 = CARTESIAN_POINT ( 'NONE',  ( 0.4453382816733590377, 4.766607801171850497E-17, 0.000000000000000000 ) ) ;
#18792 = CARTESIAN_POINT ( 'NONE',  ( -1.033464566929134687, 0.06523048226347956391, 0.7603346456692923194 ) ) ;
#18793 = CARTESIAN_POINT ( 'NONE',  ( 1.033464566929134687, -0.06523048226347956391, 0.6274606298137325178 ) ) ;
#18794 = ORIENTED_EDGE ( 'NONE', *, *, #15433, .T. ) ;
#18795 = CARTESIAN_POINT ( 'NONE',  ( 0.9873396505805591694, 0.1113553986120547346, 0.6840551181102363376 ) ) ;
#18796 = VERTEX_POINT ( 'NONE', #11206 ) ;
#18797 = CARTESIAN_POINT ( 'NONE',  ( 0.07444174185955065859, 0.01127508805474972294, 0.1797182628040039087 ) ) ;
#18798 = PRODUCT ( 'Base Plate', 'Base Plate', '', ( #24502 ) ) ;
#18799 = PLANE ( 'NONE',  #33194 ) ;
#18800 = CARTESIAN_POINT ( 'NONE',  ( 1.002407869896990045, 0.1264236179284866091, 1.601870078686393750 ) ) ;
#18801 = CONICAL_SURFACE ( 'NONE', #15002, 0.09842519685039370636, 0.9599310885968824758 ) ;
#18803 = CARTESIAN_POINT ( 'NONE',  ( 1.033464566929134687, 0.06523048226347956391, 1.902066929133858553 ) ) ;
#18802 = CARTESIAN_POINT ( 'NONE',  ( 0.1588779435336241663, -0.09971251034085006071, 0.1082054717951722450 ) ) ;
#18804 = DIRECTION ( 'NONE',  ( 0.000000000000000000, 0.000000000000000000, 1.000000000000000000 ) ) ;
#18805 = CARTESIAN_POINT ( 'NONE',  ( -0.07405724077823318263, -0.1653543306548978520, -0.1787899950787401604 ) ) ;
#18806 = ORIENTED_EDGE ( 'NONE', *, *, #5038, .F. ) ;
#18807 = CARTESIAN_POINT ( 'NONE',  ( -0.4330708661417345673, 3.105646754637360326E-15, -0.9891732283464566011 ) ) ;
#18808 = CARTESIAN_POINT ( 'NONE',  ( -0.08438807215028237829, -0.09131796649078639805, 0.2367113086201506622 ) ) ;
#18809 = EDGE_LOOP ( 'NONE', ( #3232, #1453, #32864, #5140 ) ) ;
#18810 = CARTESIAN_POINT ( 'NONE',  ( 0.6971942568897648851, -0.07405724077823297447, 0.8759842519147408302 ) ) ;
#18811 = CARTESIAN_POINT ( 'NONE',  ( 0.06523048226347956391, 0.04872047254847188674, -0.1574803149606300301 ) ) ;
#18812 = CARTESIAN_POINT ( 'NONE',  ( -0.8019270111902717657, 0.1787899950787401604, 1.299212598371432215 ) ) ;
#18813 = AXIS2_PLACEMENT_3D ( 'NONE', #17466, #17704, #43335 ) ;
#18814 = AXIS2_PLACEMENT_3D ( 'NONE', #35865, #18127, #43515 ) ;
#18815 = ORIENTED_EDGE ( 'NONE', *, *, #3239, .F. ) ;
#18816 = CARTESIAN_POINT ( 'NONE',  ( -1.284448818897637956, -0.3937007874015748254, 1.181102362204724310 ) ) ;
#18817 = CARTESIAN_POINT ( 'NONE',  ( -0.8019270111902717657, 0.1787899950787401604, 0.3149606298674962890 ) ) ;
#18818 = DIRECTION ( 'NONE',  ( -1.000000000000000000, 0.000000000000000000, 0.000000000000000000 ) ) ;
#18819 = CARTESIAN_POINT ( 'NONE',  ( 0.7185039370078739607, 1.928577636452523993E-17, 0.8070866140657008136 ) ) ;
#18820 = CARTESIAN_POINT ( 'NONE',  ( 0.1264236179284866091, -0.9760097950008916889, -0.1264236179284866091 ) ) ;
#18821 = EDGE_LOOP ( 'NONE', ( #7577, #17979, #25806, #37741 ) ) ;
#18822 = CARTESIAN_POINT ( 'NONE',  ( -0.1264236179284866091, 0.1520669291876218521, -0.1264236179284866091 ) ) ;
#18823 = ORIENTED_EDGE ( 'NONE', *, *, #17399, .T. ) ;
#18824 = CARTESIAN_POINT ( 'NONE',  ( 0.6971942568897648851, 0.07405724077823318263, 1.023622047190330342 ) ) ;
#18825 = CYLINDRICAL_SURFACE ( 'NONE', #9291, 0.09842519685039370636 ) ;
#18826 = EDGE_CURVE ( 'NONE', #44566, #22983, #30760, .T. ) ;
#18827 = DIRECTION ( 'NONE',  ( 1.000000000000000000, 0.000000000000000000, 0.000000000000000000 ) ) ;
#18828 = VECTOR ( 'NONE', #37738, 39.37007874015748143 ) ;
#18829 = CARTESIAN_POINT ( 'NONE',  ( 0.07405724077823318263, -0.5295275590013543976, -0.1787899950787401604 ) ) ;
#18830 = EDGE_CURVE ( 'NONE', #30077, #7776, #34661, .T. ) ;
#18831 = CARTESIAN_POINT ( 'NONE',  ( -1.054774247047244540, -0.07405724077823318263, 0.1033464566391499029 ) ) ;
#18832 = CARTESIAN_POINT ( 'NONE',  ( -0.9412147342319837628, 0.1574803149606300301, 0.8833661417322832277 ) ) ;
#18833 = CARTESIAN_POINT ( 'NONE',  ( 0.3849708276051176936, -3.032960542342102697E-32, 0.09842519685039370636 ) ) ;
#18834 = CARTESIAN_POINT ( 'NONE',  ( -0.1270800023317771588, -0.9409886914728091689, 0.1270800023317771588 ) ) ;
#18835 = CARTESIAN_POINT ( 'NONE',  ( -0.7185039370078739607, 1.928577636452523993E-17, 0.4133858266641259882 ) ) ;
#18836 = CARTESIAN_POINT ( 'NONE',  ( -0.7646288533564489232, 0.1113553986120547346, 1.550196850286173156 ) ) ;
#18837 = CARTESIAN_POINT ( 'NONE',  ( 1.002407869896990045, 0.1264236179284866091, 0.9768700786863937502 ) ) ;
#18838 = CARTESIAN_POINT ( 'NONE',  ( 0.8759842519685039353, 0.1787899950787401882, 1.370570866087968520 ) ) ;
#18839 = CIRCLE ( 'NONE', #35587, 0.1377952755905521298 ) ;
#18840 = CARTESIAN_POINT ( 'NONE',  ( 0.8107537697050253289, -0.1574803149606297803, 1.454232283464566677 ) ) ;
#18842 = FACE_OUTER_BOUND ( 'NONE', #43143, .T. ) ;
#18841 = CARTESIAN_POINT ( 'NONE',  ( 0.7461016248840900422, -0.1094034688171133807, 1.985470781864962841 ) ) ;
#18843 = DIRECTION ( 'NONE',  ( 0.000000000000000000, -1.000000000000000000, 0.000000000000000000 ) ) ;
#18845 = CARTESIAN_POINT ( 'NONE',  ( 0.1563805530828631662, 0.1352584698612726566, 0.04649480693109582508 ) ) ;
#18844 = CARTESIAN_POINT ( 'NONE',  ( 1.002407869896990045, 0.1264236179284866091, 0.8144685038832440993 ) ) ;
#18846 = CARTESIAN_POINT ( 'NONE',  ( -1.094772975963752103E-17, -0.7583661416785196785, -0.1787899950787401882 ) ) ;
#18847 = EDGE_LOOP ( 'NONE', ( #38322, #22735, #32466, #26872 ) ) ;
#18848 = DIRECTION ( 'NONE',  ( 1.144917494144692682E-16, -3.972230510298676574E-31, 1.000000000000000000 ) ) ;
#18849 = CARTESIAN_POINT ( 'NONE',  ( 0.1574803149606299191, 0.1200787401574803237, 2.850509043694854679E-09 ) ) ;
#18850 = CARTESIAN_POINT ( 'NONE',  ( 0.8759842519685039353, -0.1787899950787401882, 1.114665354276944909 ) ) ;
#18851 = CARTESIAN_POINT ( 'NONE',  ( 2.892866454678787531E-17, -1.631889763779527547, 0.1574803149606299191 ) ) ;
#18852 = ADVANCED_FACE ( 'NONE', ( #9724 ), #27253, .T. ) ;
#18853 = LINE ( 'NONE', #11220, #23743 ) ;
#18854 = VERTEX_POINT ( 'NONE', #15983 ) ;
#18855 = DIRECTION ( 'NONE',  ( 1.000000000000000000, 0.000000000000000000, 0.000000000000000000 ) ) ;
#18856 = CARTESIAN_POINT ( 'NONE',  ( -0.6971942568897637749, 2.189545951927499583E-17, 0.1993110235682838682 ) ) ;
#18857 = CARTESIAN_POINT ( 'NONE',  ( -9.642888182262618425E-18, 0.1200787401574803237, -0.1574803149606299191 ) ) ;
#18858 = CARTESIAN_POINT ( 'NONE',  ( 1.033464566929133799, 0.000000000000000000, 0.3543307085538902057 ) ) ;
#18859 = CARTESIAN_POINT ( 'NONE',  ( -0.8759842519685039353, -0.1787899950787401882, 1.705216535379307174 ) ) ;
#18860 = CARTESIAN_POINT ( 'NONE',  ( -0.8019270111902716547, 0.1787899950787401604, 0.8612204723871810241 ) ) ;
#18861 = CARTESIAN_POINT ( 'NONE',  ( -0.9500414927467378812, 0.1787899950787401604, 0.4675196849856070869 ) ) ;
#18862 = CARTESIAN_POINT ( 'NONE',  ( 0.1574803149606300301, -0.03986220461688239070, 0.06523048226347956391 ) ) ;
#18863 = DIRECTION ( 'NONE',  ( -0.000000000000000000, -0.2126700594527834443, 0.9771240687918547607 ) ) ;
#18864 = CARTESIAN_POINT ( 'NONE',  ( -1.033464566929133799, 1.928577636452524610E-17, 2.869337061179095023E-17 ) ) ;
#18865 = CARTESIAN_POINT ( 'NONE',  ( 0.6971942568897626646, -0.07405724077823297447, 0.04429133852891373180 ) ) ;
#18866 = CARTESIAN_POINT ( 'NONE',  ( 0.000000000000000000, -0.09842519685039370636, 0.000000000000000000 ) ) ;
#18867 = CARTESIAN_POINT ( 'NONE',  ( 0.07405724077823318263, -0.4617381414575855159, -0.1787899950787401604 ) ) ;
#18868 = CARTESIAN_POINT ( 'NONE',  ( -0.2298521815382791322, -0.08955978675932835253, 0.05126285459619552010 ) ) ;
#18869 = FACE_OUTER_BOUND ( 'NONE', #40537, .T. ) ;
#18870 = CARTESIAN_POINT ( 'NONE',  ( 0.3547871005709968273, 4.766607801171850497E-17, 0.000000000000000000 ) ) ;
#18871 = ORIENTED_EDGE ( 'NONE', *, *, #13116, .T. ) ;
#18872 = ADVANCED_FACE ( 'NONE', ( #45414 ), #46124, .T. ) ;
#18873 = CARTESIAN_POINT ( 'NONE',  ( -1.181162989532618060E-16, -0.0009842519685041700977, -0.2952755905511816326 ) ) ;
#18874 = CARTESIAN_POINT ( 'NONE',  ( -0.7495606340400177148, 0.1264236179284866091, 0.3912401574265515491 ) ) ;
#18875 = CARTESIAN_POINT ( 'NONE',  ( 0.1264236179284866091, -1.733883810748923171, 0.1264236179284866091 ) ) ;
#18876 = ADVANCED_FACE ( 'NONE', ( #16217 ), #17725, .T. ) ;
#18877 = EDGE_LOOP ( 'NONE', ( #44108, #15226, #23778, #11992 ) ) ;
#18878 = VERTEX_POINT ( 'NONE', #16906 ) ;
#18879 = CARTESIAN_POINT ( 'NONE',  ( -0.9500414927467377701, -0.1787899950787401604, 1.437007873961985593 ) ) ;
#18880 = EDGE_LOOP ( 'NONE', ( #45403, #35109, #42956, #26285 ) ) ;
#18881 = EDGE_CURVE ( 'NONE', #26454, #24716, #33442, .T. ) ;
#18882 = CARTESIAN_POINT ( 'NONE',  ( 0.1787899950787401604, -1.282480314906867314, -0.07405724077823318263 ) ) ;
#18883 = CARTESIAN_POINT ( 'NONE',  ( -0.1787899950787401604, -1.494094488135213394, 0.07405724077823318263 ) ) ;
#18884 = AXIS2_PLACEMENT_3D ( 'NONE', #18988, #27168, #26447 ) ;
#18885 = CARTESIAN_POINT ( 'NONE',  ( 0.8759842519685039353, 0.000000000000000000, 2.007874015640504162 ) ) ;
#18886 = CARTESIAN_POINT ( 'NONE',  ( 1.339088206907401712, 0.9211694353599606533, -0.8759842519689764462 ) ) ;
#18887 = CARTESIAN_POINT ( 'NONE',  ( 0.8759842519685039353, -0.1574803149606299191, 0.5118110236220472231 ) ) ;
#18888 = DIRECTION ( 'NONE',  ( 0.000000000000000000, 0.2126700594527834443, -0.9771240687918547607 ) ) ;
#18889 = CARTESIAN_POINT ( 'NONE',  ( -0.9412147342319837628, 0.1574803149606300301, 1.070374015640503496 ) ) ;
#18890 = CARTESIAN_POINT ( 'NONE',  ( 1.054774247047244096, 0.000000000000000000, 0.6176181101824566033 ) ) ;
#18891 = DIRECTION ( 'NONE',  ( -5.464378949326941559E-15, -1.000000000000000000, 0.000000000000000000 ) ) ;
#18892 = CARTESIAN_POINT ( 'NONE',  ( -0.1113553986120547346, -0.2687007874015748254, -0.1113553986120547346 ) ) ;
#18893 = CARTESIAN_POINT ( 'NONE',  ( 0.7646288533564489232, -0.1113553986120547346, 1.993110236112944911 ) ) ;
#18894 = EDGE_LOOP ( 'NONE', ( #12294, #16892, #12768, #11897 ) ) ;
#18895 = CARTESIAN_POINT ( 'NONE',  ( -0.1287886813449822809, -0.09210284872765374387, -0.1240405425130319400 ) ) ;
#18896 = CARTESIAN_POINT ( 'NONE',  ( -1.054774247047244540, -0.07405724077823318263, 1.008858267662772423 ) ) ;
#18897 = CARTESIAN_POINT ( 'NONE',  ( 0.7646288533564489232, 0.1113553986120547346, 0.9694881889763780070 ) ) ;
#18898 = CARTESIAN_POINT ( 'NONE',  ( 1.614954907737318939E-16, -8.878505979408855953E-16, 0.3937007874015748254 ) ) ;
#18899 = CARTESIAN_POINT ( 'NONE',  ( -0.3980944881889761922, 0.1864803149606355237, 0.7480314960629921295 ) ) ;
#18900 = CARTESIAN_POINT ( 'NONE',  ( -0.1695021356517113220, -0.08955111078152680482, -0.02025256367261695639 ) ) ;
#18901 = VERTEX_POINT ( 'NONE', #1326 ) ;
#18902 = DIRECTION ( 'NONE',  ( 0.000000000000000000, -1.000000000000000000, 0.000000000000000000 ) ) ;
#18903 = CARTESIAN_POINT ( 'NONE',  ( 0.8759842519685039353, 0.1787899950787401882, 0.7012795275052913224 ) ) ;
#18904 = ORIENTED_EDGE ( 'NONE', *, *, #7808, .T. ) ;
#18905 = DIRECTION ( 'NONE',  ( -1.000000000000000000, -0.000000000000000000, 0.000000000000000000 ) ) ;
#18906 = CARTESIAN_POINT ( 'NONE',  ( -0.7185039370078739607, 1.928577636452523993E-17, 0.9744094488188976833 ) ) ;
#18907 = CARTESIAN_POINT ( 'NONE',  ( -0.1787899950787401604, -1.572834645615527327, 0.07405724077823318263 ) ) ;
#18908 = CARTESIAN_POINT ( 'NONE',  ( 0.1264236179284866091, -0.6993110235682834519, 0.1264236179284866091 ) ) ;
#18909 = CARTESIAN_POINT ( 'NONE',  ( -0.06523048226347956391, -1.201279527559055538, 0.1574803149606297803 ) ) ;
#18910 = CARTESIAN_POINT ( 'NONE',  ( 0.7185039370078746268, 0.06523048226347956391, 1.198326771546015967 ) ) ;
#18911 = DIRECTION ( 'NONE',  ( -3.469446951953613794E-15, -1.000000000000000000, -1.118797478067273468E-31 ) ) ;
#18912 = EDGE_LOOP ( 'NONE', ( #46093, #4696, #36297, #24814, #41189, #21892, #983, #28641, #38448, #20562, #7830, #32610 ) ) ;
#18913 = VERTEX_POINT ( 'NONE', #30604 ) ;
#18914 = CARTESIAN_POINT ( 'NONE',  ( -1.002407869896990045, -0.1264236179284866091, 1.833169291284818758 ) ) ;
#18915 = CARTESIAN_POINT ( 'NONE',  ( 0.8759842519685039353, -0.1787899950787401882, 1.749507873961984483 ) ) ;
#18916 = CARTESIAN_POINT ( 'NONE',  ( -0.06523048226347956391, -1.309547243986961540, 0.1574803149606297803 ) ) ;
#18917 = DIRECTION ( 'NONE',  ( -1.000000000000000000, 0.000000000000000000, 0.000000000000000000 ) ) ;
#18918 = CARTESIAN_POINT ( 'NONE',  ( 0.7495606340400177148, 0.1264236179284866091, 0.3567913385289137596 ) ) ;
#18919 = CARTESIAN_POINT ( 'NONE',  ( -0.7185039370078739607, 1.928577636452523993E-17, 1.515748031388535200 ) ) ;
#18920 = CARTESIAN_POINT ( 'NONE',  ( -0.8019270111902716547, -0.1787899950787401604, 1.269685039316314601 ) ) ;
#18921 = CARTESIAN_POINT ( 'NONE',  ( -1.054774247047244540, 0.07405724077823318263, 0.8907480314422986378 ) ) ;
#18922 = AXIS2_PLACEMENT_3D ( 'NONE', #14516, #7077, #25786 ) ;
#18923 = CARTESIAN_POINT ( 'NONE',  ( -0.8759842519685039353, 0.1787899950787401882, 0.1550196849856066983 ) ) ;
#18924 = CARTESIAN_POINT ( 'NONE',  ( 0.09072581850463573572, 0.09340956239926197224, 0.2330524951300412539 ) ) ;
#18925 = CARTESIAN_POINT ( 'NONE',  ( -0.9500414927467378812, 0.1787899950787401604, 1.609251968450173376 ) ) ;
#18926 = CARTESIAN_POINT ( 'NONE',  ( -0.8107537697050253289, -0.1574803149606297803, 1.916830708553890705 ) ) ;
#18927 = ORIENTED_EDGE ( 'NONE', *, *, #10520, .T. ) ;
#18928 = CARTESIAN_POINT ( 'NONE',  ( -0.9412147342319837628, -0.1574803149606297803, 1.537893700787401841 ) ) ;
#18929 = CARTESIAN_POINT ( 'NONE',  ( 0.1805937969716511771, -0.4173683960833115547, -0.9859272360519073519 ) ) ;
#18930 = EDGE_CURVE ( 'NONE', #39413, #10497, #15453, .T. ) ;
#18931 = CARTESIAN_POINT ( 'NONE',  ( 0.7495606340400177148, 0.1264236179284866091, 1.537893700733637736 ) ) ;
#18932 = CARTESIAN_POINT ( 'NONE',  ( -0.2183122970338342572, -0.09842519685039370636, -0.1145706962327193018 ) ) ;
#18933 = CARTESIAN_POINT ( 'NONE',  ( 0.9873396505805591694, -0.1113553986120547346, 1.018700787294047228 ) ) ;
#18934 = ORIENTED_EDGE ( 'NONE', *, *, #28623, .T. ) ;
#18935 = ADVANCED_FACE ( 'NONE', ( #34418 ), #41805, .T. ) ;
#18936 = ORIENTED_EDGE ( 'NONE', *, *, #17593, .T. ) ;
#18937 = EDGE_LOOP ( 'NONE', ( #43498, #36237, #40183, #20675 ) ) ;
#18938 = EDGE_CURVE ( 'NONE', #20645, #2888, #86, .T. ) ;
#18939 = CARTESIAN_POINT ( 'NONE',  ( 0.1264236179284866091, -0.8469488188438739629, -0.1264236179284866091 ) ) ;
#18940 = CARTESIAN_POINT ( 'NONE',  ( -0.1264236179284866091, -1.058562992072220377, 0.1264236179284866091 ) ) ;
#18941 = VECTOR ( 'NONE', #2510, 39.37007874015748143 ) ;
#18942 = PRESENTATION_STYLE_ASSIGNMENT (( #22306 ) ) ;
#18943 = ( NAMED_UNIT ( * ) PLANE_ANGLE_UNIT ( ) SI_UNIT ( $, .RADIAN. ) ) ;
#18944 = CARTESIAN_POINT ( 'NONE',  ( -0.07444174185955065859, -0.3627406599767461493, -0.1797182628040039087 ) ) ;
#18945 = DIRECTION ( 'NONE',  ( -0.000000000000000000, 1.000000000000000000, -0.000000000000000000 ) ) ;
#18946 = CARTESIAN_POINT ( 'NONE',  ( -0.9412147342319837628, 0.1574803149606300301, 1.070374015640503496 ) ) ;
#18947 = CARTESIAN_POINT ( 'NONE',  ( 0.7495606340400177148, -0.1264236179284866091, 0.8341535432533228045 ) ) ;
#18948 = AXIS2_PLACEMENT_3D ( 'NONE', #23828, #13513, #24305 ) ;
#18949 = CARTESIAN_POINT ( 'NONE',  ( -0.1574803149606299191, -0.5010918323780659822, -0.8705539716229625524 ) ) ;
#18951 = CYLINDRICAL_SURFACE ( 'NONE', #27804, 0.2362204724409449064 ) ;
#18950 = DIRECTION ( 'NONE',  ( -5.159318851433039196E-16, -0.6156614753256610673, -0.7880107536067199048 ) ) ;
#18952 = CARTESIAN_POINT ( 'NONE',  ( 0.9873396505805591694, -0.1113553986120547346, 1.264763779527559029 ) ) ;
#18953 = CARTESIAN_POINT ( 'NONE',  ( 0.8759842519685039353, 0.1787899950787401882, 1.769192913332062966 ) ) ;
#18954 = CARTESIAN_POINT ( 'NONE',  ( 0.8107537697050254399, -0.1574803149606297803, 1.877460629813732407 ) ) ;
#18955 = CARTESIAN_POINT ( 'NONE',  ( 0.8107537697050234415, -0.1574803149606297803, 0.07627952755905517690 ) ) ;
#18956 = FACE_OUTER_BOUND ( 'NONE', #23490, .T. ) ;
#18958 = CARTESIAN_POINT ( 'NONE',  ( -0.1264236179284866091, -0.2859251967966303098, -0.1264236179284866091 ) ) ;
#18957 = CARTESIAN_POINT ( 'NONE',  ( 2.892866454678787531E-17, -0.9527559054042835651, 0.1574803149606299191 ) ) ;
#18959 = CARTESIAN_POINT ( 'NONE',  ( 0.1577586585109200246, 0.1055041328676883661, 0.09810528961771382284 ) ) ;
#18960 = CARTESIAN_POINT ( 'NONE',  ( 0.1264236179284866091, -1.245570866087968520, 0.1264236179284866091 ) ) ;
#18961 = CARTESIAN_POINT ( 'NONE',  ( 1.054774247047244096, 0.000000000000000000, 0.2239173227808822775 ) ) ;
#18962 = ( BOUNDED_CURVE ( )  B_SPLINE_CURVE ( 2, ( #1158, #45236, #41628, #30913, #42110, #16742, #4999, #12699, #44995 ),
 .UNSPECIFIED., .F., .T. ) 
 B_SPLINE_CURVE_WITH_KNOTS ( ( 3, 2, 2, 2, 3 ),
 ( 0.2800000000000000266, 0.2824999999999999734, 0.2849999999999999756, 0.2874999999999999778, 0.2899999999999999800 ),
 .UNSPECIFIED. ) 
 CURVE ( )  GEOMETRIC_REPRESENTATION_ITEM ( )  RATIONAL_B_SPLINE_CURVE ( ( 1.000000000000000000, 0.9238795325112849621, 1.000000000000000000, 0.9238795325112869605, 1.000000000000000000, 0.9238795325112869605, 1.000000000000000000, 0.9238795325112869605, 1.000000000000000000 ) ) 
 REPRESENTATION_ITEM ( '' )  ) ;
#18963 = CARTESIAN_POINT ( 'NONE',  ( 0.7185039370078746268, 0.06523048226347956391, 1.119586614065702035 ) ) ;
#18964 = CARTESIAN_POINT ( 'NONE',  ( -0.7495606340400177148, -0.1264236179284866091, 1.818405511757259729 ) ) ;
#18965 = ORIENTED_EDGE ( 'NONE', *, *, #8699, .T. ) ;
#18966 = CARTESIAN_POINT ( 'NONE',  ( -0.8759842519685039353, 0.1787899950787401882, 1.257381889710015743 ) ) ;
#18967 = CARTESIAN_POINT ( 'NONE',  ( -0.9873396505805591694, 0.1113553986120547346, 0.8809055118110236116 ) ) ;
#18968 = CARTESIAN_POINT ( 'NONE',  ( -1.002407869896990045, -0.1264236179284866091, 1.040846456639149764 ) ) ;
#18969 = EDGE_CURVE ( 'NONE', #2757, #19233, #12859, .T. ) ;
#18970 = CARTESIAN_POINT ( 'NONE',  ( -0.07620458454312968588, -0.09842501845840670449, -0.1617485411237021276 ) ) ;
#18971 = CARTESIAN_POINT ( 'NONE',  ( 1.033464566929133799, 0.000000000000000000, 0.03937007863263043694 ) ) ;
#18972 = CARTESIAN_POINT ( 'NONE',  ( 0.6971942568897648851, -0.07405724077823297447, 0.4822834645131655606 ) ) ;
#18973 = CARTESIAN_POINT ( 'NONE',  ( -1.054774247047244540, 0.07405724077823318263, 0.4183070865604096578 ) ) ;
#18974 = CARTESIAN_POINT ( 'NONE',  ( 1.033464566929134687, 0.06523048226347956391, 1.734744094380662904 ) ) ;
#18975 = VERTEX_POINT ( 'NONE', #9004 ) ;
#18976 = ORIENTED_EDGE ( 'NONE', *, *, #5081, .F. ) ;
#18977 = FACE_OUTER_BOUND ( 'NONE', #4537, .T. ) ;
#18978 = CARTESIAN_POINT ( 'NONE',  ( 0.8019270111902717657, 0.1787899950787401604, 0.9055118109698585549 ) ) ;
#18979 = CARTESIAN_POINT ( 'NONE',  ( -0.7646288533564489232, 0.1113553986120547346, 0.2214566929133858220 ) ) ;
#18980 = ADVANCED_FACE ( 'NONE', ( #45170 ), #27953, .T. ) ;
#18981 = CARTESIAN_POINT ( 'NONE',  ( 0.8759842519685039353, -0.1787899950787401882, 1.198326771599779628 ) ) ;
#18982 = CARTESIAN_POINT ( 'NONE',  ( 0.5966535433070866423, 0.000000000000000000, 0.000000000000000000 ) ) ;
#18983 = EDGE_LOOP ( 'NONE', ( #28981, #22805, #29782, #3297, #34264 ) ) ;
#18984 = DIRECTION ( 'NONE',  ( 0.000000000000000000, 0.000000000000000000, 1.000000000000000000 ) ) ;
#18985 = CARTESIAN_POINT ( 'NONE',  ( -0.8759842519685039353, -0.1787899950787401882, 0.8833661416785196785 ) ) ;
#18986 = AXIS2_PLACEMENT_3D ( 'NONE', #27348, #46445, #42382 ) ;
#18987 = ( BOUNDED_CURVE ( )  B_SPLINE_CURVE ( 2, ( #30640, #23194, #41357, #38511, #33771, #15542, #37808, #45201, #12425 ),
 .UNSPECIFIED., .F., .F. ) 
 B_SPLINE_CURVE_WITH_KNOTS ( ( 3, 2, 2, 2, 3 ),
 ( 0.8399999999999999689, 0.8425000000000000266, 0.8449999999999999734, 0.8475000000000000311, 0.8499999999999999778 ),
 .UNSPECIFIED. ) 
 CURVE ( )  GEOMETRIC_REPRESENTATION_ITEM ( )  RATIONAL_B_SPLINE_CURVE ( ( 1.000000000000000000, 0.9238795325112869605, 1.000000000000000000, 0.9238795325112869605, 1.000000000000000000, 0.9238795325112869605, 1.000000000000000000, 0.9238795325112869605, 1.000000000000000000 ) ) 
 REPRESENTATION_ITEM ( '' )  ) ;
#18988 = CARTESIAN_POINT ( 'NONE',  ( 0.8759842519685039353, 0.000000000000000000, 4.498031496062992574 ) ) ;
#18989 = CARTESIAN_POINT ( 'NONE',  ( 0.8107537697050234415, -0.1574803149606297803, 0.3125000000000000000 ) ) ;
#18990 = CARTESIAN_POINT ( 'NONE',  ( -0.1787899950787401604, -1.431226330433964078, 0.07405724077823318263 ) ) ;
#18991 = ORIENTED_EDGE ( 'NONE', *, *, #30363, .F. ) ;
#18992 = CARTESIAN_POINT ( 'NONE',  ( -1.094772975963752103E-17, -0.4434055117572598959, -0.1787899950787401882 ) ) ;
#18993 = LINE ( 'NONE', #14479, #27764 ) ;
#18994 = EDGE_LOOP ( 'NONE', ( #6967, #2311, #46388, #16160, #33239, #43676 ) ) ;
#18995 = CARTESIAN_POINT ( 'NONE',  ( 0.8019270111902717657, 0.1787899950787401604, 1.254921259788757348 ) ) ;
#18996 = CARTESIAN_POINT ( 'NONE',  ( 0.4736248074375882244, -0.09842519685039370636, 1.555605046820500048 ) ) ;
#18997 = FACE_OUTER_BOUND ( 'NONE', #31415, .T. ) ;
#18998 = CARTESIAN_POINT ( 'NONE',  ( 0.8019270111902717657, 0.1787899950787401604, 0.1525590550643468046 ) ) ;
#18999 = CARTESIAN_POINT ( 'NONE',  ( 0.1787899950787401604, -1.759842519631276581, 0.07405724077823318263 ) ) ;
#19000 = CARTESIAN_POINT ( 'NONE',  ( -0.07405724077823318263, -1.700787401521039355, -0.1787899950787401604 ) ) ;
#19001 = CARTESIAN_POINT ( 'NONE',  ( 1.033464566929133799, 0.000000000000000000, 1.348425196850393748 ) ) ;
#19002 = CARTESIAN_POINT ( 'NONE',  ( -1.002407869896990045, 0.1264236179284866091, 0.7012795275052913224 ) ) ;
#19004 = DIRECTION ( 'NONE',  ( -1.000000000000000000, -0.000000000000000000, -0.000000000000000000 ) ) ;
#19003 = CARTESIAN_POINT ( 'NONE',  ( -0.1574803149606297803, -0.6943897637795268807, 0.06523048226347956391 ) ) ;
#19005 = CARTESIAN_POINT ( 'NONE',  ( -1.100456976456230270E-17, -1.388823337142100378, -0.1797182628040039365 ) ) ;
#19006 = DIRECTION ( 'NONE',  ( 0.000000000000000000, 0.000000000000000000, 1.000000000000000000 ) ) ;
#19007 = CARTESIAN_POINT ( 'NONE',  ( 0.6971942568897648851, 0.07405724077823318263, 1.382874015694268044 ) ) ;
#19008 = CARTESIAN_POINT ( 'NONE',  ( 1.054774247047244540, 0.07405724077823318263, 1.756889763725764553 ) ) ;
#19009 = CARTESIAN_POINT ( 'NONE',  ( 1.054774247047244096, 0.000000000000000000, 0.2583661416785200671 ) ) ;
#19010 = CARTESIAN_POINT ( 'NONE',  ( 0.8759842519685039353, 0.1574803149606299191, 0.1377952755905511861 ) ) ;
#19011 = CARTESIAN_POINT ( 'NONE',  ( -1.033464566929134687, 0.06523048226347956391, 1.508366141732284671 ) ) ;
#19012 = CARTESIAN_POINT ( 'NONE',  ( 0.1476377952755906220, -0.2237541348899636795, -1.272196386806235813 ) ) ;
#19014 = CARTESIAN_POINT ( 'NONE',  ( 0.1184675242425320824, -0.09842519685039370636, 1.713085361781127913 ) ) ;
#19013 = CARTESIAN_POINT ( 'NONE',  ( -0.1574803149606299191, -0.8051181101286928321, 0.000000000000000000 ) ) ;
#19015 = DIRECTION ( 'NONE',  ( 2.943801717310650128E-16, -1.000000000000000000, -2.355041373848525230E-15 ) ) ;
#19016 = AXIS2_PLACEMENT_3D ( 'NONE', #40375, #7562, #41073 ) ;
#19017 = CARTESIAN_POINT ( 'NONE',  ( 1.054774247047244540, 0.07405724077823318263, 0.3395669290800945039 ) ) ;
#19019 = CARTESIAN_POINT ( 'NONE',  ( -0.7185039370078778465, -0.06523048226348396317, 1.715059055010583089 ) ) ;
#19018 = CARTESIAN_POINT ( 'NONE',  ( 0.9500414927467377701, 0.1787899950787401604, 1.249999999946235896 ) ) ;
#19020 = LINE ( 'NONE', #19738, #27385 ) ;
#19021 = CARTESIAN_POINT ( 'NONE',  ( -0.1574803149606299191, 1.928577636452524610E-17, -0.2357204724409448504 ) ) ;
#19022 = CARTESIAN_POINT ( 'NONE',  ( -1.054774247047244540, 0.07405724077823318263, 1.363188976324188895 ) ) ;
#19023 = CARTESIAN_POINT ( 'NONE',  ( 0.8759842519685039353, -0.1574803149606299191, 0.5807086613097960370 ) ) ;
#19024 = ORIENTED_EDGE ( 'NONE', *, *, #42133, .F. ) ;
#19025 = CARTESIAN_POINT ( 'NONE',  ( 0.8479045121278329100, 0.1739705042521020872, 0.03937007862467874209 ) ) ;
#19026 = ORIENTED_EDGE ( 'NONE', *, *, #24896, .F. ) ;
#19027 = CARTESIAN_POINT ( 'NONE',  ( -0.1270800023317771588, -0.07484695918934468339, 0.1270800023317771588 ) ) ;
#19028 = CARTESIAN_POINT ( 'NONE',  ( 0.07405724077823318263, -1.277559055064345861, -0.1787899950787401604 ) ) ;
#19029 = CARTESIAN_POINT ( 'NONE',  ( -0.8759842519685039353, 0.1574803149606299191, 1.112204724301921299 ) ) ;
#19030 = CARTESIAN_POINT ( 'NONE',  ( 0.8019270111902717657, -0.1787899950787401604, 1.545275590497416696 ) ) ;
#19031 = CARTESIAN_POINT ( 'NONE',  ( -1.033464566929133799, 0.000000000000000000, 1.269685039370078705 ) ) ;
#19032 = EDGE_CURVE ( 'NONE', #8850, #21023, #12392, .T. ) ;
#19033 = CYLINDRICAL_SURFACE ( 'NONE', #5202, 0.1624015748031501782 ) ;
#19035 = CARTESIAN_POINT ( 'NONE',  ( -0.8107537697050234415, -0.1574803149606297803, 0.1156496062992125873 ) ) ;
#19034 = CARTESIAN_POINT ( 'NONE',  ( 0.1644020957507539848, -0.1623118080249112138, 7.560884646099310910E-18 ) ) ;
#19036 = CARTESIAN_POINT ( 'NONE',  ( 1.054774247047244096, 0.000000000000000000, 0.06643700782025216411 ) ) ;
#19037 = CARTESIAN_POINT ( 'NONE',  ( -0.1787899950787401882, -0.1579724408911182820, 0.000000000000000000 ) ) ;
#19038 = ORIENTED_EDGE ( 'NONE', *, *, #42509, .T. ) ;
#19039 = EDGE_CURVE ( 'NONE', #11471, #24545, #41644, .T. ) ;
#19040 = LENGTH_MEASURE_WITH_UNIT ( LENGTH_MEASURE( 0.02539999999999999897 ), #34557 ) ;
#19041 = EDGE_CURVE ( 'NONE', #16635, #24379, #31625, .T. ) ;
#19042 = CARTESIAN_POINT ( 'NONE',  ( 0.8019270111902716547, -0.1787899950787401604, 0.9202755904974182499 ) ) ;
#19043 = CARTESIAN_POINT ( 'NONE',  ( -0.8019270111902716547, 0.1787899950787401604, 1.530511810969859221 ) ) ;
#19044 = CARTESIAN_POINT ( 'NONE',  ( 0.1574803149606299191, 0.001968504044534917247, -1.928577636452523993E-17 ) ) ;
#19045 = CARTESIAN_POINT ( 'NONE',  ( -1.002407869896990045, -0.1264236179284866091, 1.281988188922614125 ) ) ;
#19046 = VERTEX_POINT ( 'NONE', #46593 ) ;
#19047 = EDGE_CURVE ( 'NONE', #4670, #45034, #6099, .T. ) ;
#19048 = CARTESIAN_POINT ( 'NONE',  ( -1.002407869896990045, -0.1264236179284866091, 0.2977362204186775885 ) ) ;
#19049 = CARTESIAN_POINT ( 'NONE',  ( 0.000000000000000000, 0.000000000000000000, -0.0009999999999999347518 ) ) ;
#19050 = CARTESIAN_POINT ( 'NONE',  ( 0.9873396505805591694, 0.1113553986120547346, 0.8710629920184568276 ) ) ;
#19051 = CARTESIAN_POINT ( 'NONE',  ( 0.07405724077823318263, -0.9735491650796336272, -0.1787899950787401604 ) ) ;
#19052 = ORIENTED_EDGE ( 'NONE', *, *, #23872, .T. ) ;
#19054 = VERTEX_POINT ( 'NONE', #13773 ) ;
#19053 = AXIS2_PLACEMENT_3D ( 'NONE', #38663, #5592, #20199 ) ;
#19055 = EDGE_LOOP ( 'NONE', ( #18747, #38030, #33793, #30251, #13575, #9068 ) ) ;
#19056 = CARTESIAN_POINT ( 'NONE',  ( 0.6971942568897637749, 2.189545951927499583E-17, 1.026082677111590513 ) ) ;
#19057 = VECTOR ( 'NONE', #36040, 39.37007874015748143 ) ;
#19058 = LINE ( 'NONE', #30140, #16206 ) ;
#19059 = VECTOR ( 'NONE', #21988, 39.37007874015748143 ) ;
#19060 = DIRECTION ( 'NONE',  ( 0.000000000000000000, 1.000000000000000000, 0.000000000000000000 ) ) ;
#19061 = CARTESIAN_POINT ( 'NONE',  ( -0.8759842519685039353, -0.1787899950787401882, 0.1747047243556852092 ) ) ;
#19062 = CARTESIAN_POINT ( 'NONE',  ( -0.8107537697050253289, -0.1574803149606297803, 0.9424212598425207865 ) ) ;
#19063 = CARTESIAN_POINT ( 'NONE',  ( -0.7185039370078739607, 1.928577636452523993E-17, 1.958661417322834719 ) ) ;
#19064 = CARTESIAN_POINT ( 'NONE',  ( 0.1797182628040039087, -0.9680556206066676106, 0.07444174185955046430 ) ) ;
#19065 = CARTESIAN_POINT ( 'NONE',  ( -0.9873396505805591694, 0.1113553986120547346, 1.934055118002708573 ) ) ;
#19066 = CARTESIAN_POINT ( 'NONE',  ( -0.7646288533564489232, -0.1113553986120547346, 1.599409448711369919 ) ) ;
#19067 = CARTESIAN_POINT ( 'NONE',  ( 0.6971942568897637749, 2.189545951927499583E-17, 0.9128937007336377363 ) ) ;
#19068 = CARTESIAN_POINT ( 'NONE',  ( 0.9412147342319837628, 0.1574803149606300301, 1.434547244094487972 ) ) ;
#19070 = CARTESIAN_POINT ( 'NONE',  ( 1.033464566929133799, 0.000000000000000000, 1.702755905511810885 ) ) ;
#19069 = CARTESIAN_POINT ( 'NONE',  ( 0.7102985908446067809, 0.006325918183498560783, 1.983153498902621159 ) ) ;
#19071 = CYLINDRICAL_SURFACE ( 'NONE', #15203, 0.2952755905511810774 ) ;
#19072 = CARTESIAN_POINT ( 'NONE',  ( -0.1113553986120547346, -0.6820866140657008136, 0.1113553986120547346 ) ) ;
#19074 = DIRECTION ( 'NONE',  ( 1.822029033848725028E-16, 0.000000000000000000, 1.000000000000000000 ) ) ;
#19073 = CARTESIAN_POINT ( 'NONE',  ( 0.8019270111902716547, 0.1787899950787401604, 0.8612204723871810241 ) ) ;
#19075 = AXIS2_PLACEMENT_3D ( 'NONE', #20850, #2397, #35492 ) ;
#19076 = CARTESIAN_POINT ( 'NONE',  ( 0.8759842519685039353, 0.1787899950787401882, 1.847933070812378009 ) ) ;
#19077 = CARTESIAN_POINT ( 'NONE',  ( 0.1787899950787401604, -0.6919291338045056028, 0.07405724077823318263 ) ) ;
#19078 = DIRECTION ( 'NONE',  ( 0.000000000000000000, -0.7880107536067233465, 0.6156614753256566264 ) ) ;
#19079 = VERTEX_POINT ( 'NONE', #3215 ) ;
#19080 = CARTESIAN_POINT ( 'NONE',  ( 0.8070866141732283561, -0.3937007874015746034, -0.8559055118110230342 ) ) ;
#19081 = CARTESIAN_POINT ( 'NONE',  ( -1.054774247047244096, 0.000000000000000000, 1.995570866087968520 ) ) ;
#19082 = CARTESIAN_POINT ( 'NONE',  ( 1.002407869896990045, 0.1264236179284866091, 1.090059055064346527 ) ) ;
#19083 = LINE ( 'NONE', #30400, #40202 ) ;
#19085 = CONICAL_SURFACE ( 'NONE', #19888, 0.09842519685039370636, 0.9599310885968824758 ) ;
#19084 = CARTESIAN_POINT ( 'NONE',  ( -0.1113553986120547346, -1.715551181102362266, 0.1113553986120547346 ) ) ;
#19086 = FACE_OUTER_BOUND ( 'NONE', #17974, .T. ) ;
#19087 = ADVANCED_FACE ( 'NONE', ( #9952 ), #6217, .T. ) ;
#19088 = CARTESIAN_POINT ( 'NONE',  ( -1.054774247047244540, 0.07405724077823318263, 0.4970472440407249226 ) ) ;
#19089 = EDGE_LOOP ( 'NONE', ( #34703, #15056, #9852, #15252 ) ) ;
#19090 = DIRECTION ( 'NONE',  ( 0.000000000000000000, -0.6156614753256596240, -0.7880107536067210150 ) ) ;
#19091 = CARTESIAN_POINT ( 'NONE',  ( -0.7495606340400177148, -0.1264236179284866091, 0.2042322834108035723 ) ) ;
#19092 = CIRCLE ( 'NONE', #43580, 0.2952755905511806334 ) ;
#19093 = CARTESIAN_POINT ( 'NONE',  ( -0.7185039370078746268, 0.06523048226347956391, 0.6176181102362199304 ) ) ;
#19094 = ORIENTED_EDGE ( 'NONE', *, *, #30673, .F. ) ;
#19096 = CARTESIAN_POINT ( 'NONE',  ( -0.1264236179284866091, -1.467027559001354398, -0.1264236179284866091 ) ) ;
#19095 = CARTESIAN_POINT ( 'NONE',  ( 2.892866454678787531E-17, -0.3228346455617642219, 0.1574803149606299191 ) ) ;
#19097 = CARTESIAN_POINT ( 'NONE',  ( 0.7185039370078739607, 1.928577636452523993E-17, 0.3346456691838114450 ) ) ;
#19098 = CARTESIAN_POINT ( 'NONE',  ( -1.002407869896990045, 0.1264236179284866091, 1.798720472387181024 ) ) ;
#19099 = CARTESIAN_POINT ( 'NONE',  ( -0.8759842519685039353, -0.1787899950787401882, 0.8784448818360000022 ) ) ;
#19100 = EDGE_CURVE ( 'NONE', #5993, #21453, #17135, .T. ) ;
#19101 = CARTESIAN_POINT ( 'NONE',  ( -0.7495606340400177148, 0.1264236179284866091, 0.5536417322297008115 ) ) ;
#19102 = SHAPE_REPRESENTATION ( 'Pivot Shaft', ( #20860 ), #43813 ) ;
#19103 = CARTESIAN_POINT ( 'NONE',  ( -0.7185039370078739607, 1.928577636452523993E-17, 1.358267716427907779 ) ) ;
#19104 = CARTESIAN_POINT ( 'NONE',  ( 0.8107537697050254399, -0.1574803149606297803, 0.9817913385826764205 ) ) ;
#19105 = CARTESIAN_POINT ( 'NONE',  ( 0.1235961452251413406, 0.09842519685039370636, -0.2140748031496062798 ) ) ;
#19106 = CARTESIAN_POINT ( 'NONE',  ( -1.033464566929133799, 0.000000000000000000, 1.702755905511810885 ) ) ;
#19107 = CARTESIAN_POINT ( 'NONE',  ( 0.1264236179284866091, -0.5035688501190023203, -0.1264236179284866091 ) ) ;
#19108 = CARTESIAN_POINT ( 'NONE',  ( -0.1499592427265324934, -0.08955956716458957079, -0.1972459155580799095 ) ) ;
#19109 = CARTESIAN_POINT ( 'NONE',  ( -0.7185039370078692977, 0.06523048226347515077, 1.906988188868851797 ) ) ;
#19110 = CARTESIAN_POINT ( 'NONE',  ( 0.9873396505805591694, 0.1113553986120547346, 1.786417322834645605 ) ) ;
#19111 = CARTESIAN_POINT ( 'NONE',  ( 0.2559055096563123688, -0.08274376297360711008, -0.05534801676208721266 ) ) ;
#19112 = CARTESIAN_POINT ( 'NONE',  ( -0.9500414927467378812, -0.1787899950787401604, 0.2509842519147403861 ) ) ;
#19113 = DIRECTION ( 'NONE',  ( 1.822029033848725028E-16, 0.000000000000000000, 1.000000000000000000 ) ) ;
#19115 = ORIENTED_EDGE ( 'NONE', *, *, #41927, .F. ) ;
#19114 = VECTOR ( 'NONE', #31155, 39.37007874015748143 ) ;
#19116 = CARTESIAN_POINT ( 'NONE',  ( 0.4151545546392377273, 4.766607801171850497E-17, 0.000000000000000000 ) ) ;
#19117 = EDGE_LOOP ( 'NONE', ( #20577, #20567, #40641, #29246 ) ) ;
#19118 = CARTESIAN_POINT ( 'NONE',  ( -0.8019270111902716547, 0.1787899950787401604, 1.574803149552536530 ) ) ;
#19119 = CARTESIAN_POINT ( 'NONE',  ( -0.1787899950787401604, -1.380905511757260173, 0.07405724077823318263 ) ) ;
#19120 = VECTOR ( 'NONE', #23256, 39.37007874015748143 ) ;
#19121 = CARTESIAN_POINT ( 'NONE',  ( -0.07405724077823318263, -1.607283464513165949, 0.1787899950787401604 ) ) ;
#19122 = DIRECTION ( 'NONE',  ( 1.000000000000000000, 0.000000000000000000, -1.822029033848725275E-16 ) ) ;
#19123 = CARTESIAN_POINT ( 'NONE',  ( -0.4330708661417340677, 0.1574803149606330277, -0.9891732283464564901 ) ) ;
#19124 = CARTESIAN_POINT ( 'NONE',  ( -1.033464566929134687, 0.06523048226347956391, 1.144192913278300194 ) ) ;
#19125 = CARTESIAN_POINT ( 'NONE',  ( 1.002407869896990045, -0.1264236179284866091, 0.6126968503399370380 ) ) ;
#19126 = DIRECTION ( 'NONE',  ( 0.000000000000000000, 0.000000000000000000, 1.000000000000000000 ) ) ;
#19127 = ORIENTED_EDGE ( 'NONE', *, *, #4092, .T. ) ;
#19128 = CYLINDRICAL_SURFACE ( 'NONE', #10059, 0.3100393700787401619 ) ;
#19129 = EDGE_LOOP ( 'NONE', ( #11010, #9226, #28097, #19990 ) ) ;
#19130 = CARTESIAN_POINT ( 'NONE',  ( 0.2821522309711287368, 0.08090551181102362266, 0.000000000000000000 ) ) ;
#19131 = CARTESIAN_POINT ( 'NONE',  ( -0.7495606340400177148, 0.1264236179284866091, 0.9867125983714331028 ) ) ;
#19132 = CARTESIAN_POINT ( 'NONE',  ( 0.8107537697050253289, -0.1574803149606297803, 1.021161417322834497 ) ) ;
#19133 = DIRECTION ( 'NONE',  ( -1.000000000000000000, 0.000000000000000000, 0.000000000000000000 ) ) ;
#19134 = DIRECTION ( 'NONE',  ( 0.000000000000000000, -0.6156614753256597350, -0.7880107536067207930 ) ) ;
#19135 = CARTESIAN_POINT ( 'NONE',  ( -0.08562028147892762620, -0.08956352913554484207, 0.1336771782244998708 ) ) ;
#19136 = EDGE_LOOP ( 'NONE', ( #22926, #9736, #27564, #21308 ) ) ;
#19137 = CARTESIAN_POINT ( 'NONE',  ( 0.2871444924769520068, 1.495705267341507883, -0.3569552279982047271 ) ) ;
#19138 = B_SPLINE_CURVE_WITH_KNOTS ( 'NONE', 3,
 ( #15355, #14882, #12004, #26624, #4074, #8379, #18924, #19405, #18688, #22526, #25901, #15844, #33584, #1185, #11289, #44319, #37621, #37143, #30467 ),
 .UNSPECIFIED., .F., .F.,
 ( 4, 1, 1, 1, 2, 2, 1, 1, 1, 1, 2, 2, 4 ),
 ( 0.000000000000000000, 0.1249999999999984457, 0.1874999999999978351, 0.2187499999999978351, 0.2343749999999978351, 0.2499999999999978351, 0.3749999999999991673, 0.4375000000000000555, 0.4687500000000004996, 0.4843750000000006106, 0.4921875000000007216, 0.5000000000000007772, 1.000000000000000000 ),
 .UNSPECIFIED. ) ;
#19139 = ORIENTED_EDGE ( 'NONE', *, *, #10512, .T. ) ;
#19140 = CARTESIAN_POINT ( 'NONE',  ( 0.6971942568897637749, 2.189545951927499583E-17, 0.7111220471903307860 ) ) ;
#19141 = CARTESIAN_POINT ( 'NONE',  ( -0.08400343811428674645, 0.09129006187720335730, -0.2369336632580043012 ) ) ;
#19142 = CARTESIAN_POINT ( 'NONE',  ( -9.642888182262618425E-18, -0.03740157480314960925, -0.1574803149606299191 ) ) ;
#19143 = CARTESIAN_POINT ( 'NONE',  ( 0.07405724077823318263, -1.562992125930488196, 0.1787899950787401604 ) ) ;
#19144 = CARTESIAN_POINT ( 'NONE',  ( -0.07405724077823318263, -0.8641732282926931630, 0.1787899950787401604 ) ) ;
#19145 = CARTESIAN_POINT ( 'NONE',  ( -0.1574803149606300301, -1.250492125984252079, -0.06523048226347956391 ) ) ;
#19146 = CARTESIAN_POINT ( 'NONE',  ( 0.7185039370078739607, 1.928577636452523993E-17, 1.122047243986960652 ) ) ;
#19147 = CARTESIAN_POINT ( 'NONE',  ( -1.033464566929134687, -0.06523048226347956391, 1.660925196850393526 ) ) ;
#19148 = EDGE_CURVE ( 'NONE', #21515, #44611, #46360, .T. ) ;
#19149 = AXIS2_PLACEMENT_3D ( 'NONE', #9977, #47347, #2994 ) ;
#19150 = VERTEX_POINT ( 'NONE', #39165 ) ;
#19151 = ORIENTED_EDGE ( 'NONE', *, *, #29884, .T. ) ;
#19152 = CARTESIAN_POINT ( 'NONE',  ( -0.6971942568897637749, 2.189545951927499583E-17, 1.739665354276945131 ) ) ;
#19153 = VERTEX_POINT ( 'NONE', #31778 ) ;
#19154 = CARTESIAN_POINT ( 'NONE',  ( 0.6971942568897648851, 0.07405724077823318263, 1.737204724355685848 ) ) ;
#19155 = CARTESIAN_POINT ( 'NONE',  ( -0.6971942568897626646, 0.07405724077823318263, 0.9104330708123776761 ) ) ;
#19156 = CYLINDRICAL_SURFACE ( 'NONE', #10345, 0.1574803149606299191 ) ;
#19157 = CARTESIAN_POINT ( 'NONE',  ( 0.6971942568897626646, 0.07405724077823318263, 0.2411417322297011168 ) ) ;
#19158 = CIRCLE ( 'NONE', #4603, 0.1574803149606300579 ) ;
#19159 = CARTESIAN_POINT ( 'NONE',  ( -0.7495606340400177148, -0.1264236179284866091, 1.424704724355685181 ) ) ;
#19160 = DIRECTION ( 'NONE',  ( 0.000000000000000000, 0.000000000000000000, 1.000000000000000000 ) ) ;
#19161 = CARTESIAN_POINT ( 'NONE',  ( -1.002407869896990045, -0.1264236179284866091, 1.316437007820252081 ) ) ;
#19162 = EDGE_CURVE ( 'NONE', #21958, #44444, #2971, .T. ) ;
#19163 = CARTESIAN_POINT ( 'NONE',  ( -1.002407869896990045, -0.1264236179284866091, 0.8833661416785196785 ) ) ;
#19164 = CIRCLE ( 'NONE', #26859, 0.1574803149606299191 ) ;
#19165 = CARTESIAN_POINT ( 'NONE',  ( -0.7495606340400177148, -0.1264236179284866091, 0.05167322829269323931 ) ) ;
#19166 = DIRECTION ( 'NONE',  ( 4.750595374550219683E-16, 0.6156614753256610673, 0.7880107536067199048 ) ) ;
#19167 = CARTESIAN_POINT ( 'NONE',  ( -0.8759842519685039353, 0.1787899950787401882, 1.532972440891118060 ) ) ;
#19168 = CARTESIAN_POINT ( 'NONE',  ( -0.7495606340400177148, -0.1264236179284866091, 0.09104330703285078152 ) ) ;
#19169 = CARTESIAN_POINT ( 'NONE',  ( -1.033464566929134687, 0.06523048226347956391, 1.587106299212598826 ) ) ;
#19170 = CARTESIAN_POINT ( 'NONE',  ( 0.9873396505805591694, -0.1113553986120547346, 0.9793307085538898171 ) ) ;
#19171 = CARTESIAN_POINT ( 'NONE',  ( 0.8019270111902716547, 0.1787899950787401604, 1.653543307032850462 ) ) ;
#19172 = CARTESIAN_POINT ( 'NONE',  ( -0.1749533961349706845, -0.09842519685039370636, 0.1544953252376329023 ) ) ;
#19173 = DIRECTION ( 'NONE',  ( 1.000000000000000000, 0.000000000000000000, 0.000000000000000000 ) ) ;
#19174 = CARTESIAN_POINT ( 'NONE',  ( 0.7185039370078746268, 0.06523048226347956391, 0.2928149605223942520 ) ) ;
#19175 = VERTEX_POINT ( 'NONE', #35598 ) ;
#19176 = ORIENTED_EDGE ( 'NONE', *, *, #44093, .F. ) ;
#19177 = CARTESIAN_POINT ( 'NONE',  ( -1.002407869896990045, -0.1264236179284866091, 1.163877952702141672 ) ) ;
#19178 = CARTESIAN_POINT ( 'NONE',  ( -0.1787899950787401604, -0.9133858267178897039, -0.07405724077823318263 ) ) ;
#19179 = EDGE_CURVE ( 'NONE', #41516, #43867, #41353, .T. ) ;
#19180 = CARTESIAN_POINT ( 'NONE',  ( 0.07405724077823318263, -1.090551181048598606, 0.1787899950787401604 ) ) ;
#19181 = FILL_AREA_STYLE ('',( #18482 ) ) ;
#19182 = CARTESIAN_POINT ( 'NONE',  ( 1.054774247047244540, -0.07405724077823318263, 1.830708661363559253 ) ) ;
#19183 = CARTESIAN_POINT ( 'NONE',  ( 0.07444174185955046430, -0.3676619198192658255, -0.1797182628040039087 ) ) ;
#19184 = CARTESIAN_POINT ( 'NONE',  ( 0.1574803149606299191, 0.1102362204724409434, -1.928577636452523993E-17 ) ) ;
#19185 = PRODUCT ( 'Handle Arm Left', 'Handle Arm Left', '', ( #27426 ) ) ;
#19186 = STYLED_ITEM ( 'NONE', ( #25777 ), #20717 ) ;
#19187 = DIRECTION ( 'NONE',  ( 0.000000000000000000, 1.000000000000000000, 0.000000000000000000 ) ) ;
#19188 = CARTESIAN_POINT ( 'NONE',  ( 0.8759842519685039353, 0.1787899950787401882, 0.7406496062454487328 ) ) ;
#19189 = AXIS2_PLACEMENT_3D ( 'NONE', #22976, #16040, #11737 ) ;
#19190 = CARTESIAN_POINT ( 'NONE',  ( -1.033464566929134687, -0.06523048226347956391, 1.572342519577513142 ) ) ;
#19191 = FACE_OUTER_BOUND ( 'NONE', #44539, .T. ) ;
#19192 = CARTESIAN_POINT ( 'NONE',  ( 1.033464566929134687, -0.06523048226347956391, 1.267224409448818978 ) ) ;
#19193 = CARTESIAN_POINT ( 'NONE',  ( 0.8019270111902717657, 0.1787899950787401604, 1.771653543253322249 ) ) ;
#19194 = AXIS2_PLACEMENT_3D ( 'NONE', #43306, #21027, #6650 ) ;
#19195 = ADVANCED_FACE ( 'NONE', ( #29154 ), #22378, .F. ) ;
#19196 = ADVANCED_FACE ( 'NONE', ( #11376 ), #4380, .T. ) ;
#19197 = CARTESIAN_POINT ( 'NONE',  ( 0.7185039370078746268, -0.06523048226347956391, 0.1500984251968505434 ) ) ;
#19198 = FACE_OUTER_BOUND ( 'NONE', #11531, .T. ) ;
#19199 = CARTESIAN_POINT ( 'NONE',  ( -0.1787899950787401882, -0.4384842519147402196, 0.000000000000000000 ) ) ;
#19200 = CYLINDRICAL_SURFACE ( 'NONE', #33150, 0.1574803149606299191 ) ;
#19201 = CARTESIAN_POINT ( 'NONE',  ( 0.1264236179284866091, -1.275098425143086578, -0.1264236179284866091 ) ) ;
#19202 = CARTESIAN_POINT ( 'NONE',  ( 1.002407869896990045, -0.1264236179284866091, 0.2583661416785200671 ) ) ;
#19203 = CARTESIAN_POINT ( 'NONE',  ( 0.7646288533564489232, 0.1113553986120547346, 0.06397637795275590289 ) ) ;
#19204 = EDGE_CURVE ( 'NONE', #22479, #19538, #29862, .T. ) ;
#19205 = CARTESIAN_POINT ( 'NONE',  ( -1.002407869896990045, -0.1264236179284866091, 1.828248031442299082 ) ) ;
#19206 = EDGE_LOOP ( 'NONE', ( #11782, #21463, #23711, #42820 ) ) ;
#19207 = CARTESIAN_POINT ( 'NONE',  ( -1.054774247047244096, 0.000000000000000000, 1.286909448765133801 ) ) ;
#19208 = DIRECTION ( 'NONE',  ( 0.000000000000000000, -1.000000000000000000, 0.000000000000000000 ) ) ;
#19209 = CARTESIAN_POINT ( 'NONE',  ( -9.642888182262618425E-18, -1.208661417215307177, -0.1574803149606299191 ) ) ;
#19210 = CARTESIAN_POINT ( 'NONE',  ( -1.054774247047244096, 0.000000000000000000, 0.5388779527021417826 ) ) ;
#19211 = CARTESIAN_POINT ( 'NONE',  ( 0.8759842519685039353, -0.1787899950787401882, 1.941437007820252081 ) ) ;
#19212 = CARTESIAN_POINT ( 'NONE',  ( -1.054774247047244540, 0.07405724077823318263, 1.087598425143086578 ) ) ;
#19213 = CARTESIAN_POINT ( 'NONE',  ( 0.000000000000000000, 0.000000000000000000, 0.4921259842519685179 ) ) ;
#19214 = CARTESIAN_POINT ( 'NONE',  ( 0.03520570031223819313, -0.09841564447026268647, -0.1752971770356033798 ) ) ;
#19215 = CARTESIAN_POINT ( 'NONE',  ( -0.1574803149606299191, 0.5419727308409657551, -0.7545416139885203766 ) ) ;
#19216 = CARTESIAN_POINT ( 'NONE',  ( 1.002407869896990045, -0.1264236179284866091, 0.4945866141194645849 ) ) ;
#19217 = CARTESIAN_POINT ( 'NONE',  ( -0.6971942568897637749, 2.189545951927499583E-17, 0.3174212597887562382 ) ) ;
#19218 = EDGE_CURVE ( 'NONE', #18975, #39762, #15209, .T. ) ;
#19219 = VERTEX_POINT ( 'NONE', #4622 ) ;
#19220 = ORIENTED_EDGE ( 'NONE', *, *, #31353, .T. ) ;
#19221 = DIRECTION ( 'NONE',  ( 1.000000000000000000, 0.000000000000000000, 0.000000000000000000 ) ) ;
#19222 = ORIENTED_EDGE ( 'NONE', *, *, #25714, .T. ) ;
#19223 = CARTESIAN_POINT ( 'NONE',  ( -0.9873396505805591694, 0.1113553986120547346, 0.1328740157480315098 ) ) ;
#19224 = CARTESIAN_POINT ( 'NONE',  ( 0.7495606340400177148, 0.1264236179284866091, 1.183562992072220599 ) ) ;
#19225 = CARTESIAN_POINT ( 'NONE',  ( -0.2281991160478161473, -0.09851385135380275049, -0.09075334354666182712 ) ) ;
#19226 = VECTOR ( 'NONE', #45930, 39.37007874015748854 ) ;
#19227 = ORIENTED_EDGE ( 'NONE', *, *, #31671, .F. ) ;
#19228 = MECHANICAL_DESIGN_GEOMETRIC_PRESENTATION_REPRESENTATION (  '', ( #28463 ), #41395 ) ;
#19229 = VECTOR ( 'NONE', #44062, 39.37007874015748854 ) ;
#19230 = CARTESIAN_POINT ( 'NONE',  ( -0.7646288533564489232, -0.1113553986120547346, 0.3100393700787401619 ) ) ;
#19231 = CARTESIAN_POINT ( 'NONE',  ( 0.7185039370078739607, 1.928577636452523993E-17, 1.328740157480315043 ) ) ;
#19232 = CARTESIAN_POINT ( 'NONE',  ( 0.07405724077823318263, -1.500123968229239768, 0.1787899950787401604 ) ) ;
#19233 = VERTEX_POINT ( 'NONE', #7761 ) ;
#19234 = CARTESIAN_POINT ( 'NONE',  ( 0.07405724077823318263, -0.3671259841982050798, -0.1787899950787401604 ) ) ;
#19235 = CARTESIAN_POINT ( 'NONE',  ( 0.7185039370078739607, 1.928577636452523993E-17, 0.09842519674286673292 ) ) ;
#19236 = ORIENTED_EDGE ( 'NONE', *, *, #3121, .F. ) ;
#19237 = CARTESIAN_POINT ( 'NONE',  ( 0.3246033735368759610, 4.766607801171850497E-17, 0.000000000000000000 ) ) ;
#19238 = CARTESIAN_POINT ( 'NONE',  ( 0.9412147342319837628, -0.1574803149606297803, 0.7406496061916858498 ) ) ;
#19239 = CARTESIAN_POINT ( 'NONE',  ( -0.1476377952755905387, 1.126631386849005878, -3.440787370833236380 ) ) ;
#19240 = CARTESIAN_POINT ( 'NONE',  ( 1.002407869896990045, -0.1264236179284866091, 0.2140748030958428971 ) ) ;
#19241 = CARTESIAN_POINT ( 'NONE',  ( -0.1264236179284866091, -1.781988188922614347, -0.1264236179284866091 ) ) ;
#19242 = CARTESIAN_POINT ( 'NONE',  ( -0.1264236179284866091, -1.619586614119464585, -0.1264236179284866091 ) ) ;
#19243 = CARTESIAN_POINT ( 'NONE',  ( 0.8070866141732283561, 0.3779527559055118058, 0.7574803149606299524 ) ) ;
#19244 = EDGE_CURVE ( 'NONE', #21725, #43350, #40569, .T. ) ;
#19245 = CARTESIAN_POINT ( 'NONE',  ( 0.01230737760510134012, -0.07955613945526751607, -0.1377952755905511861 ) ) ;
#19246 = ( BOUNDED_CURVE ( )  B_SPLINE_CURVE ( 2, ( #3419, #18036, #32682, #47271, #4329, #22570, #4112, #18963, #29591 ),
 .UNSPECIFIED., .F., .F. ) 
 B_SPLINE_CURVE_WITH_KNOTS ( ( 3, 2, 2, 2, 3 ),
 ( 0.5400000000000000355, 0.5424999999999999822, 0.5450000000000000400, 0.5474999999999999867, 0.5500000000000000444 ),
 .UNSPECIFIED. ) 
 CURVE ( )  GEOMETRIC_REPRESENTATION_ITEM ( )  RATIONAL_B_SPLINE_CURVE ( ( 1.000000000000000000, 0.9238795325112869605, 1.000000000000000000, 0.9238795325112869605, 1.000000000000000000, 0.9238795325112869605, 1.000000000000000000, 0.9238795325112869605, 1.000000000000000000 ) ) 
 REPRESENTATION_ITEM ( '' )  ) ;
#19247 = CARTESIAN_POINT ( 'NONE',  ( -0.7495606340400177148, 0.1264236179284866091, 0.6323818897100157432 ) ) ;
#19249 = DIRECTION ( 'NONE',  ( 0.000000000000000000, 0.000000000000000000, -1.000000000000000000 ) ) ;
#19248 = CARTESIAN_POINT ( 'NONE',  ( 0.06523048226347956391, -0.7091535433070863537, -0.1574803149606300301 ) ) ;
#19250 = CARTESIAN_POINT ( 'NONE',  ( 0.1797182628040039087, -1.435575305646038524, -0.07444174185955065859 ) ) ;
#19251 = DIRECTION ( 'NONE',  ( -1.000000000000000000, 0.000000000000000000, 0.000000000000000000 ) ) ;
#19252 = DIRECTION ( 'NONE',  ( 0.000000000000000000, 0.2126700594527834720, -0.9771240687918549828 ) ) ;
#19253 = CARTESIAN_POINT ( 'NONE',  ( 0.7495606340400177148, 0.1264236179284866091, 1.301673228292692830 ) ) ;
#19254 = CARTESIAN_POINT ( 'NONE',  ( 0.8759842519685039353, 0.1787899950787401882, 1.882381889710015743 ) ) ;
#19255 = EDGE_CURVE ( 'NONE', #34250, #39764, #13822, .T. ) ;
#19256 = VECTOR ( 'NONE', #7982, 39.37007874015748143 ) ;
#19257 = CONICAL_SURFACE ( 'NONE', #36884, 0.1003937007874010356, 0.7853981633978647237 ) ;
#19259 = ORIENTED_EDGE ( 'NONE', *, *, #13388, .F. ) ;
#19258 = CARTESIAN_POINT ( 'NONE',  ( 1.033464566929133799, 0.000000000000000000, 0.1279527559055118058 ) ) ;
#19260 = CARTESIAN_POINT ( 'NONE',  ( 0.7185039370078739607, 1.928577636452523993E-17, 1.171259842519684957 ) ) ;
#19261 = CYLINDRICAL_SURFACE ( 'NONE', #15247, 0.1574803149606299191 ) ;
#19262 = PLANE ( 'NONE',  #22436 ) ;
#19263 = CARTESIAN_POINT ( 'NONE',  ( -0.9412147342319837628, 0.1574803149606300301, 1.227854330601133359 ) ) ;
#19264 = CARTESIAN_POINT ( 'NONE',  ( 1.002407869896990045, -0.1264236179284866091, 0.2928149605761578567 ) ) ;
#19265 = CARTESIAN_POINT ( 'NONE',  ( 0.6971942568897637749, 2.189545951927499583E-17, 1.262303149552535420 ) ) ;
#19266 = CARTESIAN_POINT ( 'NONE',  ( -0.7185039370078739607, 1.928577636452523993E-17, 0.7775590551181102983 ) ) ;
#19267 = CARTESIAN_POINT ( 'NONE',  ( 1.033464566929134687, 0.06523048226347956391, 0.6323818896562525271 ) ) ;
#19268 = ORIENTED_EDGE ( 'NONE', *, *, #23334, .T. ) ;
#19269 = CARTESIAN_POINT ( 'NONE',  ( 0.5358894627757212481, 0.09842519685039370636, 0.000000000000000000 ) ) ;
#19270 = CARTESIAN_POINT ( 'NONE',  ( 0.1574803149606300301, -0.04478346456692917921, -0.06523048226347956391 ) ) ;
#19271 = ORIENTED_EDGE ( 'NONE', *, *, #31516, .F. ) ;
#19272 = CARTESIAN_POINT ( 'NONE',  ( -0.07444174185955065859, -0.04778003005548651927, -0.1797182628040039087 ) ) ;
#19273 = CARTESIAN_POINT ( 'NONE',  ( 0.1787899950787401604, -1.243110236166709459, -0.07405724077823318263 ) ) ;
#19274 = CARTESIAN_POINT ( 'NONE',  ( 0.000000000000000000, -0.09842519685039370636, 0.1574803149606299191 ) ) ;
#19275 = CARTESIAN_POINT ( 'NONE',  ( 0.8019270111902717657, -0.1787899950787401604, 1.584645669237574994 ) ) ;
#19276 = CARTESIAN_POINT ( 'NONE',  ( -0.9412147342319837628, 0.1574803149606300301, 1.237696850393701586 ) ) ;
#19277 = CARTESIAN_POINT ( 'NONE',  ( -1.033464566929133799, 0.000000000000000000, 1.141732283357039357 ) ) ;
#19279 = DIRECTION ( 'NONE',  ( -1.000000000000000000, 0.000000000000000000, 0.000000000000000000 ) ) ;
#19278 = CARTESIAN_POINT ( 'NONE',  ( 0.1566053014577235558, -0.1284161769475049009, 0.05833949276692128316 ) ) ;
#19280 = CARTESIAN_POINT ( 'NONE',  ( -0.9873396505805591694, -0.1113553986120547346, 0.5068897636720007815 ) ) ;
#19281 = UNCERTAINTY_MEASURE_WITH_UNIT (LENGTH_MEASURE( 1.000000000000000082E-05 ), #14903, 'distance_accuracy_value', 'NONE') ;
#19282 = ORIENTED_EDGE ( 'NONE', *, *, #18617, .T. ) ;
#19283 = ( BOUNDED_CURVE ( )  B_SPLINE_CURVE ( 2, ( #29305, #3122, #3837, #36222, #7664, #3608, #22053, #17749, #43854 ),
 .UNSPECIFIED., .F., .F. ) 
 B_SPLINE_CURVE_WITH_KNOTS ( ( 3, 2, 2, 2, 3 ),
 ( 0.2099999999999999922, 0.2124999999999999944, 0.2149999999999999967, 0.2174999999999999989, 0.2200000000000000011 ),
 .UNSPECIFIED. ) 
 CURVE ( )  GEOMETRIC_REPRESENTATION_ITEM ( )  RATIONAL_B_SPLINE_CURVE ( ( 1.000000000000000000, 0.9238795325112869605, 1.000000000000000000, 0.9238795325112869605, 1.000000000000000000, 0.9238795325112869605, 1.000000000000000000, 0.9238795325112869605, 1.000000000000000000 ) ) 
 REPRESENTATION_ITEM ( '' )  ) ;
#19284 = DIRECTION ( 'NONE',  ( -0.000000000000000000, -0.000000000000000000, -1.000000000000000000 ) ) ;
#19285 = VERTEX_POINT ( 'NONE', #11850 ) ;
#19286 = CARTESIAN_POINT ( 'NONE',  ( 0.8759842519685039353, 0.1787899950787401882, 0.9424212597887559051 ) ) ;
#19287 = CARTESIAN_POINT ( 'NONE',  ( -0.8759842519685039353, -0.1787899950787401882, 1.547736220418677089 ) ) ;
#19288 = CARTESIAN_POINT ( 'NONE',  ( 0.06523048226347956391, -0.03001968493184305545, -0.1574803149606300301 ) ) ;
#19289 = ORIENTED_EDGE ( 'NONE', *, *, #33416, .F. ) ;
#19290 = AXIS2_PLACEMENT_3D ( 'NONE', #7182, #29519, #44068 ) ;
#19291 = CARTESIAN_POINT ( 'NONE',  ( -0.9500414927467378812, -0.1787899950787401604, 0.3740157479777325711 ) ) ;
#19292 = DIRECTION ( 'NONE',  ( -0.000000000000000000, 1.000000000000000000, -0.000000000000000000 ) ) ;
#19293 = FACE_OUTER_BOUND ( 'NONE', #11663, .T. ) ;
#19294 = CARTESIAN_POINT ( 'NONE',  ( -1.094772975963752103E-17, -1.010458613898529645, -0.1787899950787401882 ) ) ;
#19295 = VERTEX_POINT ( 'NONE', #41038 ) ;
#19296 = CARTESIAN_POINT ( 'NONE',  ( 0.07405724077823318263, 0.06594488194352733645, -0.1787899950787401604 ) ) ;
#19297 = EDGE_LOOP ( 'NONE', ( #25180, #33063, #38797 ) ) ;
#19298 = ORIENTED_EDGE ( 'NONE', *, *, #899, .F. ) ;
#19299 = AXIS2_PLACEMENT_3D ( 'NONE', #10357, #31928, #46517 ) ;
#19300 = AXIS2_PLACEMENT_3D ( 'NONE', #1862, #42350, #9545 ) ;
#19301 = CARTESIAN_POINT ( 'NONE',  ( -1.033464566929134687, -0.06523048226347956391, 0.2731299211523157133 ) ) ;
#19302 = DIRECTION ( 'NONE',  ( 1.000000000000000000, 0.000000000000000000, 0.000000000000000000 ) ) ;
#19303 = DIRECTION ( 'NONE',  ( 1.822029033848725028E-16, 0.000000000000000000, 1.000000000000000000 ) ) ;
#19304 = CARTESIAN_POINT ( 'NONE',  ( 0.07405724077823318263, -0.5049212597887556830, 0.1787899950787401604 ) ) ;
#19305 = EDGE_CURVE ( 'NONE', #22696, #25448, #636, .T. ) ;
#19306 = ADVANCED_FACE ( 'NONE', ( #22859 ), #18783, .F. ) ;
#19307 = CARTESIAN_POINT ( 'NONE',  ( -0.7495606340400177148, -0.1264236179284866091, 0.1697834645131657827 ) ) ;
#19308 = CARTESIAN_POINT ( 'NONE',  ( -0.9873396505805591694, -0.1113553986120547346, 0.8710629921259842590 ) ) ;
#19309 = DIRECTION ( 'NONE',  ( -1.000000000000000000, 0.000000000000000000, 0.000000000000000000 ) ) ;
#19310 = CARTESIAN_POINT ( 'NONE',  ( -1.100456976456230270E-17, -0.9951225497405256082, -0.1797182628040039365 ) ) ;
#19311 = CARTESIAN_POINT ( 'NONE',  ( -0.8759842519685039353, 0.1574803149606299191, 1.938976377845228249 ) ) ;
#19312 = CARTESIAN_POINT ( 'NONE',  ( -0.8107537697050253289, -0.1574803149606297803, 1.562499999892472458 ) ) ;
#19313 = CARTESIAN_POINT ( 'NONE',  ( 0.8019270111902717657, 0.1787899950787401604, 0.8661417322297003674 ) ) ;
#19314 = ADVANCED_FACE ( 'NONE', ( #11145 ), #44876, .T. ) ;
#19315 = EDGE_CURVE ( 'NONE', #38268, #8361, #15371, .T. ) ;
#19316 = CARTESIAN_POINT ( 'NONE',  ( -0.8759842519685039353, 0.1574803149606299191, 0.4527559055118110520 ) ) ;
#19317 = CARTESIAN_POINT ( 'NONE',  ( 0.9873396505805591694, 0.1113553986120547346, 1.628937007874015963 ) ) ;
#19319 = CARTESIAN_POINT ( 'NONE',  ( 2.892866454678787531E-17, -0.05708661417322834220, 0.1574803149606299191 ) ) ;
#19318 = CARTESIAN_POINT ( 'NONE',  ( 0.7145608061145479750, -0.04467186410878862257, 1.984103321452833191 ) ) ;
#19320 = DIRECTION ( 'NONE',  ( 0.000000000000000000, 0.6156614753256602901, 0.7880107536067203489 ) ) ;
#19321 = CARTESIAN_POINT ( 'NONE',  ( 0.1574803149606300301, -0.6648622046168815025, -0.06523048226347956391 ) ) ;
#19322 = CIRCLE ( 'NONE', #46101, 0.009842519685039371677 ) ;
#19323 = CARTESIAN_POINT ( 'NONE',  ( 0.2559055118110236116, -0.1477471161312049197, -0.2921040715117803055 ) ) ;
#19325 = DIRECTION ( 'NONE',  ( 0.000000000000000000, -1.000000000000000000, 0.000000000000000000 ) ) ;
#19324 = CARTESIAN_POINT ( 'NONE',  ( 0.8759842519685039353, -0.1787899950787401882, 0.8784448818360000022 ) ) ;
#19326 = CARTESIAN_POINT ( 'NONE',  ( 0.8759842519685039353, -0.1787899950787401882, 1.828248031442299082 ) ) ;
#19327 = CARTESIAN_POINT ( 'NONE',  ( -1.094772975963752103E-17, -0.7977362204186770889, -0.1787899950787401882 ) ) ;
#19328 = EDGE_LOOP ( 'NONE', ( #38150, #37351, #12819, #30746 ) ) ;
#19329 = AXIS2_PLACEMENT_3D ( 'NONE', #45235, #44123, #36947 ) ;
#19330 = CARTESIAN_POINT ( 'NONE',  ( 2.892866454678787531E-17, -1.464566929026330788, 0.1574803149606299191 ) ) ;
#19331 = CARTESIAN_POINT ( 'NONE',  ( -0.7185039370078746268, 0.06523048226347956391, 0.05659448808144944970 ) ) ;
#19332 = CARTESIAN_POINT ( 'NONE',  ( 1.054774247047244096, 0.000000000000000000, 1.163877952702141672 ) ) ;
#19333 = CARTESIAN_POINT ( 'NONE',  ( 0.1864803149606299171, 1.086379535891623949, -0.03715491745706168969 ) ) ;
#19334 = CARTESIAN_POINT ( 'NONE',  ( 0.06523048226347956391, -1.668799212598424342, 0.1574803149606297803 ) ) ;
#19335 = LINE ( 'NONE', #7840, #3066 ) ;
#19336 = FACE_OUTER_BOUND ( 'NONE', #13795, .T. ) ;
#19337 = CARTESIAN_POINT ( 'NONE',  ( -1.054774247047244540, -0.07405724077823318263, 0.2952755904974176393 ) ) ;
#19338 = VECTOR ( 'NONE', #26290, 39.37007874015748143 ) ;
#19339 = DIRECTION ( 'NONE',  ( 0.000000000000000000, 1.000000000000000000, 0.000000000000000000 ) ) ;
#19340 = CARTESIAN_POINT ( 'NONE',  ( -0.07405724077823318263, -1.469488188922614791, -0.1787899950787401604 ) ) ;
#19341 = CARTESIAN_POINT ( 'NONE',  ( -0.8759842519685039353, 0.1787899950787401882, 1.803641732229700700 ) ) ;
#19342 = CARTESIAN_POINT ( 'NONE',  ( -1.002407869896990045, -0.1264236179284866091, 0.9227362204186770889 ) ) ;
#19343 = CARTESIAN_POINT ( 'NONE',  ( -1.054774247047244096, 0.000000000000000000, 0.5388779527021417826 ) ) ;
#19344 = FACE_OUTER_BOUND ( 'NONE', #41945, .T. ) ;
#19345 = CARTESIAN_POINT ( 'NONE',  ( 0.1476377952755906220, -0.4889725119976396916, -0.8550419489141691809 ) ) ;
#19346 = CARTESIAN_POINT ( 'NONE',  ( 0.1787899950787401604, -0.5060294800402627136, -0.07405724077823318263 ) ) ;
#19347 = CARTESIAN_POINT ( 'NONE',  ( -0.1687763848766232477, -0.08955970710929901657, 0.1556180494977049134 ) ) ;
#19348 = CARTESIAN_POINT ( 'NONE',  ( 2.892866454678787531E-17, 0.03149606309965303358, 0.1574803149606299191 ) ) ;
#19349 = CARTESIAN_POINT ( 'NONE',  ( -0.7185039370078739607, 0.000000000000000000, -2.869337061179095023E-17 ) ) ;
#19350 = CARTESIAN_POINT ( 'NONE',  ( -1.054774247047244096, 0.000000000000000000, 0.4945866141194645849 ) ) ;
#19351 = CARTESIAN_POINT ( 'NONE',  ( 0.1264236179284866091, -1.812623968229240212, 0.1264236179284866091 ) ) ;
#19352 = B_SPLINE_CURVE_WITH_KNOTS ( 'NONE', 3,
 ( #29218, #43766, #18598, #18138, #32782, #22432, #33017, #21738, #43522, #22677, #37278, #33490, #36370, #11202, #36829, #7816, #17899 ),
 .UNSPECIFIED., .F., .F.,
 ( 4, 2, 2, 2, 2, 1, 2, 2, 4 ),
 ( 0.000000000000000000, 0.1249999999999995004, 0.1874999999999994171, 0.2499999999999993339, 0.3749999999999992784, 0.4374999999999990563, 0.4687499999999990563, 0.4999999999999990008, 1.000000000000000000 ),
 .UNSPECIFIED. ) ;
#19353 = ORIENTED_EDGE ( 'NONE', *, *, #34189, .T. ) ;
#19354 = CARTESIAN_POINT ( 'NONE',  ( 0.2471922899045338740, -0.07845124750586851547, 0.07638293795143560883 ) ) ;
#19355 = CARTESIAN_POINT ( 'NONE',  ( -1.054774247047244096, 0.000000000000000000, 1.562499999946236118 ) ) ;
#19356 = AXIS2_PLACEMENT_3D ( 'NONE', #19479, #37461, #1259 ) ;
#19357 = CARTESIAN_POINT ( 'NONE',  ( 0.07405724077823318263, -1.292322834591905778, 0.1787899950787401604 ) ) ;
#19358 = CARTESIAN_POINT ( 'NONE',  ( 0.07405724077823318263, -1.562992125930488196, 0.1787899950787401604 ) ) ;
#19360 = EDGE_CURVE ( 'NONE', #955, #43835, #29633, .T. ) ;
#19359 = CONICAL_SURFACE ( 'NONE', #46149, 0.1003937007874010356, 0.7853981633978559529 ) ;
#19361 = LINE ( 'NONE', #12438, #35590 ) ;
#19362 = FACE_OUTER_BOUND ( 'NONE', #20989, .T. ) ;
#19363 = CARTESIAN_POINT ( 'NONE',  ( -0.7185039370078739607, 1.928577636452523993E-17, 1.801181102362204633 ) ) ;
#19364 = CARTESIAN_POINT ( 'NONE',  ( -1.033464566929134687, 0.06523048226347956391, 1.026082677057828185 ) ) ;
#19365 = CARTESIAN_POINT ( 'NONE',  ( 0.8019270111902717657, 0.1787899950787401604, 0.5511811023084406402 ) ) ;
#19366 = CARTESIAN_POINT ( 'NONE',  ( 0.8019270111902716547, -0.1787899950787401604, 0.08858267711159095725 ) ) ;
#19368 = CARTESIAN_POINT ( 'NONE',  ( 1.033464566929134687, -0.06523048226347956391, 0.3617125984251969295 ) ) ;
#19367 = CARTESIAN_POINT ( 'NONE',  ( -0.06523048226347956391, -0.3351377952755906775, 0.1574803149606297803 ) ) ;
#19369 = ORIENTED_EDGE ( 'NONE', *, *, #39706, .T. ) ;
#19370 = CARTESIAN_POINT ( 'NONE',  ( 0.8759842519685039353, 0.1574803149606299191, 1.978346456585385882 ) ) ;
#19371 = ORIENTED_EDGE ( 'NONE', *, *, #9854, .F. ) ;
#19372 = ADVANCED_FACE ( 'NONE', ( #31484 ), #29915, .F. ) ;
#19373 = DIRECTION ( 'NONE',  ( 1.000000000000000000, 0.000000000000000000, 0.000000000000000000 ) ) ;
#19374 = CARTESIAN_POINT ( 'NONE',  ( -1.002407869896990045, 0.1264236179284866091, 1.094980314906866203 ) ) ;
#19375 = CARTESIAN_POINT ( 'NONE',  ( 0.9873396505805591694, -0.1113553986120547346, 0.9498031496062993018 ) ) ;
#19376 = CARTESIAN_POINT ( 'NONE',  ( -1.033464566929133799, 1.928577636452524610E-17, 2.869337061179095023E-17 ) ) ;
#19377 = CARTESIAN_POINT ( 'NONE',  ( -0.1686160743781814630, -0.08918665060197839001, 0.1880811715468738432 ) ) ;
#19379 = CARTESIAN_POINT ( 'NONE',  ( 0.3161444924769519216, 1.495705267341507883, -0.3569552279982051712 ) ) ;
#19378 = CARTESIAN_POINT ( 'NONE',  ( 0.000000000000000000, 0.000000000000000000, -0.01478361295688420882 ) ) ;
#19380 = CARTESIAN_POINT ( 'NONE',  ( -0.1062059389003459364, -0.08956135442286349002, 0.1200209881557332131 ) ) ;
#19381 = ORIENTED_EDGE ( 'NONE', *, *, #37423, .T. ) ;
#19382 = LINE ( 'NONE', #12213, #42091 ) ;
#19383 = CARTESIAN_POINT ( 'NONE',  ( 0.8019270111902717657, -0.1787899950787401604, 0.6791338582139527791 ) ) ;
#19384 = CARTESIAN_POINT ( 'NONE',  ( -1.033464566929134687, -0.06523048226347956391, 1.109744094488189115 ) ) ;
#19385 = ORIENTED_EDGE ( 'NONE', *, *, #7044, .F. ) ;
#19386 = CARTESIAN_POINT ( 'NONE',  ( -1.033464566929133799, 1.928577636452524610E-17, 2.869337061179095023E-17 ) ) ;
#19387 = DIRECTION ( 'NONE',  ( -1.000000000000000000, 0.000000000000000000, 0.000000000000000000 ) ) ;
#19388 = CARTESIAN_POINT ( 'NONE',  ( 0.07405724077823318263, -1.705708661363559253, -0.1787899950787401604 ) ) ;
#19390 = CARTESIAN_POINT ( 'NONE',  ( 0.1264236179284866091, -0.8863188975840314843, -0.1264236179284866091 ) ) ;
#19389 = CARTESIAN_POINT ( 'NONE',  ( 0.06523048226347956391, -1.014271653435780296, -0.1574803149606300301 ) ) ;
#19391 = CARTESIAN_POINT ( 'NONE',  ( -0.1113553986120547346, -1.243110236220472453, 0.1113553986120547346 ) ) ;
#19392 = CARTESIAN_POINT ( 'NONE',  ( 0.8759842519685039353, -0.1574803149606299191, 1.053149606191685184 ) ) ;
#19393 = CARTESIAN_POINT ( 'NONE',  ( -0.6195511811023656223, 0.6102362204724408601, 0.5854071585544579071 ) ) ;
#19394 = ORIENTED_EDGE ( 'NONE', *, *, #1012, .T. ) ;
#19395 = ORIENTED_EDGE ( 'NONE', *, *, #7535, .F. ) ;
#19396 = CARTESIAN_POINT ( 'NONE',  ( -0.8019270111902717657, -0.1787899950787401604, 1.786417322780882388 ) ) ;
#19397 = CARTESIAN_POINT ( 'NONE',  ( 1.054774247047244096, 0.000000000000000000, 1.719980314906866203 ) ) ;
#19398 = ORIENTED_EDGE ( 'NONE', *, *, #32638, .F. ) ;
#19400 = CARTESIAN_POINT ( 'NONE',  ( -2.680625843783058887E-15, -0.2954942322624074524, -0.2921040715117803055 ) ) ;
#19399 = CIRCLE ( 'NONE', #18639, 0.09842519685039310962 ) ;
#19401 = CARTESIAN_POINT ( 'NONE',  ( 1.054774247047244540, -0.07405724077823318263, 0.3789370078202520253 ) ) ;
#19402 = CARTESIAN_POINT ( 'NONE',  ( -1.054774247047244096, 0.000000000000000000, 1.439468503883244210 ) ) ;
#19403 = CARTESIAN_POINT ( 'NONE',  ( -0.7185039370078739607, 0.000000000000000000, -2.869337061179095023E-17 ) ) ;
#19404 = CARTESIAN_POINT ( 'NONE',  ( -1.054774247047244540, 0.07405724077823318263, 1.205708661363558365 ) ) ;
#19405 = CARTESIAN_POINT ( 'NONE',  ( 0.08994717584591196968, 0.09317026862873967197, 0.2335020446786578718 ) ) ;
#19406 = CARTESIAN_POINT ( 'NONE',  ( -0.7495606340400177148, 0.1264236179284866091, 1.695374015694267822 ) ) ;
#19407 = CARTESIAN_POINT ( 'NONE',  ( -0.6971942568897626646, -0.07405724077823297447, 0.1279527558517483676 ) ) ;
#19408 = DIRECTION ( 'NONE',  ( -1.000000000000000000, 0.000000000000000000, 6.938893903907228378E-15 ) ) ;
#19409 = CARTESIAN_POINT ( 'NONE',  ( -0.8759842519685039353, 0.1574803149606299191, 1.633858267716535639 ) ) ;
#19410 = DIRECTION ( 'NONE',  ( 0.000000000000000000, -1.000000000000000000, 0.000000000000000000 ) ) ;
#19411 = CARTESIAN_POINT ( 'NONE',  ( 0.8759842519685039353, 0.1787899950787401882, 1.611712598371433103 ) ) ;
#19412 = CARTESIAN_POINT ( 'NONE',  ( -0.09071607244976082063, -0.09842519685039370636, -0.2375934515383263668 ) ) ;
#19413 = CARTESIAN_POINT ( 'NONE',  ( 0.8107537697050254399, -0.1574803149606297803, 1.011318897530268712 ) ) ;
#19414 = CARTESIAN_POINT ( 'NONE',  ( -0.8107537697050254399, 0.1574803149606300301, 1.793799212598424342 ) ) ;
#19415 = EDGE_LOOP ( 'NONE', ( #11743, #13760, #13306, #30340 ) ) ;
#19416 = EDGE_LOOP ( 'NONE', ( #40077, #36375, #25803, #32862 ) ) ;
#19417 = ORIENTED_EDGE ( 'NONE', *, *, #20654, .T. ) ;
#19418 = VECTOR ( 'NONE', #11493, 39.37007874015748143 ) ;
#19419 = CARTESIAN_POINT ( 'NONE',  ( -0.1787899950787401604, -0.8346456692375755493, -0.07405724077823318263 ) ) ;
#19420 = CARTESIAN_POINT ( 'NONE',  ( -0.1264236179284866091, -1.097933070812378009, 0.1264236179284866091 ) ) ;
#19421 = ADVANCED_FACE ( 'NONE', ( #34365 ), #41325, .F. ) ;
#19422 = CARTESIAN_POINT ( 'NONE',  ( -0.8759842519685039353, 0.1574803149606299191, 1.279527559055118280 ) ) ;
#19423 = ( CONVERSION_BASED_UNIT ( 'INCH', #40733 ) LENGTH_UNIT ( ) NAMED_UNIT ( #46381 ) ) ;
#19424 = CARTESIAN_POINT ( 'NONE',  ( -1.100456976456230270E-17, -0.3652012898980063205, -0.1797182628040039365 ) ) ;
#19425 = DIRECTION ( 'NONE',  ( 0.000000000000000000, 2.602085213965210247E-15, -1.000000000000000000 ) ) ;
#19426 = DIRECTION ( 'NONE',  ( 1.000000000000000000, 0.000000000000000000, -0.000000000000000000 ) ) ;
#19427 = ADVANCED_FACE ( 'NONE', ( #41268 ), #45357, .T. ) ;
#19428 = CARTESIAN_POINT ( 'NONE',  ( -0.9873396505805591694, 0.1113553986120547346, 0.1328740157480315098 ) ) ;
#19429 = CARTESIAN_POINT ( 'NONE',  ( 0.7495606340400177148, -0.1264236179284866091, 0.7947834645131652831 ) ) ;
#19430 = FACE_OUTER_BOUND ( 'NONE', #43663, .T. ) ;
#19431 = AXIS2_PLACEMENT_3D ( 'NONE', #36418, #7630, #7403 ) ;
#19432 = DIRECTION ( 'NONE',  ( -8.673617379884043361E-16, 0.000000000000000000, -1.000000000000000000 ) ) ;
#19433 = CARTESIAN_POINT ( 'NONE',  ( 1.002407869896990045, 0.1264236179284866091, 1.882381889710015743 ) ) ;
#19434 = ORIENTED_EDGE ( 'NONE', *, *, #13985, .T. ) ;
#19435 = CARTESIAN_POINT ( 'NONE',  ( 0.9412147342319837628, -0.1574803149606297803, 0.1599409448818898405 ) ) ;
#19436 = DIRECTION ( 'NONE',  ( 5.159318851433039196E-16, 0.6156614753256609562, 0.7880107536067197938 ) ) ;
#19437 = CARTESIAN_POINT ( 'NONE',  ( 0.1264236179284866091, -0.4237204723871811352, 0.1264236179284866091 ) ) ;
#19438 = DIRECTION ( 'NONE',  ( 0.000000000000000000, 0.5000000000000003331, -0.8660254037844384856 ) ) ;
#19439 = CARTESIAN_POINT ( 'NONE',  ( -1.094772975963752103E-17, -1.191437007820251859, -0.1787899950787401882 ) ) ;
#19440 = CARTESIAN_POINT ( 'NONE',  ( 0.6971942568897637749, 2.189545951927499583E-17, 0.2829724408911185041 ) ) ;
#19441 = CARTESIAN_POINT ( 'NONE',  ( -0.8759842519685039353, 0.1787899950787401882, 1.685531496009228469 ) ) ;
#19442 = ORIENTED_EDGE ( 'NONE', *, *, #23008, .F. ) ;
#19443 = CARTESIAN_POINT ( 'NONE',  ( -1.002407869896990045, -0.1264236179284866091, 1.281988188922614125 ) ) ;
#19444 = CARTESIAN_POINT ( 'NONE',  ( 0.2698848154395015464, -0.09842519685039370636, 0.000000000000000000 ) ) ;
#19445 = CARTESIAN_POINT ( 'NONE',  ( 1.054774247047244540, 0.07405724077823318263, 1.289370078686393750 ) ) ;
#19446 = CARTESIAN_POINT ( 'NONE',  ( -0.8759842519685039353, 0.1787899950787401882, 1.213090551127338435 ) ) ;
#19447 = CYLINDRICAL_SURFACE ( 'NONE', #3860, 0.1574803149606299191 ) ;
#19448 = CARTESIAN_POINT ( 'NONE',  ( 0.03096532509380343218, -0.09840740886148355293, -0.1761182458273901907 ) ) ;
#19449 = CARTESIAN_POINT ( 'NONE',  ( -0.005244590715618953347, 0.5419983459879460508, -0.7609487005970287932 ) ) ;
#19450 = CARTESIAN_POINT ( 'NONE',  ( 0.8759842519685039353, 0.1787899950787401882, 0.3912401574265515491 ) ) ;
#19451 = CARTESIAN_POINT ( 'NONE',  ( -0.7495606340400177148, 0.1264236179284866091, 0.3518700786863940833 ) ) ;
#19452 = ORIENTED_EDGE ( 'NONE', *, *, #34771, .F. ) ;
#19453 = EDGE_CURVE ( 'NONE', #40844, #10631, #34695, .T. ) ;
#19454 = CARTESIAN_POINT ( 'NONE',  ( -0.8759842519685039353, 0.000000000000000000, 0.000000000000000000 ) ) ;
#19455 = EDGE_LOOP ( 'NONE', ( #10206, #43679, #30583, #23957 ) ) ;
#19456 = CARTESIAN_POINT ( 'NONE',  ( -0.8107537697050234415, -0.1574803149606297803, 0.2337598425196852070 ) ) ;
#19457 = CARTESIAN_POINT ( 'NONE',  ( 0.8759842519685039353, 0.1787899950787401882, 1.218011810969858111 ) ) ;
#19458 = CARTESIAN_POINT ( 'NONE',  ( 0.9873396505805591694, 0.1113553986120547346, 1.934055118002708573 ) ) ;
#19459 = CARTESIAN_POINT ( 'NONE',  ( 0.3649999999999999911, 0.2362204724409449064, 2.892866454678787531E-17 ) ) ;
#19460 = CIRCLE ( 'NONE', #5717, 0.009842519685039399432 ) ;
#19461 = AXIS2_PLACEMENT_3D ( 'NONE', #43226, #16674, #20719 ) ;
#19462 = EDGE_LOOP ( 'NONE', ( #17764, #44282, #22899, #44203, #27991 ) ) ;
#19463 = CARTESIAN_POINT ( 'NONE',  ( -0.6971942568897637749, 2.189545951927499583E-17, 0.8735236219934803259 ) ) ;
#19464 = CARTESIAN_POINT ( 'NONE',  ( 0.1608764814808673338, -0.07794373349925551309, -0.1405880446287836594 ) ) ;
#19465 = CARTESIAN_POINT ( 'NONE',  ( -0.7495606340400177148, 0.1264236179284866091, 0.03690944876513417572 ) ) ;
#19466 = CARTESIAN_POINT ( 'NONE',  ( -0.07405724077823318263, -1.426305070591442625, 0.1787899950787401604 ) ) ;
#19467 = AXIS2_PLACEMENT_3D ( 'NONE', #24073, #5849, #23363 ) ;
#19468 = ORIENTED_EDGE ( 'NONE', *, *, #42296, .F. ) ;
#19469 = DIRECTION ( 'NONE',  ( -6.944548107256197364E-15, -0.7880107536067206819, 0.6156614753256598460 ) ) ;
#19470 = CARTESIAN_POINT ( 'NONE',  ( 0.07405724077823318263, -0.4606299212060784853, 0.1787899950787401604 ) ) ;
#19471 = CARTESIAN_POINT ( 'NONE',  ( 1.033464566929133799, 0.000000000000000000, 1.309055118110236338 ) ) ;
#19472 = EDGE_LOOP ( 'NONE', ( #45614, #32323, #19803, #37094 ) ) ;
#19473 = CARTESIAN_POINT ( 'NONE',  ( 0.000000000000000000, 0.1473293504822035527, -0.5595480905233944924 ) ) ;
#19474 = CYLINDRICAL_SURFACE ( 'NONE', #35356, 0.1574803149606299191 ) ;
#19475 = ADVANCED_FACE ( 'NONE', ( #26713 ), #27440, .F. ) ;
#19476 = CARTESIAN_POINT ( 'NONE',  ( 0.000000000000000000, 0.000000000000000000, 0.09842519685039370636 ) ) ;
#19477 = CARTESIAN_POINT ( 'NONE',  ( 0.8019270111902717657, -0.1787899950787401604, 1.584645669237574994 ) ) ;
#19478 = CARTESIAN_POINT ( 'NONE',  ( -1.094772975963752103E-17, -1.786909448765134023, -0.1787899950787401882 ) ) ;
#19479 = CARTESIAN_POINT ( 'NONE',  ( -0.8070866141732283561, 0.3779527559055118058, -0.7574803149606299524 ) ) ;
#19480 = CARTESIAN_POINT ( 'NONE',  ( 0.1773397566031712225, -0.09842519685039370636, 0.01193638218527439190 ) ) ;
#19481 = ORIENTED_EDGE ( 'NONE', *, *, #34878, .T. ) ;
#19482 = EDGE_CURVE ( 'NONE', #20308, #40149, #37717, .T. ) ;
#19483 = ADVANCED_FACE ( 'NONE', ( #15924 ), #37956, .F. ) ;
#19484 = CARTESIAN_POINT ( 'NONE',  ( -0.8019270111902716547, 0.1787899950787401604, 0.7086614172690703928 ) ) ;
#19485 = CARTESIAN_POINT ( 'NONE',  ( -0.7185039370078766252, -0.06523048226348168721, 1.281988188868851353 ) ) ;
#19487 = CARTESIAN_POINT ( 'NONE',  ( -1.033464566929133799, 0.000000000000000000, 1.614173228238929170 ) ) ;
#19486 = CARTESIAN_POINT ( 'NONE',  ( -0.06523048226347956391, -0.7436023622047251980, -0.1574803149606300301 ) ) ;
#19488 = CARTESIAN_POINT ( 'NONE',  ( 0.1797182628040039365, -1.556146171787769594, -2.200913952912460540E-17 ) ) ;
#19489 = CYLINDRICAL_SURFACE ( 'NONE', #16440, 0.1574803149606299191 ) ;
#19490 = CARTESIAN_POINT ( 'NONE',  ( 0.06523048226347956391, -0.4630905510735751074, -0.1574803149606300301 ) ) ;
#19491 = AXIS2_PLACEMENT_3D ( 'NONE', #29389, #18536, #37453 ) ;
#19492 = DIRECTION ( 'NONE',  ( 0.000000000000000000, 0.000000000000000000, 1.000000000000000000 ) ) ;
#19493 = CARTESIAN_POINT ( 'NONE',  ( 1.002407869896990045, -0.1264236179284866091, 1.400098425143086800 ) ) ;
#19494 = CARTESIAN_POINT ( 'NONE',  ( 0.8759842519685039353, -0.1787899950787401882, 1.823326771599779406 ) ) ;
#19495 = VECTOR ( 'NONE', #15796, 39.37007874015748143 ) ;
#19496 = ORIENTED_EDGE ( 'NONE', *, *, #17197, .F. ) ;
#19498 = ORIENTED_EDGE ( 'NONE', *, *, #45633, .T. ) ;
#19497 = CARTESIAN_POINT ( 'NONE',  ( -1.033464566929133799, 1.928577636452524610E-17, 2.869337061179095023E-17 ) ) ;
#19499 = CARTESIAN_POINT ( 'NONE',  ( -0.7646288533564489232, -0.1113553986120547346, 1.441929133750740277 ) ) ;
#19500 = CARTESIAN_POINT ( 'NONE',  ( -0.1574803149606299191, 1.928577636452524610E-17, 2.731847993664263218E-16 ) ) ;
#19501 = CARTESIAN_POINT ( 'NONE',  ( -1.094772975963752103E-17, 0.02411417328210995956, -0.1787899950787401882 ) ) ;
#19502 = CARTESIAN_POINT ( 'NONE',  ( 0.8019270111902717657, -0.1787899950787401604, 0.3248031495525355306 ) ) ;
#19503 = CARTESIAN_POINT ( 'NONE',  ( -0.9412147342319837628, -0.1574803149606297803, 0.7504921259842517456 ) ) ;
#19504 = CARTESIAN_POINT ( 'NONE',  ( -0.6195511811023656223, 0.4133858267716533086, 1.186023622047243986 ) ) ;
#19505 = DIRECTION ( 'NONE',  ( 0.000000000000000000, 5.311252123978373147E-15, 1.000000000000000000 ) ) ;
#19506 = CARTESIAN_POINT ( 'NONE',  ( 0.8759842519685039353, 0.1574803149606299191, 0.8759842518609765039 ) ) ;
#19507 = EDGE_LOOP ( 'NONE', ( #8976, #38554, #42533, #28626, #9695, #15318 ) ) ;
#19508 = CARTESIAN_POINT ( 'NONE',  ( 1.033464566929134687, 0.06523048226347956391, 0.6815944881889761664 ) ) ;
#19509 = ORIENTED_EDGE ( 'NONE', *, *, #16324, .T. ) ;
#19510 = CARTESIAN_POINT ( 'NONE',  ( -0.07444174185955065859, -0.03301625052792742793, 0.1797182628040039087 ) ) ;
#19512 = VERTEX_POINT ( 'NONE', #31251 ) ;
#19511 = CARTESIAN_POINT ( 'NONE',  ( -1.094772975963752103E-17, -1.156988188922614125, -0.1787899950787401882 ) ) ;
#19513 = CARTESIAN_POINT ( 'NONE',  ( 0.8019270111902717657, 0.1787899950787401604, 1.609251968450173376 ) ) ;
#19514 = CARTESIAN_POINT ( 'NONE',  ( -0.7185039370078746268, 0.06523048226347956391, 1.247539370078740273 ) ) ;
#19515 = CARTESIAN_POINT ( 'NONE',  ( 0.9412147342319837628, 0.1574803149606300301, 0.2436023620971973780 ) ) ;
#19517 = CARTESIAN_POINT ( 'NONE',  ( -0.7185039370078746268, -0.06523048226347956391, 0.4256889763779528879 ) ) ;
#19516 = CARTESIAN_POINT ( 'NONE',  ( -0.1377952755905510751, 1.687505431895957647E-17, -0.3149606299212598381 ) ) ;
#19518 = CARTESIAN_POINT ( 'NONE',  ( 0.9873396505805591694, 0.1113553986120547346, 0.3592519683964098820 ) ) ;
#19519 = ORIENTED_EDGE ( 'NONE', *, *, #44927, .F. ) ;
#19520 = ORIENTED_EDGE ( 'NONE', *, *, #14798, .F. ) ;
#19521 = CARTESIAN_POINT ( 'NONE',  ( -0.1178667752584066641, -0.09842519685039365085, -0.2173826564421876550 ) ) ;
#19522 = ORIENTED_EDGE ( 'NONE', *, *, #4131, .F. ) ;
#19523 = CARTESIAN_POINT ( 'NONE',  ( -1.054774247047244540, 0.07405724077823318263, 1.560039370024976835 ) ) ;
#19524 = CARTESIAN_POINT ( 'NONE',  ( 0.1574803149606299191, -0.07677165343578011558, -1.928577636452523993E-17 ) ) ;
#19525 = CARTESIAN_POINT ( 'NONE',  ( -1.054774247047244540, 0.07405724077823318263, 1.249999999946235896 ) ) ;
#19526 = EDGE_LOOP ( 'NONE', ( #34644, #9810, #46323, #16868 ) ) ;
#19527 = PLANE ( 'NONE',  #42868 ) ;
#19528 = CARTESIAN_POINT ( 'NONE',  ( -1.054774247047244540, -0.07405724077823318263, 0.3395669290800945039 ) ) ;
#19529 = LINE ( 'NONE', #34399, #35631 ) ;
#19530 = CIRCLE ( 'NONE', #18769, 0.009842519685039378616 ) ;
#19531 = DIRECTION ( 'NONE',  ( 0.000000000000000000, 0.000000000000000000, 1.000000000000000000 ) ) ;
#19532 = CARTESIAN_POINT ( 'NONE',  ( -0.1787899950787401604, -0.9194153068119157446, 0.07405724077823318263 ) ) ;
#19533 = VERTEX_POINT ( 'NONE', #38181 ) ;
#19534 = CARTESIAN_POINT ( 'NONE',  ( 0.1787899950787401604, 0.06102362210100767403, -0.07405724077823318263 ) ) ;
#19535 = VERTEX_POINT ( 'NONE', #16159 ) ;
#19536 = EDGE_CURVE ( 'NONE', #20455, #1520, #9438, .T. ) ;
#19537 = AXIS2_PLACEMENT_3D ( 'NONE', #46175, #3025, #35416 ) ;
#19538 = VERTEX_POINT ( 'NONE', #34142 ) ;
#19539 = CARTESIAN_POINT ( 'NONE',  ( 0.000000000000000000, 1.478656101119254046E-17, 0.1377952755905511861 ) ) ;
#19540 = CARTESIAN_POINT ( 'NONE',  ( 0.8759842519685039353, -0.1574803149606299191, 0.1082677164279060994 ) ) ;
#19541 = ( BOUNDED_CURVE ( )  B_SPLINE_CURVE ( 2, ( #13721, #35072, #17078, #24512, #28358, #39109, #10137, #13960, #6521 ),
 .UNSPECIFIED., .F., .T. ) 
 B_SPLINE_CURVE_WITH_KNOTS ( ( 3, 2, 2, 2, 3 ),
 ( 0.9100000000000000311, 0.9124999999999999778, 0.9150000000000000355, 0.9174999999999999822, 0.9200000000000000400 ),
 .UNSPECIFIED. ) 
 CURVE ( )  GEOMETRIC_REPRESENTATION_ITEM ( )  RATIONAL_B_SPLINE_CURVE ( ( 1.000000000000000000, 0.9238795325112869605, 1.000000000000000000, 0.9238795325112869605, 1.000000000000000000, 0.9238795325112869605, 1.000000000000000000, 0.9238795325112869605, 1.000000000000000000 ) ) 
 REPRESENTATION_ITEM ( '' )  ) ;
#19542 = DIRECTION ( 'NONE',  ( 1.822029033848725028E-16, 0.000000000000000000, 1.000000000000000000 ) ) ;
#19543 = CARTESIAN_POINT ( 'NONE',  ( -0.07405724077823318263, -0.6279527558517482566, 0.1787899950787401604 ) ) ;
#19544 = EDGE_CURVE ( 'NONE', #11565, #13693, #9188, .T. ) ;
#19545 = CARTESIAN_POINT ( 'NONE',  ( -0.8759842519685039353, -0.1787899950787401882, 0.2534448818360003908 ) ) ;
#19546 = CARTESIAN_POINT ( 'NONE',  ( -1.033464566929134687, 0.06523048226347956391, 0.8784448818897642175 ) ) ;
#19547 = CARTESIAN_POINT ( 'NONE',  ( -1.181102362204724310, -0.3937007874015748254, 0.9842519685039370358 ) ) ;
#19548 = CARTESIAN_POINT ( 'NONE',  ( -0.1797182628040039087, -1.027110738716904725, -0.07444174185955065859 ) ) ;
#19549 = DIRECTION ( 'NONE',  ( 0.000000000000000000, 0.000000000000000000, -1.000000000000000000 ) ) ;
#19550 = CARTESIAN_POINT ( 'NONE',  ( 0.9500414927467378812, -0.1787899950787401604, 0.8464566928596233275 ) ) ;
#19551 = AXIS2_PLACEMENT_3D ( 'NONE', #24130, #35384, #2529 ) ;
#19552 = DIRECTION ( 'NONE',  ( 0.000000000000000000, 0.000000000000000000, 1.000000000000000000 ) ) ;
#19553 = CARTESIAN_POINT ( 'NONE',  ( 0.8107537697050253289, -0.1574803149606297803, 1.572342519685040685 ) ) ;
#19555 = CARTESIAN_POINT ( 'NONE',  ( -0.1469224761500225462, -0.2106668292959394673, -0.3144321013757213623 ) ) ;
#19554 = CARTESIAN_POINT ( 'NONE',  ( 0.7500335542904545960, 0.1023885596843875229, 1.981118523551024468 ) ) ;
#19556 = CARTESIAN_POINT ( 'NONE',  ( 1.033464566929134687, -0.06523048226347956391, 0.4699803148531029873 ) ) ;
#19557 = CARTESIAN_POINT ( 'NONE',  ( -0.07405724077823318263, 0.1102362205262043815, -0.1787899950787401604 ) ) ;
#19558 = ( BOUNDED_CURVE ( )  B_SPLINE_CURVE ( 2, ( #13587, #2789, #46883, #2556, #46409, #5925, #34949, #6393, #27784 ),
 .UNSPECIFIED., .F., .F. ) 
 B_SPLINE_CURVE_WITH_KNOTS ( ( 3, 2, 2, 2, 3 ),
 ( 0.2399999999999999911, 0.2424999999999999933, 0.2449999999999999956, 0.2474999999999999978, 0.2500000000000000000 ),
 .UNSPECIFIED. ) 
 CURVE ( )  GEOMETRIC_REPRESENTATION_ITEM ( )  RATIONAL_B_SPLINE_CURVE ( ( 1.000000000000000000, 0.9238795325112869605, 1.000000000000000000, 0.9238795325112869605, 1.000000000000000000, 0.9238795325112869605, 1.000000000000000000, 0.9238795325112869605, 1.000000000000000000 ) ) 
 REPRESENTATION_ITEM ( '' )  ) ;
#19559 = CARTESIAN_POINT ( 'NONE',  ( -0.9873396505805591694, 0.1113553986120547346, 1.550196850393700920 ) ) ;
#19561 = FACE_OUTER_BOUND ( 'NONE', #6317, .T. ) ;
#19560 = CARTESIAN_POINT ( 'NONE',  ( 1.054774247047244096, 0.000000000000000000, 0.9276574802611967652 ) ) ;
#19562 = CARTESIAN_POINT ( 'NONE',  ( 1.002407869896990045, -0.1264236179284866091, 1.872539370024976391 ) ) ;
#19563 = CARTESIAN_POINT ( 'NONE',  ( -0.1787899950787401604, -0.9872047243556864027, -0.07405724077823318263 ) ) ;
#19564 = VERTEX_POINT ( 'NONE', #34850 ) ;
#19565 = CARTESIAN_POINT ( 'NONE',  ( -1.033464566929134687, 0.06523048226347956391, 0.8390748031496062520 ) ) ;
#19566 = AXIS2_PLACEMENT_3D ( 'NONE', #38764, #10247, #43037 ) ;
#19567 = VECTOR ( 'NONE', #40427, 39.37007874015748143 ) ;
#19568 = CYLINDRICAL_SURFACE ( 'NONE', #38195, 0.02900000000000060515 ) ;
#19569 = CARTESIAN_POINT ( 'NONE',  ( 0.1113553986120547346, -1.617125984144440753, 0.1113553986120547346 ) ) ;
#19570 = CARTESIAN_POINT ( 'NONE',  ( -0.8107537697050234415, -0.1574803149606297803, 0.1058070865066461225 ) ) ;
#19571 = CARTESIAN_POINT ( 'NONE',  ( -0.3980944881889762477, 0.1574803149606354702, -0.7480314960629921295 ) ) ;
#19572 = CARTESIAN_POINT ( 'NONE',  ( 1.054774247047244096, 0.000000000000000000, 1.085137795221826629 ) ) ;
#19573 = EDGE_LOOP ( 'NONE', ( #13006, #1606, #22186, #20522, #26556 ) ) ;
#19574 = DIRECTION ( 'NONE',  ( 2.710505431213762009E-17, 0.6156614753256599570, 0.7880107536067207930 ) ) ;
#19575 = CARTESIAN_POINT ( 'NONE',  ( -0.1113553986120547346, -1.764763779527559029, -0.1113553986120547346 ) ) ;
#19576 = CARTESIAN_POINT ( 'NONE',  ( -0.7495606340400177148, 0.1264236179284866091, 0.5093503936470236138 ) ) ;
#19577 = CARTESIAN_POINT ( 'NONE',  ( 1.033464566929133799, 0.000000000000000000, 0.2460629921259842590 ) ) ;
#19578 = CARTESIAN_POINT ( 'NONE',  ( -1.002407869896990045, -0.1264236179284866091, 0.1747047243556852092 ) ) ;
#19579 = ( REPRESENTATION_RELATIONSHIP ('NONE','NONE', #9609, #20643 ) REPRESENTATION_RELATIONSHIP_WITH_TRANSFORMATION ( #17464 )SHAPE_REPRESENTATION_RELATIONSHIP( ) ) ;
#19580 = CARTESIAN_POINT ( 'NONE',  ( 3.284318927891251994E-17, -1.570374015694267600, 0.1787899950787401882 ) ) ;
#19581 = CARTESIAN_POINT ( 'NONE',  ( -0.8759842519685039353, 0.1787899950787401882, 1.843011810969858333 ) ) ;
#19582 = EDGE_CURVE ( 'NONE', #802, #6080, #39054, .T. ) ;
#19583 = CARTESIAN_POINT ( 'NONE',  ( -1.054774247047244540, 0.07405724077823318263, 0.8907480314422985268 ) ) ;
#19584 = CARTESIAN_POINT ( 'NONE',  ( -0.8759842519685039353, 0.1787899950787401882, 0.5093503936470236138 ) ) ;
#19585 = ADVANCED_FACE ( 'NONE', ( #27674 ), #40588, .T. ) ;
#19586 = DIRECTION ( 'NONE',  ( 0.000000000000000000, -0.2126700594527834720, 0.9771240687918549828 ) ) ;
#19587 = CARTESIAN_POINT ( 'NONE',  ( 0.3161444924769130083, 2.559880088878740079, -3.648497683167389649 ) ) ;
#19588 = DIRECTION ( 'NONE',  ( 0.000000000000000000, 0.000000000000000000, -1.000000000000000000 ) ) ;
#19589 = CARTESIAN_POINT ( 'NONE',  ( 0.1264236179284866091, -0.6315216060245139040, 0.1264236179284866091 ) ) ;
#19590 = CARTESIAN_POINT ( 'NONE',  ( -0.03820435495970567197, -0.08955995172511357905, 0.2191518663821425128 ) ) ;
#19591 = CARTESIAN_POINT ( 'NONE',  ( 0.1113553986120547346, 0.03641732294217271682, 0.1113553986120547346 ) ) ;
#19592 = DIRECTION ( 'NONE',  ( 0.000000000000000000, 0.000000000000000000, -1.000000000000000000 ) ) ;
#19593 = EDGE_CURVE ( 'NONE', #11736, #38566, #18412, .T. ) ;
#19594 = CIRCLE ( 'NONE', #24228, 0.09842519685039370636 ) ;
#19595 = CARTESIAN_POINT ( 'NONE',  ( 0.7185039370078739607, 0.000000000000000000, 4.498031496062992574 ) ) ;
#19596 = CARTESIAN_POINT ( 'NONE',  ( -0.6971942568897626646, -0.07405724077823297447, 0.3986220471903312301 ) ) ;
#19597 = CARTESIAN_POINT ( 'NONE',  ( -0.07405724077823318263, -1.795399558780420124, -0.1787899950787401604 ) ) ;
#19598 = ORIENTED_EDGE ( 'NONE', *, *, #39152, .F. ) ;
#19599 = AXIS2_PLACEMENT_3D ( 'NONE', #3635, #18256, #6990 ) ;
#19600 = CARTESIAN_POINT ( 'NONE',  ( 3.284318927891251994E-17, -1.412893700733637958, 0.1787899950787401882 ) ) ;
#19601 = CARTESIAN_POINT ( 'NONE',  ( -1.094772975963752103E-17, -1.585137795221826629, -0.1787899950787401882 ) ) ;
#19602 = SURFACE_STYLE_USAGE ( .BOTH. , #41140 ) ;
#19603 = CARTESIAN_POINT ( 'NONE',  ( 0.1631287631785732217, -0.08016276244899019077, 0.1388449842062895456 ) ) ;
#19604 = CARTESIAN_POINT ( 'NONE',  ( 0.8759842519685039353, 0.1574803149606299191, 0.4527559055118110520 ) ) ;
#19605 = CARTESIAN_POINT ( 'NONE',  ( 0.5314960629921260393, 0.000000000000000000, 4.498031496062992574 ) ) ;
#19606 = CARTESIAN_POINT ( 'NONE',  ( -0.7185039370078746268, -0.06523048226347956391, 1.281988188868851575 ) ) ;
#19607 = CARTESIAN_POINT ( 'NONE',  ( 0.9500414927467378812, -0.1787899950787401604, 0.4921259841982048577 ) ) ;
#19608 = CARTESIAN_POINT ( 'NONE',  ( 1.002407869896990045, -0.1264236179284866091, 0.05659448813521283234 ) ) ;
#19610 = LINE ( 'NONE', #41617, #33140 ) ;
#19609 = CARTESIAN_POINT ( 'NONE',  ( 0.06523048226347956391, -0.4089566929133856554, 0.1574803149606297803 ) ) ;
#19611 = CARTESIAN_POINT ( 'NONE',  ( 0.7185039370078739607, 1.928577636452523993E-17, 0.3346456691838114450 ) ) ;
#19612 = ORIENTED_EDGE ( 'NONE', *, *, #21912, .F. ) ;
#19613 = CARTESIAN_POINT ( 'NONE',  ( 0.1673228346456693827, 0.06415291647593675262, -0.1630605872086743346 ) ) ;
#19614 = CARTESIAN_POINT ( 'NONE',  ( 1.033464566929133799, 0.000000000000000000, 1.112204724409448842 ) ) ;
#19615 = CARTESIAN_POINT ( 'NONE',  ( -0.06523048226347956391, -0.5615157479239690774, 0.1574803149606297803 ) ) ;
#19616 = LINE ( 'NONE', #20089, #9281 ) ;
#19617 = CARTESIAN_POINT ( 'NONE',  ( -0.7646288533564489232, -0.1113553986120547346, 1.254921259842519676 ) ) ;
#19618 = CARTESIAN_POINT ( 'NONE',  ( -0.1348413527256734357, -0.08956084189530488793, 0.09142978980987383208 ) ) ;
#19619 = CARTESIAN_POINT ( 'NONE',  ( -0.1264236179284866091, -0.4778543306548976854, -0.1264236179284866091 ) ) ;
#19620 = ORIENTED_EDGE ( 'NONE', *, *, #47295, .F. ) ;
#19621 = CARTESIAN_POINT ( 'NONE',  ( 0.7185039370078739607, 1.928577636452523993E-17, 0.05905511800270921846 ) ) ;
#19622 = CARTESIAN_POINT ( 'NONE',  ( 0.7646288533564489232, -0.1113553986120547346, 0.2706692913385826960 ) ) ;
#19623 = CARTESIAN_POINT ( 'NONE',  ( 0.6971942568897626646, 0.07405724077823318263, 0.7480314960092282472 ) ) ;
#19624 = ORIENTED_EDGE ( 'NONE', *, *, #13291, .T. ) ;
#19625 = CARTESIAN_POINT ( 'NONE',  ( 0.7646288533564489232, -0.1113553986120547346, 0.8218503937007874960 ) ) ;
#19626 = LINE ( 'NONE', #4506, #21981 ) ;
#19627 = CARTESIAN_POINT ( 'NONE',  ( -0.1787899950787401604, -0.9084645668753701386, 0.07405724077823318263 ) ) ;
#19628 = CARTESIAN_POINT ( 'NONE',  ( -0.06523048226347956391, -1.255413385826771533, -0.1574803149606300301 ) ) ;
#19629 = CARTESIAN_POINT ( 'NONE',  ( 0.9412147342319837628, -0.1574803149606297803, 1.055610236112945799 ) ) ;
#19630 = DIRECTION ( 'NONE',  ( 3.547931780924148305E-15, -0.7880107536067215701, 0.6156614753256588468 ) ) ;
#19631 = CARTESIAN_POINT ( 'NONE',  ( -0.6971942568897626646, 0.07405724077823318263, 0.4724409448281262636 ) ) ;
#19632 = ORIENTED_EDGE ( 'NONE', *, *, #14732, .T. ) ;
#19633 = EDGE_LOOP ( 'NONE', ( #40007, #47346, #40923, #47015 ) ) ;
#19634 = CARTESIAN_POINT ( 'NONE',  ( -0.6971942568897648851, -0.07405724077823297447, 1.820866141678520789 ) ) ;
#19635 = CARTESIAN_POINT ( 'NONE',  ( 0.6971942568897648851, -0.07405724077823297447, 1.860236220418677089 ) ) ;
#19636 = VERTEX_POINT ( 'NONE', #31020 ) ;
#19637 = CARTESIAN_POINT ( 'NONE',  ( -0.1574803149606297803, -1.393208661309796925, 0.06523048226347956391 ) ) ;
#19638 = CARTESIAN_POINT ( 'NONE',  ( 0.7185039370078746268, -0.06523048226347956391, 1.764271653543307616 ) ) ;
#19639 = CARTESIAN_POINT ( 'NONE',  ( 0.8019270111902717657, 0.1787899950787401604, 0.4330708660879683536 ) ) ;
#19640 = CARTESIAN_POINT ( 'NONE',  ( -0.8019270111902717657, 0.1787899950787401604, 1.373031496009229135 ) ) ;
#19641 = CARTESIAN_POINT ( 'NONE',  ( 1.033464566929133799, 0.000000000000000000, 1.968503936900346529 ) ) ;
#19642 = CARTESIAN_POINT ( 'NONE',  ( -0.8759842519685039353, -0.1787899950787401882, 1.390255905458047447 ) ) ;
#19643 = EDGE_CURVE ( 'NONE', #41828, #23265, #38661, .T. ) ;
#19644 = CARTESIAN_POINT ( 'NONE',  ( -0.9500414927467378812, -0.1787899950787401604, 0.8809055117572599514 ) ) ;
#19645 = CARTESIAN_POINT ( 'NONE',  ( -1.054774247047244096, 0.000000000000000000, 0.06643700782025216411 ) ) ;
#19646 = EDGE_CURVE ( 'NONE', #1242, #15275, #15348, .T. ) ;
#19647 = CARTESIAN_POINT ( 'NONE',  ( -0.8019270111902717657, 0.1787899950787401604, 1.692913385773008539 ) ) ;
#19648 = CARTESIAN_POINT ( 'NONE',  ( -0.9412147342319837628, 0.1574803149606300301, 1.975885826664125711 ) ) ;
#19649 = CARTESIAN_POINT ( 'NONE',  ( -1.284448818897637956, -0.3937007874015748254, 1.181102362204724310 ) ) ;
#19650 = CARTESIAN_POINT ( 'NONE',  ( -1.033464566929134687, 0.06523048226347956391, 1.823326771653542178 ) ) ;
#19651 = CARTESIAN_POINT ( 'NONE',  ( -0.9412147342319837628, 0.1574803149606300301, 0.2928149606299214613 ) ) ;
#19652 = CARTESIAN_POINT ( 'NONE',  ( 1.054774247047244096, 0.000000000000000000, 1.562499999946236118 ) ) ;
#19653 = CARTESIAN_POINT ( 'NONE',  ( 0.04598081178002756675, -0.09851382463604664574, 0.1460396181123653492 ) ) ;
#19654 = CARTESIAN_POINT ( 'NONE',  ( 0.7185039370078746268, 0.06523048226347956391, 0.2140748030420794590 ) ) ;
#19655 = ADVANCED_FACE ( 'NONE', ( #11265, #2693 ), #14214, .T. ) ;
#19656 = EDGE_CURVE ( 'NONE', #6130, #35620, #28851, .T. ) ;
#19657 = VERTEX_POINT ( 'NONE', #32191 ) ;
#19658 = ORIENTED_EDGE ( 'NONE', *, *, #20676, .T. ) ;
#19659 = CARTESIAN_POINT ( 'NONE',  ( -0.1787899950787401882, -0.9502952755367874982, 0.000000000000000000 ) ) ;
#19660 = CARTESIAN_POINT ( 'NONE',  ( 3.284318927891251994E-17, -1.053641732229700700, 0.1787899950787401882 ) ) ;
#19661 = CARTESIAN_POINT ( 'NONE',  ( -0.7646288533564489232, -0.1113553986120547346, 0.5856299212598424786 ) ) ;
#19662 = CARTESIAN_POINT ( 'NONE',  ( 0.6971942568897637749, 2.189545951927499583E-17, 1.813484251914740053 ) ) ;
#19663 = CARTESIAN_POINT ( 'NONE',  ( 0.8759842519685039353, 0.1787899950787401882, 0.3863188975840318173 ) ) ;
#19664 = CARTESIAN_POINT ( 'NONE',  ( 0.1270800023317771588, -0.4094926284806834071, -0.1270800023317771588 ) ) ;
#19665 = CARTESIAN_POINT ( 'NONE',  ( 0.1574803149606299191, -1.809055118002708795, -1.928577636452523993E-17 ) ) ;
#19666 = CARTESIAN_POINT ( 'NONE',  ( 2.892866454678787531E-17, 0.1003937007874015908, 0.1574803149606299191 ) ) ;
#19667 = CARTESIAN_POINT ( 'NONE',  ( 0.1787899950787401882, -0.1825787401037169411, -2.189545951927503898E-17 ) ) ;
#19668 = CARTESIAN_POINT ( 'NONE',  ( -0.8107537697050254399, 0.1574803149606300301, 0.1402559055118110520 ) ) ;
#19669 = CARTESIAN_POINT ( 'NONE',  ( 0.8019270111902717657, -0.1787899950787401604, 0.9940944881352130613 ) ) ;
#19670 = ( BOUNDED_CURVE ( )  B_SPLINE_CURVE ( 2, ( #6705, #21318, #19625, #26121, #15334, #5005, #12216, #33808, #4760 ),
 .UNSPECIFIED., .F., .T. ) 
 B_SPLINE_CURVE_WITH_KNOTS ( ( 3, 2, 2, 2, 3 ),
 ( 0.4099999999999999756, 0.4124999999999999778, 0.4149999999999999800, 0.4174999999999999822, 0.4199999999999999845 ),
 .UNSPECIFIED. ) 
 CURVE ( )  GEOMETRIC_REPRESENTATION_ITEM ( )  RATIONAL_B_SPLINE_CURVE ( ( 1.000000000000000000, 0.9238795325112879597, 1.000000000000000000, 0.9238795325112869605, 1.000000000000000000, 0.9238795325112869605, 1.000000000000000000, 0.9238795325112869605, 1.000000000000000000 ) ) 
 REPRESENTATION_ITEM ( '' )  ) ;
#19671 = CARTESIAN_POINT ( 'NONE',  ( 0.1577476715125368523, -0.03207557811198601810, 0.1404216743935849665 ) ) ;
#19672 = CARTESIAN_POINT ( 'NONE',  ( 1.002407869896990045, 0.1264236179284866091, 1.921751968450173376 ) ) ;
#19673 = DIRECTION ( 'NONE',  ( 1.822029033848725028E-16, 0.000000000000000000, 1.000000000000000000 ) ) ;
#19674 = CARTESIAN_POINT ( 'NONE',  ( 0.1787899950787401882, -0.4581692912848189247, -2.189545951927503898E-17 ) ) ;
#19675 = DIRECTION ( 'NONE',  ( -1.000000000000000000, 0.000000000000000000, 0.000000000000000000 ) ) ;
#19677 = AXIS2_PLACEMENT_3D ( 'NONE', #21149, #42940, #4054 ) ;
#19676 = CARTESIAN_POINT ( 'NONE',  ( -0.1264236179284866091, -1.186515747977732183, -0.1264236179284866091 ) ) ;
#19678 = CARTESIAN_POINT ( 'NONE',  ( 0.6971942568897626646, 0.07405724077823318263, 0.3198818897100162983 ) ) ;
#19679 = CARTESIAN_POINT ( 'NONE',  ( -0.6971942568897648851, 0.07405724077823318263, 1.732283464513166615 ) ) ;
#19680 = EDGE_LOOP ( 'NONE', ( #36907, #34860, #42248, #33722 ) ) ;
#19681 = CARTESIAN_POINT ( 'NONE',  ( -1.054774247047244096, 0.000000000000000000, 1.365649606245448844 ) ) ;
#19682 = CARTESIAN_POINT ( 'NONE',  ( -1.033464566929134687, 0.06523048226347956391, 1.311515748031496509 ) ) ;
#19683 = CARTESIAN_POINT ( 'NONE',  ( -0.6971942568897637749, 2.189545951927499583E-17, 1.144192913332062966 ) ) ;
#19684 = CARTESIAN_POINT ( 'NONE',  ( 0.2362204724409449064, -0.5708661417322835607, 0.9783464566929134243 ) ) ;
#19685 = CARTESIAN_POINT ( 'NONE',  ( 0.07255072011368295104, -0.09842519689660865490, -0.1635392243539251500 ) ) ;
#19686 = DIRECTION ( 'NONE',  ( 0.000000000000000000, 0.2126700594527830002, -0.9771240687918550938 ) ) ;
#19687 = CARTESIAN_POINT ( 'NONE',  ( 1.054774247047244540, 0.07405724077823318263, 0.5019685038832443214 ) ) ;
#19688 = CARTESIAN_POINT ( 'NONE',  ( -0.7495606340400177148, 0.1264236179284866091, 0.3124999999462365619 ) ) ;
#19689 = EDGE_LOOP ( 'NONE', ( #8855, #47161, #6153, #22024 ) ) ;
#19690 = EDGE_CURVE ( 'NONE', #6678, #30877, #9804, .T. ) ;
#19691 = DIRECTION ( 'NONE',  ( -0.8660254037844382635, 0.5000000000000007772, 0.000000000000000000 ) ) ;
#19692 = VERTEX_POINT ( 'NONE', #13498 ) ;
#19693 = B_SPLINE_SURFACE_WITH_KNOTS ( 'NONE', 1, 3, ( 
 ( #15658, #41716, #8918, #15895, #23546, #528, #15416, #1240, #26444, #30067, #44604, #8200, #11820, #22823, #19225, #30297, #24484, #30984, #20164, #9872, #17051, #45551, #19928, #42197, #1959, #41949, #16363, #27406, #28096, #12771, #20874, #24018, #9403, #45794, #24715, #9155, #2190, #34564, #13243, #23772, #6249, #13467, #1716, #39077, #2657, #17288, #13000, #38620, #31693, #38382, #35043, #35516, #39315, #31923, #5555, #16592, #34817, #5797, #20403, #31217, #27643, #24255, #46507, #16812, #42658, #31450, #13688, #46034, #27871, #42430, #9637, #28324, #38852, #46273, #6017, #2421, #42893, #20639, #10103, #35284, #18236, #3849, #25193, #29066, #39555, #32880, #43624, #36462, #33121, #40257, #21108, #21595, #3133, #28822, #44102, #10595, #2882, #3619, #2524, #10348, #29551, #39779, #35747, #40021, #43865, #6728, #14646, #17518, #29318, #14179, #25685, #32155, #28577, #6971, #46743, #25446, #32647, #24957, #21346, #47232, #46985, #7215, #21839, #37628, #22293, #8147, #30473, #12492, #8625, #29777, #37151, #36928, #44558, #26394, #4080, #4299, #44797, #23262, #33357, #1191, #11776, #19653, #7676, #15132, #40719, #15362, #45029, #44326, #4786, #11529 ),
 ( #19412, #37878, #40957, #949, #26149, #34062, #15608, #23015, #5031, #26867, #45272, #22771, #18932, #30012, #30706, #37380, #18696, #15850, #12244, #7918, #41428, #4535, #40489, #26631, #34297, #22533, #1422, #16081, #478, #704, #33591, #19172, #33829, #30246, #12010, #41183, #8386, #9589, #2370, #45747, #19887, #42145, #12955, #30944, #27595, #9826, #6199, #45505, #9353, #13420, #39031, #24210, #17005, #28052, #20823, #42391, #20122, #35462, #31874, #34769, #24431, #38577, #45987, #16770, #31644, #38105, #27359, #46220, #38810, #5269, #27118, #1911, #9111, #1668, #23503, #34515, #35236, #16316, #42612, #31174, #16547, #5508, #46453, #12729, #23974, #41665, #20360, #41902, #2606, #20589, #8870, #17238, #23731, #38335, #5746, #34999, #2144, #31411, #13195, #27831, #5970, #40198, #43333, #29261, #6439, #32351, #32820, #14121, #11005, #14359, #28763, #22005, #32587, #13876, #18179, #25132, #32098, #28518, #18410, #33059, #25623, #24903, #6908, #47176, #47413, #28275, #39722, #14587, #39499, #21531, #43564, #36168, #3322, #17935, #29007, #10049, #10776, #7395, #25387, #36630, #39964, #7156, #36408, #4467, #26082, #22472, #419, #44493, #41359, #29493 ),
 ( #7854, #44966, #11710, #19108, #37318, #4723, #11238, #15071, #37563, #44733, #25849, #14826, #37090, #29718, #22229, #44037, #7613, #8322, #40431, #1129, #4238, #18868, #40657, #4963, #36862, #29948, #4017, #40896, #18636, #15788, #41125, #33296, #19347, #30417, #12177, #33527, #15296, #11949, #44264, #26335, #26801, #19590, #8562, #11464, #8089, #22712, #33773, #884, #15544, #30188, #26570, #23196, #22953, #37810, #5441, #13361, #1365, #8800, #34452, #9045, #38754, #23433, #31340, #38041, #16711, #45923, #30884, #13138, #9527, #27773, #1598, #20533, #16483, #2312, #16252, #20058, #5198, #27989, #31113, #16942, #27047, #41840, #35168, #34701, #31582, #34937, #38274, #42556, #20294, #45444, #46165, #1845, #19824, #45203, #38971, #6136, #9762, #12666, #27530, #2083, #24151, #34234, #45678, #24373, #27291, #23666, #42332, #12895, #42082, #9287, #23907, #16019, #30642, #12427, #38513, #41595, #39911, #39202, #35408, #25076, #46633, #43028, #20990, #17647, #14537, #2547, #6379, #13576, #21469, #17884, #10954, #6622, #35861, #32529, #28214, #28704, #17403, #47114, #7099, #36357, #28949, #14306, #43277, #43510, #21235, #6851, #13817, #9993, #3013, #24603 ) ),
 .UNSPECIFIED., .F., .F., .F.,
 ( 2, 1, 2 ),
 ( 4, 2, 2, 2, 2, 2, 2, 2, 2, 2, 2, 2, 2, 2, 2, 2, 2, 2, 2, 2, 2, 2, 2, 2, 2, 2, 2, 2, 2, 2, 2, 2, 2, 2, 2, 2, 2, 2, 2, 2, 2, 2, 2, 2, 2, 2, 2, 2, 2, 2, 2, 2, 2, 2, 2, 2, 2, 2, 2, 2, 2, 2, 2, 2, 2, 2, 2, 2, 2, 2, 2, 2, 2, 2, 4 ),
 ( -0.01000000000000000021, 0.000000000000000000, 1.000000000000000000 ),
 ( 0.001590707300269399854, 0.003174300033026545165, 0.003966096399405114568, 0.004757892765783690477, 0.005549689132162260313, 0.005945587315351550002, 0.006341485498540830150, 0.007133281864919399987, 0.007925078231297981099, 0.009508670964055120772, 0.01030046733043370015, 0.01109226369681226045, 0.01188406006319083982, 0.01227995824638011997, 0.01267585642956940012, 0.01346765279594797950, 0.01386355097913725964, 0.01425944916232653979, 0.01584304189508370028, 0.01663483826146225017, 0.01742663462784084863, 0.01782253281103009929, 0.01821843099421939852, 0.01901022736059800045, 0.01980202372697655033, 0.02019792191016584956, 0.02059382009335514879, 0.02138561645973369868, 0.02178151464292299791, 0.02217741282611225204, 0.02376100555886940038, 0.02455280192524800231, 0.02534459829162654873, 0.02613639465800515066, 0.02692819102438370055, 0.02732408920757299978, 0.02771998739076224696, 0.02851178375714085236, 0.02930358012351940225, 0.03009537648989799724, 0.03088717285627655060, 0.03128307103946584983, 0.03167896922265514559, 0.03247076558903369548, 0.03326256195541230087, 0.03405435832179084382, 0.03484615468816940065, 0.03563795105454799911, 0.03603384923773730181, 0.03642974742092654900, 0.03722154378730514745, 0.03801334015368370428, 0.03880513652006229580, 0.03959693288644084569, 0.03999283106963014839, 0.04038872925281945109, 0.04118052561919799404, 0.04197232198557655086, 0.04276411835195514932, 0.04355591471833369921, 0.04395181290152299497, 0.04434771108471229767, 0.04513950745109090307, 0.04553540563428010168, 0.04593130381746940438, 0.04672310018384799590, 0.04751489655022660130, 0.04830669291660510262, 0.04870259109979440532, 0.04909848928298370108, 0.04989028564936229954, 0.05068208201574090493, 0.05107798019893020069, 0.05147387838211939931, 0.05226567474849799777 ),
 .UNSPECIFIED. ) ;
#19694 = ORIENTED_EDGE ( 'NONE', *, *, #21362, .F. ) ;
#19695 = CARTESIAN_POINT ( 'NONE',  ( -0.8107537697050234415, -0.1574803149606297803, 0.3125000000000000000 ) ) ;
#19696 = CARTESIAN_POINT ( 'NONE',  ( 0.8019270111902716547, 0.1787899950787401604, 1.181102362150960428 ) ) ;
#19697 = CARTESIAN_POINT ( 'NONE',  ( -0.6971942568897648851, 0.07405724077823318263, 1.968503936954110412 ) ) ;
#19698 = CARTESIAN_POINT ( 'NONE',  ( -0.2559055118110236671, -0.08239886119520901941, -0.05512121553257845474 ) ) ;
#19699 = ORIENTED_EDGE ( 'NONE', *, *, #45386, .T. ) ;
#19700 = EDGE_CURVE ( 'NONE', #18061, #2480, #38282, .T. ) ;
#19701 = CARTESIAN_POINT ( 'NONE',  ( -1.002407869896990045, -0.1264236179284866091, 1.006397637741511808 ) ) ;
#19702 = CARTESIAN_POINT ( 'NONE',  ( -1.033464566929134687, -0.06523048226347956391, 0.3223425196850392971 ) ) ;
#19703 = B_SPLINE_CURVE_WITH_KNOTS ( 'NONE', 3,
 ( #4612, #4857, #19480, #27184, #34132, #37946, #5095, #19718, #45346, #8940, #23563, #39331, #35303, #9425, #31709, #2440, #20427, #17069, #46764, #43161, #35061, #42453, #6268 ),
 .UNSPECIFIED., .F., .F.,
 ( 4, 2, 2, 2, 2, 2, 2, 1, 2, 2, 2, 4 ),
 ( 0.000000000000000000, 0.001005003112249313116, 0.002010006224498626232, 0.002512507780623283223, 0.003015009336747939347, 0.004020012448997250729, 0.004522514005121907286, 0.005025015561246563844, 0.005527517117371220402, 0.006030018673495876093, 0.007035021785745188341, 0.008040024897994499722 ),
 .UNSPECIFIED. ) ;
#19704 = DIRECTION ( 'NONE',  ( 5.377642775528101993E-15, -1.000000000000000000, 0.000000000000000000 ) ) ;
#19705 = CARTESIAN_POINT ( 'NONE',  ( -0.07405724077823318263, -1.519809007599318695, -0.1787899950787401604 ) ) ;
#19706 = ORIENTED_EDGE ( 'NONE', *, *, #16146, .F. ) ;
#19707 = CARTESIAN_POINT ( 'NONE',  ( -0.7185039370078739607, 1.928577636452523993E-17, 1.397637795168062969 ) ) ;
#19708 = CARTESIAN_POINT ( 'NONE',  ( -0.07405724077823318263, -0.3868110235682837295, 0.1787899950787401604 ) ) ;
#19709 = CARTESIAN_POINT ( 'NONE',  ( -0.3069380822740674364, -0.04406989549021581021, 1.037494150940211357 ) ) ;
#19710 = ORIENTED_EDGE ( 'NONE', *, *, #2710, .F. ) ;
#19711 = CARTESIAN_POINT ( 'NONE',  ( 0.001132063567037208413, 0.1311094469945639218, 0.04850708733689491209 ) ) ;
#19712 = CARTESIAN_POINT ( 'NONE',  ( 0.7646288533564489232, -0.1113553986120547346, 0.7332677164279054471 ) ) ;
#19713 = AXIS2_PLACEMENT_3D ( 'NONE', #23950, #2348, #16981 ) ;
#19714 = CARTESIAN_POINT ( 'NONE',  ( -1.033464566929134687, 0.06523048226347956391, 1.429625984251967852 ) ) ;
#19715 = CARTESIAN_POINT ( 'NONE',  ( 0.8019270111902717657, 0.1787899950787401604, 1.648622047190331230 ) ) ;
#19716 = CARTESIAN_POINT ( 'NONE',  ( 0.1264236179284866091, -1.762303149552535642, 0.1264236179284866091 ) ) ;
#19717 = APPLICATION_PROTOCOL_DEFINITION ( 'draft international standard', 'automotive_design', 1998, #12884 ) ;
#19718 = CARTESIAN_POINT ( 'NONE',  ( 0.1495489095487642639, -0.09842519685039370636, 0.08573672929712505830 ) ) ;
#19719 = EDGE_CURVE ( 'NONE', #6124, #8964, #41156, .T. ) ;
#19720 = CARTESIAN_POINT ( 'NONE',  ( -1.054774247047244540, -0.07405724077823318263, 0.5757874015210393548 ) ) ;
#19722 = CARTESIAN_POINT ( 'NONE',  ( 0.4028871391076110364, 4.616380251121755931E-17, 0.000000000000000000 ) ) ;
#19721 = CARTESIAN_POINT ( 'NONE',  ( 0.1574803149606299191, -0.7952755905511811330, -1.928577636452523993E-17 ) ) ;
#19723 = CARTESIAN_POINT ( 'NONE',  ( -1.100456976456230270E-17, -1.625043809583045284, -0.1797182628040039365 ) ) ;
#19724 = CYLINDRICAL_SURFACE ( 'NONE', #5718, 0.1574803149606299191 ) ;
#19725 = CARTESIAN_POINT ( 'NONE',  ( -0.7185039370078739607, 0.000000000000000000, -2.869337061179095023E-17 ) ) ;
#19726 = CARTESIAN_POINT ( 'NONE',  ( 0.9500414927467378812, -0.1787899950787401604, 1.476377952702141449 ) ) ;
#19727 = CARTESIAN_POINT ( 'NONE',  ( 1.054774247047244540, -0.07405724077823318263, 1.830708661363559253 ) ) ;
#19728 = CARTESIAN_POINT ( 'NONE',  ( 0.8019270111902716547, 0.1787899950787401604, 0.2706692912848194243 ) ) ;
#19729 = ORIENTED_EDGE ( 'NONE', *, *, #25831, .F. ) ;
#19730 = DIRECTION ( 'NONE',  ( 1.822029033848725028E-16, 0.000000000000000000, 1.000000000000000000 ) ) ;
#19732 = CARTESIAN_POINT ( 'NONE',  ( -0.7397356941743765679, 0.08920912498191986562, 1.981439465340073536 ) ) ;
#19731 = DIRECTION ( 'NONE',  ( 0.000000000000000000, -1.000000000000000000, 0.000000000000000000 ) ) ;
#19733 = CARTESIAN_POINT ( 'NONE',  ( 0.2449982982384770469, -0.1540443988234191652, -0.2957398093692971686 ) ) ;
#19734 = CARTESIAN_POINT ( 'NONE',  ( 3.284318927891251994E-17, 0.04379921265218874454, 0.1787899950787401882 ) ) ;
#19735 = CARTESIAN_POINT ( 'NONE',  ( 0.8019270111902717657, -0.1787899950787401604, 0.4035433070328508509 ) ) ;
#19737 = CARTESIAN_POINT ( 'NONE',  ( 0.7185039370078739607, 1.928577636452523993E-17, 1.948818897530267602 ) ) ;
#19736 = CARTESIAN_POINT ( 'NONE',  ( 0.8759842519685039353, 0.1787899950787401882, 1.291830708607653477 ) ) ;
#19738 = CARTESIAN_POINT ( 'NONE',  ( 0.7185039370078739607, 0.000000000000000000, 4.498031496062992574 ) ) ;
#19739 = CARTESIAN_POINT ( 'NONE',  ( 0.9412147342319837628, 0.1574803149606300301, 0.2140748031496061965 ) ) ;
#19740 = CARTESIAN_POINT ( 'NONE',  ( 0.9412147342319837628, -0.1574803149606297803, 0.7800196849318438153 ) ) ;
#19741 = VERTEX_POINT ( 'NONE', #4756 ) ;
#19742 = CARTESIAN_POINT ( 'NONE',  ( -0.6971942568897648851, -0.07405724077823297447, 1.072834645615528659 ) ) ;
#19743 = CARTESIAN_POINT ( 'NONE',  ( -0.4240551181102362177, -0.2559055118110236116, 0.000000000000000000 ) ) ;
#19744 = CARTESIAN_POINT ( 'NONE',  ( 0.06523048226347956391, -0.03986220472440944740, -0.1574803149606300301 ) ) ;
#19745 = ORIENTED_EDGE ( 'NONE', *, *, #4160, .F. ) ;
#19747 = ORIENTED_EDGE ( 'NONE', *, *, #30758, .F. ) ;
#19746 = CARTESIAN_POINT ( 'NONE',  ( 0.1113553986120547346, -1.095472440837354400, -0.1113553986120547346 ) ) ;
#19748 = CARTESIAN_POINT ( 'NONE',  ( -0.7646288533564489232, -0.1113553986120547346, 0.4970472439869613734 ) ) ;
#19749 = CARTESIAN_POINT ( 'NONE',  ( -0.8107537697050254399, 0.1574803149606300301, 0.8095472440944886383 ) ) ;
#19750 = CARTESIAN_POINT ( 'NONE',  ( 0.8759842519685039353, 0.1787899950787401882, 1.685531496009228469 ) ) ;
#19751 = CARTESIAN_POINT ( 'NONE',  ( -0.7646288533564489232, -0.1113553986120547346, 1.294291338582677309 ) ) ;
#19752 = CARTESIAN_POINT ( 'NONE',  ( -0.9412147342319837628, -0.1574803149606297803, 1.055610236112945577 ) ) ;
#19754 = CARTESIAN_POINT ( 'NONE',  ( 0.8107537697050254399, 0.1574803149606300301, 1.951279527559056870 ) ) ;
#19753 = CARTESIAN_POINT ( 'NONE',  ( 0.8759842519685039353, 0.000000000000000000, 4.498031496062992574 ) ) ;
#19755 = CARTESIAN_POINT ( 'NONE',  ( 1.033464566929133799, 0.000000000000000000, 0.3543307085538902057 ) ) ;
#19756 = EDGE_CURVE ( 'NONE', #42619, #28693, #32225, .T. ) ;
#19757 = EDGE_CURVE ( 'NONE', #6624, #12524, #28393, .T. ) ;
#19758 = CARTESIAN_POINT ( 'NONE',  ( 1.033464566929133799, 0.000000000000000000, 1.377952755797984263 ) ) ;
#19759 = EDGE_LOOP ( 'NONE', ( #7430, #16111, #35285, #2424 ) ) ;
#19760 = VERTEX_POINT ( 'NONE', #19621 ) ;
#19761 = ADVANCED_FACE ( 'NONE', ( #30219 ), #35261, .T. ) ;
#19762 = EDGE_LOOP ( 'NONE', ( #41004, #33807, #26365, #16129 ) ) ;
#19763 = CARTESIAN_POINT ( 'NONE',  ( -1.054774247047244540, -0.07405724077823318263, 1.515748031442299526 ) ) ;
#19764 = CARTESIAN_POINT ( 'NONE',  ( 0.1113553986120547346, -0.07185039359326043928, -0.1113553986120547346 ) ) ;
#19765 = CARTESIAN_POINT ( 'NONE',  ( -0.7495606340400177148, -0.1264236179284866091, 1.390255905458047447 ) ) ;
#19766 = EDGE_CURVE ( 'NONE', #33336, #4491, #29982, .T. ) ;
#19767 = EDGE_LOOP ( 'NONE', ( #17913, #24417, #21784, #450 ) ) ;
#19768 = DIRECTION ( 'NONE',  ( 0.000000000000000000, 0.000000000000000000, 1.000000000000000000 ) ) ;
#19769 = CARTESIAN_POINT ( 'NONE',  ( -0.7185039370078739607, 1.928577636452523993E-17, 1.870078740049952559 ) ) ;
#19770 = CARTESIAN_POINT ( 'NONE',  ( -0.1264236179284866091, -1.035064913111127805, 0.1264236179284866091 ) ) ;
#19771 = ORIENTED_EDGE ( 'NONE', *, *, #7379, .F. ) ;
#19772 = CARTESIAN_POINT ( 'NONE',  ( 0.07405724077823318263, -0.02755905506434671789, 0.1787899950787401604 ) ) ;
#19773 = VERTEX_POINT ( 'NONE', #27083 ) ;
#19774 = VERTEX_POINT ( 'NONE', #11496 ) ;
#19775 = FACE_OUTER_BOUND ( 'NONE', #19055, .T. ) ;
#19776 = CARTESIAN_POINT ( 'NONE',  ( 0.8107537697050234415, -0.1574803149606297803, 0.1058070865066461363 ) ) ;
#19777 = CIRCLE ( 'NONE', #25912, 0.1003937007874011050 ) ;
#19778 = CARTESIAN_POINT ( 'NONE',  ( -0.07405724077823318263, -0.6427165353793066194, -0.1787899950787401604 ) ) ;
#19779 = CIRCLE ( 'NONE', #34343, 0.04921259842519683236 ) ;
#19780 = CARTESIAN_POINT ( 'NONE',  ( -0.8759842519685039353, 0.1574803149606299191, 1.082677165354330784 ) ) ;
#19781 = CARTESIAN_POINT ( 'NONE',  ( 0.1270800023317771588, -1.127996565488557090, 0.1270800023317771588 ) ) ;
#19782 = CARTESIAN_POINT ( 'NONE',  ( 0.8019270111902717657, 0.1787899950787401604, 0.9055118109698585549 ) ) ;
#19783 = CARTESIAN_POINT ( 'NONE',  ( 1.054774247047244096, 0.000000000000000000, 1.400098425143086800 ) ) ;
#19784 = CARTESIAN_POINT ( 'NONE',  ( 0.9500414927467377701, -0.1787899950787401604, 0.1328740156942679884 ) ) ;
#19785 = DIRECTION ( 'NONE',  ( 1.000000000000000000, 0.000000000000000000, -1.822029033848725275E-16 ) ) ;
#19786 = CARTESIAN_POINT ( 'NONE',  ( 1.033464566929134687, 0.06523048226347956391, 1.587106299212598826 ) ) ;
#19787 = PLANE ( 'NONE',  #30065 ) ;
#19788 = DIRECTION ( 'NONE',  ( -1.000000000000000000, 0.000000000000000000, 0.000000000000000000 ) ) ;
#19789 = CARTESIAN_POINT ( 'NONE',  ( 0.1113553986120547346, -0.7411417321759370402, -0.1113553986120547346 ) ) ;
#19790 = CARTESIAN_POINT ( 'NONE',  ( -0.1264236179284866091, 0.1225393701325037388, 0.1264236179284866091 ) ) ;
#19791 = DIRECTION ( 'NONE',  ( 1.000000000000000000, -5.472378587457090550E-15, 4.280079833532960850E-15 ) ) ;
#19792 = CARTESIAN_POINT ( 'NONE',  ( 0.7495606340400177148, -0.1264236179284866091, 0.9128937007336377363 ) ) ;
#19793 = CARTESIAN_POINT ( 'NONE',  ( 0.6971942568897648851, 0.07405724077823318263, 1.894685039316315489 ) ) ;
#19794 = CARTESIAN_POINT ( 'NONE',  ( 0.7185039370078746268, 0.06523048226347956391, 0.2928149605223941965 ) ) ;
#19795 = VERTEX_POINT ( 'NONE', #8839 ) ;
#19796 = EDGE_CURVE ( 'NONE', #7898, #28992, #19382, .T. ) ;
#19797 = CARTESIAN_POINT ( 'NONE',  ( -0.1377952755905511861, 0.1574803149606320007, 0.8070866141732283561 ) ) ;
#19798 = CARTESIAN_POINT ( 'NONE',  ( 0.7185039370078766252, -0.06523048226348168721, 1.882381889763779625 ) ) ;
#19799 = CARTESIAN_POINT ( 'NONE',  ( -0.1113553986120547346, -1.636811023514519681, -0.1113553986120547346 ) ) ;
#19800 = CARTESIAN_POINT ( 'NONE',  ( -0.8759842519685039353, -0.1574803149606299191, 0.1870078739082208508 ) ) ;
#19801 = DIRECTION ( 'NONE',  ( 0.000000000000000000, 1.000000000000000000, 0.000000000000000000 ) ) ;
#19802 = CARTESIAN_POINT ( 'NONE',  ( 0.8019270111902717657, -0.1787899950787401604, 1.151574803095843036 ) ) ;
#19803 = ORIENTED_EDGE ( 'NONE', *, *, #15366, .F. ) ;
#19804 = CARTESIAN_POINT ( 'NONE',  ( 0.09932472909918407811, -0.09575019180979010835, 0.2280862973329967069 ) ) ;
#19805 = CARTESIAN_POINT ( 'NONE',  ( -0.1264236179284866091, 0.1126968504474643862, -0.1264236179284866091 ) ) ;
#19806 = CARTESIAN_POINT ( 'NONE',  ( -0.8759842519685039353, 0.000000000000000000, 0.000000000000000000 ) ) ;
#19807 = ADVANCED_FACE ( 'NONE', ( #44528, #1161 ), #33802, .F. ) ;
#19808 = CARTESIAN_POINT ( 'NONE',  ( -1.054774247047244096, 0.000000000000000000, 0.5733267715997795166 ) ) ;
#19809 = CYLINDRICAL_SURFACE ( 'NONE', #12250, 0.1574803149606299191 ) ;
#19810 = CARTESIAN_POINT ( 'NONE',  ( -0.05275482926409180012, 0.07559918600399900823, 0.2549750559894655155 ) ) ;
#19811 = ORIENTED_EDGE ( 'NONE', *, *, #22, .F. ) ;
#19812 = DIRECTION ( 'NONE',  ( 1.000000000000000000, 0.000000000000000000, -1.822029033848725275E-16 ) ) ;
#19813 = CIRCLE ( 'NONE', #660, 0.02900000000000001882 ) ;
#19814 = CARTESIAN_POINT ( 'NONE',  ( -0.07405724077823318263, -1.508858267662772867, -0.1787899950787401604 ) ) ;
#19815 = CARTESIAN_POINT ( 'NONE',  ( -0.8759842519685039353, -0.1787899950787401882, 1.823326771599779406 ) ) ;
#19816 = ORIENTED_EDGE ( 'NONE', *, *, #39271, .T. ) ;
#19817 = AXIS2_PLACEMENT_3D ( 'NONE', #2309, #6619, #35404 ) ;
#19818 = CARTESIAN_POINT ( 'NONE',  ( -1.002407869896990045, 0.1264236179284866091, 0.5831692912848189803 ) ) ;
#19819 = VERTEX_POINT ( 'NONE', #37594 ) ;
#19820 = CARTESIAN_POINT ( 'NONE',  ( -0.1977610074736072532, 0.1813162243850413025, -0.3078067560680682324 ) ) ;
#19821 = PRODUCT_RELATED_PRODUCT_CATEGORY ( 'part', '', ( #18798 ) ) ;
#19822 = CARTESIAN_POINT ( 'NONE',  ( -0.3094147346904633222, 0.02254976514608475827, -1.042157649583289158 ) ) ;
#19823 = CARTESIAN_POINT ( 'NONE',  ( 0.1787899950787401604, -0.5503208186229400223, 0.07405724077823318263 ) ) ;
#19824 = CARTESIAN_POINT ( 'NONE',  ( 0.02124828133781109935, -0.08956063275447755101, -0.1867302004102397717 ) ) ;
#19825 = AXIS2_PLACEMENT_3D ( 'NONE', #8782, #31323, #34677 ) ;
#19826 = CARTESIAN_POINT ( 'NONE',  ( -0.3161444924769509779, 2.177585298233989164, -3.731703755406937439 ) ) ;
#19827 = CARTESIAN_POINT ( 'NONE',  ( -0.7495606340400177148, 0.1264236179284866091, 0.5093503936470236138 ) ) ;
#19828 = CARTESIAN_POINT ( 'NONE',  ( 0.1264236179284866091, -1.802781448544200860, -0.1264236179284866091 ) ) ;
#19829 = ORIENTED_EDGE ( 'NONE', *, *, #46477, .F. ) ;
#19830 = LINE ( 'NONE', #34240, #1148 ) ;
#19831 = CARTESIAN_POINT ( 'NONE',  ( -0.8019270111902716547, -0.1787899950787401604, 1.471456692859622217 ) ) ;
#19832 = CARTESIAN_POINT ( 'NONE',  ( 0.1787899950787401604, -1.523622047190330564, 0.07405724077823318263 ) ) ;
#19833 = CARTESIAN_POINT ( 'NONE',  ( 0.000000000000000000, 0.000000000000000000, -1.181102362204724310 ) ) ;
#19834 = ( BOUNDED_CURVE ( )  B_SPLINE_CURVE ( 2, ( #9644, #24262, #42206, #38156, #31458, #46042, #23319, #34121, #9164 ),
 .UNSPECIFIED., .F., .T. ) 
 B_SPLINE_CURVE_WITH_KNOTS ( ( 3, 2, 2, 2, 3 ),
 ( 0.5000000000000000000, 0.5024999999999999467, 0.5050000000000000044, 0.5074999999999999512, 0.5100000000000000089 ),
 .UNSPECIFIED. ) 
 CURVE ( )  GEOMETRIC_REPRESENTATION_ITEM ( )  RATIONAL_B_SPLINE_CURVE ( ( 1.000000000000000000, 0.9238795325112869605, 1.000000000000000000, 0.9238795325112869605, 1.000000000000000000, 0.9238795325112869605, 1.000000000000000000, 0.9238795325112869605, 1.000000000000000000 ) ) 
 REPRESENTATION_ITEM ( '' )  ) ;
#19835 = AXIS2_PLACEMENT_3D ( 'NONE', #7706, #7001, #36949 ) ;
#19836 = CARTESIAN_POINT ( 'NONE',  ( 0.7185039370078746268, -0.06523048226347956391, 0.1894685039370079815 ) ) ;
#19837 = CARTESIAN_POINT ( 'NONE',  ( 0.1637019648883152323, -0.08049522773984678359, 0.1394218127426261888 ) ) ;
#19838 = CARTESIAN_POINT ( 'NONE',  ( 0.9412147342319837628, 0.1574803149606300301, 0.4896653543307081802 ) ) ;
#19839 = CARTESIAN_POINT ( 'NONE',  ( 0.1270800023317771588, -0.7342957780869823203, 0.1270800023317771588 ) ) ;
#19840 = DIRECTION ( 'NONE',  ( 0.000000000000000000, 0.000000000000000000, -1.000000000000000000 ) ) ;
#19841 = CARTESIAN_POINT ( 'NONE',  ( -0.9412147342319837628, 0.1574803149606300301, 1.306594488081449290 ) ) ;
#19842 = CARTESIAN_POINT ( 'NONE',  ( 0.6971942568897637749, 2.189545951927499583E-17, 0.5191929133320630774 ) ) ;
#19844 = DIRECTION ( 'NONE',  ( -0.000000000000000000, 0.2126700594527834443, -0.9771240687918547607 ) ) ;
#19843 = CARTESIAN_POINT ( 'NONE',  ( -0.06523048226347956391, -0.3745078740157483099, 0.1574803149606297803 ) ) ;
#19845 = LINE ( 'NONE', #9067, #42153 ) ;
#19846 = VERTEX_POINT ( 'NONE', #5232 ) ;
#19847 = ADVANCED_FACE ( 'NONE', ( #26116 ), #44727, .F. ) ;
#19848 = DIRECTION ( 'NONE',  ( 0.000000000000000000, 1.000000000000000000, 0.000000000000000000 ) ) ;
#19849 = CARTESIAN_POINT ( 'NONE',  ( -0.7495606340400177148, -0.1264236179284866091, 1.114665354276944909 ) ) ;
#19850 = CARTESIAN_POINT ( 'NONE',  ( 0.9412147342319837628, -0.1574803149606297803, 1.104822834645670104 ) ) ;
#19851 = DIRECTION ( 'NONE',  ( 1.000000000000000000, 0.000000000000000000, 0.000000000000000000 ) ) ;
#19852 = VECTOR ( 'NONE', #1310, 39.37007874015748143 ) ;
#19853 = CARTESIAN_POINT ( 'NONE',  ( 0.1574803149606299191, 0.08719492171395729074, -0.5641677032617165022 ) ) ;
#19855 = CARTESIAN_POINT ( 'NONE',  ( 0.7185039370078778465, -0.06523048226348396317, 1.675688976270425457 ) ) ;
#19854 = DIRECTION ( 'NONE',  ( 1.000000000000000000, 0.000000000000000000, 0.000000000000000000 ) ) ;
#19856 = CARTESIAN_POINT ( 'NONE',  ( 0.1602931993194442739, -0.07955613945526318620, 0.1377952755905511861 ) ) ;
#19857 = CARTESIAN_POINT ( 'NONE',  ( 0.1787899950787401604, -0.6082677164816695514, -0.07405724077823318263 ) ) ;
#19858 = CARTESIAN_POINT ( 'NONE',  ( 2.892866454678787531E-17, -0.04724409438066189126, 0.1574803149606299191 ) ) ;
#19859 = ORIENTED_EDGE ( 'NONE', *, *, #26804, .T. ) ;
#19860 = ADVANCED_FACE ( 'NONE', ( #44764 ), #9324, .T. ) ;
#19861 = CARTESIAN_POINT ( 'NONE',  ( 0.1608764898047789493, 0.08278099671294095185, -0.1377952755905511861 ) ) ;
#19862 = DIRECTION ( 'NONE',  ( 0.000000000000000000, -1.000000000000000000, 0.000000000000000000 ) ) ;
#19863 = VERTEX_POINT ( 'NONE', #38551 ) ;
#19864 = CARTESIAN_POINT ( 'NONE',  ( 0.7185039370078739607, 1.928577636452523993E-17, 1.200787401467275695 ) ) ;
#19865 = CARTESIAN_POINT ( 'NONE',  ( -0.9873396505805591694, 0.1113553986120547346, 0.4379921258767244252 ) ) ;
#19866 = CARTESIAN_POINT ( 'NONE',  ( -1.094772975963752103E-17, -1.742618110182456714, -0.1787899950787401882 ) ) ;
#19867 = CARTESIAN_POINT ( 'NONE',  ( -0.1264236179284866091, -0.8371062991588346103, -0.1264236179284866091 ) ) ;
#19868 = CARTESIAN_POINT ( 'NONE',  ( 0.06523048226347956391, -1.417814960629922627, -0.1574803149606300301 ) ) ;
#19869 = CARTESIAN_POINT ( 'NONE',  ( 0.9412147342319837628, 0.1574803149606300301, 1.109744094380661572 ) ) ;
#19870 = CARTESIAN_POINT ( 'NONE',  ( -1.033464566929133799, 0.000000000000000000, 1.850393700679873854 ) ) ;
#19871 = ORIENTED_EDGE ( 'NONE', *, *, #37918, .F. ) ;
#19872 = ORIENTED_EDGE ( 'NONE', *, *, #11074, .F. ) ;
#19873 = CARTESIAN_POINT ( 'NONE',  ( -0.9500414927467378812, -0.1787899950787401604, 1.830708661363559253 ) ) ;
#19874 = ORIENTED_EDGE ( 'NONE', *, *, #45431, .T. ) ;
#19875 = CARTESIAN_POINT ( 'NONE',  ( 0.1113553986120547346, 0.006889763887054606122, -0.1113553986120547346 ) ) ;
#19876 = CARTESIAN_POINT ( 'NONE',  ( -1.054774247047244096, 0.000000000000000000, 1.321358267662771757 ) ) ;
#19877 = CARTESIAN_POINT ( 'NONE',  ( 0.09011016336849961283, 0.2434714151302298513, -0.3128311589625373812 ) ) ;
#19878 = CARTESIAN_POINT ( 'NONE',  ( -0.6971942568897626646, 0.07405724077823318263, 0.9055118109698585549 ) ) ;
#19879 = CARTESIAN_POINT ( 'NONE',  ( -0.7495606340400177148, 0.1264236179284866091, 0.1205708660879689087 ) ) ;
#19880 = CIRCLE ( 'NONE', #1488, 0.1864803149606299171 ) ;
#19881 = CARTESIAN_POINT ( 'NONE',  ( -1.054774247047244096, 0.000000000000000000, 1.759350393647023614 ) ) ;
#19882 = CARTESIAN_POINT ( 'NONE',  ( -0.9500414927467378812, -0.1787899950787401604, 0.05905511805647267048 ) ) ;
#19883 = CARTESIAN_POINT ( 'NONE',  ( -0.1235961452251413406, 0.09842519685039370636, 0.2140748031496062798 ) ) ;
#19884 = CARTESIAN_POINT ( 'NONE',  ( -0.7646288533564489232, 0.1113553986120547346, 1.756889763779527547 ) ) ;
#19885 = DIRECTION ( 'NONE',  ( 0.000000000000000000, -0.000000000000000000, -1.000000000000000000 ) ) ;
#19886 = CARTESIAN_POINT ( 'NONE',  ( 0.9500414927467377701, -0.1787899950787401604, 1.673228346402929834 ) ) ;
#19887 = CARTESIAN_POINT ( 'NONE',  ( -0.05397493303295378131, -0.09842519685039370636, 0.2204705300331200601 ) ) ;
#19888 = AXIS2_PLACEMENT_3D ( 'NONE', #16124, #38377, #12767 ) ;
#19889 = ORIENTED_EDGE ( 'NONE', *, *, #21147, .T. ) ;
#19890 = ORIENTED_EDGE ( 'NONE', *, *, #46956, .F. ) ;
#19891 = CARTESIAN_POINT ( 'NONE',  ( 0.1264236179284866091, -1.014271653489543290, 0.1264236179284866091 ) ) ;
#19892 = CARTESIAN_POINT ( 'NONE',  ( 0.1787899950787401604, -1.080708661363559919, -0.07405724077823318263 ) ) ;
#19893 = CARTESIAN_POINT ( 'NONE',  ( -0.8759842519685039353, -0.1574803149606299191, 0.5905511811023621549 ) ) ;
#19894 = ( NAMED_UNIT ( * ) PLANE_ANGLE_UNIT ( ) SI_UNIT ( $, .RADIAN. ) ) ;
#19895 = CARTESIAN_POINT ( 'NONE',  ( 3.301370929368692659E-17, -0.4242564080082424915, 0.1797182628040039365 ) ) ;
#19896 = CARTESIAN_POINT ( 'NONE',  ( 0.06523048226347956391, -1.777066929026330344, 0.1574803149606297803 ) ) ;
#19897 = CARTESIAN_POINT ( 'NONE',  ( -1.033464566929133799, 0.000000000000000000, 0.8267716534357796299 ) ) ;
#19898 = CARTESIAN_POINT ( 'NONE',  ( -0.1574803149606300301, -0.03001968503937006705, -0.06523048226347956391 ) ) ;
#19899 = CARTESIAN_POINT ( 'NONE',  ( -0.07405724077823318263, -0.1309055117572600901, -0.1787899950787401604 ) ) ;
#19900 = EDGE_CURVE ( 'NONE', #38566, #35894, #24650, .T. ) ;
#19901 = CARTESIAN_POINT ( 'NONE',  ( 0.7495606340400177148, -0.1264236179284866091, 0.9128937007336377363 ) ) ;
#19902 = EDGE_CURVE ( 'NONE', #3057, #11821, #12297, .T. ) ;
#19903 = AXIS2_PLACEMENT_3D ( 'NONE', #11932, #44952, #33510 ) ;
#19904 = CARTESIAN_POINT ( 'NONE',  ( 0.1964094517284671326, 0.1820971824355889779, -0.05295753290289392790 ) ) ;
#19905 = CARTESIAN_POINT ( 'NONE',  ( 0.8759842519685039353, 0.1787899950787401882, 1.966043307032850462 ) ) ;
#19906 = EDGE_CURVE ( 'NONE', #3623, #38634, #20251, .T. ) ;
#19907 = AXIS2_PLACEMENT_3D ( 'NONE', #1563, #16447, #13324 ) ;
#19908 = EDGE_CURVE ( 'NONE', #14505, #32389, #14807, .T. ) ;
#19909 = CYLINDRICAL_SURFACE ( 'NONE', #31356, 0.1574803149606299191 ) ;
#19910 = CARTESIAN_POINT ( 'NONE',  ( 0.1787899950787401604, -0.4212598424659216856, 0.07405724077823318263 ) ) ;
#19911 = CARTESIAN_POINT ( 'NONE',  ( 0.2204724409448818867, 0.1591122789105269553, 0.000000000000000000 ) ) ;
#19912 = CARTESIAN_POINT ( 'NONE',  ( -0.07405724077823318263, -1.331692913332063855, 0.1787899950787401604 ) ) ;
#19913 = CARTESIAN_POINT ( 'NONE',  ( -0.9500414927467378812, 0.1787899950787401604, 1.722440944828125930 ) ) ;
#19914 = ORIENTED_EDGE ( 'NONE', *, *, #36817, .F. ) ;
#19915 = CARTESIAN_POINT ( 'NONE',  ( -1.054774247047244540, -0.07405724077823318263, 1.284448818843874740 ) ) ;
#19916 = DIRECTION ( 'NONE',  ( 1.000000000000000000, 0.000000000000000000, -1.822029033848725275E-16 ) ) ;
#19917 = CARTESIAN_POINT ( 'NONE',  ( 0.8019270111902717657, 0.1787899950787401604, 1.417322834591906222 ) ) ;
#19918 = CARTESIAN_POINT ( 'NONE',  ( 0.9500414927467378812, 0.1787899950787401604, 0.07381889758403178958 ) ) ;
#19919 = CARTESIAN_POINT ( 'NONE',  ( -0.8019270111902717657, -0.1787899950787401604, 1.269685039316314601 ) ) ;
#19920 = CARTESIAN_POINT ( 'NONE',  ( 0.08391120367376535272, -0.09842556176169890703, -0.1578933197585290493 ) ) ;
#19921 = CARTESIAN_POINT ( 'NONE',  ( -0.8107537697050254399, 0.1574803149606300301, 1.350885826664126821 ) ) ;
#19922 = CARTESIAN_POINT ( 'NONE',  ( 0.8759842519685039353, 0.1787899950787401882, 0.6274606298674959559 ) ) ;
#19923 = CARTESIAN_POINT ( 'NONE',  ( -1.054774247047244540, -0.07405724077823318263, 0.3346456692375752162 ) ) ;
#19924 = CARTESIAN_POINT ( 'NONE',  ( -0.05636151600970552150, -0.07780576619187905274, 0.2528927375204715888 ) ) ;
#19925 = CARTESIAN_POINT ( 'NONE',  ( 0.7185039370078739607, 1.928577636452523993E-17, 1.673228346349165285 ) ) ;
#19926 = ORIENTED_EDGE ( 'NONE', *, *, #2957, .F. ) ;
#19927 = CARTESIAN_POINT ( 'NONE',  ( -0.9412147342319837628, 0.1574803149606300301, 0.2534448818897637734 ) ) ;
#19928 = CARTESIAN_POINT ( 'NONE',  ( -0.2304365790506456846, -0.09851385065409645758, 0.06211564517574902355 ) ) ;
#19929 = CARTESIAN_POINT ( 'NONE',  ( -0.4240551181102362177, -2.591110818884263559E-17, 0.000000000000000000 ) ) ;
#19930 = ORIENTED_EDGE ( 'NONE', *, *, #14951, .F. ) ;
#19931 = CARTESIAN_POINT ( 'NONE',  ( -0.7495606340400177148, -0.1264236179284866091, 0.9571850393163149340 ) ) ;
#19932 = VECTOR ( 'NONE', #16118, 39.37007874015748854 ) ;
#19933 = CARTESIAN_POINT ( 'NONE',  ( -1.002407869896990045, 0.1264236179284866091, 0.1058070865604098382 ) ) ;
#19934 = CARTESIAN_POINT ( 'NONE',  ( 0.1787899950787401882, -1.610852314685931264, -2.189545951927503898E-17 ) ) ;
#19935 = ORIENTED_EDGE ( 'NONE', *, *, #29161, .T. ) ;
#19936 = DIRECTION ( 'NONE',  ( -1.000000000000000000, 0.000000000000000000, 0.000000000000000000 ) ) ;
#19937 = CARTESIAN_POINT ( 'NONE',  ( 0.1264236179284866091, -0.6156496062454488438, 0.1264236179284866091 ) ) ;
#19938 = CARTESIAN_POINT ( 'NONE',  ( -0.9873396505805591694, -0.1113553986120547346, 0.08366141732283464971 ) ) ;
#19939 = ORIENTED_EDGE ( 'NONE', *, *, #21733, .F. ) ;
#19940 = CARTESIAN_POINT ( 'NONE',  ( 0.9500414927467378812, 0.1787899950787401604, 1.289370078686393750 ) ) ;
#19941 = AXIS2_PLACEMENT_3D ( 'NONE', #20936, #42496, #28887 ) ;
#19942 = CARTESIAN_POINT ( 'NONE',  ( 0.4453382816733590377, 0.09842519685039370636, 0.000000000000000000 ) ) ;
#19943 = ( BOUNDED_CURVE ( )  B_SPLINE_CURVE ( 2, ( #33535, #47420, #29724, #28330, #28105, #24490, #6256, #20882, #35524 ),
 .UNSPECIFIED., .F., .T. ) 
 B_SPLINE_CURVE_WITH_KNOTS ( ( 3, 2, 2, 2, 3 ),
 ( 0.8100000000000000533, 0.8125000000000000000, 0.8149999999999999467, 0.8175000000000000044, 0.8199999999999999512 ),
 .UNSPECIFIED. ) 
 CURVE ( )  GEOMETRIC_REPRESENTATION_ITEM ( )  RATIONAL_B_SPLINE_CURVE ( ( 1.000000000000000000, 0.9238795325112869605, 1.000000000000000000, 0.9238795325112869605, 1.000000000000000000, 0.9238795325112869605, 1.000000000000000000, 0.9238795325112829637, 1.000000000000000000 ) ) 
 REPRESENTATION_ITEM ( '' )  ) ;
#19944 = CARTESIAN_POINT ( 'NONE',  ( 0.7646288533564489232, 0.1113553986120547346, 1.875000000000000000 ) ) ;
#19945 = CARTESIAN_POINT ( 'NONE',  ( 0.8019270111902717657, 0.1787899950787401604, 1.609251968450173376 ) ) ;
#19946 = CARTESIAN_POINT ( 'NONE',  ( 0.1264236179284866091, 0.1165098900384777536, 0.1264236179284866091 ) ) ;
#19947 = CARTESIAN_POINT ( 'NONE',  ( -0.1264236179284866091, -1.806594488135212728, 0.1264236179284866091 ) ) ;
#19948 = CARTESIAN_POINT ( 'NONE',  ( 0.2066929133858268486, 1.126631386849005212, -3.440787370833234604 ) ) ;
#19949 = CARTESIAN_POINT ( 'NONE',  ( 0.7495606340400177148, -0.1264236179284866091, 0.4798228345919055560 ) ) ;
#19950 = EDGE_CURVE ( 'NONE', #32133, #3713, #17674, .T. ) ;
#19951 = CARTESIAN_POINT ( 'NONE',  ( -1.002407869896990045, -0.1264236179284866091, 0.7701771653005669016 ) ) ;
#19953 = CYLINDRICAL_SURFACE ( 'NONE', #40779, 0.1574803149606299191 ) ;
#19952 = CARTESIAN_POINT ( 'NONE',  ( -0.1113553986120547346, -0.7805118110236219930, -0.1113553986120547346 ) ) ;
#19955 = CARTESIAN_POINT ( 'NONE',  ( -0.8391708915589655149, -0.1694580354647786113, 1.987530892951425043 ) ) ;
#19954 = CARTESIAN_POINT ( 'NONE',  ( -0.1270800023317771588, -1.649650108795643666, 0.1270800023317771588 ) ) ;
#19956 = CARTESIAN_POINT ( 'NONE',  ( -0.06523048226347956391, -0.04970472430192177798, 0.1574803149606297803 ) ) ;
#19957 = CARTESIAN_POINT ( 'NONE',  ( 0.1113553986120547346, -0.4655511809948346680, -0.1113553986120547346 ) ) ;
#19958 = CARTESIAN_POINT ( 'NONE',  ( 0.1787899950787401604, -0.4114173227808823330, -0.07405724077823318263 ) ) ;
#19959 = DIRECTION ( 'NONE',  ( 1.000000000000000000, 0.000000000000000000, 0.000000000000000000 ) ) ;
#19960 = CARTESIAN_POINT ( 'NONE',  ( 0.6971942568897648851, 0.07405724077823318263, 1.461614173174583753 ) ) ;
#19961 = CARTESIAN_POINT ( 'NONE',  ( 0.8759842519685039353, 0.1787899950787401882, 1.843011810969858333 ) ) ;
#19962 = CARTESIAN_POINT ( 'NONE',  ( 1.054774247047244540, 0.07405724077823318263, 0.4576771653005669016 ) ) ;
#19963 = ORIENTED_EDGE ( 'NONE', *, *, #44983, .T. ) ;
#19964 = DIRECTION ( 'NONE',  ( 0.000000000000000000, -1.000000000000000000, 0.000000000000000000 ) ) ;
#19965 = EDGE_CURVE ( 'NONE', #3128, #39269, #10985, .T. ) ;
#19966 = CARTESIAN_POINT ( 'NONE',  ( -1.033464566929133799, 1.928577636452524610E-17, 2.869337061179095023E-17 ) ) ;
#19967 = CYLINDRICAL_SURFACE ( 'NONE', #30586, 0.1574803149606299191 ) ;
#19968 = CARTESIAN_POINT ( 'NONE',  ( 0.07405724077823318263, 0.02165354336085014916, -0.1787899950787401604 ) ) ;
#19970 = CARTESIAN_POINT ( 'NONE',  ( 0.8759842519685039353, 0.1787899950787401882, 0.4256889763241890057 ) ) ;
#19969 = ( BOUNDED_CURVE ( )  B_SPLINE_CURVE ( 2, ( #27964, #6113, #24123 ),
 .UNSPECIFIED., .F., .F. ) 
 B_SPLINE_CURVE_WITH_KNOTS ( ( 3, 3 ),
 ( 0.9975000000000000533, 1.000000000000000000 ),
 .UNSPECIFIED. ) 
 CURVE ( )  GEOMETRIC_REPRESENTATION_ITEM ( )  RATIONAL_B_SPLINE_CURVE ( ( 1.000000000000000000, 0.9238795325112869605, 1.000000000000000000 ) ) 
 REPRESENTATION_ITEM ( '' )  ) ;
#19971 = CARTESIAN_POINT ( 'NONE',  ( 0.7556365493957359902, -0.1147211060030528113, 0.03937312978427136290 ) ) ;
#19972 = CARTESIAN_POINT ( 'NONE',  ( 0.6141732283464567121, 0.000000000000000000, 0.000000000000000000 ) ) ;
#19973 = AXIS2_PLACEMENT_3D ( 'NONE', #24118, #32009, #46601 ) ;
#19974 = DIRECTION ( 'NONE',  ( 1.000000000000000000, 0.000000000000000000, -1.822029033848725275E-16 ) ) ;
#19975 = CARTESIAN_POINT ( 'NONE',  ( -1.054774247047244096, 0.000000000000000000, 1.321358267662771757 ) ) ;
#19976 = CARTESIAN_POINT ( 'NONE',  ( 0.7185039370078746268, 0.06523048226347956391, 0.8046259841444418637 ) ) ;
#19977 = ORIENTED_EDGE ( 'NONE', *, *, #19544, .F. ) ;
#19978 = CARTESIAN_POINT ( 'NONE',  ( 0.9500414927467378812, 0.1787899950787401604, 1.058070866087969186 ) ) ;
#19979 = CARTESIAN_POINT ( 'NONE',  ( 0.1264236179284866091, -1.329232283410803239, 0.1264236179284866091 ) ) ;
#19980 = CARTESIAN_POINT ( 'NONE',  ( -0.7185039370078746268, 0.06523048226347956391, 0.4896653542231815259 ) ) ;
#19981 = CIRCLE ( 'NONE', #13096, 0.1864803149606300003 ) ;
#19982 = CARTESIAN_POINT ( 'NONE',  ( 1.229559056033039366E-16, -0.3937007874015746034, 0.3937007874015748254 ) ) ;
#19983 = CARTESIAN_POINT ( 'NONE',  ( 0.8019270111902717657, -0.1787899950787401604, 1.742125984198204858 ) ) ;
#19984 = CARTESIAN_POINT ( 'NONE',  ( -0.9873396505805591694, -0.1113553986120547346, 1.186023622047243986 ) ) ;
#19986 = CARTESIAN_POINT ( 'NONE',  ( -0.9412147342319837628, 0.1574803149606300301, 0.7554133857192454338 ) ) ;
#19985 = CARTESIAN_POINT ( 'NONE',  ( -0.9873396505805591694, 0.1113553986120547346, 0.7234251968503936370 ) ) ;
#19987 = CARTESIAN_POINT ( 'NONE',  ( 0.6971942568897626646, 0.07405724077823318263, 0.08366141726907130871 ) ) ;
#19988 = CARTESIAN_POINT ( 'NONE',  ( 1.033464566929134687, -0.06523048226347956391, 1.493602362097197211 ) ) ;
#19989 = EDGE_LOOP ( 'NONE', ( #28824, #22824, #34185, #45239 ) ) ;
#19990 = ORIENTED_EDGE ( 'NONE', *, *, #19204, .F. ) ;
#19991 = ORIENTED_EDGE ( 'NONE', *, *, #39545, .T. ) ;
#19992 = AXIS2_PLACEMENT_3D ( 'NONE', #1280, #4879, #19505 ) ;
#19993 = CARTESIAN_POINT ( 'NONE',  ( 0.8019270111902716547, 0.1787899950787401604, 0.9842519684501743749 ) ) ;
#19994 = CARTESIAN_POINT ( 'NONE',  ( -0.6971942568897648851, 0.07405724077823318263, 1.614173228292692386 ) ) ;
#19995 = CARTESIAN_POINT ( 'NONE',  ( 2.892866454678787531E-17, -0.04724409438066189126, 0.1574803149606299191 ) ) ;
#19996 = CARTESIAN_POINT ( 'NONE',  ( -0.7495606340400177148, -0.1264236179284866091, 1.468996062938362046 ) ) ;
#19997 = EDGE_CURVE ( 'NONE', #43450, #31512, #40112, .T. ) ;
#19998 = CARTESIAN_POINT ( 'NONE',  ( -0.9873396505805591694, 0.1113553986120547346, 0.2411417321759374011 ) ) ;
#19999 = FACE_OUTER_BOUND ( 'NONE', #19989, .T. ) ;
#20000 = CARTESIAN_POINT ( 'NONE',  ( 0.2642359194686346169, 4.766607801171850497E-17, 0.000000000000000000 ) ) ;
#20001 = CARTESIAN_POINT ( 'NONE',  ( 0.1787899950787401882, -1.217151527284356272, -2.189545951927503898E-17 ) ) ;
#20002 = EDGE_LOOP ( 'NONE', ( #20875, #36175, #11225, #31063 ) ) ;
#20003 = CARTESIAN_POINT ( 'NONE',  ( -0.1264236179284866091, 0.07332677170730689253, -0.1264236179284866091 ) ) ;
#20004 = ORIENTED_EDGE ( 'NONE', *, *, #38758, .T. ) ;
#20005 = CARTESIAN_POINT ( 'NONE',  ( 0.8759842519685039353, 0.1574803149606299191, 1.742125984144440975 ) ) ;
#20006 = LINE ( 'NONE', #37996, #42160 ) ;
#20007 = AXIS2_PLACEMENT_3D ( 'NONE', #2912, #20903, #42923 ) ;
#20008 = CARTESIAN_POINT ( 'NONE',  ( 0.8759842519685039353, 0.1574803149606299191, 1.830708661417322913 ) ) ;
#20009 = AXIS2_PLACEMENT_3D ( 'NONE', #21336, #38613, #46265 ) ;
#20010 = CARTESIAN_POINT ( 'NONE',  ( -0.1787899950787401604, -0.6377952755367874982, -0.07405724077823318263 ) ) ;
#20011 = ORIENTED_EDGE ( 'NONE', *, *, #31414, .T. ) ;
#20012 = AXIS2_PLACEMENT_3D ( 'NONE', #5219, #20320, #23687 ) ;
#20013 = EDGE_CURVE ( 'NONE', #32919, #11416, #46953, .T. ) ;
#20014 = CARTESIAN_POINT ( 'NONE',  ( -1.002407869896990045, 0.1264236179284866091, 0.2682086613635594752 ) ) ;
#20015 = CARTESIAN_POINT ( 'NONE',  ( -0.9412147342319837628, -0.1574803149606297803, 1.065452755905511806 ) ) ;
#20016 = CARTESIAN_POINT ( 'NONE',  ( 0.1797182628040039087, -1.199354833205092730, -0.07444174185955065859 ) ) ;
#20017 = CARTESIAN_POINT ( 'NONE',  ( 0.1641447577951997139, 0.1299212598425197596, -0.05120236303050382243 ) ) ;
#20018 = CARTESIAN_POINT ( 'NONE',  ( 1.002407869896990045, 0.1264236179284866091, 1.016240157426551161 ) ) ;
#20019 = CARTESIAN_POINT ( 'NONE',  ( 1.054774247047244540, 0.07405724077823318263, 0.1427165353793073133 ) ) ;
#20020 = DIRECTION ( 'NONE',  ( -5.244653365444468611E-15, 0.2126700594527759225, -0.9771240687918565371 ) ) ;
#20021 = ADVANCED_FACE ( 'NONE', ( #3045 ), #25108, .T. ) ;
#20022 = CARTESIAN_POINT ( 'NONE',  ( 0.7646288533564489232, -0.1113553986120547346, 1.569881889763779625 ) ) ;
#20024 = CARTESIAN_POINT ( 'NONE',  ( -0.1550611416717992963, -0.2059691479693902261, -0.3138705397960867005 ) ) ;
#20023 = CARTESIAN_POINT ( 'NONE',  ( 0.8024386162957400925, 0.1423545520052694469, 1.979847512675880994 ) ) ;
#20025 = CARTESIAN_POINT ( 'NONE',  ( -0.7185039370078739607, 0.000000000000000000, -2.869337061179095023E-17 ) ) ;
#20026 = CARTESIAN_POINT ( 'NONE',  ( 0.1787899950787401604, 0.05610236225848785896, 0.07405724077823318263 ) ) ;
#20027 = FACE_OUTER_BOUND ( 'NONE', #15011, .T. ) ;
#20028 = CARTESIAN_POINT ( 'NONE',  ( 0.6971942568897648851, 0.07405724077823318263, 0.9842519684501743749 ) ) ;
#20029 = CARTESIAN_POINT ( 'NONE',  ( 0.8019270111902716547, -0.1787899950787401604, 1.825787401521040243 ) ) ;
#20030 = CARTESIAN_POINT ( 'NONE',  ( 1.033464566929134687, 0.06523048226347956391, 0.3174212597349925224 ) ) ;
#20031 = ORIENTED_EDGE ( 'NONE', *, *, #36822, .T. ) ;
#20032 = CARTESIAN_POINT ( 'NONE',  ( 0.2871444924769515628, 0.9382165298418956301, -1.070508272602716637 ) ) ;
#20033 = DIRECTION ( 'NONE',  ( 1.822029033848725028E-16, 0.000000000000000000, 1.000000000000000000 ) ) ;
#20034 = CARTESIAN_POINT ( 'NONE',  ( -0.1574803149606299191, -1.749999999892472458, 0.000000000000000000 ) ) ;
#20035 = CARTESIAN_POINT ( 'NONE',  ( -0.7646288533564489232, -0.1113553986120547346, 0.1820866140657015630 ) ) ;
#20036 = CARTESIAN_POINT ( 'NONE',  ( -0.1787899950787401604, -0.08169291333206318839, -0.07405724077823318263 ) ) ;
#20037 = CARTESIAN_POINT ( 'NONE',  ( 0.8759842519685039353, 0.1787899950787401882, 1.291830708607653477 ) ) ;
#20038 = PRESENTATION_LAYER_ASSIGNMENT (  '', '', ( #25515 ) ) ;
#20039 = ORIENTED_EDGE ( 'NONE', *, *, #15828, .F. ) ;
#20040 = CARTESIAN_POINT ( 'NONE',  ( 0.7185039370078714072, 0.06523048226347728795, 1.237696850286174932 ) ) ;
#20041 = DIMENSIONAL_EXPONENTS ( 1.000000000000000000, 0.000000000000000000, 0.000000000000000000, 0.000000000000000000, 0.000000000000000000, 0.000000000000000000, 0.000000000000000000 ) ;
#20042 = CARTESIAN_POINT ( 'NONE',  ( -0.1574803149606300301, -1.762303149606299968, -0.06523048226347956391 ) ) ;
#20043 = CARTESIAN_POINT ( 'NONE',  ( 0.7185039370078739607, 0.000000000000000000, 4.498031496062992574 ) ) ;
#20044 = AXIS2_PLACEMENT_3D ( 'NONE', #21754, #39941, #21501 ) ;
#20045 = CARTESIAN_POINT ( 'NONE',  ( 0.8759842519685039353, 0.1574803149606299191, 0.2559055118110236116 ) ) ;
#20046 = CARTESIAN_POINT ( 'NONE',  ( 0.1377952755905513804, 1.687505431895961653E-17, -0.3001770169643759867 ) ) ;
#20047 = EDGE_LOOP ( 'NONE', ( #20104, #35920, #16085, #25432 ) ) ;
#20048 = CARTESIAN_POINT ( 'NONE',  ( -0.1787899950787401604, -1.538385826717890703, 0.07405724077823318263 ) ) ;
#20049 = CARTESIAN_POINT ( 'NONE',  ( -0.7495606340400177148, 0.1264236179284866091, 0.9867125983714331028 ) ) ;
#20050 = AXIS2_PLACEMENT_3D ( 'NONE', #26221, #33655, #26459 ) ;
#20051 = CARTESIAN_POINT ( 'NONE',  ( -1.054774247047244540, -0.07405724077823318263, 1.870078740103715331 ) ) ;
#20052 = CARTESIAN_POINT ( 'NONE',  ( -0.8759842519685039353, 0.1787899950787401882, 0.6274606298674959559 ) ) ;
#20053 = EDGE_CURVE ( 'NONE', #14779, #13566, #19158, .T. ) ;
#20054 = CARTESIAN_POINT ( 'NONE',  ( -0.2343326035689475839, 0.1601959449158263660, -0.2989494884452092993 ) ) ;
#20055 = CARTESIAN_POINT ( 'NONE',  ( 0.1459804379636932548, 0.1272537536561319516, -0.07636242287093111814 ) ) ;
#20056 = PLANE ( 'NONE',  #28255 ) ;
#20057 = CARTESIAN_POINT ( 'NONE',  ( -0.1787899950787401882, -0.5675452280717583342, 0.000000000000000000 ) ) ;
#20058 = CARTESIAN_POINT ( 'NONE',  ( 0.1913537776491429088, -0.08956048629241221415, -0.05990061976413484091 ) ) ;
#20059 = CYLINDRICAL_SURFACE ( 'NONE', #31802, 0.1574803149606299191 ) ;
#20060 = ORIENTED_EDGE ( 'NONE', *, *, #20654, .F. ) ;
#20061 = DIRECTION ( 'NONE',  ( -1.000000000000000000, 0.000000000000000000, 0.000000000000000000 ) ) ;
#20062 = CARTESIAN_POINT ( 'NONE',  ( 0.4142125984251969206, -0.1870078740157480324, 0.000000000000000000 ) ) ;
#20063 = CARTESIAN_POINT ( 'NONE',  ( -0.8759842519685039353, -0.1787899950787401882, 0.5241141731745827537 ) ) ;
#20064 = CARTESIAN_POINT ( 'NONE',  ( 0.7646288533564489232, 0.1113553986120547346, 1.195866141624756018 ) ) ;
#20065 = ORIENTED_EDGE ( 'NONE', *, *, #40985, .F. ) ;
#20066 = EDGE_CURVE ( 'NONE', #24265, #41049, #47153, .T. ) ;
#20067 = CARTESIAN_POINT ( 'NONE',  ( -0.8759842519685039353, -0.1787899950787401882, 1.473917322780881722 ) ) ;
#20068 = EDGE_CURVE ( 'NONE', #19535, #14831, #7133, .T. ) ;
#20069 = TOROIDAL_SURFACE ( 'NONE', #44506, 0.2047244094488188948, 0.01968503937007873988 ) ;
#20070 = CARTESIAN_POINT ( 'NONE',  ( 0.1787899950787401882, -1.481791338528913426, -2.189545951927503898E-17 ) ) ;
#20071 = FACE_OUTER_BOUND ( 'NONE', #1652, .T. ) ;
#20072 = ADVANCED_FACE ( 'NONE', ( #17440 ), #28490, .T. ) ;
#20073 = CARTESIAN_POINT ( 'NONE',  ( -0.4620708661417322616, 0.1864803149606299448, -1.186023622047243986 ) ) ;
#20074 = CARTESIAN_POINT ( 'NONE',  ( 0.1606807218793907532, -0.07955611661335547369, 0.1377952755905512694 ) ) ;
#20075 = CYLINDRICAL_SURFACE ( 'NONE', #43920, 0.1377952755905511306 ) ;
#20076 = CARTESIAN_POINT ( 'NONE',  ( -1.033464566929133799, 0.000000000000000000, 1.220472440837354400 ) ) ;
#20077 = CARTESIAN_POINT ( 'NONE',  ( 0.6971942568897626646, -0.07405724077823297447, 0.6397637794737947026 ) ) ;
#20079 = CARTESIAN_POINT ( 'NONE',  ( -0.8107537697050254399, 0.1574803149606300301, 1.626476377845228916 ) ) ;
#20078 = CARTESIAN_POINT ( 'NONE',  ( 0.1574803149606299191, -0.4409448818897637734, -1.928577636452523993E-17 ) ) ;
#20080 = VECTOR ( 'NONE', #13046, 39.37007874015748143 ) ;
#20081 = CARTESIAN_POINT ( 'NONE',  ( 0.000000000000000000, 0.1299212598425196763, 0.000000000000000000 ) ) ;
#20082 = PLANE ( 'NONE',  #32298 ) ;
#20083 = EDGE_CURVE ( 'NONE', #35490, #14813, #15098, .T. ) ;
#20084 = CARTESIAN_POINT ( 'NONE',  ( -0.8759842519685039353, -0.1787899950787401882, 1.119586614119464585 ) ) ;
#20085 = CARTESIAN_POINT ( 'NONE',  ( 0.9412147342319837628, 0.1574803149606300301, 1.080216535433071501 ) ) ;
#20087 = CARTESIAN_POINT ( 'NONE',  ( -0.7185039370078739607, 1.928577636452523993E-17, 0.2657480314960630197 ) ) ;
#20086 = DIRECTION ( 'NONE',  ( 1.000000000000000000, -3.532562060772751952E-15, 0.000000000000000000 ) ) ;
#20088 = CARTESIAN_POINT ( 'NONE',  ( 0.1235961452251413406, 0.09842519685039370636, -0.2140748031496062798 ) ) ;
#20090 = DIRECTION ( 'NONE',  ( 2.710505431213758620E-17, -0.6156614753256599570, -0.7880107536067207930 ) ) ;
#20089 = CARTESIAN_POINT ( 'NONE',  ( 0.3161444924769145626, 1.890321945096787193, -4.194630839571732217 ) ) ;
#20091 = CARTESIAN_POINT ( 'NONE',  ( 0.8759842519685039353, 0.000000000000000000, 4.498031496062992574 ) ) ;
#20092 = PRODUCT ( 'MAS-231', 'MAS-231', '', ( #37224 ) ) ;
#20093 = CARTESIAN_POINT ( 'NONE',  ( 3.284318927891251994E-17, -0.5418307086076535883, 0.1787899950787401882 ) ) ;
#20094 = VERTEX_POINT ( 'NONE', #19080 ) ;
#20095 = CARTESIAN_POINT ( 'NONE',  ( 1.033464566929134687, -0.06523048226347956391, 0.2829724409448821643 ) ) ;
#20096 = CARTESIAN_POINT ( 'NONE',  ( 0.7495606340400177148, 0.1264236179284866091, 0.8636811023084409733 ) ) ;
#20097 = VERTEX_POINT ( 'NONE', #26780 ) ;
#20098 = FACE_OUTER_BOUND ( 'NONE', #40600, .T. ) ;
#20099 = DIRECTION ( 'NONE',  ( 1.000000000000000000, 0.000000000000000000, 0.000000000000000000 ) ) ;
#20100 = CARTESIAN_POINT ( 'NONE',  ( -0.1787899950787401604, -1.695866141678520567, -0.07405724077823318263 ) ) ;
#20101 = CARTESIAN_POINT ( 'NONE',  ( -0.1787899950787401604, -0.9527559054580476694, -0.07405724077823318263 ) ) ;
#20102 = CARTESIAN_POINT ( 'NONE',  ( 2.892866454678787531E-17, -1.435039370078740273, 0.1574803149606299191 ) ) ;
#20103 = CARTESIAN_POINT ( 'NONE',  ( 0.1555213372790611448, 0.1336203177416501464, -0.04415337192905793851 ) ) ;
#20104 = ORIENTED_EDGE ( 'NONE', *, *, #31626, .F. ) ;
#20105 = VERTEX_POINT ( 'NONE', #45183 ) ;
#20106 = CARTESIAN_POINT ( 'NONE',  ( -0.9500414927467378812, 0.1787899950787401604, 1.963582677111591401 ) ) ;
#20107 = CARTESIAN_POINT ( 'NONE',  ( 1.054774247047244096, 0.000000000000000000, 1.916830708607653477 ) ) ;
#20108 = ORIENTED_EDGE ( 'NONE', *, *, #14788, .T. ) ;
#20109 = CARTESIAN_POINT ( 'NONE',  ( 1.054774247047244540, -0.07405724077823318263, 0.4970472440407249226 ) ) ;
#20110 = CARTESIAN_POINT ( 'NONE',  ( -0.8019270111902717657, -0.1787899950787401604, 1.387795275536786610 ) ) ;
#20111 = CARTESIAN_POINT ( 'NONE',  ( 0.1574803149606299746, 0.3648440108500936585, -3.619166627704266670 ) ) ;
#20112 = CARTESIAN_POINT ( 'NONE',  ( -0.7495606340400177148, 0.1264236179284866091, 0.2780511810485988278 ) ) ;
#20113 = VECTOR ( 'NONE', #45852, 39.37007874015748143 ) ;
#20114 = FACE_OUTER_BOUND ( 'NONE', #41454, .T. ) ;
#20115 = CARTESIAN_POINT ( 'NONE',  ( -1.002407869896990045, -0.1264236179284866091, 1.675688976324189117 ) ) ;
#20116 = CARTESIAN_POINT ( 'NONE',  ( -0.9500414927467378812, -0.1787899950787401604, 0.09842519679663024046 ) ) ;
#20117 = CARTESIAN_POINT ( 'NONE',  ( -0.1854001451104914655, 0.08095196624128615792, 0.1783922471788038089 ) ) ;
#20118 = CARTESIAN_POINT ( 'NONE',  ( -0.8107537697050253289, 0.1574803149606300301, 1.793799212598424342 ) ) ;
#20119 = LINE ( 'NONE', #34766, #44257 ) ;
#20120 = B_SPLINE_CURVE_WITH_KNOTS ( 'NONE', 3,
 ( #28910, #14271, #3221, #29639, #2979, #36321, #39403, #18087, #14025, #11152, #39877, #21199, #44181, #91, #32733, #24805, #10680, #14738, #39635, #6817, #7308, #25288, #21927, #29410, #47328, #17612, #14499, #29160, #28671, #43717, #7532, #33213, #43239, #10921, #40114, #25544, #40342, #10442, #36777, #14986, #36547, #35833, #21437, #3708, #43954, #22867, #34148, #45123, #25996, #37008, #4388, #33682, #15458, #41046, #8240, #4630, #27445, #19971, #8959, #5347, #20682, #34611, #46320, #35322, #9447, #12579, #9910, #1760, #16852, #42693, #24520, #35085, #17089, #2233, #2462, #38430, #9193, #17325, #45365, #31257, #13044, #38670, #13504, #27206 ),
 .UNSPECIFIED., .F., .F.,
 ( 4, 2, 2, 2, 1, 1, 2, 2, 2, 2, 1, 1, 1, 1, 2, 2, 2, 2, 2, 1, 1, 1, 2, 2, 2, 2, 2, 1, 1, 1, 1, 2, 2, 2, 2, 2, 2, 1, 2, 2, 2, 2, 1, 1, 2, 2, 2, 2, 2, 4 ),
 ( 0.000000000000000000, 0.06249999999982676357, 0.09374999999974004128, 0.1093749999996965483, 0.1171874999996747879, 0.1210937499996639910, 0.1230468749996585232, 0.1249999999996530553, 0.1874999999994784727, 0.2187499999993911814, 0.2343749999993474664, 0.2421874999993256228, 0.2460937499993147703, 0.2480468749993092747, 0.2490234374993065269, 0.2499999999993037514, 0.3124999999991173172, 0.3437499999990241140, 0.3593749999989774846, 0.3671874999989540034, 0.3710937499989422350, 0.3730468749989364619, 0.3740234374989336308, 0.3749999999989308552, 0.4374999999987470578, 0.4687499999986551869, 0.4843749999986092791, 0.4921874999985862975, 0.4960937499985745291, 0.4980468749985661470, 0.4990234374985619281, 0.4995117187485633714, 0.4999999999985648702, 0.5624999999987573274, 0.5937499999988538057, 0.6093749999989021005, 0.6171874999989263033, 0.6210937499989379607, 0.6230468749989432897, 0.6249999999989486188, 0.6874999999991322497, 0.7187499999992240651, 0.7343749999992700284, 0.7421874999992934541, 0.7460937499993046673, 0.7499999999993158806, 0.8124999999994878541, 0.8437499999995732303, 0.8749999999996586064, 1.000000000000000000 ),
 .UNSPECIFIED. ) ;
#20121 = CARTESIAN_POINT ( 'NONE',  ( 1.002407869896990045, 0.1264236179284866091, 1.685531496009228469 ) ) ;
#20122 = CARTESIAN_POINT ( 'NONE',  ( 0.1141172636152937014, -0.09842519685039370636, 0.1860162816150570941 ) ) ;
#20123 = CARTESIAN_POINT ( 'NONE',  ( -0.7185039370078760701, -0.06523048226348075740, 0.7308070865066462751 ) ) ;
#20124 = AXIS2_PLACEMENT_3D ( 'NONE', #2570, #20090, #13166 ) ;
#20125 = EDGE_CURVE ( 'NONE', #17766, #28143, #43641, .T. ) ;
#20126 = ( BOUNDED_CURVE ( )  B_SPLINE_CURVE ( 2, ( #23727, #27590, #45501, #2601, #23969, #9822, #34512, #1907, #13416 ),
 .UNSPECIFIED., .F., .T. ) 
 B_SPLINE_CURVE_WITH_KNOTS ( ( 3, 2, 2, 2, 3 ),
 ( 0.6899999999999999467, 0.6925000000000000044, 0.6949999999999999512, 0.6975000000000000089, 0.6999999999999999556 ),
 .UNSPECIFIED. ) 
 CURVE ( )  GEOMETRIC_REPRESENTATION_ITEM ( )  RATIONAL_B_SPLINE_CURVE ( ( 1.000000000000000000, 0.9238795325112939549, 1.000000000000000000, 0.9238795325112869605, 1.000000000000000000, 0.9238795325112869605, 1.000000000000000000, 0.9238795325112829637, 1.000000000000000000 ) ) 
 REPRESENTATION_ITEM ( '' )  ) ;
#20127 = EDGE_CURVE ( 'NONE', #36143, #18901, #18703, .T. ) ;
#20128 = ORIENTED_EDGE ( 'NONE', *, *, #11174, .T. ) ;
#20129 = ( BOUNDED_CURVE ( )  B_SPLINE_CURVE ( 2, ( #29877, #806, #29420, #43965, #19029, #4402, #11163, #40350, #18569 ),
 .UNSPECIFIED., .F., .F. ) 
 B_SPLINE_CURVE_WITH_KNOTS ( ( 3, 2, 2, 2, 3 ),
 ( 0.5400000000000000355, 0.5424999999999999822, 0.5450000000000000400, 0.5474999999999999867, 0.5500000000000000444 ),
 .UNSPECIFIED. ) 
 CURVE ( )  GEOMETRIC_REPRESENTATION_ITEM ( )  RATIONAL_B_SPLINE_CURVE ( ( 1.000000000000000000, 0.9238795325112869605, 1.000000000000000000, 0.9238795325112869605, 1.000000000000000000, 0.9238795325112869605, 1.000000000000000000, 0.9238795325112869605, 1.000000000000000000 ) ) 
 REPRESENTATION_ITEM ( '' )  ) ;
#20130 = AXIS2_PLACEMENT_3D ( 'NONE', #17669, #43054, #20554 ) ;
#20131 = ADVANCED_FACE ( 'NONE', ( #26062 ), #8538, .T. ) ;
#20132 = CARTESIAN_POINT ( 'NONE',  ( -1.094772975963752103E-17, -1.078248031442299304, -0.1787899950787401882 ) ) ;
#20133 = CARTESIAN_POINT ( 'NONE',  ( 0.1264236179284866091, -1.206200787347811110, 0.1264236179284866091 ) ) ;
#20134 = LINE ( 'NONE', #27604, #40856 ) ;
#20135 = CARTESIAN_POINT ( 'NONE',  ( 0.1797182628040039365, -0.5325241245436755921, -2.200913952912460540E-17 ) ) ;
#20136 = CARTESIAN_POINT ( 'NONE',  ( 0.1574803149606299191, -5.122214988120488358E-16, -8.878505979408856939E-16 ) ) ;
#20137 = CARTESIAN_POINT ( 'NONE',  ( -0.1113553986120547346, 0.006889763779527558960, -0.1113553986120547346 ) ) ;
#20138 = CARTESIAN_POINT ( 'NONE',  ( -0.1264236179284866091, -0.1678149605761578844, -0.1264236179284866091 ) ) ;
#20139 = CARTESIAN_POINT ( 'NONE',  ( 0.6971942568897626646, -0.07405724077823297447, 0.8710629920722218200 ) ) ;
#20141 = CARTESIAN_POINT ( 'NONE',  ( 0.1573498687646869010, -0.02697554138024618048, 0.1404067023994647889 ) ) ;
#20140 = CARTESIAN_POINT ( 'NONE',  ( 0.4509871776442260227, 4.466152701071653354E-17, 0.000000000000000000 ) ) ;
#20142 = CARTESIAN_POINT ( 'NONE',  ( 0.8759842519685039353, -0.1574803149606299191, 0.06889763768774861963 ) ) ;
#20143 = AXIS2_PLACEMENT_3D ( 'NONE', #3576, #11018, #4252 ) ;
#20144 = VECTOR ( 'NONE', #6451, 39.37007874015748143 ) ;
#20145 = CARTESIAN_POINT ( 'NONE',  ( -0.7108038343253642033, 0.06841996760810098444, 0.03937007874015843040 ) ) ;
#20146 = CARTESIAN_POINT ( 'NONE',  ( 0.1787899950787401604, -0.4606299212060784853, 0.07405724077823318263 ) ) ;
#20147 = DIRECTION ( 'NONE',  ( -0.000000000000000000, -0.7880107536067176843, 0.6156614753256636208 ) ) ;
#20148 = CARTESIAN_POINT ( 'NONE',  ( -0.1264236179284866091, -1.462106299158834721, -0.1264236179284866091 ) ) ;
#20149 = CARTESIAN_POINT ( 'NONE',  ( -0.8759842519685039353, -0.1787899950787401882, 1.902066929080094448 ) ) ;
#20150 = ORIENTED_EDGE ( 'NONE', *, *, #22835, .F. ) ;
#20151 = CARTESIAN_POINT ( 'NONE',  ( -0.6971942568897637749, 2.189545951927499583E-17, 1.503444881836000002 ) ) ;
#20152 = LINE ( 'NONE', #15878, #6946 ) ;
#20153 = CARTESIAN_POINT ( 'NONE',  ( 1.002407869896990045, -0.1264236179284866091, 1.439468503883244210 ) ) ;
#20154 = CARTESIAN_POINT ( 'NONE',  ( 0.4620708661417356478, 0.9842519685039370358, -0.7135826771653542844 ) ) ;
#20155 = CARTESIAN_POINT ( 'NONE',  ( -0.8019270111902717657, 0.1787899950787401604, 0.5118110235682844511 ) ) ;
#20156 = CARTESIAN_POINT ( 'NONE',  ( -1.054774247047244540, 0.07405724077823318263, 1.205708661363558365 ) ) ;
#20157 = CARTESIAN_POINT ( 'NONE',  ( 0.1159354540250667615, -0.09844533245960994383, -0.1362465444070161402 ) ) ;
#20158 = CARTESIAN_POINT ( 'NONE',  ( 0.6971942568897648851, 0.07405724077823318263, 0.6742125983714336579 ) ) ;
#20159 = CARTESIAN_POINT ( 'NONE',  ( -1.054774247047244540, -0.07405724077823318263, 0.4921259841982049132 ) ) ;
#20160 = DIRECTION ( 'NONE',  ( 1.000000000000000000, 0.000000000000000000, -1.822029033848725275E-16 ) ) ;
#20161 = ORIENTED_EDGE ( 'NONE', *, *, #30773, .T. ) ;
#20162 = CARTESIAN_POINT ( 'NONE',  ( -0.8107537697050253289, 0.1574803149606300301, 0.3764763779527559029 ) ) ;
#20163 = CARTESIAN_POINT ( 'NONE',  ( 0.6971942568897648851, -0.07405724077823297447, 1.348425196796630976 ) ) ;
#20164 = CARTESIAN_POINT ( 'NONE',  ( -0.2423783858011515635, -0.09851385377439449142, -0.009343542218490177159 ) ) ;
#20165 = ORIENTED_EDGE ( 'NONE', *, *, #19041, .F. ) ;
#20166 = ADVANCED_FACE ( 'NONE', ( #399 ), #3104, .T. ) ;
#20167 = CARTESIAN_POINT ( 'NONE',  ( -0.1377952755905509363, 1.687505431895957030E-17, -0.1045766232635885612 ) ) ;
#20168 = CARTESIAN_POINT ( 'NONE',  ( -0.9500414927467378812, 0.1787899950787401604, 0.9399606298674970661 ) ) ;
#20169 = EDGE_CURVE ( 'NONE', #12054, #25373, #1341, .T. ) ;
#20170 = CARTESIAN_POINT ( 'NONE',  ( -1.002407869896990045, 0.1264236179284866091, 0.1845472440407248116 ) ) ;
#20171 = CARTESIAN_POINT ( 'NONE',  ( 3.284318927891251994E-17, -1.541954676890655573, 0.1787899950787401882 ) ) ;
#20172 = ORIENTED_EDGE ( 'NONE', *, *, #42303, .F. ) ;
#20173 = CARTESIAN_POINT ( 'NONE',  ( 0.1574803149606299746, 0.6241017553149654784, 0.3240160679609099259 ) ) ;
#20174 = CARTESIAN_POINT ( 'NONE',  ( -1.094772975963752103E-17, -0.6402559054580471143, -0.1787899950787401882 ) ) ;
#20175 = EDGE_CURVE ( 'NONE', #19533, #35669, #46280, .T. ) ;
#20176 = CARTESIAN_POINT ( 'NONE',  ( -0.2665235116888309275, -0.1584712422872024407, 0.8211962908093238811 ) ) ;
#20177 = EDGE_LOOP ( 'NONE', ( #30591, #47424, #1478, #4063 ) ) ;
#20178 = CARTESIAN_POINT ( 'NONE',  ( 1.054774247047244096, 0.000000000000000000, 1.360728346402929168 ) ) ;
#20179 = EDGE_CURVE ( 'NONE', #110, #25251, #23622, .T. ) ;
#20180 = CARTESIAN_POINT ( 'NONE',  ( 1.033464566929134687, 0.06523048226347956391, 0.8784448818897643285 ) ) ;
#20181 = DIRECTION ( 'NONE',  ( 0.000000000000000000, 0.000000000000000000, -1.000000000000000000 ) ) ;
#20182 = CARTESIAN_POINT ( 'NONE',  ( -0.1264236179284866091, -0.8223425196312754704, 0.1264236179284866091 ) ) ;
#20183 = DIRECTION ( 'NONE',  ( -1.000000000000000000, 0.000000000000000000, 0.000000000000000000 ) ) ;
#20184 = CARTESIAN_POINT ( 'NONE',  ( 1.002407869896990045, -0.1264236179284866091, 1.631397637741511808 ) ) ;
#20185 = CARTESIAN_POINT ( 'NONE',  ( -0.1787899950787401882, -0.05573420444971117355, 0.000000000000000000 ) ) ;
#20186 = SHAPE_DEFINITION_REPRESENTATION ( #30063, #14237 ) ;
#20187 = CARTESIAN_POINT ( 'NONE',  ( -0.7646288533564489232, 0.1113553986120547346, 1.747047243986960652 ) ) ;
#20188 = CARTESIAN_POINT ( 'NONE',  ( -0.6971942568897648851, 0.07405724077823318263, 0.8710629920722218200 ) ) ;
#20190 = CARTESIAN_POINT ( 'NONE',  ( 1.033464566929133799, 0.000000000000000000, 0.07874015737278799998 ) ) ;
#20189 = CARTESIAN_POINT ( 'NONE',  ( -0.1113553986120547346, -0.9379921259842519676, -0.1113553986120547346 ) ) ;
#20192 = CARTESIAN_POINT ( 'NONE',  ( -0.7749013318191750876, -0.1380202477924483417, 1.986195989362255832 ) ) ;
#20191 = CARTESIAN_POINT ( 'NONE',  ( -1.100456976456230270E-17, -1.506933573362572831, -0.1797182628040039365 ) ) ;
#20193 = CARTESIAN_POINT ( 'NONE',  ( 0.1264236179284866091, -0.3302165353793074520, -0.1264236179284866091 ) ) ;
#20194 = CARTESIAN_POINT ( 'NONE',  ( -0.9873396505805591694, 0.1113553986120547346, 1.028543306979086802 ) ) ;
#20195 = CARTESIAN_POINT ( 'NONE',  ( 0.8019270111902717657, -0.1787899950787401604, 1.550196850339937926 ) ) ;
#20196 = CARTESIAN_POINT ( 'NONE',  ( 0.8759842519685039353, -0.1787899950787401882, 1.902066929080094448 ) ) ;
#20197 = CARTESIAN_POINT ( 'NONE',  ( 1.054774247047244540, 0.07405724077823318263, 0.4183070865604096578 ) ) ;
#20198 = CARTESIAN_POINT ( 'NONE',  ( -0.7646288533564489232, -0.1113553986120547346, 0.1427165353255439029 ) ) ;
#20199 = DIRECTION ( 'NONE',  ( 1.000000000000000000, 0.000000000000000000, -1.822029033848725275E-16 ) ) ;
#20200 = CARTESIAN_POINT ( 'NONE',  ( -1.284448818897637956, -0.3937007874015748254, -1.181102362204724310 ) ) ;
#20201 = CARTESIAN_POINT ( 'NONE',  ( 0.1264236179284866091, 0.009350393754550925460, 0.1264236179284866091 ) ) ;
#20202 = FACE_OUTER_BOUND ( 'NONE', #41434, .T. ) ;
#20203 = CARTESIAN_POINT ( 'NONE',  ( 1.002407869896990045, -0.1264236179284866091, 0.4502952755367874427 ) ) ;
#20204 = CARTESIAN_POINT ( 'NONE',  ( -1.033464566929133799, 0.000000000000000000, 0.2755905510735752184 ) ) ;
#20206 = CARTESIAN_POINT ( 'NONE',  ( 0.1574803149606299746, 0.3740157480314960647, 1.713085361781126803 ) ) ;
#20205 = CARTESIAN_POINT ( 'NONE',  ( 0.8759842519685039353, -0.1787899950787401882, 1.311515747977732405 ) ) ;
#20207 = CARTESIAN_POINT ( 'NONE',  ( 0.9873396505805591694, 0.1113553986120547346, 0.2116141732283464416 ) ) ;
#20208 = CARTESIAN_POINT ( 'NONE',  ( 1.033464566929134687, 0.06523048226347956391, 0.8686023620971983217 ) ) ;
#20209 = ORIENTED_EDGE ( 'NONE', *, *, #11817, .F. ) ;
#20210 = CARTESIAN_POINT ( 'NONE',  ( -0.6971942568897637749, 2.189545951927499583E-17, 1.070374015694267600 ) ) ;
#20211 = LINE ( 'NONE', #34861, #22235 ) ;
#20212 = CARTESIAN_POINT ( 'NONE',  ( 0.8759842519685039353, -0.1787899950787401882, 0.9621062991588346103 ) ) ;
#20213 = ORIENTED_EDGE ( 'NONE', *, *, #20610, .F. ) ;
#20215 = CARTESIAN_POINT ( 'NONE',  ( 0.1787899950787401604, -1.400590551127339323, -0.07405724077823318263 ) ) ;
#20214 = CARTESIAN_POINT ( 'NONE',  ( -0.06523048226347956391, -1.112696850286173600, 0.1574803149606297803 ) ) ;
#20216 = CARTESIAN_POINT ( 'NONE',  ( -0.7185039370078746268, -0.06523048226347956391, 0.5339566928058587791 ) ) ;
#20217 = CARTESIAN_POINT ( 'NONE',  ( -0.7185039370078739607, 1.928577636452523993E-17, 1.368110236220472675 ) ) ;
#20218 = CARTESIAN_POINT ( 'NONE',  ( 0.7185039370078766252, -0.06523048226348168721, 1.793799212490897688 ) ) ;
#20220 = CARTESIAN_POINT ( 'NONE',  ( -0.8759842519685039353, -0.1574803149606299191, 0.4330708661417322913 ) ) ;
#20219 = CARTESIAN_POINT ( 'NONE',  ( 0.000000000000000000, 0.09842519685039370636, 0.000000000000000000 ) ) ;
#20221 = CARTESIAN_POINT ( 'NONE',  ( 0.8759842519685039353, 0.1787899950787401882, 0.1943897637257641919 ) ) ;
#20222 = CARTESIAN_POINT ( 'NONE',  ( -0.7495606340400177148, 0.1264236179284866091, 0.1156496062454492185 ) ) ;
#20223 = CARTESIAN_POINT ( 'NONE',  ( 0.8107537697050253289, -0.1574803149606297803, 1.365649606191684295 ) ) ;
#20224 = ORIENTED_EDGE ( 'NONE', *, *, #12295, .T. ) ;
#20225 = ORIENTED_EDGE ( 'NONE', *, *, #35400, .F. ) ;
#20226 = FACE_OUTER_BOUND ( 'NONE', #32748, .T. ) ;
#20227 = CARTESIAN_POINT ( 'NONE',  ( -0.09431337879932527590, -0.09445537554013608283, -0.2309807168375144215 ) ) ;
#20228 = VERTEX_POINT ( 'NONE', #30396 ) ;
#20229 = CARTESIAN_POINT ( 'NONE',  ( 1.054774247047244096, 0.000000000000000000, 0.9719488188438739629 ) ) ;
#20230 = CARTESIAN_POINT ( 'NONE',  ( -1.054774247047244540, -0.07405724077823318263, 1.712598425143087466 ) ) ;
#20231 = CARTESIAN_POINT ( 'NONE',  ( -0.1113553986120547346, -0.2490157479239688831, 0.1113553986120547346 ) ) ;
#20232 = ( BOUNDED_CURVE ( )  B_SPLINE_CURVE ( 2, ( #45234, #1874, #34255, #12926, #41626, #5936, #16511, #1387, #39001 ),
 .UNSPECIFIED., .F., .F. ) 
 B_SPLINE_CURVE_WITH_KNOTS ( ( 3, 2, 2, 2, 3 ),
 ( 0.2700000000000000178, 0.2725000000000000200, 0.2750000000000000222, 0.2775000000000000244, 0.2800000000000000266 ),
 .UNSPECIFIED. ) 
 CURVE ( )  GEOMETRIC_REPRESENTATION_ITEM ( )  RATIONAL_B_SPLINE_CURVE ( ( 1.000000000000000000, 0.9238795325112869605, 1.000000000000000000, 0.9238795325112869605, 1.000000000000000000, 0.9238795325112869605, 1.000000000000000000, 0.9238795325112879597, 1.000000000000000000 ) ) 
 REPRESENTATION_ITEM ( '' )  ) ;
#20233 = EDGE_CURVE ( 'NONE', #18241, #34008, #38728, .T. ) ;
#20234 = CARTESIAN_POINT ( 'NONE',  ( -0.1968503937007874127, -0.5192708129487058066, -0.8938220056861535534 ) ) ;
#20235 = DIRECTION ( 'NONE',  ( 3.469446951953613794E-15, 1.000000000000000000, 0.000000000000000000 ) ) ;
#20236 = DIRECTION ( 'NONE',  ( 0.000000000000000000, 0.6156614753256575145, 0.7880107536067225693 ) ) ;
#20237 = CARTESIAN_POINT ( 'NONE',  ( 0.1787899950787401882, -1.099041291063883818, -2.189545951927503898E-17 ) ) ;
#20238 = ORIENTED_EDGE ( 'NONE', *, *, #47358, .F. ) ;
#20239 = CARTESIAN_POINT ( 'NONE',  ( -0.1787899950787401604, -0.1210629920722208208, -0.07405724077823318263 ) ) ;
#20240 = ORIENTED_EDGE ( 'NONE', *, *, #30605, .F. ) ;
#20241 = EDGE_CURVE ( 'NONE', #1697, #12053, #28257, .T. ) ;
#20242 = ORIENTED_EDGE ( 'NONE', *, *, #44884, .F. ) ;
#20243 = VECTOR ( 'NONE', #8961, 39.37007874015748854 ) ;
#20244 = EDGE_CURVE ( 'NONE', #529, #46399, #25336, .T. ) ;
#20245 = LINE ( 'NONE', #38706, #47029 ) ;
#20246 = CARTESIAN_POINT ( 'NONE',  ( 0.2395294000716133853, -0.1968503937007874127, -0.4921259842519685179 ) ) ;
#20247 = CARTESIAN_POINT ( 'NONE',  ( 1.033464566929133799, 0.000000000000000000, 1.899606299212598604 ) ) ;
#20248 = VECTOR ( 'NONE', #44218, 39.37007874015748143 ) ;
#20249 = AXIS2_PLACEMENT_3D ( 'NONE', #31303, #39161, #2733 ) ;
#20250 = CARTESIAN_POINT ( 'NONE',  ( -0.1264236179284866091, -0.6008858267178898149, -0.1264236179284866091 ) ) ;
#20251 = ( BOUNDED_CURVE ( )  B_SPLINE_CURVE ( 2, ( #3545, #43784, #7376, #33033, #36389, #14093, #158, #25828, #28740 ),
 .UNSPECIFIED., .F., .T. ) 
 B_SPLINE_CURVE_WITH_KNOTS ( ( 3, 2, 2, 2, 3 ),
 ( 0.5799999999999999600, 0.5825000000000000178, 0.5849999999999999645, 0.5875000000000000222, 0.5899999999999999689 ),
 .UNSPECIFIED. ) 
 CURVE ( )  GEOMETRIC_REPRESENTATION_ITEM ( )  RATIONAL_B_SPLINE_CURVE ( ( 1.000000000000000000, 0.9238795325112869605, 1.000000000000000000, 0.9238795325112869605, 1.000000000000000000, 0.9238795325112869605, 1.000000000000000000, 0.9238795325112869605, 1.000000000000000000 ) ) 
 REPRESENTATION_ITEM ( '' )  ) ;
#20252 = CARTESIAN_POINT ( 'NONE',  ( -0.7495606340400177148, 0.1264236179284866091, 0.3174212597887562382 ) ) ;
#20253 = CARTESIAN_POINT ( 'NONE',  ( 0.07444174185955065859, -1.130457195409817039, 0.1797182628040039087 ) ) ;
#20254 = CARTESIAN_POINT ( 'NONE',  ( -0.1997612633124555837, 0.1801620131153011950, -0.05546260682012547211 ) ) ;
#20255 = CARTESIAN_POINT ( 'NONE',  ( 1.054774247047244096, 0.000000000000000000, 1.050688976324189117 ) ) ;
#20256 = CARTESIAN_POINT ( 'NONE',  ( -0.8759842519685039353, 0.1574803149606299191, 0.6397637794200314865 ) ) ;
#20257 = EDGE_CURVE ( 'NONE', #31526, #22319, #3902, .T. ) ;
#20258 = CARTESIAN_POINT ( 'NONE',  ( 1.033464566929134687, 0.06523048226347956391, 1.508366141732284449 ) ) ;
#20260 = DIRECTION ( 'NONE',  ( -3.580839449783114748E-16, 0.6156614753256610673, 0.7880107536067199048 ) ) ;
#20259 = CARTESIAN_POINT ( 'NONE',  ( 0.5057057357416000487, 0.09842519685039370636, 0.000000000000000000 ) ) ;
#20261 = CARTESIAN_POINT ( 'NONE',  ( 1.033464566929133799, 0.000000000000000000, 0.4724409447743622148 ) ) ;
#20262 = CARTESIAN_POINT ( 'NONE',  ( -0.9873396505805591694, -0.1113553986120547346, 1.648622047136566904 ) ) ;
#20263 = DIRECTION ( 'NONE',  ( -0.000000000000000000, 1.000000000000000000, -0.000000000000000000 ) ) ;
#20264 = CARTESIAN_POINT ( 'NONE',  ( 1.054774247047244540, 0.07405724077823318263, 1.008858267662772423 ) ) ;
#20265 = CARTESIAN_POINT ( 'NONE',  ( 1.033464566929133799, 0.000000000000000000, 0.2755905510735752184 ) ) ;
#20266 = ORIENTED_EDGE ( 'NONE', *, *, #17805, .F. ) ;
#20267 = DIRECTION ( 'NONE',  ( 0.000000000000000000, 1.000000000000000000, 0.000000000000000000 ) ) ;
#20268 = CARTESIAN_POINT ( 'NONE',  ( 1.004041291822608928, 0.1039877302390117553, 0.03936817812369314967 ) ) ;
#20269 = CARTESIAN_POINT ( 'NONE',  ( 0.1574803149606299191, -1.690944881782236120, -1.928577636452523993E-17 ) ) ;
#20270 = CARTESIAN_POINT ( 'NONE',  ( -0.7185039370078746268, -0.06523048226347956391, 0.2977362203649139283 ) ) ;
#20271 = CARTESIAN_POINT ( 'NONE',  ( 0.1781957201322358353, -0.09842519685039370636, -0.01456528979491370120 ) ) ;
#20272 = CARTESIAN_POINT ( 'NONE',  ( 1.054774247047244096, 0.000000000000000000, 1.242618110182456714 ) ) ;
#20273 = CARTESIAN_POINT ( 'NONE',  ( 0.1235961452251413406, -0.09842519685039370636, 0.2140748031496062798 ) ) ;
#20274 = CARTESIAN_POINT ( 'NONE',  ( 0.07405724077823318263, 0.06594488194352733645, -0.1787899950787401604 ) ) ;
#20275 = DIRECTION ( 'NONE',  ( 0.000000000000000000, 0.000000000000000000, 1.000000000000000000 ) ) ;
#20276 = CARTESIAN_POINT ( 'NONE',  ( -0.6971942568897626646, -0.07405724077823297447, 0.6348425196312760255 ) ) ;
#20277 = CIRCLE ( 'NONE', #15039, 0.1377952755905509363 ) ;
#20279 = CARTESIAN_POINT ( 'NONE',  ( 1.033464566929133799, 0.000000000000000000, 1.377952755797984263 ) ) ;
#20278 = VECTOR ( 'NONE', #4069, 39.37007874015748143 ) ;
#20280 = CARTESIAN_POINT ( 'NONE',  ( -0.6195511811023656223, 1.354170115732555191, -0.4197102375732078561 ) ) ;
#20281 = CARTESIAN_POINT ( 'NONE',  ( 3.284318927891251994E-17, -1.688484251914740275, 0.1787899950787401882 ) ) ;
#20282 = CARTESIAN_POINT ( 'NONE',  ( -0.9500414927467378812, 0.1787899950787401604, 0.9793307086076531442 ) ) ;
#20283 = VECTOR ( 'NONE', #4966, 39.37007874015748143 ) ;
#20284 = AXIS2_PLACEMENT_3D ( 'NONE', #42427, #42194, #31690 ) ;
#20285 = CARTESIAN_POINT ( 'NONE',  ( -1.033464566929133799, 0.000000000000000000, 0.04921259842519685318 ) ) ;
#20286 = CARTESIAN_POINT ( 'NONE',  ( -0.7495606340400177148, -0.1264236179284866091, 0.9916338582139527791 ) ) ;
#20287 = CARTESIAN_POINT ( 'NONE',  ( -1.054774247047244540, 0.07405724077823318263, 0.6988188975840318173 ) ) ;
#20288 = ORIENTED_EDGE ( 'NONE', *, *, #21305, .F. ) ;
#20289 = ADVANCED_FACE ( 'NONE', ( #31557 ), #35145, .T. ) ;
#20290 = CARTESIAN_POINT ( 'NONE',  ( 2.892866454678787531E-17, -0.04724409438066189126, 0.1574803149606299191 ) ) ;
#20291 = CARTESIAN_POINT ( 'NONE',  ( -0.7646288533564489232, 0.1113553986120547346, 0.09350393690034704275 ) ) ;
#20292 = CARTESIAN_POINT ( 'NONE',  ( 0.1787899950787401882, -0.6659704249221517491, -2.189545951927503898E-17 ) ) ;
#20293 = VERTEX_POINT ( 'NONE', #16228 ) ;
#20294 = CARTESIAN_POINT ( 'NONE',  ( 0.08074247269275255934, -0.08956073568337362401, -0.1736237762710417243 ) ) ;
#20295 = DIRECTION ( 'NONE',  ( -1.000000000000000000, 0.000000000000000000, 0.000000000000000000 ) ) ;
#20296 = ORIENTED_EDGE ( 'NONE', *, *, #32657, .T. ) ;
#20297 = DIRECTION ( 'NONE',  ( 0.000000000000000000, -1.000000000000000000, -0.000000000000000000 ) ) ;
#20298 = EDGE_CURVE ( 'NONE', #31809, #26252, #19969, .T. ) ;
#20299 = DIRECTION ( 'NONE',  ( -1.000000000000000000, 0.000000000000000000, 0.000000000000000000 ) ) ;
#20300 = CARTESIAN_POINT ( 'NONE',  ( -0.8759842519685039353, 0.1787899950787401882, 0.5437992125446614589 ) ) ;
#20301 = CARTESIAN_POINT ( 'NONE',  ( 0.000000000000000000, 0.000000000000000000, 0.000000000000000000 ) ) ;
#20302 = VERTEX_POINT ( 'NONE', #13111 ) ;
#20303 = CARTESIAN_POINT ( 'NONE',  ( -0.9500414927467377701, 0.1787899950787401604, 1.648622047190331230 ) ) ;
#20304 = VECTOR ( 'NONE', #45003, 39.37007874015748143 ) ;
#20305 = CARTESIAN_POINT ( 'NONE',  ( -0.1787899950787401882, -1.540846456639149542, 0.000000000000000000 ) ) ;
#20306 = CARTESIAN_POINT ( 'NONE',  ( -9.642888182262618425E-18, 0.09055118120988918384, -0.1574803149606299191 ) ) ;
#20307 = CARTESIAN_POINT ( 'NONE',  ( 0.000000000000000000, 0.000000000000000000, -0.3149606299212598381 ) ) ;
#20308 = VERTEX_POINT ( 'NONE', #42531 ) ;
#20309 = CARTESIAN_POINT ( 'NONE',  ( 0.9412147342319837628, 0.1574803149606300301, 0.5684055118110235005 ) ) ;
#20310 = CARTESIAN_POINT ( 'NONE',  ( 0.1270800023317771588, -0.7244532584019429677, -0.1270800023317771588 ) ) ;
#20311 = VECTOR ( 'NONE', #5509, 39.37007874015748854 ) ;
#20312 = CYLINDRICAL_SURFACE ( 'NONE', #12589, 0.1574803149606299191 ) ;
#20313 = CARTESIAN_POINT ( 'NONE',  ( -0.7185039370078746268, -0.06523048226347956391, 1.203248031388535200 ) ) ;
#20314 = CARTESIAN_POINT ( 'NONE',  ( 0.6971942568897626646, 0.07405724077823318263, 0.6348425196312760255 ) ) ;
#20316 = DIRECTION ( 'NONE',  ( 0.000000000000000000, 0.000000000000000000, 1.000000000000000000 ) ) ;
#20315 = CARTESIAN_POINT ( 'NONE',  ( 0.1113553986120547346, -0.4753937007874016185, -0.1113553986120547346 ) ) ;
#20317 = AXIS2_PLACEMENT_3D ( 'NONE', #639, #23193, #37807 ) ;
#20318 = CARTESIAN_POINT ( 'NONE',  ( -1.033464566929133799, 0.000000000000000000, 0.4035433070866141780 ) ) ;
#20319 = EDGE_LOOP ( 'NONE', ( #38849, #4584, #38629, #36018 ) ) ;
#20320 = DIRECTION ( 'NONE',  ( 1.000000000000000000, 0.000000000000000000, -0.000000000000000000 ) ) ;
#20321 = CARTESIAN_POINT ( 'NONE',  ( 0.9873396505805591694, -0.1113553986120547346, 1.067913385826771755 ) ) ;
#20323 = CARTESIAN_POINT ( 'NONE',  ( 0.2944196465027555387, 4.766607801171850497E-17, 0.000000000000000000 ) ) ;
#20322 = CARTESIAN_POINT ( 'NONE',  ( -1.033464566929134687, 0.06523048226347956391, 1.262303149498772425 ) ) ;
#20324 = CARTESIAN_POINT ( 'NONE',  ( 0.1184675242425320824, -0.5708661417322835607, 1.713085361781127913 ) ) ;
#20325 = EDGE_CURVE ( 'NONE', #43060, #8144, #33776, .T. ) ;
#20327 = CARTESIAN_POINT ( 'NONE',  ( -1.033464566929133799, 0.000000000000000000, 1.968503936900346529 ) ) ;
#20326 = FACE_OUTER_BOUND ( 'NONE', #16756, .T. ) ;
#20328 = LINE ( 'NONE', #5227, #30082 ) ;
#20329 = CARTESIAN_POINT ( 'NONE',  ( -0.1549096836786406084, -0.08956169654156308224, -0.08259319978823646824 ) ) ;
#20330 = CARTESIAN_POINT ( 'NONE',  ( -0.1264236179284866091, -0.4680118109698582773, 0.1264236179284866091 ) ) ;
#20331 = DIRECTION ( 'NONE',  ( -0.000000000000000000, -0.000000000000000000, -1.000000000000000000 ) ) ;
#20332 = CARTESIAN_POINT ( 'NONE',  ( -0.7185039370078739607, 1.928577636452523993E-17, 1.053149606299212504 ) ) ;
#20333 = CARTESIAN_POINT ( 'NONE',  ( 0.9873396505805591694, 0.1113553986120547346, 1.156496062992125928 ) ) ;
#20334 = CARTESIAN_POINT ( 'NONE',  ( 1.054774247047244540, -0.07405724077823318263, 0.7677165353793073965 ) ) ;
#20335 = ORIENTED_EDGE ( 'NONE', *, *, #42444, .F. ) ;
#20336 = CARTESIAN_POINT ( 'NONE',  ( 0.8759842519685039353, -0.1574803149606299191, 1.456692913385826849 ) ) ;
#20337 = CYLINDRICAL_SURFACE ( 'NONE', #25057, 0.09842519685039370636 ) ;
#20338 = CARTESIAN_POINT ( 'NONE',  ( 0.1787899950787401604, -1.754921259788755128, 0.07405724077823318263 ) ) ;
#20339 = CARTESIAN_POINT ( 'NONE',  ( -0.07405724077823318263, -0.9970472440407247561, -0.1787899950787401604 ) ) ;
#20340 = CARTESIAN_POINT ( 'NONE',  ( -0.1113553986120547346, -1.410433070866141891, -0.1113553986120547346 ) ) ;
#20341 = CARTESIAN_POINT ( 'NONE',  ( 1.033464566929134687, 0.06523048226347956391, 1.222933070758614127 ) ) ;
#20342 = CARTESIAN_POINT ( 'NONE',  ( 1.033464566929134687, -0.06523048226347956391, 1.178641732175937040 ) ) ;
#20343 = ORIENTED_EDGE ( 'NONE', *, *, #9816, .F. ) ;
#20344 = VERTEX_POINT ( 'NONE', #9733 ) ;
#20345 = CARTESIAN_POINT ( 'NONE',  ( -1.054774247047244540, -0.07405724077823318263, 1.953740157426552715 ) ) ;
#20346 = VERTEX_POINT ( 'NONE', #5178 ) ;
#20347 = CARTESIAN_POINT ( 'NONE',  ( -0.1574803149606300301, -1.358759842412158081, -0.06523048226347956391 ) ) ;
#20348 = CARTESIAN_POINT ( 'NONE',  ( 2.892866454678787531E-17, -0.007874015640504449659, 0.1574803149606299191 ) ) ;
#20349 = CARTESIAN_POINT ( 'NONE',  ( -0.6971942568897637749, 2.189545951927499583E-17, 1.459153543253322693 ) ) ;
#20350 = AXIS2_PLACEMENT_3D ( 'NONE', #23421, #16461, #6117 ) ;
#20351 = EDGE_CURVE ( 'NONE', #13348, #32806, #16176, .T. ) ;
#20352 = EDGE_CURVE ( 'NONE', #9934, #21151, #24350, .T. ) ;
#20353 = CARTESIAN_POINT ( 'NONE',  ( -1.054774247047244540, -0.07405724077823318263, 0.3001968503399373711 ) ) ;
#20354 = EDGE_CURVE ( 'NONE', #37817, #4137, #1600, .T. ) ;
#20355 = CARTESIAN_POINT ( 'NONE',  ( 0.7646288533564489232, -0.1113553986120547346, 1.569881889763779625 ) ) ;
#20356 = CARTESIAN_POINT ( 'NONE',  ( -0.8019270111902717657, -0.1787899950787401604, 1.668307086560410157 ) ) ;
#20357 = CARTESIAN_POINT ( 'NONE',  ( -1.033464566929134687, -0.06523048226347956391, 1.818405511811023167 ) ) ;
#20358 = FACE_OUTER_BOUND ( 'NONE', #37718, .T. ) ;
#20359 = CARTESIAN_POINT ( 'NONE',  ( 0.6971942568897648851, 0.07405724077823318263, 1.737204724355685626 ) ) ;
#20360 = CARTESIAN_POINT ( 'NONE',  ( 0.1101299531113933000, -0.09842519685039370636, -0.1631579918895759984 ) ) ;
#20361 = DIRECTION ( 'NONE',  ( 0.000000000000000000, -1.000000000000000000, -0.000000000000000000 ) ) ;
#20362 = CIRCLE ( 'NONE', #3530, 0.1567662409572586624 ) ;
#20363 = EDGE_CURVE ( 'NONE', #22586, #38634, #23639, .T. ) ;
#20364 = DIMENSIONAL_EXPONENTS ( 1.000000000000000000, 0.000000000000000000, 0.000000000000000000, 0.000000000000000000, 0.000000000000000000, 0.000000000000000000, 0.000000000000000000 ) ;
#20365 = ORIENTED_EDGE ( 'NONE', *, *, #38804, .T. ) ;
#20366 = CARTESIAN_POINT ( 'NONE',  ( -0.8759842519685039353, 0.1787899950787401882, 1.218011810969858111 ) ) ;
#20367 = CARTESIAN_POINT ( 'NONE',  ( 3.284318927891251994E-17, -1.211122047190330786, 0.1787899950787401882 ) ) ;
#20368 = CARTESIAN_POINT ( 'NONE',  ( -0.07444174185955065859, -0.5202209749373758463, -0.1797182628040039087 ) ) ;
#20369 = CARTESIAN_POINT ( 'NONE',  ( -1.033464566929134687, -0.06523048226347956391, 0.8243110235145187925 ) ) ;
#20370 = CARTESIAN_POINT ( 'NONE',  ( -0.9873396505805591694, -0.1113553986120547346, 0.7135826771653542844 ) ) ;
#20371 = CARTESIAN_POINT ( 'NONE',  ( 0.1574803149606299191, -0.04724409448818897572, -1.928577636452523993E-17 ) ) ;
#20372 = CARTESIAN_POINT ( 'NONE',  ( 0.8019270111902717657, -0.1787899950787401604, 0.9547244093950547628 ) ) ;
#20374 = CARTESIAN_POINT ( 'NONE',  ( 0.004734662961524557616, 0.09521559318215297441, 0.1106847963720228034 ) ) ;
#20373 = FACE_OUTER_BOUND ( 'NONE', #25478, .T. ) ;
#20375 = CARTESIAN_POINT ( 'NONE',  ( 0.8759842519685039353, -0.1574803149606299191, 1.092519684931842594 ) ) ;
#20376 = CARTESIAN_POINT ( 'NONE',  ( 0.7185039370078746268, 0.06523048226347956391, 0.09596456682160688090 ) ) ;
#20377 = CARTESIAN_POINT ( 'NONE',  ( -0.7185039370078739607, 1.928577636452523993E-17, 1.171259842519684957 ) ) ;
#20379 = CARTESIAN_POINT ( 'NONE',  ( 0.1264236179284866091, -0.5713582676627716461, -0.1264236179284866091 ) ) ;
#20378 = CARTESIAN_POINT ( 'NONE',  ( 0.1574803149606300301, -0.9798228345381415627, -0.06523048226347956391 ) ) ;
#20380 = CARTESIAN_POINT ( 'NONE',  ( -0.07405724077823318263, -1.346456692859623550, -0.1787899950787401604 ) ) ;
#20381 = CARTESIAN_POINT ( 'NONE',  ( 0.6141732283464567121, 0.000000000000000000, 0.000000000000000000 ) ) ;
#20382 = CARTESIAN_POINT ( 'NONE',  ( -0.8759842519685039353, 0.1787899950787401882, 1.882381889710015743 ) ) ;
#20383 = EDGE_LOOP ( 'NONE', ( #33878, #42123, #24288, #17923 ) ) ;
#20384 = ORIENTED_EDGE ( 'NONE', *, *, #6553, .F. ) ;
#20385 = CARTESIAN_POINT ( 'NONE',  ( -1.002407869896990045, -0.1264236179284866091, 1.439468503883244210 ) ) ;
#20386 = EDGE_CURVE ( 'NONE', #15821, #37845, #35293, .T. ) ;
#20387 = CARTESIAN_POINT ( 'NONE',  ( 0.8019270111902717657, 0.1787899950787401604, 1.377952755851748146 ) ) ;
#20388 = CARTESIAN_POINT ( 'NONE',  ( -0.1574803149606299191, -0.9875035750853327077, -1.463737590216208861 ) ) ;
#20389 = CARTESIAN_POINT ( 'NONE',  ( -0.7495606340400177148, 0.1264236179284866091, 0.7111220471903307860 ) ) ;
#20390 = CARTESIAN_POINT ( 'NONE',  ( 0.6971942568897637749, 2.189545951927499583E-17, 0.08612204719033110523 ) ) ;
#20391 = CARTESIAN_POINT ( 'NONE',  ( -0.8759842519685039353, 0.1787899950787401882, 1.291830708607653477 ) ) ;
#20392 = FACE_OUTER_BOUND ( 'NONE', #7039, .T. ) ;
#20393 = CARTESIAN_POINT ( 'NONE',  ( -0.5555748031496036132, 0.9100161909011723615, 0.01858545845903165558 ) ) ;
#20394 = CARTESIAN_POINT ( 'NONE',  ( 0.7495606340400177148, 0.1264236179284866091, 0.6717519684501732646 ) ) ;
#20395 = CARTESIAN_POINT ( 'NONE',  ( -0.8759842519685039353, 0.1787899950787401882, 0.5044291338045039375 ) ) ;
#20396 = CARTESIAN_POINT ( 'NONE',  ( 0.1945459183828945893, -0.07553294269967773811, 0.1731116344631672688 ) ) ;
#20397 = EDGE_CURVE ( 'NONE', #8724, #21404, #16905, .T. ) ;
#20398 = CARTESIAN_POINT ( 'NONE',  ( 0.000000000000000000, 0.000000000000000000, 2.731847993664263218E-16 ) ) ;
#20399 = EDGE_LOOP ( 'NONE', ( #39552, #15807, #39505, #2074 ) ) ;
#20400 = CARTESIAN_POINT ( 'NONE',  ( 0.1377952755905510751, 0.000000000000000000, -0.3149606299212598381 ) ) ;
#20401 = CARTESIAN_POINT ( 'NONE',  ( -0.7646288533564489232, 0.1113553986120547346, 0.2608267716535432879 ) ) ;
#20402 = CARTESIAN_POINT ( 'NONE',  ( 0.8019270111902716547, -0.1787899950787401604, 1.353346456639149986 ) ) ;
#20403 = CARTESIAN_POINT ( 'NONE',  ( 0.1267340139221234119, -0.09851384784732598876, 0.1767400091468230294 ) ) ;
#20404 = CARTESIAN_POINT ( 'NONE',  ( -1.033464566929134687, -0.06523048226347956391, 1.847933070758615237 ) ) ;
#20405 = ORIENTED_EDGE ( 'NONE', *, *, #4702, .T. ) ;
#20406 = ADVANCED_FACE ( 'NONE', ( #13555 ), #41574, .F. ) ;
#20407 = EDGE_CURVE ( 'NONE', #9939, #36104, #28414, .T. ) ;
#20408 = CARTESIAN_POINT ( 'NONE',  ( -0.8019270111902717657, 0.1787899950787401604, 1.023622047190330342 ) ) ;
#20409 = EDGE_CURVE ( 'NONE', #10797, #37122, #42897, .T. ) ;
#20410 = PRODUCT_DEFINITION ( 'UNKNOWN', '', #22435, #24535 ) ;
#20411 = MANIFOLD_SOLID_BREP ( 'Pivot Shaft', #8762 ) ;
#20412 = CARTESIAN_POINT ( 'NONE',  ( 0.1787899950787401604, -1.647761763504828947, -0.07405724077823318263 ) ) ;
#20413 = VERTEX_POINT ( 'NONE', #43481 ) ;
#20414 = CYLINDRICAL_SURFACE ( 'NONE', #44793, 0.3937007874015748254 ) ;
#20415 = CARTESIAN_POINT ( 'NONE',  ( 0.1787899950787401882, -0.5319881889226142357, -2.189545951927503898E-17 ) ) ;
#20416 = CARTESIAN_POINT ( 'NONE',  ( 0.2471922904502826812, -0.09842519685039370636, -5.914624404477007554E-17 ) ) ;
#20417 = ORIENTED_EDGE ( 'NONE', *, *, #36217, .T. ) ;
#20418 = CARTESIAN_POINT ( 'NONE',  ( 0.7495606340400177148, 0.1264236179284866091, 1.375492125930488196 ) ) ;
#20419 = DIRECTION ( 'NONE',  ( 0.5735764363510447161, 0.8191520442889925757, 0.000000000000000000 ) ) ;
#20420 = CARTESIAN_POINT ( 'NONE',  ( -1.094772975963752103E-17, -0.3695866141194649179, -0.1787899950787401882 ) ) ;
#20421 = CARTESIAN_POINT ( 'NONE',  ( 0.07405724077823318263, -0.7362204723871804690, 0.1787899950787401604 ) ) ;
#20422 = DIRECTION ( 'NONE',  ( -1.000000000000000000, 0.000000000000000000, 0.000000000000000000 ) ) ;
#20423 = CARTESIAN_POINT ( 'NONE',  ( 0.1377952755905511306, 0.000000000000000000, -0.3149606299212598381 ) ) ;
#20424 = CARTESIAN_POINT ( 'NONE',  ( 1.002407869896990045, 0.1264236179284866091, 1.601870078686393750 ) ) ;
#20425 = CARTESIAN_POINT ( 'NONE',  ( 0.1264236179284866091, 0.03776973255816284264, 0.1264236179284866091 ) ) ;
#20426 = CONTEXT_DEPENDENT_SHAPE_REPRESENTATION ( #35206, #4644 ) ;
#20427 = CARTESIAN_POINT ( 'NONE',  ( 0.05568348810326462922, -0.09842519685039373412, 0.1550565792168007162 ) ) ;
#20428 = CARTESIAN_POINT ( 'NONE',  ( 0.8019270111902717657, 0.1787899950787401604, 0.5068897637257642197 ) ) ;
#20429 = AXIS2_PLACEMENT_3D ( 'NONE', #26685, #45328, #12545 ) ;
#20430 = CARTESIAN_POINT ( 'NONE',  ( -0.6971942568897637749, 2.189545951927499583E-17, 0.7554133857730077617 ) ) ;
#20432 = CARTESIAN_POINT ( 'NONE',  ( 0.8107537697050254399, 0.1574803149606300301, 0.09104330697908723236 ) ) ;
#20431 = CARTESIAN_POINT ( 'NONE',  ( -0.1574803149606297803, -0.9306102362204727863, 0.06523048226347956391 ) ) ;
#20434 = CARTESIAN_POINT ( 'NONE',  ( -0.8097075710689116690, -0.1591366973851143507, 1.986952455759391389 ) ) ;
#20433 = CARTESIAN_POINT ( 'NONE',  ( 0.1797182628040039087, -1.519236722968871467, 0.07444174185955046430 ) ) ;
#20435 = CARTESIAN_POINT ( 'NONE',  ( -0.1574803149606297803, -0.4483267715460167446, 0.06523048226347956391 ) ) ;
#20436 = CARTESIAN_POINT ( 'NONE',  ( 0.6971942568897637749, 2.189545951927499583E-17, 1.582185039316315045 ) ) ;
#20437 = CARTESIAN_POINT ( 'NONE',  ( -0.2066929133858267931, 0.2876548164643190630, -0.2627373885913885099 ) ) ;
#20438 = CARTESIAN_POINT ( 'NONE',  ( 0.9500414927467377701, 0.1787899950787401604, 0.3838582676627718127 ) ) ;
#20440 = EDGE_CURVE ( 'NONE', #2480, #39584, #29168, .T. ) ;
#20439 = DIRECTION ( 'NONE',  ( -1.000000000000000000, 0.000000000000000000, 0.000000000000000000 ) ) ;
#20441 = CARTESIAN_POINT ( 'NONE',  ( 0.9873396505805591694, -0.1113553986120547346, 0.8612204723334173639 ) ) ;
#20442 = DIRECTION ( 'NONE',  ( 1.000000000000000000, 0.000000000000000000, 0.000000000000000000 ) ) ;
#20444 = CARTESIAN_POINT ( 'NONE',  ( 0.1264236179284866091, -0.03001968498560653523, 0.1264236179284866091 ) ) ;
#20443 = CARTESIAN_POINT ( 'NONE',  ( -0.1574803149606299191, -0.8838582676090078749, 0.000000000000000000 ) ) ;
#20445 = CARTESIAN_POINT ( 'NONE',  ( 1.054774247047244096, 0.000000000000000000, 0.4158464566391496531 ) ) ;
#20446 = CARTESIAN_POINT ( 'NONE',  ( 3.284318927891251994E-17, -0.9355314960092283583, 0.1787899950787401882 ) ) ;
#20447 = CARTESIAN_POINT ( 'NONE',  ( 0.8107537697050234415, -0.1574803149606297803, 0.07627952755905519078 ) ) ;
#20448 = CARTESIAN_POINT ( 'NONE',  ( -0.5555748031496021699, 1.332209862199694284, -0.06082000038405668829 ) ) ;
#20449 = CARTESIAN_POINT ( 'NONE',  ( -0.8759842519685039353, 0.1787899950787401882, 1.449311023568283341 ) ) ;
#20450 = CARTESIAN_POINT ( 'NONE',  ( 0.8759842519685039353, 0.1574803149606299191, 0.7578740156405039397 ) ) ;
#20451 = ORIENTED_EDGE ( 'NONE', *, *, #38521, .T. ) ;
#20452 = CYLINDRICAL_SURFACE ( 'NONE', #18413, 0.1574803149606299191 ) ;
#20453 = ADVANCED_FACE ( 'NONE', ( #43722 ), #36554, .F. ) ;
#20454 = CARTESIAN_POINT ( 'NONE',  ( 0.9500414927467378812, -0.1787899950787401604, 0.9645669290800953366 ) ) ;
#20455 = VERTEX_POINT ( 'NONE', #32015 ) ;
#20456 = CARTESIAN_POINT ( 'NONE',  ( 0.06523048226347956391, -1.068405511703496069, 0.1574803149606297803 ) ) ;
#20457 = CARTESIAN_POINT ( 'NONE',  ( -0.7185039370078746268, 0.06523048226347956391, 0.5684055117034967353 ) ) ;
#20458 = FACE_OUTER_BOUND ( 'NONE', #9455, .T. ) ;
#20459 = CARTESIAN_POINT ( 'NONE',  ( 1.054774247047244540, -0.07405724077823318263, 1.712598425143087688 ) ) ;
#20460 = CARTESIAN_POINT ( 'NONE',  ( -0.7646288533564489232, -0.1113553986120547346, 1.451771653543306950 ) ) ;
#20461 = CARTESIAN_POINT ( 'NONE',  ( -0.4620708661417322616, 0.9842519685039375910, -0.8759842519685044904 ) ) ;
#20462 = CARTESIAN_POINT ( 'NONE',  ( -0.9412147342319837628, 0.1574803149606300301, 0.7258858267716534751 ) ) ;
#20463 = CARTESIAN_POINT ( 'NONE',  ( 0.8019270111902716547, -0.1787899950787401604, 0.2116141731745827814 ) ) ;
#20464 = CARTESIAN_POINT ( 'NONE',  ( -1.054774247047244540, 0.07405724077823318263, 0.1033464566391499029 ) ) ;
#20465 = CARTESIAN_POINT ( 'NONE',  ( 0.9412147342319837628, 0.1574803149606300301, 1.424704724301921743 ) ) ;
#20466 = ORIENTED_EDGE ( 'NONE', *, *, #21253, .F. ) ;
#20467 = EDGE_LOOP ( 'NONE', ( #5309, #44877, #31177, #17903, #2148 ) ) ;
#20468 = CARTESIAN_POINT ( 'NONE',  ( -0.07405724077823318263, 0.1200787402112438867, 0.1787899950787401604 ) ) ;
#20469 = CARTESIAN_POINT ( 'NONE',  ( 0.1994795808946360216, -0.1803246425350570614, -0.05524818609633110750 ) ) ;
#20470 = ORIENTED_EDGE ( 'NONE', *, *, #40556, .T. ) ;
#20471 = CARTESIAN_POINT ( 'NONE',  ( -0.6971942568897637749, 2.189545951927499583E-17, 1.774114173174582643 ) ) ;
#20472 = VECTOR ( 'NONE', #44422, 39.37007874015748143 ) ;
#20473 = DIRECTION ( 'NONE',  ( 0.8191520442889873577, 0.000000000000000000, 0.5735764363510523767 ) ) ;
#20474 = FACE_OUTER_BOUND ( 'NONE', #4445, .T. ) ;
#20475 = LINE ( 'NONE', #46104, #38967 ) ;
#20476 = CARTESIAN_POINT ( 'NONE',  ( 0.1264236179284866091, -1.143332629646561127, 0.1264236179284866091 ) ) ;
#20477 = ORIENTED_EDGE ( 'NONE', *, *, #36334, .F. ) ;
#20478 = CARTESIAN_POINT ( 'NONE',  ( -0.1264236179284866091, -0.1136811023084411398, 0.1264236179284866091 ) ) ;
#20479 = EDGE_LOOP ( 'NONE', ( #17802, #18209, #35579, #1550 ) ) ;
#20480 = ORIENTED_EDGE ( 'NONE', *, *, #45312, .F. ) ;
#20481 = CARTESIAN_POINT ( 'NONE',  ( 1.002407869896990045, -0.1264236179284866091, 1.080216535379306952 ) ) ;
#20482 = CARTESIAN_POINT ( 'NONE',  ( -9.642888182262618425E-18, 0.05118110246973173183, -0.1574803149606299191 ) ) ;
#20483 = CARTESIAN_POINT ( 'NONE',  ( -1.033464566929133799, 0.000000000000000000, 0.9842519683964094934 ) ) ;
#20484 = CARTESIAN_POINT ( 'NONE',  ( 0.7185039370078746268, -0.06523048226347956391, 1.843011811023621327 ) ) ;
#20485 = APPLICATION_CONTEXT ( 'automotive_design' ) ;
#20486 = CARTESIAN_POINT ( 'NONE',  ( -0.1787899950787401882, -0.6747047243556849594, 0.000000000000000000 ) ) ;
#20487 = CARTESIAN_POINT ( 'NONE',  ( -1.054774247047244096, 0.000000000000000000, 0.3420275590013546751 ) ) ;
#20488 = CARTESIAN_POINT ( 'NONE',  ( -0.7646288533564489232, 0.1113553986120547346, 1.008858267716535417 ) ) ;
#20489 = CONICAL_SURFACE ( 'NONE', #562, 0.1574803149606299191, 0.9599310885968713736 ) ;
#20490 = CARTESIAN_POINT ( 'NONE',  ( -0.1270800023317771588, -1.226421762338950838, -0.1270800023317771588 ) ) ;
#20491 = CARTESIAN_POINT ( 'NONE',  ( -0.1849324350982172738, 0.1887234410765585568, -0.04495255068435553836 ) ) ;
#20492 = CARTESIAN_POINT ( 'NONE',  ( 1.002407869896990045, -0.1264236179284866091, 1.124507873961984261 ) ) ;
#20493 = CARTESIAN_POINT ( 'NONE',  ( 0.8759842519685039353, -0.1787899950787401882, 1.587106299158834721 ) ) ;
#20495 = EDGE_CURVE ( 'NONE', #33124, #20413, #7068, .T. ) ;
#20494 = DIRECTION ( 'NONE',  ( -1.000000000000000000, 0.000000000000000000, 0.000000000000000000 ) ) ;
#20497 = CARTESIAN_POINT ( 'NONE',  ( -0.8360297024941153454, 0.1537365954182407513, 1.979133126318196823 ) ) ;
#20496 = CARTESIAN_POINT ( 'NONE',  ( 0.7668818483817357867, 0.1192326576165682328, 1.980675047218597218 ) ) ;
#20498 = DIRECTION ( 'NONE',  ( -1.000000000000000000, 0.000000000000000000, 0.000000000000000000 ) ) ;
#20499 = CARTESIAN_POINT ( 'NONE',  ( 0.7185039370078739607, 1.928577636452523993E-17, 0.6889763778452283605 ) ) ;
#20500 = CARTESIAN_POINT ( 'NONE',  ( 0.06523048226347956391, -0.7140748030420803749, 0.1574803149606297803 ) ) ;
#20501 = AXIS2_PLACEMENT_3D ( 'NONE', #232, #40479, #6959 ) ;
#20502 = EDGE_CURVE ( 'NONE', #42193, #8550, #13786, .T. ) ;
#20503 = CARTESIAN_POINT ( 'NONE',  ( 0.8107537697050254399, -0.1574803149606297803, 1.651082677165354839 ) ) ;
#20504 = CARTESIAN_POINT ( 'NONE',  ( 1.002407869896990045, -0.1264236179284866091, 1.001476377898992132 ) ) ;
#20505 = CARTESIAN_POINT ( 'NONE',  ( 1.002407869896990045, -0.1264236179284866091, 1.911909448765133801 ) ) ;
#20506 = CARTESIAN_POINT ( 'NONE',  ( 0.9412147342319837628, -0.1574803149606297803, 0.3075787400499532809 ) ) ;
#20507 = VERTEX_POINT ( 'NONE', #21696 ) ;
#20508 = CARTESIAN_POINT ( 'NONE',  ( 0.4330708661417322913, 0.08090551181102362266, 9.908067607274841931E-18 ) ) ;
#20509 = EDGE_CURVE ( 'NONE', #43030, #6306, #17618, .T. ) ;
#20510 = CARTESIAN_POINT ( 'NONE',  ( 0.1113553986120547346, -1.686023621939716444, -0.1113553986120547346 ) ) ;
#20511 = CARTESIAN_POINT ( 'NONE',  ( -0.8107537697050234415, -0.1574803149606297803, 0.3026574802074335491 ) ) ;
#20512 = CARTESIAN_POINT ( 'NONE',  ( 0.7495606340400177148, 0.1264236179284866091, 1.296751968450173154 ) ) ;
#20513 = EDGE_CURVE ( 'NONE', #34093, #32371, #42750, .T. ) ;
#20515 = CARTESIAN_POINT ( 'NONE',  ( 0.8107537697050234415, -0.1574803149606297803, 0.06643700776648873985 ) ) ;
#20514 = DIRECTION ( 'NONE',  ( 0.000000000000000000, -1.000000000000000000, 0.000000000000000000 ) ) ;
#20516 = CARTESIAN_POINT ( 'NONE',  ( -0.06523048226347956391, -1.791830708661417138, 0.1574803149606297803 ) ) ;
#20517 = DIRECTION ( 'NONE',  ( -1.000000000000000000, 0.000000000000000000, 0.000000000000000000 ) ) ;
#20518 = ( BOUNDED_CURVE ( )  B_SPLINE_CURVE ( 2, ( #5839, #2001, #23579, #20447, #38189, #20915, #46078, #42475, #35554 ),
 .UNSPECIFIED., .F., .T. ) 
 B_SPLINE_CURVE_WITH_KNOTS ( ( 3, 2, 2, 2, 3 ),
 ( 0.02999999999999999889, 0.03250000000000000111, 0.03500000000000000333, 0.03749999999999999861, 0.04000000000000000083 ),
 .UNSPECIFIED. ) 
 CURVE ( )  GEOMETRIC_REPRESENTATION_ITEM ( )  RATIONAL_B_SPLINE_CURVE ( ( 1.000000000000000000, 0.9238795325112869605, 1.000000000000000000, 0.9238795325112869605, 1.000000000000000000, 0.9238795325112869605, 1.000000000000000000, 0.9238795325112869605, 1.000000000000000000 ) ) 
 REPRESENTATION_ITEM ( '' )  ) ;
#20519 = CARTESIAN_POINT ( 'NONE',  ( 0.7185039370078766252, -0.06523048226348168721, 1.360728346349167284 ) ) ;
#20520 = CARTESIAN_POINT ( 'NONE',  ( -0.8759842519685039353, 0.1574803149606299191, 0.2066929132782996115 ) ) ;
#20521 = CARTESIAN_POINT ( 'NONE',  ( -0.8759842519685039353, 0.000000000000000000, 1.978346456692913646 ) ) ;
#20522 = ORIENTED_EDGE ( 'NONE', *, *, #7247, .F. ) ;
#20523 = CARTESIAN_POINT ( 'NONE',  ( -1.002407869896990045, -0.1264236179284866091, 1.395177165300567124 ) ) ;
#20524 = CARTESIAN_POINT ( 'NONE',  ( 0.1787899950787401882, -1.718011810969858333, -2.189545951927503898E-17 ) ) ;
#20525 = CARTESIAN_POINT ( 'NONE',  ( -0.8759842519685039353, -0.1787899950787401882, 0.9227362204186770889 ) ) ;
#20526 = CARTESIAN_POINT ( 'NONE',  ( -0.9873396505805591694, 0.1113553986120547346, 0.01476377952755905665 ) ) ;
#20527 = EDGE_LOOP ( 'NONE', ( #7332, #14777, #7773, #12714 ) ) ;
#20528 = CARTESIAN_POINT ( 'NONE',  ( -1.054774247047244540, -0.07405724077823318263, 1.003937007820253413 ) ) ;
#20529 = CARTESIAN_POINT ( 'NONE',  ( -0.8019270111902717657, 0.1787899950787401604, 0.6299212597887560161 ) ) ;
#20530 = CIRCLE ( 'NONE', #13648, 0.3912448816427701037 ) ;
#20531 = DIRECTION ( 'NONE',  ( -1.000000000000000000, 0.000000000000000000, 0.000000000000000000 ) ) ;
#20532 = ORIENTED_EDGE ( 'NONE', *, *, #31462, .F. ) ;
#20533 = CARTESIAN_POINT ( 'NONE',  ( 0.2027848556993381846, -0.08956017357703426052, -0.01042671155077139894 ) ) ;
#20534 = ORIENTED_EDGE ( 'NONE', *, *, #7370, .F. ) ;
#20535 = LINE ( 'NONE', #45447, #9597 ) ;
#20536 = AXIS2_PLACEMENT_3D ( 'NONE', #16305, #31865, #42134 ) ;
#20537 = ( BOUNDED_CURVE ( )  B_SPLINE_CURVE ( 2, ( #4779, #30239, #4528, #41177, #7669, #12237, #29542, #7911, #3842 ),
 .UNSPECIFIED., .F., .F. ) 
 B_SPLINE_CURVE_WITH_KNOTS ( ( 3, 2, 2, 2, 3 ),
 ( 0.8199999999999999512, 0.8225000000000000089, 0.8249999999999999556, 0.8275000000000000133, 0.8299999999999999600 ),
 .UNSPECIFIED. ) 
 CURVE ( )  GEOMETRIC_REPRESENTATION_ITEM ( )  RATIONAL_B_SPLINE_CURVE ( ( 1.000000000000000000, 0.9238795325112899581, 1.000000000000000000, 0.9238795325112869605, 1.000000000000000000, 0.9238795325112869605, 1.000000000000000000, 0.9238795325112799661, 1.000000000000000000 ) ) 
 REPRESENTATION_ITEM ( '' )  ) ;
#20538 = CARTESIAN_POINT ( 'NONE',  ( -0.8759842519685039353, 0.1787899950787401882, 0.6619094487651338010 ) ) ;
#20539 = CARTESIAN_POINT ( 'NONE',  ( -0.7185039370078739607, 1.928577636452523993E-17, 0.5708661416247566844 ) ) ;
#20540 = ORIENTED_EDGE ( 'NONE', *, *, #4304, .T. ) ;
#20541 = CARTESIAN_POINT ( 'NONE',  ( -0.8759842519685039353, -0.1787899950787401882, 1.631397637741511808 ) ) ;
#20542 = CARTESIAN_POINT ( 'NONE',  ( -0.2026160082443592969, -0.5228204797047604213, -0.8983653719476394350 ) ) ;
#20543 = FILL_AREA_STYLE_COLOUR ( '', #46276 ) ;
#20544 = CARTESIAN_POINT ( 'NONE',  ( 0.9412147342319837628, -0.1574803149606297803, 0.5930118110236219930 ) ) ;
#20545 = CARTESIAN_POINT ( 'NONE',  ( -1.033464566929133799, 0.000000000000000000, 0.9547244094488189781 ) ) ;
#20546 = CARTESIAN_POINT ( 'NONE',  ( -0.7646288533564489232, 0.1113553986120547346, 1.274606299105070839 ) ) ;
#20548 = DIRECTION ( 'NONE',  ( 0.000000000000000000, 1.000000000000000000, 0.000000000000000000 ) ) ;
#20547 = CARTESIAN_POINT ( 'NONE',  ( -0.1574803149606299191, -0.4606299212598425341, 0.000000000000000000 ) ) ;
#20549 = PLANE ( 'NONE',  #23852 ) ;
#20550 = EDGE_LOOP ( 'NONE', ( #28819, #44776, #38319, #19520, #296 ) ) ;
#20551 = LINE ( 'NONE', #35427, #38352 ) ;
#20552 = CARTESIAN_POINT ( 'NONE',  ( 0.9412147342319837628, -0.1574803149606297803, 1.144192913385827737 ) ) ;
#20554 = DIRECTION ( 'NONE',  ( 1.000000000000000000, -3.368395098984090098E-15, 0.000000000000000000 ) ) ;
#20553 = CARTESIAN_POINT ( 'NONE',  ( -0.8759842519685039353, 0.1574803149606299191, 1.269685039262551163 ) ) ;
#20555 = CARTESIAN_POINT ( 'NONE',  ( 0.7185039370078746268, -0.06523048226347956391, 1.961122047244095778 ) ) ;
#20556 = EDGE_CURVE ( 'NONE', #47261, #31760, #35612, .T. ) ;
#20557 = CARTESIAN_POINT ( 'NONE',  ( 0.4632545931758527691, 4.616380251121755931E-17, 0.000000000000000000 ) ) ;
#20558 = VECTOR ( 'NONE', #4440, 39.37007874015748143 ) ;
#20559 = CARTESIAN_POINT ( 'NONE',  ( -0.1476731086701386642, -0.08957115901137824299, -0.09624711833952896700 ) ) ;
#20560 = CARTESIAN_POINT ( 'NONE',  ( -0.1787899950787401604, -0.5541338582139530011, -0.07405724077823318263 ) ) ;
#20561 = CARTESIAN_POINT ( 'NONE',  ( 0.000000000000000000, 0.000000000000000000, -0.3001770169643759867 ) ) ;
#20562 = ORIENTED_EDGE ( 'NONE', *, *, #43163, .F. ) ;
#20563 = CARTESIAN_POINT ( 'NONE',  ( -0.8759842519685039353, -0.1574803149606299191, 1.062992125984252079 ) ) ;
#20564 = CARTESIAN_POINT ( 'NONE',  ( 0.1583744855326529033, 0.03901141430315911013, -0.1404421906569247869 ) ) ;
#20565 = CARTESIAN_POINT ( 'NONE',  ( 0.8759842519685039353, 0.1787899950787401882, 0.8587598424659212970 ) ) ;
#20566 = EDGE_CURVE ( 'NONE', #3060, #42269, #19981, .T. ) ;
#20567 = ORIENTED_EDGE ( 'NONE', *, *, #44394, .F. ) ;
#20568 = CARTESIAN_POINT ( 'NONE',  ( -7.957671378281915615E-17, 0.1564960629921311464, -0.3937007874015748254 ) ) ;
#20569 = CARTESIAN_POINT ( 'NONE',  ( 0.5358894627757212481, 4.766607801171850497E-17, 0.000000000000000000 ) ) ;
#20570 = CARTESIAN_POINT ( 'NONE',  ( 0.1270800023317771588, 0.1318459541964820958, 0.1270800023317771588 ) ) ;
#20571 = CARTESIAN_POINT ( 'NONE',  ( -0.1787899950787401882, -1.068405511757259951, 0.000000000000000000 ) ) ;
#20572 = CARTESIAN_POINT ( 'NONE',  ( 0.1574803149606299191, -1.307086614173228467, -1.928577636452523993E-17 ) ) ;
#20573 = CARTESIAN_POINT ( 'NONE',  ( 0.1608764814808673338, 0.1607246848665348227, 0.002792769038232334466 ) ) ;
#20574 = ORIENTED_EDGE ( 'NONE', *, *, #36269, .F. ) ;
#20575 = CARTESIAN_POINT ( 'NONE',  ( -0.8019270111902717657, -0.1787899950787401604, 1.865157480261195877 ) ) ;
#20576 = CARTESIAN_POINT ( 'NONE',  ( 1.054774247047244096, 0.000000000000000000, 1.877460629867496067 ) ) ;
#20577 = ORIENTED_EDGE ( 'NONE', *, *, #9039, .F. ) ;
#20578 = CYLINDRICAL_SURFACE ( 'NONE', #35588, 0.1574803149606299191 ) ;
#20579 = CARTESIAN_POINT ( 'NONE',  ( -0.7495606340400177148, -0.1264236179284866091, 1.503444881836000002 ) ) ;
#20580 = DIRECTION ( 'NONE',  ( -1.000000000000000000, 0.000000000000000000, 0.000000000000000000 ) ) ;
#20581 = CARTESIAN_POINT ( 'NONE',  ( -0.9500414927467378812, 0.1787899950787401604, 1.013779527505291878 ) ) ;
#20582 = CARTESIAN_POINT ( 'NONE',  ( -0.6971942568897637749, 2.189545951927499583E-17, 0.1648622046706460786 ) ) ;
#20583 = DIRECTION ( 'NONE',  ( 7.659124183791938496E-17, -1.000000000000000000, 1.016400108624885935E-16 ) ) ;
#20584 = CARTESIAN_POINT ( 'NONE',  ( -1.054774247047244540, -0.07405724077823318263, 1.914370078686394860 ) ) ;
#20585 = CARTESIAN_POINT ( 'NONE',  ( 0.06215339161709781957, -0.08126078924485156951, -0.2495487439734428159 ) ) ;
#20586 = CARTESIAN_POINT ( 'NONE',  ( -1.033464566929133799, 0.000000000000000000, 1.820866141732283561 ) ) ;
#20587 = CARTESIAN_POINT ( 'NONE',  ( -0.8759842519685039353, 0.000000000000000000, 1.995570866087968520 ) ) ;
#20588 = CARTESIAN_POINT ( 'NONE',  ( -0.07405724077823318263, -0.2599664879142782326, -0.1787899950787401604 ) ) ;
#20589 = CARTESIAN_POINT ( 'NONE',  ( 0.06243605173690295468, -0.09842519685039370636, -0.1835744151064638008 ) ) ;
#20590 = DIRECTION ( 'NONE',  ( 0.000000000000000000, 0.000000000000000000, -1.000000000000000000 ) ) ;
#20591 = DIRECTION ( 'NONE',  ( 0.000000000000000000, 0.000000000000000000, -1.000000000000000000 ) ) ;
#20592 = EDGE_CURVE ( 'NONE', #37242, #32711, #5445, .T. ) ;
#20593 = AXIS2_PLACEMENT_3D ( 'NONE', #39346, #45831, #20442 ) ;
#20594 = ORIENTED_EDGE ( 'NONE', *, *, #32334, .T. ) ;
#20595 = CARTESIAN_POINT ( 'NONE',  ( -1.054774247047244540, 0.07405724077823318263, 1.249999999946235896 ) ) ;
#20596 = ORIENTED_EDGE ( 'NONE', *, *, #45925, .F. ) ;
#20597 = CARTESIAN_POINT ( 'NONE',  ( -1.094772975963752103E-17, -1.038877952702141672, -0.1787899950787401882 ) ) ;
#20598 = AXIS2_PLACEMENT_3D ( 'NONE', #37265, #26280, #8033 ) ;
#20599 = CARTESIAN_POINT ( 'NONE',  ( 0.1787899950787401604, -1.282480314906867314, 0.07405724077823318263 ) ) ;
#20600 = CARTESIAN_POINT ( 'NONE',  ( -0.1586641775163213364, 2.559880088878760951, -3.648497683167374550 ) ) ;
#20601 = CARTESIAN_POINT ( 'NONE',  ( 0.6971942568897626646, -0.07405724077823297447, 0.3986220471903312301 ) ) ;
#20602 = CARTESIAN_POINT ( 'NONE',  ( -0.1797182628040039087, -0.5497485339924945702, 0.07444174185955065859 ) ) ;
#20603 = CYLINDRICAL_SURFACE ( 'NONE', #14829, 0.1377952755905510751 ) ;
#20604 = CARTESIAN_POINT ( 'NONE',  ( -0.9873396505805591694, -0.1113553986120547346, 0.7824803148531023211 ) ) ;
#20605 = CARTESIAN_POINT ( 'NONE',  ( -0.8107537697050253289, 0.1574803149606300301, 0.7308070866141725963 ) ) ;
#20606 = AXIS2_PLACEMENT_3D ( 'NONE', #24242, #10088, #38605 ) ;
#20607 = CARTESIAN_POINT ( 'NONE',  ( 0.06523048226347956391, -0.03986220472440944740, -0.1574803149606300301 ) ) ;
#20608 = CARTESIAN_POINT ( 'NONE',  ( 0.8019270111902717657, -0.1787899950787401604, 0.8759842519147408302 ) ) ;
#20609 = CARTESIAN_POINT ( 'NONE',  ( 0.1677835123531307704, -0.1986243762397479629, -0.03618545512907316714 ) ) ;
#20610 = EDGE_CURVE ( 'NONE', #32499, #43205, #10770, .T. ) ;
#20611 = DIRECTION ( 'NONE',  ( 0.000000000000000000, 0.000000000000000000, -1.000000000000000000 ) ) ;
#20612 = CARTESIAN_POINT ( 'NONE',  ( 0.7495606340400177148, -0.1264236179284866091, 1.980807086560409491 ) ) ;
#20613 = ORIENTED_EDGE ( 'NONE', *, *, #20566, .F. ) ;
#20614 = ORIENTED_EDGE ( 'NONE', *, *, #38037, .T. ) ;
#20615 = CARTESIAN_POINT ( 'NONE',  ( 0.7185039370078741827, 0.06523048226347841205, 0.7258858266641272650 ) ) ;
#20616 = CARTESIAN_POINT ( 'NONE',  ( 0.1787899950787401604, -0.6574803149068665364, 0.07405724077823318263 ) ) ;
#20617 = CARTESIAN_POINT ( 'NONE',  ( 0.1787899950787401882, -1.358759842465921297, -2.189545951927503898E-17 ) ) ;
#20618 = CARTESIAN_POINT ( 'NONE',  ( 1.054774247047244096, 0.000000000000000000, 0.3420275590013546751 ) ) ;
#20619 = CIRCLE ( 'NONE', #9137, 0.09842519685039310962 ) ;
#20620 = CARTESIAN_POINT ( 'NONE',  ( -0.6971942568897648851, 0.07405724077823318263, 1.968503936954110189 ) ) ;
#20621 = EDGE_LOOP ( 'NONE', ( #44647, #39593 ) ) ;
#20622 = CARTESIAN_POINT ( 'NONE',  ( -1.054774247047244540, 0.07405724077823318263, 1.407480314906865981 ) ) ;
#20623 = CARTESIAN_POINT ( 'NONE',  ( 0.8019270111902717657, -0.1787899950787401604, 1.353346456639149986 ) ) ;
#20624 = DIRECTION ( 'NONE',  ( 0.000000000000000000, 0.000000000000000000, 1.000000000000000000 ) ) ;
#20625 = CARTESIAN_POINT ( 'NONE',  ( 0.1574803149606300301, -1.255413385719243768, -0.06523048226347956391 ) ) ;
#20626 = CARTESIAN_POINT ( 'NONE',  ( -0.6971942568897637749, 2.189545951927499583E-17, 0.7160433070328504623 ) ) ;
#20627 = CARTESIAN_POINT ( 'NONE',  ( 0.1344414905952618366, -0.09842522719093642347, -0.1178619895492928893 ) ) ;
#20628 = CARTESIAN_POINT ( 'NONE',  ( -1.033464566929134687, 0.06523048226347956391, 1.616633858160190229 ) ) ;
#20629 = CARTESIAN_POINT ( 'NONE',  ( 0.8759842519685039353, -0.1787899950787401882, 0.6471456692375747721 ) ) ;
#20630 = CARTESIAN_POINT ( 'NONE',  ( -1.054774247047244540, 0.07405724077823318263, 0.4970472440407249226 ) ) ;
#20631 = CIRCLE ( 'NONE', #32914, 0.1574803149606299191 ) ;
#20632 = CARTESIAN_POINT ( 'NONE',  ( 0.1715440989610381162, -0.08785038237333182842, 0.1863907177291471429 ) ) ;
#20633 = CARTESIAN_POINT ( 'NONE',  ( 0.9873396505805591694, 0.1113553986120547346, 1.658464566821606256 ) ) ;
#20634 = ORIENTED_EDGE ( 'NONE', *, *, #34007, .F. ) ;
#20635 = FACE_BOUND ( 'NONE', #45464, .T. ) ;
#20636 = CARTESIAN_POINT ( 'NONE',  ( -0.7646288533564489232, -0.1113553986120547346, 0.5068897637795275468 ) ) ;
#20637 = VECTOR ( 'NONE', #30818, 39.37007874015748143 ) ;
#20638 = CARTESIAN_POINT ( 'NONE',  ( 1.002407869896990045, -0.1264236179284866091, 1.242618110182456714 ) ) ;
#20639 = CARTESIAN_POINT ( 'NONE',  ( 0.1815679472391334703, -0.09851384343985296332, -0.08954567948069468153 ) ) ;
#20640 = ORIENTED_EDGE ( 'NONE', *, *, #2007, .F. ) ;
#20641 = DIRECTION ( 'NONE',  ( 1.000000000000000000, -0.000000000000000000, -0.000000000000000000 ) ) ;
#20642 = CARTESIAN_POINT ( 'NONE',  ( -0.9500414927467378812, -0.1787899950787401604, 1.003937007820251193 ) ) ;
#20643 = SHAPE_REPRESENTATION ( 'ISO 4162 M5x10 Hex Flange Bolt', ( #20860 ), #30086 ) ;
#20644 = CARTESIAN_POINT ( 'NONE',  ( 3.284318927891251994E-17, -1.581324755630813206, 0.1787899950787401882 ) ) ;
#20645 = VERTEX_POINT ( 'NONE', #7540 ) ;
#20646 = CARTESIAN_POINT ( 'NONE',  ( 0.1264236179284866091, -0.5664370078202519698, -0.1264236179284866091 ) ) ;
#20647 = CARTESIAN_POINT ( 'NONE',  ( 0.7185039370078746268, 0.06523048226347956391, 0.4995078740157475883 ) ) ;
#20648 = DIRECTION ( 'NONE',  ( -0.000000000000000000, 0.000000000000000000, -1.000000000000000000 ) ) ;
#20649 = CARTESIAN_POINT ( 'NONE',  ( 0.1264236179284866091, -0.2563976377415121966, -0.1264236179284866091 ) ) ;
#20650 = CARTESIAN_POINT ( 'NONE',  ( -0.1787899950787401882, -0.7485236219934803259, 0.000000000000000000 ) ) ;
#20651 = VECTOR ( 'NONE', #18163, 39.37007874015748143 ) ;
#20652 = CARTESIAN_POINT ( 'NONE',  ( -0.4955489724641236604, 0.3740157480314960647, 0.3997690233743834698 ) ) ;
#20653 = CARTESIAN_POINT ( 'NONE',  ( -0.8107537697050254399, -0.1574803149606297803, 0.9719488187901104137 ) ) ;
#20654 = EDGE_CURVE ( 'NONE', #28784, #24486, #7774, .T. ) ;
#20655 = CARTESIAN_POINT ( 'NONE',  ( 0.1787899950787401882, 0.003320913660525051311, -2.189545951927503898E-17 ) ) ;
#20656 = FACE_OUTER_BOUND ( 'NONE', #25409, .T. ) ;
#20657 = CARTESIAN_POINT ( 'NONE',  ( 1.002407869896990045, -0.1264236179284866091, 0.4502952755367874427 ) ) ;
#20658 = DIMENSIONAL_EXPONENTS ( 1.000000000000000000, 0.000000000000000000, 0.000000000000000000, 0.000000000000000000, 0.000000000000000000, 0.000000000000000000, 0.000000000000000000 ) ;
#20659 = AXIS2_PLACEMENT_3D ( 'NONE', #12723, #38329, #31638 ) ;
#20660 = CARTESIAN_POINT ( 'NONE',  ( -1.002407869896990045, -0.1264236179284866091, 0.8489173227808819444 ) ) ;
#20661 = EDGE_CURVE ( 'NONE', #18242, #40994, #17182, .T. ) ;
#20662 = CARTESIAN_POINT ( 'NONE',  ( -1.033464566929133799, 0.000000000000000000, 1.299212598317669221 ) ) ;
#20664 = CARTESIAN_POINT ( 'NONE',  ( 0.000000000000000000, 0.000000000000000000, 0.000000000000000000 ) ) ;
#20663 = CARTESIAN_POINT ( 'NONE',  ( 0.1113553986120547346, -0.8297244094488188670, -0.1113553986120547346 ) ) ;
#20665 = CARTESIAN_POINT ( 'NONE',  ( -0.07444174185955065859, -1.740693415882258011, -0.1797182628040039087 ) ) ;
#20666 = CARTESIAN_POINT ( 'NONE',  ( -0.1574803149606297803, -0.4876968502861737664, 0.06523048226347956391 ) ) ;
#20667 = CARTESIAN_POINT ( 'NONE',  ( 0.07405724077823318263, -0.3425196849856064762, 0.1787899950787401604 ) ) ;
#20668 = CARTESIAN_POINT ( 'NONE',  ( -0.7646288533564489232, -0.1113553986120547346, 1.245078740049952559 ) ) ;
#20669 = CARTESIAN_POINT ( 'NONE',  ( 1.054774247047244096, 0.000000000000000000, 1.444389763725763665 ) ) ;
#20671 = CARTESIAN_POINT ( 'NONE',  ( 0.5057057357416000487, 0.09842519685039370636, 0.000000000000000000 ) ) ;
#20670 = CARTESIAN_POINT ( 'NONE',  ( 0.9500414927467377701, 0.1787899950787401604, 1.958661417269071947 ) ) ;
#20672 = CARTESIAN_POINT ( 'NONE',  ( 0.8759842519685039353, -0.1787899950787401882, 0.3272637794737956463 ) ) ;
#20673 = VERTEX_POINT ( 'NONE', #19269 ) ;
#20675 = ORIENTED_EDGE ( 'NONE', *, *, #40562, .T. ) ;
#20674 = CARTESIAN_POINT ( 'NONE',  ( -0.1945459183830246241, -0.07553294269955267148, -0.1731116344631301873 ) ) ;
#20676 = EDGE_CURVE ( 'NONE', #21819, #24360, #26728, .T. ) ;
#20677 = DIRECTION ( 'NONE',  ( 1.000000000000000000, 0.000000000000000000, 0.000000000000000000 ) ) ;
#20678 = DIRECTION ( 'NONE',  ( 1.000000000000000000, 0.000000000000000000, 0.000000000000000000 ) ) ;
#20679 = CARTESIAN_POINT ( 'NONE',  ( -0.1787899950787401604, -0.1259842519147404416, -0.07405724077823318263 ) ) ;
#20680 = CARTESIAN_POINT ( 'NONE',  ( 0.9500414927467378812, -0.1787899950787401604, 0.5659448818360001132 ) ) ;
#20681 = CARTESIAN_POINT ( 'NONE',  ( 0.1787899950787401604, -0.8887795275052913224, 0.07405724077823318263 ) ) ;
#20682 = CARTESIAN_POINT ( 'NONE',  ( 0.7593162293221857873, -0.1180121082641624880, 0.03937054915593885679 ) ) ;
#20683 = CARTESIAN_POINT ( 'NONE',  ( -0.9873396505805591694, -0.1113553986120547346, 0.9399606298137322957 ) ) ;
#20684 = EDGE_CURVE ( 'NONE', #8447, #27121, #26002, .T. ) ;
#20685 = CARTESIAN_POINT ( 'NONE',  ( -0.6971942568897648851, 0.07405724077823318263, 1.417322834591906222 ) ) ;
#20686 = ORIENTED_EDGE ( 'NONE', *, *, #37025, .F. ) ;
#20687 = DIRECTION ( 'NONE',  ( 1.822029033848725028E-16, 0.000000000000000000, 1.000000000000000000 ) ) ;
#20688 = CARTESIAN_POINT ( 'NONE',  ( 0.8759842519685039353, -0.1787899950787401882, 1.001476377898992132 ) ) ;
#20689 = CARTESIAN_POINT ( 'NONE',  ( -1.033464566929134687, 0.06523048226347956391, 0.5536417321759372623 ) ) ;
#20690 = CARTESIAN_POINT ( 'NONE',  ( -0.1184675242425147906, -0.09842519685039370636, 1.713085361781125471 ) ) ;
#20691 = CARTESIAN_POINT ( 'NONE',  ( -1.054774247047244096, 0.000000000000000000, 0.8882874015210394658 ) ) ;
#20692 = CARTESIAN_POINT ( 'NONE',  ( -1.033464566929133799, 0.000000000000000000, 0.5118110235145196807 ) ) ;
#20693 = CARTESIAN_POINT ( 'NONE',  ( 1.054774247047244096, 0.000000000000000000, 0.1451771653005673179 ) ) ;
#20694 = CARTESIAN_POINT ( 'NONE',  ( -0.7495606340400177148, -0.1264236179284866091, 0.08612204719033110523 ) ) ;
#20695 = CARTESIAN_POINT ( 'NONE',  ( 0.9412147342319837628, 0.1574803149606300301, 1.345964566821607589 ) ) ;
#20696 = ORIENTED_EDGE ( 'NONE', *, *, #13812, .T. ) ;
#20697 = DIRECTION ( 'NONE',  ( -1.000000000000000000, 0.000000000000000000, 0.000000000000000000 ) ) ;
#20698 = CARTESIAN_POINT ( 'NONE',  ( 0.4330708661417289052, 1.006139616066741879E-16, -1.186023622047243986 ) ) ;
#20699 = CARTESIAN_POINT ( 'NONE',  ( -0.6971942568897648851, 0.07405724077823318263, 1.732283464513166615 ) ) ;
#20700 = EDGE_LOOP ( 'NONE', ( #29959, #30649, #9520, #10256 ) ) ;
#20701 = AXIS2_PLACEMENT_3D ( 'NONE', #34605, #23346, #23806 ) ;
#20702 = CARTESIAN_POINT ( 'NONE',  ( -0.2471922904502826535, 0.09442133267706682986, -0.03395025085956321353 ) ) ;
#20703 = CARTESIAN_POINT ( 'NONE',  ( -0.8759842519685039353, -0.1574803149606299191, 0.7874015748031496509 ) ) ;
#20704 = CARTESIAN_POINT ( 'NONE',  ( -0.07405724077823318263, -1.126108220197742371, -0.1787899950787401604 ) ) ;
#20705 = ORIENTED_EDGE ( 'NONE', *, *, #39094, .T. ) ;
#20706 = CARTESIAN_POINT ( 'NONE',  ( 0.1787899950787401604, -0.05708661411946481384, -0.07405724077823318263 ) ) ;
#20708 = EDGE_LOOP ( 'NONE', ( #25021, #29416, #42752, #14346 ) ) ;
#20707 = B_SPLINE_CURVE_WITH_KNOTS ( 'NONE', 3,
 ( #13563, #21452, #17868, #10937, #6601, #35845, #32511, #28198, #28688, #17387, #14287, #39896 ),
 .UNSPECIFIED., .F., .F.,
 ( 4, 2, 2, 2, 2, 4 ),
 ( 0.000000000000000000, 0.2500000000000009437, 0.3750000000000012212, 0.4375000000000013323, 0.5000000000000013323, 1.000000000000000000 ),
 .UNSPECIFIED. ) ;
#20709 = ORIENTED_EDGE ( 'NONE', *, *, #17582, .T. ) ;
#20710 = EDGE_CURVE ( 'NONE', #36693, #37979, #14994, .T. ) ;
#20711 = CARTESIAN_POINT ( 'NONE',  ( 0.9412147342319837628, 0.1574803149606300301, 1.739665354223181470 ) ) ;
#20712 = CARTESIAN_POINT ( 'NONE',  ( -1.033464566929133799, 1.928577636452524610E-17, 2.869337061179095023E-17 ) ) ;
#20713 = CARTESIAN_POINT ( 'NONE',  ( 0.8107537697050253289, 0.1574803149606300301, 1.793799212598424342 ) ) ;
#20714 = EDGE_CURVE ( 'NONE', #8512, #24150, #11631, .T. ) ;
#20715 = CARTESIAN_POINT ( 'NONE',  ( 0.1797182628040039087, -0.1363627072208409285, -0.07444174185955065859 ) ) ;
#20716 = CARTESIAN_POINT ( 'NONE',  ( -0.7185039370078739607, 1.928577636452523993E-17, 1.053149606299212504 ) ) ;
#20717 = MANIFOLD_SOLID_BREP ( 'Base Plate', #14804 ) ;
#20718 = CARTESIAN_POINT ( 'NONE',  ( 0.1797182628040039087, -1.238724911945250362, -0.07444174185955065859 ) ) ;
#20719 = DIRECTION ( 'NONE',  ( 0.000000000000000000, -1.000000000000000000, 0.000000000000000000 ) ) ;
#20720 = CARTESIAN_POINT ( 'NONE',  ( 1.054774247047244096, 0.000000000000000000, 1.011318897584031484 ) ) ;
#20721 = CARTESIAN_POINT ( 'NONE',  ( 0.7495606340400177148, -0.1264236179284866091, 1.582185039316315045 ) ) ;
#20722 = VECTOR ( 'NONE', #9746, 39.37007874015748143 ) ;
#20723 = CARTESIAN_POINT ( 'NONE',  ( 0.9873396505805591694, 0.1113553986120547346, 1.668307086614173373 ) ) ;
#20725 = CARTESIAN_POINT ( 'NONE',  ( 0.000000000000000000, -0.09842519685039370636, 0.000000000000000000 ) ) ;
#20724 = CARTESIAN_POINT ( 'NONE',  ( 0.8314579112631774738, 0.1526854885466115419, 1.979225999458145813 ) ) ;
#20727 = CARTESIAN_POINT ( 'NONE',  ( 0.1634463026673921293, -0.08033096794652530570, -0.1391362646951039561 ) ) ;
#20726 = CONICAL_SURFACE ( 'NONE', #18445, 0.1377952755905509363, 0.9599310885968936891 ) ;
#20728 = CARTESIAN_POINT ( 'NONE',  ( 0.7646288533564489232, 0.1113553986120547346, 0.6840551180027086842 ) ) ;
#20729 = CARTESIAN_POINT ( 'NONE',  ( 2.892866454678787531E-17, -0.7165354329633386588, 0.1574803149606299191 ) ) ;
#20730 = CARTESIAN_POINT ( 'NONE',  ( -1.033464566929133799, 0.000000000000000000, 1.653543306979086580 ) ) ;
#20731 = CARTESIAN_POINT ( 'NONE',  ( -1.094772975963752103E-17, -0.01033464561552785432, -0.1787899950787401882 ) ) ;
#20732 = DIRECTION ( 'NONE',  ( 1.000000000000000000, 0.000000000000000000, -1.822029033848725275E-16 ) ) ;
#20733 = CARTESIAN_POINT ( 'NONE',  ( 0.6971942568897648851, -0.07405724077823297447, 1.067913385773007651 ) ) ;
#20734 = CARTESIAN_POINT ( 'NONE',  ( -0.6195511811023656223, 1.354170115732555191, -0.4197102375732078561 ) ) ;
#20735 = CARTESIAN_POINT ( 'NONE',  ( 0.8759842519685039353, -0.1574803149606299191, 0.5413385825696385156 ) ) ;
#20736 = ORIENTED_EDGE ( 'NONE', *, *, #37998, .T. ) ;
#20737 = CARTESIAN_POINT ( 'NONE',  ( 0.2642359194686346169, 4.766607801171850497E-17, 0.000000000000000000 ) ) ;
#20738 = CARTESIAN_POINT ( 'NONE',  ( 0.9873396505805591694, 0.1113553986120547346, 0.2509842519685039353 ) ) ;
#20739 = CARTESIAN_POINT ( 'NONE',  ( -0.9412147342319837628, 0.1574803149606300301, 0.2829724408373550104 ) ) ;
#20740 = ORIENTED_EDGE ( 'NONE', *, *, #1082, .T. ) ;
#20741 = CARTESIAN_POINT ( 'NONE',  ( 0.8759842519685039353, -0.1787899950787401882, 1.232775590497417362 ) ) ;
#20743 = DIRECTION ( 'NONE',  ( -1.000000000000000000, 0.000000000000000000, 0.000000000000000000 ) ) ;
#20742 = FACE_OUTER_BOUND ( 'NONE', #10692, .T. ) ;
#20744 = CARTESIAN_POINT ( 'NONE',  ( -0.1264236179284866091, -0.07431102356828367395, 0.1264236179284866091 ) ) ;
#20745 = CARTESIAN_POINT ( 'NONE',  ( 0.8759842519685039353, 0.1574803149606299191, 0.4429133857192448787 ) ) ;
#20746 = ORIENTED_EDGE ( 'NONE', *, *, #1075, .F. ) ;
#20747 = CARTESIAN_POINT ( 'NONE',  ( 0.1350291203832761910, 0.09842519685039370636, 0.2074739718644189046 ) ) ;
#20748 = LINE ( 'NONE', #12882, #17721 ) ;
#20749 = ORIENTED_EDGE ( 'NONE', *, *, #35980, .F. ) ;
#20750 = CARTESIAN_POINT ( 'NONE',  ( -1.054774247047244540, -0.07405724077823318263, 1.358267716481669662 ) ) ;
#20751 = CARTESIAN_POINT ( 'NONE',  ( -1.094772975963752103E-17, -1.747539370024976391, -0.1787899950787401882 ) ) ;
#20752 = CARTESIAN_POINT ( 'NONE',  ( -0.8759842519685039353, 0.1787899950787401882, 0.9817913385289134265 ) ) ;
#20753 = CARTESIAN_POINT ( 'NONE',  ( -1.054774247047244540, 0.07405724077823318263, 1.914370078686394860 ) ) ;
#20754 = ORIENTED_EDGE ( 'NONE', *, *, #37158, .F. ) ;
#20755 = CARTESIAN_POINT ( 'NONE',  ( -0.7495606340400177148, -0.1264236179284866091, 0.6422244093950550958 ) ) ;
#20756 = CIRCLE ( 'NONE', #34558, 0.2007874015748031815 ) ;
#20757 = CARTESIAN_POINT ( 'NONE',  ( 0.1574803149606299191, 0.1200787401574803237, 2.850509043694854679E-09 ) ) ;
#20758 = CARTESIAN_POINT ( 'NONE',  ( -0.9412147342319837628, 0.1574803149606300301, 0.08612204713656733401 ) ) ;
#20759 = ORIENTED_EDGE ( 'NONE', *, *, #36313, .T. ) ;
#20760 = CARTESIAN_POINT ( 'NONE',  ( -1.033464566929133799, 0.000000000000000000, 1.456692913278299084 ) ) ;
#20761 = LINE ( 'NONE', #43029, #2683 ) ;
#20762 = ORIENTED_EDGE ( 'NONE', *, *, #9766, .F. ) ;
#20763 = CARTESIAN_POINT ( 'NONE',  ( 0.1237557312196567866, 1.170665729134807931, -0.1030065087509293015 ) ) ;
#20764 = VECTOR ( 'NONE', #35646, 39.37007874015748143 ) ;
#20765 = AXIS2_PLACEMENT_3D ( 'NONE', #113, #35624, #2998 ) ;
#20766 = EDGE_CURVE ( 'NONE', #22060, #23610, #45009, .T. ) ;
#20767 = DIRECTION ( 'NONE',  ( 0.000000000000000000, -1.000000000000000000, 0.000000000000000000 ) ) ;
#20768 = CARTESIAN_POINT ( 'NONE',  ( -0.8019270111902717657, -0.1787899950787401604, 0.6397637794737947026 ) ) ;
#20769 = CARTESIAN_POINT ( 'NONE',  ( 0.7185039370078739607, 1.928577636452523993E-17, 1.358267716427907779 ) ) ;
#20770 = EDGE_CURVE ( 'NONE', #13680, #12253, #31569, .T. ) ;
#20771 = ORIENTED_EDGE ( 'NONE', *, *, #37662, .F. ) ;
#20772 = EDGE_CURVE ( 'NONE', #43655, #44249, #27974, .T. ) ;
#20773 = ADVANCED_FACE ( 'NONE', ( #23892 ), #16468, .T. ) ;
#20774 = CARTESIAN_POINT ( 'NONE',  ( 0.000000000000000000, 0.000000000000000000, 0.09842519685039370636 ) ) ;
#20775 = CARTESIAN_POINT ( 'NONE',  ( -0.9412147342319837628, -0.1574803149606297803, 0.1894685038294807999 ) ) ;
#20776 = ORIENTED_EDGE ( 'NONE', *, *, #35537, .F. ) ;
#20777 = CARTESIAN_POINT ( 'NONE',  ( 0.8759842519685039353, 0.1574803149606299191, 0.6102362204724409711 ) ) ;
#20778 = CARTESIAN_POINT ( 'NONE',  ( 0.8107537697050254399, 0.1574803149606300301, 0.6422244093412927679 ) ) ;
#20779 = CARTESIAN_POINT ( 'NONE',  ( 1.054774247047244096, 0.000000000000000000, 0.6569881889226141247 ) ) ;
#20781 = DIRECTION ( 'NONE',  ( -1.000000000000000000, -5.372880794957750686E-15, 4.197754538034109710E-15 ) ) ;
#20780 = CARTESIAN_POINT ( 'NONE',  ( -0.1574803149606300301, -0.5418307086614178036, -0.06523048226347956391 ) ) ;
#20782 = CARTESIAN_POINT ( 'NONE',  ( -0.1518774605348951201, 0.1248780621282413877, -0.05777686690714941425 ) ) ;
#20783 = ORIENTED_EDGE ( 'NONE', *, *, #251, .F. ) ;
#20784 = CARTESIAN_POINT ( 'NONE',  ( 0.2395294000716134131, 3.218313930830148909E-16, -1.043307086614172929 ) ) ;
#20785 = CARTESIAN_POINT ( 'NONE',  ( 0.8107537697050253289, 0.1574803149606300301, 1.203248031496062520 ) ) ;
#20786 = CARTESIAN_POINT ( 'NONE',  ( 0.3649999999999999911, 3.414809992080327174E-17, 0.000000000000000000 ) ) ;
#20787 = CARTESIAN_POINT ( 'NONE',  ( 0.8107537697050254399, -0.1574803149606297803, 1.847933070866142780 ) ) ;
#20788 = ( BOUNDED_CURVE ( )  B_SPLINE_CURVE ( 2, ( #11440, #38480, #9008, #1813, #12863, #5651, #41809, #19556, #20261 ),
 .UNSPECIFIED., .F., .T. ) 
 B_SPLINE_CURVE_WITH_KNOTS ( ( 3, 2, 2, 2, 3 ),
 ( 0.2099999999999999922, 0.2124999999999999944, 0.2149999999999999967, 0.2174999999999999989, 0.2200000000000000011 ),
 .UNSPECIFIED. ) 
 CURVE ( )  GEOMETRIC_REPRESENTATION_ITEM ( )  RATIONAL_B_SPLINE_CURVE ( ( 1.000000000000000000, 0.9238795325112869605, 1.000000000000000000, 0.9238795325112869605, 1.000000000000000000, 0.9238795325112869605, 1.000000000000000000, 0.9238795325112869605, 1.000000000000000000 ) ) 
 REPRESENTATION_ITEM ( '' )  ) ;
#20789 = EDGE_LOOP ( 'NONE', ( #6661, #1779, #39270, #30666 ) ) ;
#20791 = FACE_OUTER_BOUND ( 'NONE', #3845, .T. ) ;
#20790 = CARTESIAN_POINT ( 'NONE',  ( 0.6971942568897648851, 0.07405724077823318263, 0.7480314960092282472 ) ) ;
#20792 = CARTESIAN_POINT ( 'NONE',  ( -0.1476377952755905387, -0.4872761608334559846, -0.8688576204587790119 ) ) ;
#20793 = LINE ( 'NONE', #27324, #3909 ) ;
#20794 = DIRECTION ( 'NONE',  ( 0.000000000000000000, 0.000000000000000000, 1.000000000000000000 ) ) ;
#20795 = CARTESIAN_POINT ( 'NONE',  ( 0.1099100077094851968, 0.1299212598425196763, 0.1429462536667461814 ) ) ;
#20796 = AXIS2_PLACEMENT_3D ( 'NONE', #7046, #33193, #46816 ) ;
#20798 = CARTESIAN_POINT ( 'NONE',  ( 7.107660667884922897E-05, 0.1159713038039417443, -0.07472206960542350507 ) ) ;
#20797 = AXIS2_PLACEMENT_3D ( 'NONE', #12815, #23580, #5598 ) ;
#20799 = CARTESIAN_POINT ( 'NONE',  ( 1.054774247047244540, 0.07405724077823318263, 0.8907480314422986378 ) ) ;
#20800 = FACE_OUTER_BOUND ( 'NONE', #202, .T. ) ;
#20801 = CARTESIAN_POINT ( 'NONE',  ( -0.7646288533564489232, 0.1113553986120547346, 0.5364173228346457156 ) ) ;
#20802 = CARTESIAN_POINT ( 'NONE',  ( -0.1270800023317771588, 0.1121609148264033490, -0.1270800023317771588 ) ) ;
#20803 = CARTESIAN_POINT ( 'NONE',  ( -1.094772975963752103E-17, -0.9995078739619842612, -0.1787899950787401882 ) ) ;
#20804 = CARTESIAN_POINT ( 'NONE',  ( -0.06523048226347956391, -1.398129921259843478, 0.1574803149606297803 ) ) ;
#20805 = CARTESIAN_POINT ( 'NONE',  ( 0.9873396505805591694, 0.1113553986120547346, 1.225393700679874076 ) ) ;
#20806 = CARTESIAN_POINT ( 'NONE',  ( 0.1563805530828639712, 0.1078949188770173262, -0.09388986751133071573 ) ) ;
#20807 = ADVANCED_FACE ( 'NONE', ( #45664 ), #33012, .T. ) ;
#20808 = CARTESIAN_POINT ( 'NONE',  ( -1.054774247047244096, 0.000000000000000000, 1.838090551127338657 ) ) ;
#20809 = CARTESIAN_POINT ( 'NONE',  ( -0.9412147342319837628, -0.1574803149606297803, 0.8193897636719996713 ) ) ;
#20810 = EDGE_LOOP ( 'NONE', ( #40845, #18150 ) ) ;
#20811 = CARTESIAN_POINT ( 'NONE',  ( -9.642888182262618425E-18, -1.405511810916094451, -0.1574803149606299191 ) ) ;
#20812 = CARTESIAN_POINT ( 'NONE',  ( -0.6971942568897648851, -0.07405724077823297447, 1.899606299158834943 ) ) ;
#20813 = CARTESIAN_POINT ( 'NONE',  ( -0.8759842519685039353, -0.1787899950787401882, 1.508366141678519678 ) ) ;
#20814 = CARTESIAN_POINT ( 'NONE',  ( 0.06197108496688099460, 0.2597152231171855341, -0.3085539532670620311 ) ) ;
#20815 = CARTESIAN_POINT ( 'NONE',  ( -1.054774247047244540, 0.07405724077823318263, 1.008858267662772423 ) ) ;
#20816 = CARTESIAN_POINT ( 'NONE',  ( -0.8019270111902717657, 0.1787899950787401604, 0.1968503936470238913 ) ) ;
#20817 = ( BOUNDED_CURVE ( )  B_SPLINE_CURVE ( 2, ( #25747, #39848, #47051, #21898, #7037, #10417, #25017, #21663, #36521 ),
 .UNSPECIFIED., .F., .T. ) 
 B_SPLINE_CURVE_WITH_KNOTS ( ( 3, 2, 2, 2, 3 ),
 ( 0.6600000000000000311, 0.6624999999999999778, 0.6650000000000000355, 0.6674999999999999822, 0.6700000000000000400 ),
 .UNSPECIFIED. ) 
 CURVE ( )  GEOMETRIC_REPRESENTATION_ITEM ( )  RATIONAL_B_SPLINE_CURVE ( ( 1.000000000000000000, 0.9238795325112869605, 1.000000000000000000, 0.9238795325112869605, 1.000000000000000000, 0.9238795325112869605, 1.000000000000000000, 0.9238795325112869605, 1.000000000000000000 ) ) 
 REPRESENTATION_ITEM ( '' )  ) ;
#20818 = CARTESIAN_POINT ( 'NONE',  ( -0.1768440709656272092, 0.08559642391439407916, -0.1833320988895476844 ) ) ;
#20819 = CARTESIAN_POINT ( 'NONE',  ( -0.7495606340400177148, 0.1264236179284866091, 1.970964566875370139 ) ) ;
#20820 = CARTESIAN_POINT ( 'NONE',  ( -0.8759842519685039353, 0.1574803149606299191, 1.830708661417322913 ) ) ;
#20821 = DIRECTION ( 'NONE',  ( -1.000000000000000000, 0.000000000000000000, 0.000000000000000000 ) ) ;
#20822 = CARTESIAN_POINT ( 'NONE',  ( -0.1787899950787401604, -0.2107538894890813030, 0.07405724077823318263 ) ) ;
#20823 = CARTESIAN_POINT ( 'NONE',  ( 0.09661541192592146277, -0.09842519685039370636, 0.1970456418925724540 ) ) ;
#20824 = CARTESIAN_POINT ( 'NONE',  ( 0.000000000000000000, 0.3883517482604913473, -0.6419475548153091848 ) ) ;
#20825 = AXIS2_PLACEMENT_3D ( 'NONE', #24740, #28121, #10857 ) ;
#20826 = EDGE_CURVE ( 'NONE', #24150, #17791, #38740, .T. ) ;
#20827 = CIRCLE ( 'NONE', #19290, 0.09842519685039370636 ) ;
#20828 = ORIENTED_EDGE ( 'NONE', *, *, #43207, .F. ) ;
#20829 = ORIENTED_EDGE ( 'NONE', *, *, #106, .F. ) ;
#20830 = VECTOR ( 'NONE', #18532, 39.37007874015748854 ) ;
#20831 = AXIS2_PLACEMENT_3D ( 'NONE', #1761, #2234, #34373 ) ;
#20832 = EDGE_CURVE ( 'NONE', #26918, #873, #46387, .T. ) ;
#20833 = CARTESIAN_POINT ( 'NONE',  ( 0.1264236179284866091, -1.043799212544661348, -0.1264236179284866091 ) ) ;
#20834 = CARTESIAN_POINT ( 'NONE',  ( 0.1264236179284866091, -1.156988188922614125, -0.1264236179284866091 ) ) ;
#20835 = FACE_BOUND ( 'NONE', #24139, .T. ) ;
#20836 = LENGTH_MEASURE_WITH_UNIT ( LENGTH_MEASURE( 0.02539999999999999897 ), #39735 ) ;
#20837 = CARTESIAN_POINT ( 'NONE',  ( 0.07444174185955046430, -0.5645123135200530440, -0.1797182628040039087 ) ) ;
#20838 = DIRECTION ( 'NONE',  ( -1.000000000000000000, 0.000000000000000000, 0.000000000000000000 ) ) ;
#20839 = CARTESIAN_POINT ( 'NONE',  ( -1.033464566929134687, 0.06523048226347956391, 0.7504921258767240921 ) ) ;
#20840 = CARTESIAN_POINT ( 'NONE',  ( -0.7646288533564489232, 0.1113553986120547346, 0.7726377952755906220 ) ) ;
#20841 = CARTESIAN_POINT ( 'NONE',  ( -0.1113553986120547346, -0.06200787401574803237, 0.1113553986120547346 ) ) ;
#20842 = CARTESIAN_POINT ( 'NONE',  ( 1.033464566929134687, -0.06523048226347956391, 0.7554133858267707557 ) ) ;
#20843 = CARTESIAN_POINT ( 'NONE',  ( 0.1404189863467218691, -0.2144232926957947427, -0.02742975588281126517 ) ) ;
#20844 = CARTESIAN_POINT ( 'NONE',  ( -0.8107537697050254399, 0.1574803149606300301, 1.085137795275590955 ) ) ;
#20846 = CARTESIAN_POINT ( 'NONE',  ( 0.1644020957507539848, -0.08115590401245571794, -0.1405661490837558925 ) ) ;
#20845 = CARTESIAN_POINT ( 'NONE',  ( 0.08985779549332124916, 0.2436148098455510058, -0.03544556188504843774 ) ) ;
#20847 = CARTESIAN_POINT ( 'NONE',  ( 0.9412147342319837628, -0.1574803149606297803, 0.1107283463491660208 ) ) ;
#20848 = EDGE_LOOP ( 'NONE', ( #38883, #9157, #25480, #14705 ) ) ;
#20849 = ORIENTED_EDGE ( 'NONE', *, *, #40550, .F. ) ;
#20850 = CARTESIAN_POINT ( 'NONE',  ( -0.6195511811023656223, 0.000000000000000000, 1.186023622047243986 ) ) ;
#20851 = CARTESIAN_POINT ( 'NONE',  ( -0.1787899950787401604, -0.5196850393163150450, -0.07405724077823318263 ) ) ;
#20852 = CARTESIAN_POINT ( 'NONE',  ( -0.1264236179284866091, -1.412893700733637958, 0.1264236179284866091 ) ) ;
#20853 = AXIS2_PLACEMENT_3D ( 'NONE', #8188, #41222, #16120 ) ;
#20854 = VERTEX_POINT ( 'NONE', #16927 ) ;
#20855 = CARTESIAN_POINT ( 'NONE',  ( -0.6971942568897648851, 0.07405724077823318263, 1.422244094434426120 ) ) ;
#20856 = CARTESIAN_POINT ( 'NONE',  ( 0.8759842519685039353, -0.1787899950787401882, 1.513287401521039355 ) ) ;
#20857 = ORIENTED_EDGE ( 'NONE', *, *, #23701, .T. ) ;
#20858 = CARTESIAN_POINT ( 'NONE',  ( 0.7185039370078746268, -0.06523048226347956391, 0.9276574802074332160 ) ) ;
#20859 = CARTESIAN_POINT ( 'NONE',  ( -1.002407869896990045, -0.1264236179284866091, 0.5733267715997795166 ) ) ;
#20860 = AXIS2_PLACEMENT_3D ( 'NONE', #25692, #32652, #10835 ) ;
#20861 = CONICAL_SURFACE ( 'NONE', #2495, 0.1567662409572586624, 0.9599310885969887241 ) ;
#20862 = CARTESIAN_POINT ( 'NONE',  ( 0.8759842519685039353, -0.1787899950787401882, 0.1353346456155279653 ) ) ;
#20863 = CARTESIAN_POINT ( 'NONE',  ( 1.054774247047244540, 0.07405724077823318263, 0.6594488188438737408 ) ) ;
#20864 = CARTESIAN_POINT ( 'NONE',  ( -1.054774247047244540, 0.07405724077823318263, 0.5364173227808820554 ) ) ;
#20865 = CARTESIAN_POINT ( 'NONE',  ( 0.000000000000000000, 0.000000000000000000, -0.3149606299212598381 ) ) ;
#20866 = PLANE ( 'NONE',  #41257 ) ;
#20867 = VERTEX_POINT ( 'NONE', #46153 ) ;
#20868 = PRODUCT_DEFINITION_SHAPE ( 'NONE', 'NONE',  #1359 ) ;
#20869 = CARTESIAN_POINT ( 'NONE',  ( -0.8759842519685039353, -0.1787899950787401882, 1.395177165300567124 ) ) ;
#20870 = CARTESIAN_POINT ( 'NONE',  ( -1.033464566929134687, -0.06523048226347956391, 1.464074803149607140 ) ) ;
#20871 = AXIS2_PLACEMENT_3D ( 'NONE', #34733, #4098, #19851 ) ;
#20872 = CARTESIAN_POINT ( 'NONE',  ( -0.7185039370078746268, 0.06523048226347956391, 0.4995078740157484765 ) ) ;
#20873 = CARTESIAN_POINT ( 'NONE',  ( 0.8019270111902716547, 0.1787899950787401604, 1.377952755851748368 ) ) ;
#20874 = CARTESIAN_POINT ( 'NONE',  ( -0.1855074086109543274, -0.09851385092611850136, 0.1431435806659169252 ) ) ;
#20875 = ORIENTED_EDGE ( 'NONE', *, *, #27637, .T. ) ;
#20876 = DIRECTION ( 'NONE',  ( 0.000000000000000000, -2.355041373848501170E-15, 1.000000000000000000 ) ) ;
#20877 = EDGE_CURVE ( 'NONE', #11036, #21900, #20748, .T. ) ;
#20878 = CARTESIAN_POINT ( 'NONE',  ( -0.07405724077823318263, -1.637919243819790704, -0.1787899950787401604 ) ) ;
#20879 = ORIENTED_EDGE ( 'NONE', *, *, #12750, .T. ) ;
#20880 = LINE ( 'NONE', #36174, #33470 ) ;
#20881 = CARTESIAN_POINT ( 'NONE',  ( -0.1264236179284866091, -0.6353346456155275490, -0.1264236179284866091 ) ) ;
#20882 = CARTESIAN_POINT ( 'NONE',  ( 1.033464566929136907, -0.06523048226347749612, 1.621555118110237670 ) ) ;
#20883 = DIRECTION ( 'NONE',  ( -1.000000000000000000, 0.000000000000000000, 0.000000000000000000 ) ) ;
#20884 = ORIENTED_EDGE ( 'NONE', *, *, #27375, .F. ) ;
#20885 = CARTESIAN_POINT ( 'NONE',  ( 0.6971942568897648851, 0.07405724077823318263, 1.417322834591906222 ) ) ;
#20886 = EDGE_CURVE ( 'NONE', #6712, #9090, #2072, .T. ) ;
#20887 = CARTESIAN_POINT ( 'NONE',  ( 0.07405724077823318263, -0.3474409448281265411, 0.1787899950787401604 ) ) ;
#20888 = CARTESIAN_POINT ( 'NONE',  ( 0.1264236179284866091, -0.8124999999462361178, 0.1264236179284866091 ) ) ;
#20889 = CONICAL_SURFACE ( 'NONE', #20825, 0.08090551181102362266, 0.9599310885968742602 ) ;
#20890 = LINE ( 'NONE', #12555, #45538 ) ;
#20891 = FACE_OUTER_BOUND ( 'NONE', #11025, .T. ) ;
#20892 = CARTESIAN_POINT ( 'NONE',  ( 0.9500414927467378812, -0.1787899950787401604, 0.3297244093950552069 ) ) ;
#20893 = CARTESIAN_POINT ( 'NONE',  ( 1.033464566929133799, 0.000000000000000000, 1.062992125876724314 ) ) ;
#20894 = VECTOR ( 'NONE', #39276, 39.37007874015748143 ) ;
#20895 = CARTESIAN_POINT ( 'NONE',  ( -0.1787899950787401604, -0.2342519684501733479, 0.07405724077823318263 ) ) ;
#20896 = CARTESIAN_POINT ( 'NONE',  ( 0.1264236179284866091, 0.09793307091990532953, -0.1264236179284866091 ) ) ;
#20897 = PLANE ( 'NONE',  #33382 ) ;
#20898 = AXIS2_PLACEMENT_3D ( 'NONE', #44193, #25780, #3943 ) ;
#20899 = CARTESIAN_POINT ( 'NONE',  ( -1.054774247047244096, 0.000000000000000000, 0.7750984251430865779 ) ) ;
#20900 = CARTESIAN_POINT ( 'NONE',  ( 0.06523048226347956391, -0.8420275590551181688, 0.1574803149606297803 ) ) ;
#20901 = CARTESIAN_POINT ( 'NONE',  ( 0.07444174185955046430, -1.784984754464935541, -0.1797182628040039087 ) ) ;
#20902 = CARTESIAN_POINT ( 'NONE',  ( -0.1787899950787401882, -0.3548228345919058890, 0.000000000000000000 ) ) ;
#20903 = DIRECTION ( 'NONE',  ( 0.000000000000000000, 0.000000000000000000, -1.000000000000000000 ) ) ;
#20904 = CARTESIAN_POINT ( 'NONE',  ( 1.054774247047244540, 0.07405724077823318263, 1.722440944828125930 ) ) ;
#20906 = CARTESIAN_POINT ( 'NONE',  ( 0.1631287632119293174, 0.1603246647599305685, 4.966163489190320679E-07 ) ) ;
#20905 = CARTESIAN_POINT ( 'NONE',  ( 0.8759842519685039353, 0.1787899950787401882, 1.961122047190330786 ) ) ;
#20907 = CARTESIAN_POINT ( 'NONE',  ( 0.8019270111902716547, -0.1787899950787401604, 0.4035433070328507954 ) ) ;
#20908 = EDGE_LOOP ( 'NONE', ( #38815, #7383, #9685, #32051 ) ) ;
#20909 = DIRECTION ( 'NONE',  ( 0.000000000000000000, 0.000000000000000000, 1.000000000000000000 ) ) ;
#20910 = CARTESIAN_POINT ( 'NONE',  ( 0.8759842519685039353, 0.000000000000000000, 4.498031496062992574 ) ) ;
#20911 = CARTESIAN_POINT ( 'NONE',  ( 0.07405724077823318263, -0.1112204723871813017, 0.1787899950787401604 ) ) ;
#20912 = CARTESIAN_POINT ( 'NONE',  ( 0.6971942568897626646, -0.07405724077823297447, 0.5561023621509617598 ) ) ;
#20913 = EDGE_CURVE ( 'NONE', #40723, #7704, #45434, .T. ) ;
#20914 = CARTESIAN_POINT ( 'NONE',  ( -0.1787899950787401604, -0.8690944881352120621, -0.07405724077823318263 ) ) ;
#20915 = CARTESIAN_POINT ( 'NONE',  ( 0.9412147342319837628, -0.1574803149606297803, 0.08120078740157483932 ) ) ;
#20916 = CARTESIAN_POINT ( 'NONE',  ( -0.7185039370078766252, -0.06523048226348168721, 1.518208661309796481 ) ) ;
#20917 = CARTESIAN_POINT ( 'NONE',  ( -1.054774247047244540, 0.07405724077823318263, 1.441929133804504604 ) ) ;
#20918 = VERTEX_POINT ( 'NONE', #28200 ) ;
#20919 = CARTESIAN_POINT ( 'NONE',  ( -0.3052312982475722247, -0.05465342266228452595, -0.7177420118880897260 ) ) ;
#20920 = CARTESIAN_POINT ( 'NONE',  ( 0.8019270111902717657, -0.1787899950787401604, 1.156496062938362046 ) ) ;
#20921 = CARTESIAN_POINT ( 'NONE',  ( -0.8107537697050253289, -0.1574803149606297803, 0.6569881888688503535 ) ) ;
#20922 = CARTESIAN_POINT ( 'NONE',  ( 1.054774247047244096, 0.000000000000000000, 1.872539370024976391 ) ) ;
#20923 = CARTESIAN_POINT ( 'NONE',  ( -0.7185039370078746268, 0.06523048226347956391, 1.444389763779527991 ) ) ;
#20924 = CARTESIAN_POINT ( 'NONE',  ( -0.8759842519685039353, 0.1787899950787401882, 0.8981299212060788184 ) ) ;
#20925 = CARTESIAN_POINT ( 'NONE',  ( -0.1184675242425147629, 0.3740157480314960647, 1.224299699984020551 ) ) ;
#20926 = CARTESIAN_POINT ( 'NONE',  ( -0.8212486197303469071, -0.1522654806920532289, 0.03937007874015844427 ) ) ;
#20927 = CARTESIAN_POINT ( 'NONE',  ( 1.002407869896990045, 0.1264236179284866091, 0.07135826766277185429 ) ) ;
#20928 = CARTESIAN_POINT ( 'NONE',  ( 0.7185039370078739607, 1.928577636452523993E-17, 1.555118110128692832 ) ) ;
#20929 = VERTEX_POINT ( 'NONE', #30872 ) ;
#20930 = CARTESIAN_POINT ( 'NONE',  ( 0.5717220857807087109, 4.466152701071653354E-17, 0.000000000000000000 ) ) ;
#20931 = DIRECTION ( 'NONE',  ( -0.8660254037844389297, -1.060575238724907285E-16, -0.4999999999999994449 ) ) ;
#20932 = ORIENTED_EDGE ( 'NONE', *, *, #1297, .T. ) ;
#20933 = ORIENTED_EDGE ( 'NONE', *, *, #24423, .T. ) ;
#20934 = CARTESIAN_POINT ( 'NONE',  ( -0.7495606340400177148, -0.1264236179284866091, 1.621555118056472455 ) ) ;
#20935 = ADVANCED_FACE ( 'NONE', ( #42068 ), #9272, .T. ) ;
#20936 = CARTESIAN_POINT ( 'NONE',  ( -0.1377952755905511861, 0.1564960629921283985, 0.8070866141732283561 ) ) ;
#20937 = CARTESIAN_POINT ( 'NONE',  ( 0.5057057357416000487, 4.766607801171850497E-17, 0.000000000000000000 ) ) ;
#20938 = CARTESIAN_POINT ( 'NONE',  ( 3.284318927891251994E-17, -1.148253889489080803, 0.1787899950787401882 ) ) ;
#20939 = AXIS2_PLACEMENT_3D ( 'NONE', #15619, #40502, #15375 ) ;
#20940 = ORIENTED_EDGE ( 'NONE', *, *, #35921, .T. ) ;
#20941 = CARTESIAN_POINT ( 'NONE',  ( -1.094772975963752103E-17, -0.04970472435568527164, -0.1787899950787401882 ) ) ;
#20942 = CARTESIAN_POINT ( 'NONE',  ( 1.054774247047244096, 0.000000000000000000, 1.085137795221826629 ) ) ;
#20943 = EDGE_CURVE ( 'NONE', #6112, #2820, #25758, .T. ) ;
#20944 = CARTESIAN_POINT ( 'NONE',  ( 0.2395294000716133853, -0.1968503937007874127, 0.4921259842519685179 ) ) ;
#20945 = DIRECTION ( 'NONE',  ( 3.469446951953613794E-15, 1.000000000000000000, 0.000000000000000000 ) ) ;
#20946 = CARTESIAN_POINT ( 'NONE',  ( 0.8759842519685039353, 0.1574803149606299191, 1.870078740157480324 ) ) ;
#20947 = CARTESIAN_POINT ( 'NONE',  ( -0.6971942568897648851, -0.07405724077823297447, 0.3641732282926931630 ) ) ;
#20948 = MANIFOLD_SOLID_BREP ( 'Pivot Pin', #45396 ) ;
#20949 = CARTESIAN_POINT ( 'NONE',  ( -1.100456976456230270E-17, -1.270713100921627703, -0.1797182628040039365 ) ) ;
#20950 = CARTESIAN_POINT ( 'NONE',  ( 0.5555748031496077211, 2.215965818540671970E-15, 0.7480314960629921295 ) ) ;
#20951 = CARTESIAN_POINT ( 'NONE',  ( 0.6971942568897648851, -0.07405724077823297447, 1.112204724355684959 ) ) ;
#20952 = CARTESIAN_POINT ( 'NONE',  ( 1.054774247047244096, 0.000000000000000000, 1.596948818843874074 ) ) ;
#20954 = CARTESIAN_POINT ( 'NONE',  ( 0.8107537697050254399, 0.1574803149606300301, 1.715059055118110631 ) ) ;
#20953 = CARTESIAN_POINT ( 'NONE',  ( 0.1554368334888477088, 0.02742154311898540794, 0.1377952755905511584 ) ) ;
#20955 = CARTESIAN_POINT ( 'NONE',  ( 1.033464566929133799, 0.000000000000000000, 0.7874015746956221085 ) ) ;
#20956 = CARTESIAN_POINT ( 'NONE',  ( -0.7646288533564489232, -0.1113553986120547346, 1.796259842412157415 ) ) ;
#20957 = CARTESIAN_POINT ( 'NONE',  ( -0.1787899950787401604, 0.03641732288840918152, -0.07405724077823318263 ) ) ;
#20958 = CARTESIAN_POINT ( 'NONE',  ( 1.002407869896990045, 0.1264236179284866091, 0.1845472440407248116 ) ) ;
#20959 = DIRECTION ( 'NONE',  ( 0.000000000000000000, 0.000000000000000000, -1.000000000000000000 ) ) ;
#20961 = CARTESIAN_POINT ( 'NONE',  ( -0.7185039370078739607, 1.928577636452523993E-17, 1.958661417322834719 ) ) ;
#20960 = CARTESIAN_POINT ( 'NONE',  ( 0.6971942568897648851, -0.07405724077823297447, 1.146653543253323582 ) ) ;
#20962 = CARTESIAN_POINT ( 'NONE',  ( 1.054774247047244540, -0.07405724077823318263, 1.953740157426552715 ) ) ;
#20963 = CARTESIAN_POINT ( 'NONE',  ( 0.8107537697050253289, -0.1574803149606297803, 0.4995078739082208230 ) ) ;
#20964 = ORIENTED_EDGE ( 'NONE', *, *, #40609, .T. ) ;
#20965 = AXIS2_PLACEMENT_3D ( 'NONE', #1203, #30713, #12964 ) ;
#20966 = CARTESIAN_POINT ( 'NONE',  ( -0.8759842519685039353, 0.1574803149606299191, 1.122047244094488194 ) ) ;
#20967 = CARTESIAN_POINT ( 'NONE',  ( -0.7185039370078739607, 1.928577636452523993E-17, 0.3346456691838114450 ) ) ;
#20968 = CARTESIAN_POINT ( 'NONE',  ( -0.7185039370078739607, 1.928577636452523993E-17, 1.525590551181102317 ) ) ;
#20969 = CARTESIAN_POINT ( 'NONE',  ( 1.002407869896990045, 0.1264236179284866091, 1.286909448765133801 ) ) ;
#20971 = CARTESIAN_POINT ( 'NONE',  ( -0.9412147342319837628, 0.1574803149606300301, 0.2829724408373550104 ) ) ;
#20970 = CARTESIAN_POINT ( 'NONE',  ( 1.033464566929133799, 0.000000000000000000, 0.9842519683964094934 ) ) ;
#20972 = CARTESIAN_POINT ( 'NONE',  ( 0.1787899950787401604, -0.05708661411946481384, -0.07405724077823318263 ) ) ;
#20973 = DIRECTION ( 'NONE',  ( 0.000000000000000000, -0.1045284632676499459, 0.9945218953682736229 ) ) ;
#20974 = ORIENTED_EDGE ( 'NONE', *, *, #21276, .F. ) ;
#20975 = CARTESIAN_POINT ( 'NONE',  ( 0.1910524284696302755, 0.07767250275969661555, 0.1751288998598690416 ) ) ;
#20976 = DIRECTION ( 'NONE',  ( 0.000000000000000000, -1.000000000000000000, 0.000000000000000000 ) ) ;
#20977 = ORIENTED_EDGE ( 'NONE', *, *, #36302, .T. ) ;
#20978 = CARTESIAN_POINT ( 'NONE',  ( 0.8019270111902717657, -0.1787899950787401604, 0.4084645668753704717 ) ) ;
#20979 = EDGE_CURVE ( 'NONE', #5079, #44357, #26919, .T. ) ;
#20980 = ORIENTED_EDGE ( 'NONE', *, *, #36215, .T. ) ;
#20982 = CARTESIAN_POINT ( 'NONE',  ( -0.07405724077823318263, -1.769685039316315267, 0.1787899950787401604 ) ) ;
#20981 = CARTESIAN_POINT ( 'NONE',  ( -9.642888182262618425E-18, -0.4212598424121582474, -0.1574803149606299191 ) ) ;
#20983 = CARTESIAN_POINT ( 'NONE',  ( -1.002407869896990045, 0.1264236179284866091, 1.956200787347811110 ) ) ;
#20984 = CARTESIAN_POINT ( 'NONE',  ( -0.9500414927467377701, -0.1787899950787401604, 1.077755905458048113 ) ) ;
#20985 = CARTESIAN_POINT ( 'NONE',  ( -1.054774247047244540, -0.07405724077823318263, 0.7332677164816707727 ) ) ;
#20986 = AXIS2_PLACEMENT_3D ( 'NONE', #19237, #41021, #15194 ) ;
#20987 = DIRECTION ( 'NONE',  ( 1.000000000000000000, 0.000000000000000000, 0.000000000000000000 ) ) ;
#20988 = CARTESIAN_POINT ( 'NONE',  ( -0.1264236179284866091, -0.7201042831898681884, 0.1264236179284866091 ) ) ;
#20989 = EDGE_LOOP ( 'NONE', ( #5941, #11877, #37546, #17743 ) ) ;
#20990 = CARTESIAN_POINT ( 'NONE',  ( -0.1505467838310571016, -0.08956164613504763450, 0.06735808213815078216 ) ) ;
#20991 = DIRECTION ( 'NONE',  ( 0.000000000000000000, 1.000000000000000000, 6.980778575359379259E-17 ) ) ;
#20992 = AXIS2_PLACEMENT_3D ( 'NONE', #16898, #44868, #12080 ) ;
#20993 = ORIENTED_EDGE ( 'NONE', *, *, #22350, .F. ) ;
#20994 = CARTESIAN_POINT ( 'NONE',  ( 0.7185039370078739607, 1.928577636452523993E-17, 0.7775590551181102983 ) ) ;
#20995 = ADVANCED_FACE ( 'NONE', ( #25559 ), #18110, .T. ) ;
#20996 = CARTESIAN_POINT ( 'NONE',  ( -0.8759842519685039353, 0.000000000000000000, 0.000000000000000000 ) ) ;
#20997 = CARTESIAN_POINT ( 'NONE',  ( -0.9500414927467378812, -0.1787899950787401604, 0.6446850393163160442 ) ) ;
#20998 = CARTESIAN_POINT ( 'NONE',  ( -9.642888182262618425E-18, 0.001968503937007873988, -0.1574803149606299191 ) ) ;
#20999 = ORIENTED_EDGE ( 'NONE', *, *, #35855, .T. ) ;
#21000 = ADVANCED_FACE ( 'NONE', ( #47349 ), #2388, .T. ) ;
#21001 = VECTOR ( 'NONE', #24527, 39.37007874015748143 ) ;
#21002 = CARTESIAN_POINT ( 'NONE',  ( -0.6971942568897637749, 2.189545951927499583E-17, 1.621555118056472455 ) ) ;
#21003 = CARTESIAN_POINT ( 'NONE',  ( -0.1586641775163213364, 0.9310112235910577017, -1.064878870394357691 ) ) ;
#21004 = CARTESIAN_POINT ( 'NONE',  ( 0.8107537697050254399, 0.1574803149606300301, 1.035925196742866650 ) ) ;
#21005 = CARTESIAN_POINT ( 'NONE',  ( 0.2362204724409448509, 0.000000000000000000, 0.9891732283464566011 ) ) ;
#21006 = ORIENTED_EDGE ( 'NONE', *, *, #35133, .F. ) ;
#21007 = CARTESIAN_POINT ( 'NONE',  ( 0.1797182628040039087, -0.7712052269058795595, 0.07444174185955046430 ) ) ;
#21008 = CARTESIAN_POINT ( 'NONE',  ( -0.8107537697050253289, 0.1574803149606300301, 1.429625984144440531 ) ) ;
#21009 = CARTESIAN_POINT ( 'NONE',  ( 0.6971942568897626646, -0.07405724077823297447, 0.6791338582139527791 ) ) ;
#21010 = CARTESIAN_POINT ( 'NONE',  ( -0.1574803149606297803, -0.6156496062992122820, 0.06523048226347956391 ) ) ;
#21011 = CARTESIAN_POINT ( 'NONE',  ( 0.2471922904502825424, 0.04213860324412696534, -0.1312291345420432964 ) ) ;
#21012 = EDGE_LOOP ( 'NONE', ( #14860, #43783, #1407, #2299 ) ) ;
#21013 = B_SPLINE_CURVE_WITH_KNOTS ( 'NONE', 3,
 ( #47411, #33525, #641, #15294, #36628, #11708, #26333, #39961, #29491, #32586, #22227, #44035, #40894, #37316, #11236, #21778, #25847, #40429, #14585, #7612, #4465, #14357, #36860, #4015, #18634, #29259, #33294, #29005, #10774, #37561, #11947, #19822, #16250, #9284 ),
 .UNSPECIFIED., .F., .F.,
 ( 4, 2, 2, 2, 2, 2, 2, 2, 2, 2, 2, 2, 2, 2, 2, 2, 4 ),
 ( 0.01356295551947107707, 0.01440869495260771981, 0.01525443438574436081, 0.01610017381888100355, 0.01694591325201764628, 0.01779165268515428555, 0.01863739211829092829, 0.01948313155142757103, 0.02032887098456421376, 0.02117461041770085650, 0.02202034985083749924, 0.02286608928397414198, 0.02371182871711078471, 0.02455756815024742745, 0.02540330758338407019, 0.02624904701652071293, 0.02709478644965735220 ),
 .UNSPECIFIED. ) ;
#21014 = CARTESIAN_POINT ( 'NONE',  ( 0.7185039370078739607, 1.928577636452523993E-17, 1.289370078740157632 ) ) ;
#21016 = DIRECTION ( 'NONE',  ( 0.000000000000000000, 0.000000000000000000, 1.000000000000000000 ) ) ;
#21015 = DIRECTION ( 'NONE',  ( 0.000000000000000000, 0.000000000000000000, -1.000000000000000000 ) ) ;
#21017 = DIRECTION ( 'NONE',  ( 0.000000000000000000, 0.000000000000000000, -1.000000000000000000 ) ) ;
#21019 = DIRECTION ( 'NONE',  ( -1.000000000000000000, 3.469446951953614189E-15, 0.000000000000000000 ) ) ;
#21018 = CARTESIAN_POINT ( 'NONE',  ( 0.8019270111902716547, -0.1787899950787401604, 0.6003937007336380693 ) ) ;
#21020 = CARTESIAN_POINT ( 'NONE',  ( -0.7185039370078739607, 1.928577636452523993E-17, 0.6988188976377952555 ) ) ;
#21021 = CIRCLE ( 'NONE', #14175, 0.02900000000000001882 ) ;
#21022 = DIRECTION ( 'NONE',  ( 1.000000000000000000, 0.000000000000000000, 0.000000000000000000 ) ) ;
#21023 = VERTEX_POINT ( 'NONE', #14759 ) ;
#21024 = CARTESIAN_POINT ( 'NONE',  ( 0.1619802298545178210, 0.07975292738397864178, 0.1381419564372848019 ) ) ;
#21025 = AXIS2_PLACEMENT_3D ( 'NONE', #29955, #12671, #22961 ) ;
#21026 = AXIS2_PLACEMENT_3D ( 'NONE', #44098, #46981, #17515 ) ;
#21027 = DIRECTION ( 'NONE',  ( -1.000000000000000000, -0.000000000000000000, 0.000000000000000000 ) ) ;
#21028 = CARTESIAN_POINT ( 'NONE',  ( 0.9500414927467378812, -0.1787899950787401604, 0.8415354330171019859 ) ) ;
#21029 = EDGE_CURVE ( 'NONE', #2394, #3498, #42161, .T. ) ;
#21030 = CARTESIAN_POINT ( 'NONE',  ( -1.033464566929133799, 0.000000000000000000, 0.7185039370078739607 ) ) ;
#21031 = CYLINDRICAL_SURFACE ( 'NONE', #28929, 0.1574803149606299191 ) ;
#21032 = CARTESIAN_POINT ( 'NONE',  ( 0.1797182628040039365, 0.05802705655868669460, -2.200913952912460540E-17 ) ) ;
#21033 = CARTESIAN_POINT ( 'NONE',  ( 0.1787899950787401604, -1.011811023568284451, 0.07405724077823318263 ) ) ;
#21034 = CARTESIAN_POINT ( 'NONE',  ( -9.642888182262618425E-18, -1.454724409448818756, -0.1574803149606299191 ) ) ;
#21035 = CARTESIAN_POINT ( 'NONE',  ( 0.7185039370078739607, 1.928577636452523993E-17, 1.279527558947590515 ) ) ;
#21036 = ADVANCED_FACE ( 'NONE', ( #6362 ), #35848, .T. ) ;
#21037 = ORIENTED_EDGE ( 'NONE', *, *, #21157, .T. ) ;
#21038 = CARTESIAN_POINT ( 'NONE',  ( -0.8019270111902717657, -0.1787899950787401604, 1.943897637741510254 ) ) ;
#21039 = EDGE_LOOP ( 'NONE', ( #36117, #29659, #21538, #37654 ) ) ;
#21040 = ORIENTED_EDGE ( 'NONE', *, *, #40875, .F. ) ;
#21041 = EDGE_CURVE ( 'NONE', #8391, #15306, #2765, .T. ) ;
#21042 = CARTESIAN_POINT ( 'NONE',  ( 0.8759842519685039353, 0.1787899950787401882, 1.926673228292693052 ) ) ;
#21043 = ORIENTED_EDGE ( 'NONE', *, *, #43437, .T. ) ;
#21044 = CARTESIAN_POINT ( 'NONE',  ( -0.8759842519685039353, 0.1787899950787401882, 1.926673228292693052 ) ) ;
#21045 = CARTESIAN_POINT ( 'NONE',  ( -1.054774247047244096, 0.000000000000000000, 1.557578740103716441 ) ) ;
#21046 = CARTESIAN_POINT ( 'NONE',  ( -0.8759842519685039353, -0.1787899950787401882, 1.035925196796629866 ) ) ;
#21047 = CARTESIAN_POINT ( 'NONE',  ( -0.9500414927467378812, 0.1787899950787401604, 0.1919291338045042428 ) ) ;
#21048 = CARTESIAN_POINT ( 'NONE',  ( -0.2471922904502826535, 0.04213860324413871983, 0.1312291345420296129 ) ) ;
#21049 = CARTESIAN_POINT ( 'NONE',  ( -0.8019270111902717657, -0.1787899950787401604, 1.904527559001354398 ) ) ;
#21050 = CARTESIAN_POINT ( 'NONE',  ( 0.06756161724125105128, -0.08412760742795728774, -0.2464250160559827429 ) ) ;
#21051 = CARTESIAN_POINT ( 'NONE',  ( -0.7185039370078746268, -0.06523048226347956391, 1.961122047244095778 ) ) ;
#21052 = DIRECTION ( 'NONE',  ( 0.000000000000000000, 0.1045284632676499320, -0.9945218953682736229 ) ) ;
#21053 = CARTESIAN_POINT ( 'NONE',  ( -0.1264236179284866091, -0.2181357792528606510, -0.1264236179284866091 ) ) ;
#21054 = CARTESIAN_POINT ( 'NONE',  ( -9.642888182262618425E-18, 0.001968503937007873988, -0.1574803149606299191 ) ) ;
#21055 = AXIS2_PLACEMENT_3D ( 'NONE', #34265, #15822, #5237 ) ;
#21056 = CARTESIAN_POINT ( 'NONE',  ( -0.8759842519685039353, 0.1787899950787401882, 0.1107283464029295283 ) ) ;
#21057 = VERTEX_POINT ( 'NONE', #6835 ) ;
#21058 = VECTOR ( 'NONE', #22772, 39.37007874015748143 ) ;
#21059 = CARTESIAN_POINT ( 'NONE',  ( -0.6971942568897648851, -0.07405724077823297447, 1.269685039316314601 ) ) ;
#21060 = VERTEX_POINT ( 'NONE', #17632 ) ;
#21061 = AXIS2_PLACEMENT_3D ( 'NONE', #10117, #24728, #46758 ) ;
#21062 = VECTOR ( 'NONE', #33998, 39.37007874015748854 ) ;
#21063 = CARTESIAN_POINT ( 'NONE',  ( -0.1787899950787401604, -1.144685039316316599, 0.07405724077823318263 ) ) ;
#21064 = CARTESIAN_POINT ( 'NONE',  ( -0.1787899950787401882, -1.220964566875370139, 0.000000000000000000 ) ) ;
#21065 = ( BOUNDED_CURVE ( )  B_SPLINE_CURVE ( 2, ( #11905, #34196, #15981, #8285, #30602, #34656, #45638, #37525, #45166 ),
 .UNSPECIFIED., .F., .T. ) 
 B_SPLINE_CURVE_WITH_KNOTS ( ( 3, 2, 2, 2, 3 ),
 ( 0.5500000000000000444, 0.5524999999999999911, 0.5550000000000000488, 0.5574999999999999956, 0.5600000000000000533 ),
 .UNSPECIFIED. ) 
 CURVE ( )  GEOMETRIC_REPRESENTATION_ITEM ( )  RATIONAL_B_SPLINE_CURVE ( ( 1.000000000000000000, 0.9238795325112869605, 1.000000000000000000, 0.9238795325112869605, 1.000000000000000000, 0.9238795325112869605, 1.000000000000000000, 0.9238795325112869605, 1.000000000000000000 ) ) 
 REPRESENTATION_ITEM ( '' )  ) ;
#21066 = CARTESIAN_POINT ( 'NONE',  ( -0.7185039370078766252, -0.06523048226348168721, 1.360728346349167284 ) ) ;
#21067 = CARTESIAN_POINT ( 'NONE',  ( 0.1270800023317771588, -0.5276028647011559158, -0.1270800023317771588 ) ) ;
#21068 = CARTESIAN_POINT ( 'NONE',  ( 0.000000000000000000, 0.000000000000000000, -0.3149606299212598381 ) ) ;
#21069 = CARTESIAN_POINT ( 'NONE',  ( -0.8107537697050253289, -0.1574803149606297803, 0.8932086613097963701 ) ) ;
#21070 = CARTESIAN_POINT ( 'NONE',  ( -0.7646288533564489232, 0.1113553986120547346, 0.7332677165354331006 ) ) ;
#21071 = CARTESIAN_POINT ( 'NONE',  ( 0.1574803149606300301, -0.08415354330708657571, -0.06523048226347956391 ) ) ;
#21072 = CARTESIAN_POINT ( 'NONE',  ( 1.033464566929134687, 0.06523048226347956391, 1.813484251860976393 ) ) ;
#21073 = LINE ( 'NONE', #32372, #23832 ) ;
#21074 = CARTESIAN_POINT ( 'NONE',  ( 0.7185039370078739607, 1.928577636452523993E-17, 0.8562992125984251190 ) ) ;
#21075 = CARTESIAN_POINT ( 'NONE',  ( 0.09357655176633394856, -0.2414677849102791207, -0.03395687952546033034 ) ) ;
#21076 = DIRECTION ( 'NONE',  ( 0.000000000000000000, 0.000000000000000000, 1.000000000000000000 ) ) ;
#21078 = CARTESIAN_POINT ( 'NONE',  ( 0.1587072800412991924, -0.1427694538647072964, -0.03362159989229708545 ) ) ;
#21077 = FACE_OUTER_BOUND ( 'NONE', #39620, .T. ) ;
#21079 = CARTESIAN_POINT ( 'NONE',  ( 1.033464566929134687, 0.06523048226347956391, 0.1993110235145201248 ) ) ;
#21080 = AXIS2_PLACEMENT_3D ( 'NONE', #23885, #5665, #20514 ) ;
#21081 = EDGE_CURVE ( 'NONE', #25548, #17121, #43710, .T. ) ;
#21082 = LINE ( 'NONE', #12341, #5704 ) ;
#21083 = PLANE ( 'NONE',  #19075 ) ;
#21084 = CARTESIAN_POINT ( 'NONE',  ( -0.1264236179284866091, -0.6402559054580471143, -0.1264236179284866091 ) ) ;
#21085 = CARTESIAN_POINT ( 'NONE',  ( -0.1113553986120547346, -1.016732283464566899, -0.1113553986120547346 ) ) ;
#21086 = ( BOUNDED_CURVE ( )  B_SPLINE_CURVE ( 2, ( #19769, #8270, #26512, #23138, #44673, #31059, #45623, #16193, #12126 ),
 .UNSPECIFIED., .F., .F. ) 
 B_SPLINE_CURVE_WITH_KNOTS ( ( 3, 2, 2, 2, 3 ),
 ( 0.9300000000000000488, 0.9324999999999999956, 0.9350000000000000533, 0.9375000000000000000, 0.9399999999999999467 ),
 .UNSPECIFIED. ) 
 CURVE ( )  GEOMETRIC_REPRESENTATION_ITEM ( )  RATIONAL_B_SPLINE_CURVE ( ( 1.000000000000000000, 0.9238795325112899581, 1.000000000000000000, 0.9238795325112869605, 1.000000000000000000, 0.9238795325112869605, 1.000000000000000000, 0.9238795325112829637, 1.000000000000000000 ) ) 
 REPRESENTATION_ITEM ( '' )  ) ;
#21087 = EDGE_CURVE ( 'NONE', #5618, #3128, #42848, .T. ) ;
#21088 = LINE ( 'NONE', #10573, #37455 ) ;
#21089 = CARTESIAN_POINT ( 'NONE',  ( -0.6971942568897648851, 0.07405724077823318263, 1.889763779473794258 ) ) ;
#21090 = EDGE_LOOP ( 'NONE', ( #16637, #700, #24015, #15342 ) ) ;
#21091 = EDGE_LOOP ( 'NONE', ( #18526, #35846, #25306, #17762 ) ) ;
#21092 = CARTESIAN_POINT ( 'NONE',  ( -0.6971942568897648851, -0.07405724077823297447, 1.387795275536786610 ) ) ;
#21093 = EDGE_CURVE ( 'NONE', #28863, #27412, #21143, .T. ) ;
#21095 = CARTESIAN_POINT ( 'NONE',  ( 0.2944196465027555387, 4.766607801171850497E-17, 0.000000000000000000 ) ) ;
#21094 = VECTOR ( 'NONE', #28711, 39.37007874015748143 ) ;
#21096 = CARTESIAN_POINT ( 'NONE',  ( -0.9500414927467378812, -0.1787899950787401604, 0.6102362204186774219 ) ) ;
#21097 = EDGE_CURVE ( 'NONE', #18573, #40024, #4675, .T. ) ;
#21098 = CARTESIAN_POINT ( 'NONE',  ( -0.8759842519685039353, 0.000000000000000000, 0.000000000000000000 ) ) ;
#21099 = CARTESIAN_POINT ( 'NONE',  ( 1.002407869896990045, 0.1264236179284866091, 0.7800196849856062542 ) ) ;
#21100 = CARTESIAN_POINT ( 'NONE',  ( -0.9500414927467377701, -0.1787899950787401604, 0.4872047243556847929 ) ) ;
#21101 = DIRECTION ( 'NONE',  ( 0.000000000000000000, -0.2432573283306649070, 0.9699617890481186944 ) ) ;
#21102 = CARTESIAN_POINT ( 'NONE',  ( 0.8107537697050254399, -0.1574803149606297803, 1.139271653543306506 ) ) ;
#21103 = CARTESIAN_POINT ( 'NONE',  ( -0.1574803149606300301, -0.1382874014672760277, -0.06523048226347956391 ) ) ;
#21104 = CARTESIAN_POINT ( 'NONE',  ( -0.6971942568897648851, 0.07405724077823318263, 1.500984251914741607 ) ) ;
#21105 = CARTESIAN_POINT ( 'NONE',  ( -0.9873396505805591694, -0.1113553986120547346, 1.461614173228346525 ) ) ;
#21106 = CARTESIAN_POINT ( 'NONE',  ( -1.033464566929133799, 0.000000000000000000, 0.4822834645669291653 ) ) ;
#21107 = CARTESIAN_POINT ( 'NONE',  ( 0.6971942568897637749, 2.189545951927499583E-17, 1.306594488135212728 ) ) ;
#21108 = CARTESIAN_POINT ( 'NONE',  ( 0.05242207689368432594, -0.09851384127917696409, -0.1861051744488299298 ) ) ;
#21109 = VERTEX_POINT ( 'NONE', #41711 ) ;
#21110 = DIRECTION ( 'NONE',  ( -0.8191520442889991260, 0.000000000000000000, -0.5735764363510355013 ) ) ;
#21111 = MANIFOLD_SOLID_BREP ( 'Link Bar', #39268 ) ;
#21112 = CARTESIAN_POINT ( 'NONE',  ( -0.1787899950787401882, -1.709277511536324790, 0.000000000000000000 ) ) ;
#21113 = ORIENTED_EDGE ( 'NONE', *, *, #21177, .F. ) ;
#21114 = CARTESIAN_POINT ( 'NONE',  ( 0.2471922904502826812, -0.09842519685039370636, -5.914624404477007554E-17 ) ) ;
#21115 = CARTESIAN_POINT ( 'NONE',  ( 0.7185039370078739607, 0.000000000000000000, 4.498031496062992574 ) ) ;
#21116 = ORIENTED_EDGE ( 'NONE', *, *, #13012, .F. ) ;
#21117 = CARTESIAN_POINT ( 'NONE',  ( 0.8019270111902717657, -0.1787899950787401604, 1.387795275536786610 ) ) ;
#21118 = CIRCLE ( 'NONE', #27293, 0.09842519685039310962 ) ;
#21119 = EDGE_CURVE ( 'NONE', #28934, #18699, #10838, .T. ) ;
#21120 = DIRECTION ( 'NONE',  ( 0.000000000000000000, 0.000000000000000000, -1.000000000000000000 ) ) ;
#21121 = CARTESIAN_POINT ( 'NONE',  ( 3.284318927891251994E-17, -0.2711614172690712810, 0.1787899950787401882 ) ) ;
#21122 = CARTESIAN_POINT ( 'NONE',  ( -0.1264236179284866091, -0.7140748030958424808, -0.1264236179284866091 ) ) ;
#21123 = CARTESIAN_POINT ( 'NONE',  ( 0.1673228346456693549, -0.4812165006432427838, -0.8611016091043821596 ) ) ;
#21124 = CARTESIAN_POINT ( 'NONE',  ( 0.1639941273274911349, -0.1614384449312174230, -8.749531877264769744E-07 ) ) ;
#21125 = CARTESIAN_POINT ( 'NONE',  ( 0.6971942568897626646, -0.07405724077823297447, 0.2805118109698587214 ) ) ;
#21126 = CARTESIAN_POINT ( 'NONE',  ( -0.1264236179284866091, -0.05081294460719149725, 0.1264236179284866091 ) ) ;
#21127 = CARTESIAN_POINT ( 'NONE',  ( 0.1787899950787401882, 0.01427165359707061217, -2.189545951927503898E-17 ) ) ;
#21128 = CARTESIAN_POINT ( 'NONE',  ( -0.7185039370078739607, 1.928577636452523993E-17, 0.1870078740157480324 ) ) ;
#21129 = CARTESIAN_POINT ( 'NONE',  ( -0.8759842519685039353, -0.1574803149606299191, 1.486220472333417142 ) ) ;
#21130 = EDGE_CURVE ( 'NONE', #46334, #7028, #26157, .T. ) ;
#21131 = CARTESIAN_POINT ( 'NONE',  ( 0.6971942568897626646, 0.07405724077823318263, 0.6299212597887560161 ) ) ;
#21132 = CARTESIAN_POINT ( 'NONE',  ( -0.9500414927467377701, -0.1787899950787401604, 1.043307086560409269 ) ) ;
#21134 = FACE_OUTER_BOUND ( 'NONE', #29620, .T. ) ;
#21133 = CARTESIAN_POINT ( 'NONE',  ( 0.06523048226347956391, -0.9601377952755901779, 0.1574803149606297803 ) ) ;
#21135 = CARTESIAN_POINT ( 'NONE',  ( 0.1797182628040039365, -1.713626486748399680, -2.200913952912460540E-17 ) ) ;
#21136 = CARTESIAN_POINT ( 'NONE',  ( 1.002407869896990045, -0.1264236179284866091, 1.675688976324189117 ) ) ;
#21138 = CARTESIAN_POINT ( 'NONE',  ( 0.1574803149606300023, -0.2142072668875218133, -1.269802121763611291 ) ) ;
#21137 = DIRECTION ( 'NONE',  ( 0.7986355100472981583, -0.000000000000000000, 0.6018150231520413840 ) ) ;
#21139 = EDGE_LOOP ( 'NONE', ( #10220, #21540, #31457 ) ) ;
#21140 = CARTESIAN_POINT ( 'NONE',  ( -0.1925175471592172338, -0.07678538764761655422, -0.1742829424377035086 ) ) ;
#21141 = CARTESIAN_POINT ( 'NONE',  ( 0.1711365707900877331, -0.1966896243418751189, -0.3121915932859509191 ) ) ;
#21142 = CARTESIAN_POINT ( 'NONE',  ( 0.1787899950787401604, -0.1456692912848192578, 0.07405724077823318263 ) ) ;
#21143 = B_SPLINE_CURVE_WITH_KNOTS ( 'NONE', 3,
 ( #27400, #360, #7788, #40362, #15241, #11646, #36799, #4182, #16123, #41942, #3952, #19924, #29887, #38376, #25791, #33232, #18808, #33465, #30978, #29662, #8912, #37259, #7552 ),
 .UNSPECIFIED., .F., .F.,
 ( 4, 2, 2, 1, 1, 1, 2, 2, 2, 1, 1, 2, 2, 4 ),
 ( 0.000000000000000000, 0.2500000000000059397, 0.3750000000000091593, 0.4375000000000106026, 0.4687500000000113798, 0.4843750000000119349, 0.4921875000000120459, 0.5000000000000121014, 0.6250000000000104361, 0.6875000000000094369, 0.7187500000000087708, 0.7343750000000082157, 0.7500000000000076605, 1.000000000000000000 ),
 .UNSPECIFIED. ) ;
#21144 = CARTESIAN_POINT ( 'NONE',  ( 1.054774247047244096, 0.000000000000000000, 0.6520669290800944484 ) ) ;
#21145 = CARTESIAN_POINT ( 'NONE',  ( -0.07405724077823318263, -0.8740157479777336258, -0.1787899950787401604 ) ) ;
#21146 = CARTESIAN_POINT ( 'NONE',  ( 0.7495606340400177148, -0.1264236179284866091, 0.1304133857730082613 ) ) ;
#21147 = EDGE_CURVE ( 'NONE', #19692, #37242, #2183, .T. ) ;
#21148 = DIRECTION ( 'NONE',  ( 0.000000000000000000, -1.000000000000000000, 0.000000000000000000 ) ) ;
#21149 = CARTESIAN_POINT ( 'NONE',  ( 0.1184675242425320824, -0.09842519685039370636, 1.713085361781127913 ) ) ;
#21150 = CARTESIAN_POINT ( 'NONE',  ( -0.9500414927467378812, 0.1787899950787401604, 1.486220472387181690 ) ) ;
#21151 = VERTEX_POINT ( 'NONE', #46498 ) ;
#21152 = CARTESIAN_POINT ( 'NONE',  ( -0.3010365421720465617, -0.07487990393731468186, -0.7259551242400892335 ) ) ;
#21153 = CARTESIAN_POINT ( 'NONE',  ( -0.7185039370078739607, 1.928577636452523993E-17, 0.6496062991050708391 ) ) ;
#21154 = CARTESIAN_POINT ( 'NONE',  ( 1.054774247047244096, 0.000000000000000000, 1.793799212544661348 ) ) ;
#21155 = CARTESIAN_POINT ( 'NONE',  ( -0.7185039370078746268, -0.06523048226347956391, 1.331200787401575436 ) ) ;
#21156 = CARTESIAN_POINT ( 'NONE',  ( -1.054774247047244096, 0.000000000000000000, 0.9670275590013542866 ) ) ;
#21157 = EDGE_CURVE ( 'NONE', #22637, #42566, #17044, .T. ) ;
#21158 = CARTESIAN_POINT ( 'NONE',  ( -0.7646288533564489232, 0.1113553986120547346, 0.5265748030420794867 ) ) ;
#21159 = CARTESIAN_POINT ( 'NONE',  ( 1.181102362204724310, -0.3937007874015748254, -0.9842519685039370358 ) ) ;
#21160 = CARTESIAN_POINT ( 'NONE',  ( 1.002407869896990045, -0.1264236179284866091, 0.3371062991588349989 ) ) ;
#21161 = CARTESIAN_POINT ( 'NONE',  ( -0.9500414927467377701, -0.1787899950787401604, 0.09350393695411057804 ) ) ;
#21162 = CARTESIAN_POINT ( 'NONE',  ( -0.9500414927467378812, -0.1787899950787401604, 0.5659448818360001132 ) ) ;
#21163 = CARTESIAN_POINT ( 'NONE',  ( 0.7185039370078739607, 1.928577636452523993E-17, 1.515748031388535200 ) ) ;
#21164 = ORIENTED_EDGE ( 'NONE', *, *, #24208, .T. ) ;
#21165 = CARTESIAN_POINT ( 'NONE',  ( 0.1787899950787401882, -0.06446850388324429360, -2.189545951927503898E-17 ) ) ;
#21166 = CARTESIAN_POINT ( 'NONE',  ( 1.002407869896990045, -0.1264236179284866091, 0.7308070865604093802 ) ) ;
#21167 = CARTESIAN_POINT ( 'NONE',  ( -1.002407869896990045, -0.1264236179284866091, 1.710137795221826851 ) ) ;
#21168 = CARTESIAN_POINT ( 'NONE',  ( 0.1787899950787401604, -1.479330708607653699, 0.07405724077823318263 ) ) ;
#21169 = ORIENTED_EDGE ( 'NONE', *, *, #22552, .T. ) ;
#21170 = CARTESIAN_POINT ( 'NONE',  ( -0.8759842519685039353, 0.1574803149606299191, 0.6496062992125984925 ) ) ;
#21171 = CARTESIAN_POINT ( 'NONE',  ( 0.03901279071809810040, -0.09842519685039370636, 2.185526306663017504 ) ) ;
#21172 = CARTESIAN_POINT ( 'NONE',  ( 0.07405724077823318263, -1.303273574528451384, 0.1787899950787401604 ) ) ;
#21173 = ORIENTED_EDGE ( 'NONE', *, *, #29973, .T. ) ;
#21174 = CARTESIAN_POINT ( 'NONE',  ( -0.1264236179284866091, -0.1530511810485988278, 0.1264236179284866091 ) ) ;
#21175 = ORIENTED_EDGE ( 'NONE', *, *, #44030, .T. ) ;
#21176 = CARTESIAN_POINT ( 'NONE',  ( 0.001132063566998833728, -0.1311094469944007745, -0.04850708733712583154 ) ) ;
#21177 = EDGE_CURVE ( 'NONE', #47236, #27709, #28543, .T. ) ;
#21178 = CARTESIAN_POINT ( 'NONE',  ( -0.9412147342319837628, 0.1574803149606300301, 0.9128937006798734100 ) ) ;
#21179 = AXIS2_PLACEMENT_3D ( 'NONE', #23552, #12304, #19936 ) ;
#21180 = CARTESIAN_POINT ( 'NONE',  ( 0.7185039370078746268, -0.06523048226347956391, 1.961122047244095778 ) ) ;
#21181 = CARTESIAN_POINT ( 'NONE',  ( -0.1264236179284866091, -1.457185039316315045, 0.1264236179284866091 ) ) ;
#21182 = VECTOR ( 'NONE', #30266, 39.37007874015748143 ) ;
#21183 = CARTESIAN_POINT ( 'NONE',  ( 0.1264236179284866091, -0.7288385826234015097, -0.1264236179284866091 ) ) ;
#21184 = CARTESIAN_POINT ( 'NONE',  ( -1.054774247047244540, -0.07405724077823318263, 0.3395669290800949480 ) ) ;
#21185 = CARTESIAN_POINT ( 'NONE',  ( 0.1270800023317771588, -1.285476880449186954, 0.1270800023317771588 ) ) ;
#21186 = CARTESIAN_POINT ( 'NONE',  ( -0.2151545284320415252, 0.1712747073548011034, -0.06815351164859909106 ) ) ;
#21187 = CARTESIAN_POINT ( 'NONE',  ( 0.8019270111902716547, 0.1787899950787401604, 1.530511810969859221 ) ) ;
#21188 = CARTESIAN_POINT ( 'NONE',  ( 0.6971942568897637749, 2.189545951927499583E-17, 0.1599409448281264023 ) ) ;
#21189 = CARTESIAN_POINT ( 'NONE',  ( -0.8759842519685039353, 0.1574803149606299191, 1.909448818897637956 ) ) ;
#21190 = CARTESIAN_POINT ( 'NONE',  ( 0.8107537697050253289, 0.1574803149606300301, 1.675688976377952777 ) ) ;
#21191 = CARTESIAN_POINT ( 'NONE',  ( 0.008579867197626878106, 0.1299212598425198151, 0.1749887852363761209 ) ) ;
#21193 = CARTESIAN_POINT ( 'NONE',  ( 0.7185039370078746268, 0.06523048226347956391, 1.719980314960630086 ) ) ;
#21192 = CARTESIAN_POINT ( 'NONE',  ( -0.9873396505805591694, 0.1113553986120547346, 0.9990157480314961758 ) ) ;
#21194 = CARTESIAN_POINT ( 'NONE',  ( 0.8107537697050254399, -0.1574803149606297803, 1.444389763672000671 ) ) ;
#21195 = CYLINDRICAL_SURFACE ( 'NONE', #2184, 0.1574803149606299191 ) ;
#21196 = CARTESIAN_POINT ( 'NONE',  ( -0.7185039370078739607, 1.928577636452523993E-17, 1.673228346349165285 ) ) ;
#21197 = CARTESIAN_POINT ( 'NONE',  ( 1.002407869896990045, 0.1264236179284866091, 0.1451771653005673179 ) ) ;
#21198 = ( BOUNDED_CURVE ( )  B_SPLINE_CURVE ( 2, ( #29352, #21564, #14151, #28073, #36202, #39291, #17030, #39527, #17966 ),
 .UNSPECIFIED., .F., .T. ) 
 B_SPLINE_CURVE_WITH_KNOTS ( ( 3, 2, 2, 2, 3 ),
 ( 0.9100000000000000311, 0.9124999999999999778, 0.9150000000000000355, 0.9174999999999999822, 0.9200000000000000400 ),
 .UNSPECIFIED. ) 
 CURVE ( )  GEOMETRIC_REPRESENTATION_ITEM ( )  RATIONAL_B_SPLINE_CURVE ( ( 1.000000000000000000, 0.9238795325112899581, 1.000000000000000000, 0.9238795325112869605, 1.000000000000000000, 0.9238795325112869605, 1.000000000000000000, 0.9238795325112869605, 1.000000000000000000 ) ) 
 REPRESENTATION_ITEM ( '' )  ) ;
#21199 = CARTESIAN_POINT ( 'NONE',  ( 0.7020444741911990860, 0.02838807324270386373, 0.03937007977071780435 ) ) ;
#21200 = ADVANCED_FACE ( 'NONE', ( #35739 ), #9863, .T. ) ;
#21201 = CARTESIAN_POINT ( 'NONE',  ( 1.054774247047244540, -0.07405724077823318263, 1.200787401521039355 ) ) ;
#21202 = CARTESIAN_POINT ( 'NONE',  ( 0.8759842519685039353, -0.1787899950787401882, 1.906988188922614125 ) ) ;
#21203 = CARTESIAN_POINT ( 'NONE',  ( 0.7646288533564489232, 0.1113553986120547346, 0.4872047243019220208 ) ) ;
#21204 = ORIENTED_EDGE ( 'NONE', *, *, #26383, .F. ) ;
#21205 = DIRECTION ( 'NONE',  ( 0.000000000000000000, 0.000000000000000000, -1.000000000000000000 ) ) ;
#21206 = CARTESIAN_POINT ( 'NONE',  ( 0.8905045487882523592, 0.1730449873529631977, 0.03937009343063418987 ) ) ;
#21207 = CARTESIAN_POINT ( 'NONE',  ( -0.7185039370078746268, 0.06523048226347956391, 0.4109251967428667052 ) ) ;
#21208 = VERTEX_POINT ( 'NONE', #35035 ) ;
#21209 = CARTESIAN_POINT ( 'NONE',  ( 0.7495606340400177148, -0.1264236179284866091, 1.503444881836000002 ) ) ;
#21210 = ADVANCED_FACE ( 'NONE', ( #46736 ), #16806, .F. ) ;
#21212 = DIRECTION ( 'NONE',  ( 0.000000000000000000, 0.000000000000000000, -1.000000000000000000 ) ) ;
#21211 = DIRECTION ( 'NONE',  ( -1.000000000000000000, 0.000000000000000000, 0.000000000000000000 ) ) ;
#21213 = CARTESIAN_POINT ( 'NONE',  ( -1.094772975963752103E-17, 0.02903543312462964626, -0.1787899950787401882 ) ) ;
#21214 = ORIENTED_EDGE ( 'NONE', *, *, #26756, .F. ) ;
#21215 = VECTOR ( 'NONE', #14989, 39.37007874015748143 ) ;
#21216 = CYLINDRICAL_SURFACE ( 'NONE', #19149, 0.1574803149606299191 ) ;
#21217 = VERTEX_POINT ( 'NONE', #27636 ) ;
#21218 = CARTESIAN_POINT ( 'NONE',  ( -0.8759842519685039353, 0.000000000000000000, 0.000000000000000000 ) ) ;
#21219 = CARTESIAN_POINT ( 'NONE',  ( -0.4330708661417322913, 0.1864803149606299448, -1.186023622047243986 ) ) ;
#21220 = ORIENTED_EDGE ( 'NONE', *, *, #16650, .F. ) ;
#21221 = CARTESIAN_POINT ( 'NONE',  ( 1.054774247047244096, 0.000000000000000000, 0.5782480314422993040 ) ) ;
#21222 = CARTESIAN_POINT ( 'NONE',  ( -1.002407869896990045, 0.1264236179284866091, 1.326279527505291433 ) ) ;
#21224 = CARTESIAN_POINT ( 'NONE',  ( 0.07405724077823318263, -1.631889763725764553, -0.1787899950787401604 ) ) ;
#21223 = CARTESIAN_POINT ( 'NONE',  ( 0.1574803149606299191, -0.4311023620971976555, -1.928577636452523993E-17 ) ) ;
#21225 = CARTESIAN_POINT ( 'NONE',  ( -1.054774247047244540, -0.07405724077823318263, 1.205708661363558365 ) ) ;
#21226 = CARTESIAN_POINT ( 'NONE',  ( -0.9412147342319837628, 0.1574803149606300301, 0.01722440944881892255 ) ) ;
#21227 = VERTEX_POINT ( 'NONE', #24950 ) ;
#21228 = CARTESIAN_POINT ( 'NONE',  ( -0.6971942568897637749, 2.189545951927499583E-17, 1.026082677111590513 ) ) ;
#21229 = CARTESIAN_POINT ( 'NONE',  ( -1.002407869896990045, -0.1264236179284866091, 0.8095472440407244230 ) ) ;
#21230 = CARTESIAN_POINT ( 'NONE',  ( -1.002407869896990045, -0.1264236179284866091, 0.1796259841982051075 ) ) ;
#21231 = CARTESIAN_POINT ( 'NONE',  ( -0.7185039370078739607, 1.928577636452523993E-17, 0.3444881889763780070 ) ) ;
#21232 = DIRECTION ( 'NONE',  ( 1.000000000000000000, 0.000000000000000000, 0.000000000000000000 ) ) ;
#21233 = CARTESIAN_POINT ( 'NONE',  ( -0.1787899950787401604, -0.8455964091741210442, -0.07405724077823318263 ) ) ;
#21234 = ORIENTED_EDGE ( 'NONE', *, *, #12375, .F. ) ;
#21235 = CARTESIAN_POINT ( 'NONE',  ( 0.07139542023256004177, -0.08956251728346555085, 0.1284121166753139920 ) ) ;
#21236 = EDGE_LOOP ( 'NONE', ( #17867, #37267, #6285, #4585, #34863 ) ) ;
#21237 = CARTESIAN_POINT ( 'NONE',  ( 0.000000000000000000, 0.000000000000000000, -0.3149606299212598381 ) ) ;
#21238 = LINE ( 'NONE', #3016, #40877 ) ;
#21239 = CARTESIAN_POINT ( 'NONE',  ( -1.054774247047244540, -0.07405724077823318263, 0.6496062991588353874 ) ) ;
#21240 = CARTESIAN_POINT ( 'NONE',  ( 0.1574803149606300301, -0.005413385826771673418, -0.06523048226347956391 ) ) ;
#21241 = ORIENTED_EDGE ( 'NONE', *, *, #43050, .F. ) ;
#21242 = VECTOR ( 'NONE', #13499, 39.37007874015748143 ) ;
#21243 = CARTESIAN_POINT ( 'NONE',  ( -1.054774247047244540, 0.07405724077823318263, 1.643700787347811998 ) ) ;
#21244 = CARTESIAN_POINT ( 'NONE',  ( -0.8070866141732283561, 0.000000000000000000, -0.6590551181102368705 ) ) ;
#21245 = CIRCLE ( 'NONE', #27419, 0.09842519685039370636 ) ;
#21246 = FACE_OUTER_BOUND ( 'NONE', #31862, .T. ) ;
#21247 = FACE_OUTER_BOUND ( 'NONE', #27772, .T. ) ;
#21248 = ORIENTED_EDGE ( 'NONE', *, *, #19756, .F. ) ;
#21249 = CARTESIAN_POINT ( 'NONE',  ( 0.7185039370078746268, 0.06523048226347956391, 0.6176181102362200415 ) ) ;
#21250 = CARTESIAN_POINT ( 'NONE',  ( 0.07444174185955046430, -0.9188430221814710697, -0.1797182628040039087 ) ) ;
#21251 = DIRECTION ( 'NONE',  ( -1.000000000000000000, 0.000000000000000000, 0.000000000000000000 ) ) ;
#21252 = CARTESIAN_POINT ( 'NONE',  ( -0.7646288533564489232, -0.1113553986120547346, 1.323818897530267602 ) ) ;
#21253 = EDGE_CURVE ( 'NONE', #8606, #15186, #24248, .T. ) ;
#21254 = CARTESIAN_POINT ( 'NONE',  ( 0.9500414927467378812, 0.1787899950787401604, 0.7824803149068669805 ) ) ;
#21255 = CARTESIAN_POINT ( 'NONE',  ( 0.1113553986120547346, -0.5639763779527559029, 0.1113553986120547346 ) ) ;
#21256 = CARTESIAN_POINT ( 'NONE',  ( -0.1360083797011654438, 0.1240348912602861897, -0.08737303594299716814 ) ) ;
#21257 = CARTESIAN_POINT ( 'NONE',  ( -0.2559055118110236116, -4.908314874579054539E-16, -0.02740704184215039460 ) ) ;
#21258 = CARTESIAN_POINT ( 'NONE',  ( 0.7185039370078746268, -0.06523048226347956391, 1.331200787401575436 ) ) ;
#21260 = FACE_OUTER_BOUND ( 'NONE', #15967, .T. ) ;
#21259 = CARTESIAN_POINT ( 'NONE',  ( 0.9335544921821857800, -0.1666633839053672239, 1.989226213591378301 ) ) ;
#21261 = DIRECTION ( 'NONE',  ( 1.000000000000000000, 0.000000000000000000, 0.000000000000000000 ) ) ;
#21262 = EDGE_CURVE ( 'NONE', #22666, #36464, #21786, .T. ) ;
#21264 = CARTESIAN_POINT ( 'NONE',  ( 0.7185039370078739607, 1.928577636452523993E-17, 0.2559055117034968463 ) ) ;
#21263 = CARTESIAN_POINT ( 'NONE',  ( 0.9500414927467377701, -0.1787899950787401604, 0.6053149605761580787 ) ) ;
#21265 = CARTESIAN_POINT ( 'NONE',  ( 0.7185039370078746268, 0.06523048226347956391, 1.562500000000000000 ) ) ;
#21266 = CARTESIAN_POINT ( 'NONE',  ( 0.1602931993194442739, 0.07955613945526338049, 0.1377952755905511861 ) ) ;
#21267 = CARTESIAN_POINT ( 'NONE',  ( 0.7185039370078760701, -0.06523048226348075740, 0.7012795275590564259 ) ) ;
#21268 = CARTESIAN_POINT ( 'NONE',  ( 1.054774247047244096, 0.000000000000000000, 0.9670275590013542866 ) ) ;
#21269 = VERTEX_POINT ( 'NONE', #39070 ) ;
#21270 = CARTESIAN_POINT ( 'NONE',  ( 0.9873396505805591694, 0.1113553986120547346, 1.471456692913385877 ) ) ;
#21271 = DIRECTION ( 'NONE',  ( 0.000000000000000000, 0.000000000000000000, -1.000000000000000000 ) ) ;
#21272 = CARTESIAN_POINT ( 'NONE',  ( 0.1270800023317771588, 0.09247587545632461603, 0.1270800023317771588 ) ) ;
#21273 = CARTESIAN_POINT ( 'NONE',  ( -0.1787899950787401882, -1.107775590497417362, 0.000000000000000000 ) ) ;
#21274 = CARTESIAN_POINT ( 'NONE',  ( 2.892866454678787531E-17, -1.592519685039370136, 0.1574803149606299191 ) ) ;
#21275 = CYLINDRICAL_SURFACE ( 'NONE', #46680, 0.1377952755905510751 ) ;
#21276 = EDGE_CURVE ( 'NONE', #21602, #7313, #46793, .T. ) ;
#21277 = VECTOR ( 'NONE', #37117, 39.37007874015748854 ) ;
#21278 = ORIENTED_EDGE ( 'NONE', *, *, #20068, .F. ) ;
#21279 = CARTESIAN_POINT ( 'NONE',  ( -0.8019270111902717657, -0.1787899950787401604, 0.04921259837143338034 ) ) ;
#21280 = EDGE_LOOP ( 'NONE', ( #24020, #13642, #7805, #4754 ) ) ;
#21281 = CARTESIAN_POINT ( 'NONE',  ( -0.6971942568897648851, -0.07405724077823297447, 1.938976377898990799 ) ) ;
#21282 = CARTESIAN_POINT ( 'NONE',  ( -1.054774247047244096, 0.000000000000000000, 1.518208661363559031 ) ) ;
#21283 = CARTESIAN_POINT ( 'NONE',  ( -0.8759842519685039353, 0.1787899950787401882, 1.094980314906866203 ) ) ;
#21284 = VECTOR ( 'NONE', #34054, 39.37007874015748143 ) ;
#21285 = CARTESIAN_POINT ( 'NONE',  ( -0.1916154494608382219, 0.07733267719194408807, -0.1748038395390359157 ) ) ;
#21286 = CARTESIAN_POINT ( 'NONE',  ( -1.054774247047244540, 0.07405724077823318263, 1.879921259788756016 ) ) ;
#21287 = CARTESIAN_POINT ( 'NONE',  ( -1.033464566929133799, 0.000000000000000000, 1.466535433070866201 ) ) ;
#21288 = CARTESIAN_POINT ( 'NONE',  ( -1.033464566929133799, 0.000000000000000000, 1.860236220472440971 ) ) ;
#21289 = CARTESIAN_POINT ( 'NONE',  ( 0.2559043235492289292, 0.06578104287837578668, -0.04518399471589295419 ) ) ;
#21290 = CARTESIAN_POINT ( 'NONE',  ( 0.1787899950787401604, -0.2698090075993175296, -0.07405724077823318263 ) ) ;
#21291 = DIRECTION ( 'NONE',  ( 0.000000000000000000, 0.000000000000000000, -1.000000000000000000 ) ) ;
#21292 = FACE_OUTER_BOUND ( 'NONE', #31277, .T. ) ;
#21293 = CARTESIAN_POINT ( 'NONE',  ( -0.6971942568897626646, 0.07405724077823318263, 0.2362204723871814960 ) ) ;
#21294 = EDGE_LOOP ( 'NONE', ( #26952, #39246, #37640, #26910 ) ) ;
#21295 = CARTESIAN_POINT ( 'NONE',  ( -0.7495606340400177148, -0.1264236179284866091, 1.272145669237574772 ) ) ;
#21296 = ORIENTED_EDGE ( 'NONE', *, *, #30947, .T. ) ;
#21297 = EDGE_CURVE ( 'NONE', #23068, #25630, #3141, .T. ) ;
#21298 = CARTESIAN_POINT ( 'NONE',  ( 3.284318927891251994E-17, -1.216043307032850462, 0.1787899950787401882 ) ) ;
#21299 = CARTESIAN_POINT ( 'NONE',  ( 0.1787899950787401882, -1.319389763725763665, -2.189545951927503898E-17 ) ) ;
#21300 = VECTOR ( 'NONE', #32254, 39.37007874015748143 ) ;
#21301 = DIRECTION ( 'NONE',  ( 0.000000000000000000, 0.000000000000000000, 1.000000000000000000 ) ) ;
#21302 = CARTESIAN_POINT ( 'NONE',  ( -1.100456976456230270E-17, -0.6407918410791082486, -0.1797182628040039365 ) ) ;
#21303 = CARTESIAN_POINT ( 'NONE',  ( -0.7646288533564489232, -0.1113553986120547346, 0.9301181101286929431 ) ) ;
#21304 = CARTESIAN_POINT ( 'NONE',  ( -0.7185039370078746268, -0.06523048226347956391, 0.7012795275590552047 ) ) ;
#21305 = EDGE_CURVE ( 'NONE', #23548, #22068, #36224, .T. ) ;
#21306 = CARTESIAN_POINT ( 'NONE',  ( 0.1113553986120547346, -0.1604330708661417249, -0.1113553986120547346 ) ) ;
#21307 = CARTESIAN_POINT ( 'NONE',  ( 1.033464566929134687, -0.06523048226347956391, 1.847933070758615015 ) ) ;
#21308 = ORIENTED_EDGE ( 'NONE', *, *, #3018, .F. ) ;
#21309 = CARTESIAN_POINT ( 'NONE',  ( 0.000000000000000000, 0.000000000000000000, -0.1828167807439035619 ) ) ;
#21310 = CARTESIAN_POINT ( 'NONE',  ( 0.7646288533564489232, -0.1113553986120547346, 0.7824803149606299746 ) ) ;
#21311 = CARTESIAN_POINT ( 'NONE',  ( -0.1184675242425147629, -0.09842519685039327615, 1.224299699984020107 ) ) ;
#21312 = DIRECTION ( 'NONE',  ( 1.766281030386342844E-15, 0.000000000000000000, -1.000000000000000000 ) ) ;
#21314 = CARTESIAN_POINT ( 'NONE',  ( -0.7185039370078739607, 1.928577636452523993E-17, 1.446850393700787274 ) ) ;
#21313 = DIRECTION ( 'NONE',  ( 0.000000000000000000, 0.000000000000000000, 1.000000000000000000 ) ) ;
#21315 = CARTESIAN_POINT ( 'NONE',  ( 0.7646288533564489232, 0.1113553986120547346, 0.2509842518609771700 ) ) ;
#21316 = ORIENTED_EDGE ( 'NONE', *, *, #24215, .F. ) ;
#21317 = ORIENTED_EDGE ( 'NONE', *, *, #20886, .F. ) ;
#21318 = CARTESIAN_POINT ( 'NONE',  ( 0.7185039370078760701, -0.06523048226348075740, 0.8193897637795283240 ) ) ;
#21319 = LINE ( 'NONE', #35950, #17180 ) ;
#21320 = CARTESIAN_POINT ( 'NONE',  ( -9.642888182262618425E-18, -1.562992125876726535, -0.1574803149606299191 ) ) ;
#21321 = CARTESIAN_POINT ( 'NONE',  ( 0.1787899950787401882, -0.5369094487651339120, -2.189545951927503898E-17 ) ) ;
#21322 = CARTESIAN_POINT ( 'NONE',  ( 0.1574803149606300301, -0.9945866141732289112, 0.06523048226347956391 ) ) ;
#21323 = CARTESIAN_POINT ( 'NONE',  ( 0.7646288533564489232, -0.1113553986120547346, 0.9694881888688504645 ) ) ;
#21324 = CARTESIAN_POINT ( 'NONE',  ( 0.8759842519685039353, 0.1574803149606299191, 0.5314960629921260393 ) ) ;
#21325 = CARTESIAN_POINT ( 'NONE',  ( -0.7495606340400177148, -0.1264236179284866091, 0.3617125983714334359 ) ) ;
#21326 = ORIENTED_EDGE ( 'NONE', *, *, #41625, .T. ) ;
#21327 = CARTESIAN_POINT ( 'NONE',  ( -0.9500414927467378812, -0.1787899950787401604, 1.594488188922613237 ) ) ;
#21328 = ORIENTED_EDGE ( 'NONE', *, *, #26606, .F. ) ;
#21329 = CARTESIAN_POINT ( 'NONE',  ( 1.002407869896990045, -0.1264236179284866091, 1.557578740103716441 ) ) ;
#21330 = CARTESIAN_POINT ( 'NONE',  ( 0.1602931993194442739, -0.07955613945526357478, -0.1377952755905511861 ) ) ;
#21331 = CARTESIAN_POINT ( 'NONE',  ( -1.054774247047244540, -0.07405724077823318263, 0.5757874015210394658 ) ) ;
#21332 = CARTESIAN_POINT ( 'NONE',  ( 0.9500414927467378812, 0.1787899950787401604, 0.1919291338045042428 ) ) ;
#21333 = DIRECTION ( 'NONE',  ( -1.000000000000000000, 0.000000000000000000, 0.000000000000000000 ) ) ;
#21334 = CARTESIAN_POINT ( 'NONE',  ( 0.8759842519685039353, -0.1787899950787401882, 0.7652559054580472253 ) ) ;
#21335 = CARTESIAN_POINT ( 'NONE',  ( -0.7495606340400177148, 0.1264236179284866091, 0.7455708660879684091 ) ) ;
#21336 = CARTESIAN_POINT ( 'NONE',  ( 0.000000000000000000, -0.09842519685039370636, 0.000000000000000000 ) ) ;
#21337 = VECTOR ( 'NONE', #38427, 39.37007874015748143 ) ;
#21338 = DIRECTION ( 'NONE',  ( 1.822029033848725028E-16, 0.000000000000000000, 1.000000000000000000 ) ) ;
#21339 = CARTESIAN_POINT ( 'NONE',  ( 0.06523048226347956391, -0.2662401573727879445, -0.1574803149606300301 ) ) ;
#21340 = CARTESIAN_POINT ( 'NONE',  ( -0.9500414927467378812, 0.1787899950787401604, 1.373031496009229135 ) ) ;
#21341 = ORIENTED_EDGE ( 'NONE', *, *, #26096, .T. ) ;
#21342 = CARTESIAN_POINT ( 'NONE',  ( -1.033464566929134687, 0.06523048226347956391, 1.468996062992126150 ) ) ;
#21343 = CARTESIAN_POINT ( 'NONE',  ( -0.7185039370078746268, 0.06523048226347956391, 0.3813976377952755237 ) ) ;
#21344 = AXIS2_PLACEMENT_3D ( 'NONE', #2106, #34732, #13161 ) ;
#21345 = CARTESIAN_POINT ( 'NONE',  ( 0.9500414927467377701, -0.1787899950787401604, 1.515748031442299526 ) ) ;
#21346 = CARTESIAN_POINT ( 'NONE',  ( -0.1674536925976815027, -0.09851383442626908404, 0.03546406509531940809 ) ) ;
#21347 = ORIENTED_EDGE ( 'NONE', *, *, #30488, .T. ) ;
#21348 = CIRCLE ( 'NONE', #4495, 0.2471922904502826812 ) ;
#21349 = CARTESIAN_POINT ( 'NONE',  ( -0.1264236179284866091, -1.674828692638687277, -0.1264236179284866091 ) ) ;
#21350 = ORIENTED_EDGE ( 'NONE', *, *, #5250, .T. ) ;
#21351 = DIRECTION ( 'NONE',  ( 1.000000000000000000, -0.000000000000000000, -0.000000000000000000 ) ) ;
#21352 = ORIENTED_EDGE ( 'NONE', *, *, #16140, .T. ) ;
#21353 = CARTESIAN_POINT ( 'NONE',  ( 0.8019270111902717657, 0.1787899950787401604, 1.412401574749386990 ) ) ;
#21354 = EDGE_CURVE ( 'NONE', #37269, #23265, #3377, .T. ) ;
#21355 = DIRECTION ( 'NONE',  ( 0.000000000000000000, -0.6156614753256598460, -0.7880107536067207930 ) ) ;
#21356 = CARTESIAN_POINT ( 'NONE',  ( -1.094772975963752103E-17, -0.3302165353793074520, -0.1787899950787401882 ) ) ;
#21357 = ADVANCED_FACE ( 'NONE', ( #39772 ), #29058, .T. ) ;
#21358 = CARTESIAN_POINT ( 'NONE',  ( -1.094772975963752103E-17, -0.8371062991588346103, -0.1787899950787401882 ) ) ;
#21359 = DIRECTION ( 'NONE',  ( 0.000000000000000000, 0.000000000000000000, 1.000000000000000000 ) ) ;
#21360 = FACE_OUTER_BOUND ( 'NONE', #28584, .T. ) ;
#21361 = CARTESIAN_POINT ( 'NONE',  ( 0.9500414927467378812, -0.1787899950787401604, 0.2903543306548980185 ) ) ;
#21362 = EDGE_CURVE ( 'NONE', #32919, #6075, #18229, .T. ) ;
#21363 = CARTESIAN_POINT ( 'NONE',  ( 0.1787899950787401604, -0.1516987713788451320, -0.07405724077823318263 ) ) ;
#21364 = CARTESIAN_POINT ( 'NONE',  ( 0.1787899950787401604, -0.2933070865604095467, -0.07405724077823318263 ) ) ;
#21365 = CARTESIAN_POINT ( 'NONE',  ( -0.1787899950787401604, 0.07578740162856664742, 0.07405724077823318263 ) ) ;
#21366 = CARTESIAN_POINT ( 'NONE',  ( 0.2559055118110236116, -0.09499862663905693505, -0.3051626384476439635 ) ) ;
#21367 = CYLINDRICAL_SURFACE ( 'NONE', #16870, 0.09842519685039310962 ) ;
#21368 = EDGE_CURVE ( 'NONE', #33104, #30751, #3745, .T. ) ;
#21369 = CARTESIAN_POINT ( 'NONE',  ( 0.9500414927467378812, -0.1787899950787401604, 0.6446850393163160442 ) ) ;
#21370 = ( BOUNDED_CURVE ( )  B_SPLINE_CURVE ( 2, ( #27578, #19638, #9342, #42129, #31399, #42380, #5733, #23491, #45970 ),
 .UNSPECIFIED., .F., .T. ) 
 B_SPLINE_CURVE_WITH_KNOTS ( ( 3, 2, 2, 2, 3 ),
 ( 0.8900000000000000133, 0.8924999999999999600, 0.8950000000000000178, 0.8974999999999999645, 0.9000000000000000222 ),
 .UNSPECIFIED. ) 
 CURVE ( )  GEOMETRIC_REPRESENTATION_ITEM ( )  RATIONAL_B_SPLINE_CURVE ( ( 1.000000000000000000, 0.9238795325112869605, 1.000000000000000000, 0.9238795325112869605, 1.000000000000000000, 0.9238795325112869605, 1.000000000000000000, 0.9238795325112869605, 1.000000000000000000 ) ) 
 REPRESENTATION_ITEM ( '' )  ) ;
#21371 = CARTESIAN_POINT ( 'NONE',  ( -1.002407869896990045, 0.1264236179284866091, 1.016240157426551161 ) ) ;
#21372 = CIRCLE ( 'NONE', #24461, 0.09842519685039370636 ) ;
#21374 = DIRECTION ( 'NONE',  ( 1.000000000000000000, 0.000000000000000000, 0.000000000000000000 ) ) ;
#21373 = DIRECTION ( 'NONE',  ( 0.000000000000000000, 0.000000000000000000, -1.000000000000000000 ) ) ;
#21376 = CARTESIAN_POINT ( 'NONE',  ( -0.8898633633897504724, -0.1743928684788044192, 1.988427853007691981 ) ) ;
#21375 = CARTESIAN_POINT ( 'NONE',  ( -0.1270800023317771588, -1.777602864701157692, -0.1270800023317771588 ) ) ;
#21377 = DIRECTION ( 'NONE',  ( 1.000000000000000000, -0.000000000000000000, -0.000000000000000000 ) ) ;
#21378 = CARTESIAN_POINT ( 'NONE',  ( 1.054774247047244096, 0.000000000000000000, 1.641240157426551161 ) ) ;
#21380 = CARTESIAN_POINT ( 'NONE',  ( 0.1606807218938896276, 0.1591122674893432898, -1.978207022268160401E-08 ) ) ;
#21379 = CARTESIAN_POINT ( 'NONE',  ( 0.8019270111902716547, 0.1787899950787401604, 1.963582677111591401 ) ) ;
#21381 = ORIENTED_EDGE ( 'NONE', *, *, #5406, .T. ) ;
#21382 = CARTESIAN_POINT ( 'NONE',  ( 0.1596650774283295271, -0.1494101348903348336, 0.02216197906078582955 ) ) ;
#21383 = CARTESIAN_POINT ( 'NONE',  ( -0.1264236179284866091, -0.1284448818360001965, -0.1264236179284866091 ) ) ;
#21384 = VECTOR ( 'NONE', #11355, 39.37007874015748143 ) ;
#21385 = CARTESIAN_POINT ( 'NONE',  ( 0.7495606340400177148, 0.1264236179284866091, 0.6668307086076534773 ) ) ;
#21386 = CARTESIAN_POINT ( 'NONE',  ( 0.1264236179284866091, -1.038877952702141672, -0.1264236179284866091 ) ) ;
#21387 = CARTESIAN_POINT ( 'NONE',  ( 1.054774247047244096, 0.000000000000000000, 0.1451771653005673179 ) ) ;
#21388 = CARTESIAN_POINT ( 'NONE',  ( 0.3161444924769554743, 1.357244529069700612, -1.397888825503271759 ) ) ;
#21389 = CARTESIAN_POINT ( 'NONE',  ( -1.054774247047244540, -0.07405724077823318263, 1.594488188922613237 ) ) ;
#21390 = EDGE_LOOP ( 'NONE', ( #26714, #7714, #43990, #24094 ) ) ;
#21391 = CARTESIAN_POINT ( 'NONE',  ( 1.033464566929133799, 0.000000000000000000, 0.1673228346456692994 ) ) ;
#21392 = CARTESIAN_POINT ( 'NONE',  ( 0.9500414927467378812, -0.1787899950787401604, 1.161417322780881278 ) ) ;
#21393 = CARTESIAN_POINT ( 'NONE',  ( 0.1113553986120547346, -1.144685039262551163, 0.1113553986120547346 ) ) ;
#21394 = LINE ( 'NONE', #13979, #17186 ) ;
#21395 = CARTESIAN_POINT ( 'NONE',  ( 0.6971942568897648851, 0.07405724077823318263, 1.850393700733638624 ) ) ;
#21396 = CARTESIAN_POINT ( 'NONE',  ( -0.7646288533564489232, 0.1113553986120547346, 0.5757874015748032370 ) ) ;
#21397 = CARTESIAN_POINT ( 'NONE',  ( -0.6971942568897637749, 2.189545951927499583E-17, 0.8686023621509606496 ) ) ;
#21398 = CARTESIAN_POINT ( 'NONE',  ( -0.7646288533564489232, -0.1113553986120547346, 1.609251968503937036 ) ) ;
#21399 = DIRECTION ( 'NONE',  ( 0.000000000000000000, -1.000000000000000000, 0.000000000000000000 ) ) ;
#21400 = CARTESIAN_POINT ( 'NONE',  ( 0.7495606340400177148, 0.1264236179284866091, 0.2386811023084413619 ) ) ;
#21401 = CARTESIAN_POINT ( 'NONE',  ( -0.6971942568897626646, 0.07405724077823318263, 0.1968503936470238636 ) ) ;
#21402 = CARTESIAN_POINT ( 'NONE',  ( -1.002407869896990045, 0.1264236179284866091, 0.6569881889226141247 ) ) ;
#21403 = CARTESIAN_POINT ( 'NONE',  ( 0.7185039370078746268, 0.06523048226347956391, 1.592027558947591848 ) ) ;
#21404 = VERTEX_POINT ( 'NONE', #11521 ) ;
#21405 = CARTESIAN_POINT ( 'NONE',  ( 0.1787899950787401604, 0.05610236225848794223, -0.07405724077823318263 ) ) ;
#21406 = CARTESIAN_POINT ( 'NONE',  ( 0.8019270111902717657, 0.1787899950787401604, 0.7480314960092282472 ) ) ;
#21407 = CARTESIAN_POINT ( 'NONE',  ( -1.002407869896990045, -0.1264236179284866091, 1.788877952702141672 ) ) ;
#21408 = ORIENTED_EDGE ( 'NONE', *, *, #5694, .F. ) ;
#21409 = CARTESIAN_POINT ( 'NONE',  ( -0.2471922904502826812, 0.09773636000336974328, -0.01649811039748649497 ) ) ;
#21410 = VECTOR ( 'NONE', #30869, 39.37007874015748143 ) ;
#21411 = DIRECTION ( 'NONE',  ( 3.385139170096289319E-15, 1.000000000000000000, 0.000000000000000000 ) ) ;
#21412 = CARTESIAN_POINT ( 'NONE',  ( -0.1264236179284866091, -1.241757826496954875, -0.1264236179284866091 ) ) ;
#21413 = ORIENTED_EDGE ( 'NONE', *, *, #31931, .F. ) ;
#21414 = CARTESIAN_POINT ( 'NONE',  ( 0.1264236179284866091, -0.2219488188438744347, 0.1264236179284866091 ) ) ;
#21415 = ORIENTED_EDGE ( 'NONE', *, *, #6804, .F. ) ;
#21416 = CARTESIAN_POINT ( 'NONE',  ( 0.8759842519685039353, -0.1787899950787401882, 1.114665354276944909 ) ) ;
#21417 = CARTESIAN_POINT ( 'NONE',  ( 0.4509871776442260227, 4.466152701071653354E-17, 0.000000000000000000 ) ) ;
#21418 = CIRCLE ( 'NONE', #8389, 0.7874015748031496509 ) ;
#21419 = DIRECTION ( 'NONE',  ( 0.000000000000000000, 0.000000000000000000, 1.000000000000000000 ) ) ;
#21420 = EDGE_CURVE ( 'NONE', #31223, #16843, #18390, .T. ) ;
#21421 = CARTESIAN_POINT ( 'NONE',  ( 1.033464566929134687, 0.06523048226347956391, 1.941437007874014187 ) ) ;
#21422 = CARTESIAN_POINT ( 'NONE',  ( -0.07405724077823318263, -1.612204724355685403, 0.1787899950787401604 ) ) ;
#21423 = EDGE_CURVE ( 'NONE', #3237, #36143, #40250, .T. ) ;
#21424 = CARTESIAN_POINT ( 'NONE',  ( -0.6971942568897648851, -0.07405724077823297447, 0.5216535432533228045 ) ) ;
#21426 = CARTESIAN_POINT ( 'NONE',  ( -0.7124453589342143456, -0.03434907305620428508, 1.983904522674447390 ) ) ;
#21425 = CARTESIAN_POINT ( 'NONE',  ( 0.1270800023317771588, -1.275634360764147601, -0.1270800023317771588 ) ) ;
#21427 = DIRECTION ( 'NONE',  ( -1.363218471095259303E-17, -0.6156614753256575145, -0.7880107536067225693 ) ) ;
#21428 = CARTESIAN_POINT ( 'NONE',  ( 1.002407869896990045, -0.1264236179284866091, 1.163877952702141672 ) ) ;
#21429 = CARTESIAN_POINT ( 'NONE',  ( 0.8019270111902716547, 0.1787899950787401604, 1.569881889710015299 ) ) ;
#21430 = CARTESIAN_POINT ( 'NONE',  ( 0.8107537697050253289, 0.1574803149606300301, 1.715059055118110631 ) ) ;
#21431 = CARTESIAN_POINT ( 'NONE',  ( 1.033464566929133799, 0.000000000000000000, 0.009842519685039369942 ) ) ;
#21432 = LINE ( 'NONE', #43232, #10559 ) ;
#21433 = CARTESIAN_POINT ( 'NONE',  ( 0.9873396505805591694, -0.1113553986120547346, 0.7824803148531023211 ) ) ;
#21434 = CARTESIAN_POINT ( 'NONE',  ( -1.033464566929134687, -0.06523048226347956391, 1.808562992018457383 ) ) ;
#21435 = CARTESIAN_POINT ( 'NONE',  ( -0.1264236179284866091, 0.04379921265218866822, 0.1264236179284866091 ) ) ;
#21436 = CARTESIAN_POINT ( 'NONE',  ( 0.7495606340400177148, 0.1264236179284866091, 0.2337598424659216578 ) ) ;
#21437 = CARTESIAN_POINT ( 'NONE',  ( 0.7318012926787728079, -0.08735924986328225117, 0.03937095280083596077 ) ) ;
#21439 = CARTESIAN_POINT ( 'NONE',  ( -0.7646288533564489232, 0.1113553986120547346, 1.825787401467275473 ) ) ;
#21438 = CARTESIAN_POINT ( 'NONE',  ( 1.054774247047244540, 0.07405724077823318263, 1.205708661363558365 ) ) ;
#21440 = CARTESIAN_POINT ( 'NONE',  ( 0.7185039370078739607, 1.928577636452523993E-17, 1.053149606299212504 ) ) ;
#21441 = CARTESIAN_POINT ( 'NONE',  ( 0.7646288533564489232, 0.1113553986120547346, 0.4478346455617645550 ) ) ;
#21442 = ORIENTED_EDGE ( 'NONE', *, *, #36491, .T. ) ;
#21443 = CARTESIAN_POINT ( 'NONE',  ( 0.9617971027165344022, 0.1454179922531197988, 0.03936767230047344412 ) ) ;
#21444 = PRODUCT_DEFINITION_SHAPE ( 'NONE', 'NONE',  #47478 ) ;
#21445 = CARTESIAN_POINT ( 'NONE',  ( -1.033464566929133799, 0.000000000000000000, 0.4724409447743622148 ) ) ;
#21446 = CARTESIAN_POINT ( 'NONE',  ( -1.033464566929134687, -0.06523048226347956391, 1.542814960629921073 ) ) ;
#21447 = CARTESIAN_POINT ( 'NONE',  ( 0.7495606340400177148, 0.1264236179284866091, 1.375492125930488196 ) ) ;
#21449 = CARTESIAN_POINT ( 'NONE',  ( -1.033464566929133799, 0.000000000000000000, 0.2755905510735752184 ) ) ;
#21448 = CARTESIAN_POINT ( 'NONE',  ( -0.7646288533564489232, 0.1113553986120547346, 0.1033464566929133965 ) ) ;
#21450 = CARTESIAN_POINT ( 'NONE',  ( 0.07405724077823318263, 0.01181102367581074800, 0.1787899950787401604 ) ) ;
#21451 = EDGE_LOOP ( 'NONE', ( #28328, #26340, #16246, #16732 ) ) ;
#21452 = CARTESIAN_POINT ( 'NONE',  ( 0.1631243713103771309, -0.07417819129880506845, -0.1405411351623387928 ) ) ;
#21453 = VERTEX_POINT ( 'NONE', #29309 ) ;
#21454 = CARTESIAN_POINT ( 'NONE',  ( 0.8107537697050254399, -0.1574803149606297803, 1.286909448711370585 ) ) ;
#21455 = DIRECTION ( 'NONE',  ( 0.000000000000000000, -1.000000000000000000, 0.000000000000000000 ) ) ;
#21456 = ORIENTED_EDGE ( 'NONE', *, *, #31785, .T. ) ;
#21457 = CARTESIAN_POINT ( 'NONE',  ( 0.6971942568897637749, 2.189545951927499583E-17, 0.5585629920722204877 ) ) ;
#21458 = ORIENTED_EDGE ( 'NONE', *, *, #19041, .T. ) ;
#21459 = CARTESIAN_POINT ( 'NONE',  ( -1.054774247047244540, 0.07405724077823318263, 1.481299212544662902 ) ) ;
#21460 = CARTESIAN_POINT ( 'NONE',  ( -0.1787899950787401604, -1.774606299158834277, 0.07405724077823318263 ) ) ;
#21461 = CARTESIAN_POINT ( 'NONE',  ( -0.9500414927467378812, -0.1787899950787401604, 1.122047244040725644 ) ) ;
#21462 = CARTESIAN_POINT ( 'NONE',  ( -0.8759842519685039353, -0.1574803149606299191, 0.1181102362204724532 ) ) ;
#21463 = ORIENTED_EDGE ( 'NONE', *, *, #6648, .F. ) ;
#21464 = CARTESIAN_POINT ( 'NONE',  ( -1.054774247047244540, -0.07405724077823318263, 1.082677165300567346 ) ) ;
#21465 = DIRECTION ( 'NONE',  ( -1.177520686924230272E-15, -0.7880107536067199048, 0.6156614753256609562 ) ) ;
#21466 = CARTESIAN_POINT ( 'NONE',  ( 1.033464566929133799, 0.000000000000000000, 0.7874015746956221085 ) ) ;
#21467 = CARTESIAN_POINT ( 'NONE',  ( 3.284318927891251994E-17, -0.8726633383079782647, 0.1787899950787401882 ) ) ;
#21468 = ORIENTED_EDGE ( 'NONE', *, *, #15135, .F. ) ;
#21469 = CARTESIAN_POINT ( 'NONE',  ( -0.1126596323294454804, -0.08956130712551850503, 0.1148527042348372190 ) ) ;
#21470 = CARTESIAN_POINT ( 'NONE',  ( 0.8075642843603819676, 0.1651804176431314886, 0.03937007863263043694 ) ) ;
#21471 = ORIENTED_EDGE ( 'NONE', *, *, #19039, .F. ) ;
#21472 = CARTESIAN_POINT ( 'NONE',  ( 0.7646288533564489232, 0.1113553986120547346, 0.7726377952755906220 ) ) ;
#21473 = CARTESIAN_POINT ( 'NONE',  ( -0.8759842519685039353, 0.1574803149606299191, 0.5610236219397165547 ) ) ;
#21474 = CARTESIAN_POINT ( 'NONE',  ( -1.054774247047244540, 0.07405724077823318263, 0.6545275590013545086 ) ) ;
#21475 = ADVANCED_FACE ( 'NONE', ( #25674 ), #10588, .T. ) ;
#21477 = VERTEX_POINT ( 'NONE', #14881 ) ;
#21476 = AXIS2_PLACEMENT_3D ( 'NONE', #24178, #2340, #16971 ) ;
#21478 = CARTESIAN_POINT ( 'NONE',  ( -0.8759842519685039353, 0.1787899950787401882, 1.808562992072220377 ) ) ;
#21479 = VECTOR ( 'NONE', #16918, 39.37007874015748143 ) ;
#21480 = EDGE_CURVE ( 'NONE', #22163, #33650, #46564, .T. ) ;
#21481 = VECTOR ( 'NONE', #37189, 39.37007874015748143 ) ;
#21482 = LINE ( 'NONE', #28960, #9655 ) ;
#21483 = ( BOUNDED_CURVE ( )  B_SPLINE_CURVE ( 2, ( #16152, #35540, #32667, #13954, #13490, #46299, #21620, #29089, #39337 ),
 .UNSPECIFIED., .F., .F. ) 
 B_SPLINE_CURVE_WITH_KNOTS ( ( 3, 2, 2, 2, 3 ),
 ( 0.4799999999999999822, 0.4824999999999999845, 0.4849999999999999867, 0.4874999999999999889, 0.4899999999999999911 ),
 .UNSPECIFIED. ) 
 CURVE ( )  GEOMETRIC_REPRESENTATION_ITEM ( )  RATIONAL_B_SPLINE_CURVE ( ( 1.000000000000000000, 0.9238795325112869605, 1.000000000000000000, 0.9238795325112869605, 1.000000000000000000, 0.9238795325112869605, 1.000000000000000000, 0.9238795325112869605, 1.000000000000000000 ) ) 
 REPRESENTATION_ITEM ( '' )  ) ;
#21484 = CARTESIAN_POINT ( 'NONE',  ( -0.7747078546254108078, 0.1515708385138800074, 0.04064907247438850901 ) ) ;
#21485 = ORIENTED_EDGE ( 'NONE', *, *, #4540, .F. ) ;
#21486 = CARTESIAN_POINT ( 'NONE',  ( 0.9412147342319837628, 0.1574803149606300301, 0.6865157480314957317 ) ) ;
#21487 = CARTESIAN_POINT ( 'NONE',  ( 3.301370929368692659E-17, -0.8179571954098169284, 0.1797182628040039365 ) ) ;
#21488 = CARTESIAN_POINT ( 'NONE',  ( 0.8759842519685039353, 0.000000000000000000, 4.498031496062992574 ) ) ;
#21489 = CARTESIAN_POINT ( 'NONE',  ( -0.9873396505805591694, 0.1113553986120547346, 1.382874015640503940 ) ) ;
#21490 = CARTESIAN_POINT ( 'NONE',  ( 0.6971942568897637749, 2.189545951927499583E-17, 0.7160433070328504623 ) ) ;
#21491 = CARTESIAN_POINT ( 'NONE',  ( 0.1574803149606299191, -0.6377952755905511584, -1.928577636452523993E-17 ) ) ;
#21492 = CARTESIAN_POINT ( 'NONE',  ( 0.7185039370078739607, 1.928577636452523993E-17, 1.879921259842519676 ) ) ;
#21493 = CARTESIAN_POINT ( 'NONE',  ( -0.2559055118110236671, 0.04128066261331859998, -0.03449252736539444586 ) ) ;
#21494 = CARTESIAN_POINT ( 'NONE',  ( 0.8107537697050253289, -0.1574803149606297803, 1.336122047244094446 ) ) ;
#21496 = CARTESIAN_POINT ( 'NONE',  ( 0.1377952755905512139, -1.365923996832131609E-16, 0.7066929133858274037 ) ) ;
#21495 = CARTESIAN_POINT ( 'NONE',  ( 0.8107812902180758785, -0.1596208643658766357, 1.986974409371305095 ) ) ;
#21497 = FACE_OUTER_BOUND ( 'NONE', #26849, .T. ) ;
#21499 = CARTESIAN_POINT ( 'NONE',  ( 0.7646288533564489232, -0.1113553986120547346, 0.2608267715460165226 ) ) ;
#21498 = CARTESIAN_POINT ( 'NONE',  ( 0.7495606340400177148, -0.1264236179284866091, 0.6766732282926929409 ) ) ;
#21500 = CARTESIAN_POINT ( 'NONE',  ( -0.1264236179284866091, -0.6648622046706456068, 0.1264236179284866091 ) ) ;
#21501 = DIRECTION ( 'NONE',  ( 3.469446951953613794E-15, 1.000000000000000000, 0.000000000000000000 ) ) ;
#21502 = EDGE_LOOP ( 'NONE', ( #19598, #13471, #21788, #1351 ) ) ;
#21503 = CARTESIAN_POINT ( 'NONE',  ( 0.1626913500577309712, 0.07997639175683110557, 0.1385232029213226412 ) ) ;
#21504 = CARTESIAN_POINT ( 'NONE',  ( 0.1565984635743036257, 0.01350052470346802501, -0.1403812994534590630 ) ) ;
#21505 = CARTESIAN_POINT ( 'NONE',  ( 1.002407869896990045, -0.1264236179284866091, 1.001476377898992132 ) ) ;
#21506 = CARTESIAN_POINT ( 'NONE',  ( 0.1377952755905511861, 0.1574803149606299191, -0.8070866141732283561 ) ) ;
#21507 = CARTESIAN_POINT ( 'NONE',  ( -1.100456976456230270E-17, 0.02849949750356862294, -0.1797182628040039365 ) ) ;
#21508 = CARTESIAN_POINT ( 'NONE',  ( -1.094772975963752103E-17, -1.196358267662771757, -0.1787899950787401882 ) ) ;
#21509 = CARTESIAN_POINT ( 'NONE',  ( -0.1574803149606297803, -1.481791338582676643, 0.06523048226347956391 ) ) ;
#21510 = ADVANCED_FACE ( 'NONE', ( #8617 ), #34980, .F. ) ;
#21511 = CARTESIAN_POINT ( 'NONE',  ( 0.7185039370078739607, 0.000000000000000000, 4.498031496062992574 ) ) ;
#21512 = ORIENTED_EDGE ( 'NONE', *, *, #44949, .T. ) ;
#21513 = CARTESIAN_POINT ( 'NONE',  ( -1.054774247047244540, 0.07405724077823318263, 0.06397637789899228433 ) ) ;
#21514 = CARTESIAN_POINT ( 'NONE',  ( 0.8019270111902717657, -0.1787899950787401604, 1.943897637741510254 ) ) ;
#21515 = VERTEX_POINT ( 'NONE', #7372 ) ;
#21516 = CARTESIAN_POINT ( 'NONE',  ( 3.284318927891251994E-17, -1.412893700733637958, 0.1787899950787401882 ) ) ;
#21517 = CARTESIAN_POINT ( 'NONE',  ( -0.7185039370078746268, -0.06523048226347956391, 1.843011811023621327 ) ) ;
#21518 = AXIS2_PLACEMENT_3D ( 'NONE', #15973, #37517, #30596 ) ;
#21519 = VECTOR ( 'NONE', #3124, 39.37007874015748143 ) ;
#21520 = CARTESIAN_POINT ( 'NONE',  ( -0.7495606340400177148, -0.1264236179284866091, 1.700295275536787498 ) ) ;
#21521 = CARTESIAN_POINT ( 'NONE',  ( 0.8759842519685039353, 0.1787899950787401882, 0.9030511810485984947 ) ) ;
#21522 = CIRCLE ( 'NONE', #22266, 0.009842519685039354330 ) ;
#21523 = CARTESIAN_POINT ( 'NONE',  ( -0.7495606340400177148, 0.1264236179284866091, 0.3567913385289137596 ) ) ;
#21524 = CARTESIAN_POINT ( 'NONE',  ( 1.033464566929133799, 0.000000000000000000, 0.5511811022546778682 ) ) ;
#21525 = CARTESIAN_POINT ( 'NONE',  ( -1.054774247047244096, 0.000000000000000000, 1.877460629867496067 ) ) ;
#21526 = CARTESIAN_POINT ( 'NONE',  ( -0.8759842519685039353, 0.1574803149606299191, 1.476377952755905554 ) ) ;
#21527 = CARTESIAN_POINT ( 'NONE',  ( -0.7185039370078739607, 1.928577636452523993E-17, 1.840551181102362266 ) ) ;
#21528 = CARTESIAN_POINT ( 'NONE',  ( 0.2559055118110210025, 0.007196880244715129354, -0.02740704184215201136 ) ) ;
#21529 = CARTESIAN_POINT ( 'NONE',  ( -0.07405724077823318263, -0.4026830233473494003, 0.1787899950787401604 ) ) ;
#21530 = EDGE_CURVE ( 'NONE', #40723, #13679, #45241, .T. ) ;
#21531 = CARTESIAN_POINT ( 'NONE',  ( -0.1028752476446956748, -0.09842519685039370636, 0.1273875674447041140 ) ) ;
#21532 = CARTESIAN_POINT ( 'NONE',  ( 0.4509871776442260227, -0.09842519685039370636, 0.000000000000000000 ) ) ;
#21533 = CARTESIAN_POINT ( 'NONE',  ( -0.1377952755905511861, -1.331775896911328393E-15, 0.8070866141732283561 ) ) ;
#21534 = EDGE_CURVE ( 'NONE', #40174, #17524, #32069, .T. ) ;
#21535 = CARTESIAN_POINT ( 'NONE',  ( -1.054774247047244540, 0.07405724077823318263, 0.1427165353793072855 ) ) ;
#21536 = EDGE_CURVE ( 'NONE', #9918, #32777, #7807, .T. ) ;
#21537 = ORIENTED_EDGE ( 'NONE', *, *, #40284, .F. ) ;
#21538 = ORIENTED_EDGE ( 'NONE', *, *, #22025, .T. ) ;
#21539 = CARTESIAN_POINT ( 'NONE',  ( -1.054774247047244540, -0.07405724077823318263, 1.363188976324188673 ) ) ;
#21540 = ORIENTED_EDGE ( 'NONE', *, *, #21660, .T. ) ;
#21541 = EDGE_CURVE ( 'NONE', #5864, #43030, #46899, .T. ) ;
#21542 = CARTESIAN_POINT ( 'NONE',  ( -0.07405724077823318263, -1.179133858213953001, 0.1787899950787401604 ) ) ;
#21543 = CARTESIAN_POINT ( 'NONE',  ( 0.07405724077823318263, -1.390748031442299082, -0.1787899950787401604 ) ) ;
#21544 = VECTOR ( 'NONE', #439, 39.37007874015748143 ) ;
#21545 = FACE_BOUND ( 'NONE', #34728, .T. ) ;
#21546 = CARTESIAN_POINT ( 'NONE',  ( 0.7185039370078739607, 1.928577636452523993E-17, 0.3444881889763780070 ) ) ;
#21547 = CARTESIAN_POINT ( 'NONE',  ( -1.033464566929134687, -0.06523048226347956391, 0.2436023622047245041 ) ) ;
#21548 = CARTESIAN_POINT ( 'NONE',  ( -0.9412147342319837628, -0.1574803149606297803, 0.9768700786326298680 ) ) ;
#21549 = CARTESIAN_POINT ( 'NONE',  ( -0.8107537697050253289, 0.1574803149606300301, 0.9276574803149607584 ) ) ;
#21550 = CARTESIAN_POINT ( 'NONE',  ( 1.054774247047244096, 0.000000000000000000, 0.4601377952218267953 ) ) ;
#21551 = AXIS2_PLACEMENT_3D ( 'NONE', #11213, #19325, #29924 ) ;
#21552 = CARTESIAN_POINT ( 'NONE',  ( 0.7185039370078739607, 1.928577636452523993E-17, 1.751968503829480106 ) ) ;
#21553 = ORIENTED_EDGE ( 'NONE', *, *, #9036, .T. ) ;
#21554 = CARTESIAN_POINT ( 'NONE',  ( -0.2066929133858267931, 0.3648440108500937140, -3.619166627704267114 ) ) ;
#21555 = CARTESIAN_POINT ( 'NONE',  ( 0.7185039370078739607, 1.928577636452523993E-17, 0.7381889763779527769 ) ) ;
#21556 = AXIS2_PLACEMENT_3D ( 'NONE', #7819, #29458, #44003 ) ;
#21557 = CARTESIAN_POINT ( 'NONE',  ( 0.1644020957507539848, -0.08115590401245571794, -0.1405661490837558925 ) ) ;
#21558 = CARTESIAN_POINT ( 'NONE',  ( -0.3551574803149606385, -0.1574803149606299191, 0.000000000000000000 ) ) ;
#21560 = CARTESIAN_POINT ( 'NONE',  ( 0.1618536817989234267, -0.08807120157698605789, -0.1284887221114794087 ) ) ;
#21559 = FACE_OUTER_BOUND ( 'NONE', #25663, .T. ) ;
#21561 = CARTESIAN_POINT ( 'NONE',  ( 0.9873396505805591694, 0.1113553986120547346, 0.1624015746956226358 ) ) ;
#21562 = ORIENTED_EDGE ( 'NONE', *, *, #11600, .F. ) ;
#21563 = CARTESIAN_POINT ( 'NONE',  ( 0.8759842519685039353, -0.1574803149606299191, 0.2362204724409449064 ) ) ;
#21564 = CARTESIAN_POINT ( 'NONE',  ( 0.7185039370078766252, -0.06523048226348168721, 1.833169291231055542 ) ) ;
#21565 = CARTESIAN_POINT ( 'NONE',  ( 2.892866454678787531E-17, -1.543307086506645609, 0.1574803149606299191 ) ) ;
#21566 = CARTESIAN_POINT ( 'NONE',  ( 3.284318927891251994E-17, -0.7829724408911181710, 0.1787899950787401882 ) ) ;
#21567 = CARTESIAN_POINT ( 'NONE',  ( -0.8759842519685039353, -0.1574803149606299191, 0.1476377951680635792 ) ) ;
#21568 = CARTESIAN_POINT ( 'NONE',  ( 0.1574803149606299191, -1.031496062992126150, -1.928577636452523993E-17 ) ) ;
#21569 = CARTESIAN_POINT ( 'NONE',  ( 0.9412147342319837628, 0.1574803149606300301, 0.9522637794200313754 ) ) ;
#21570 = DIRECTION ( 'NONE',  ( 0.000000000000000000, 0.000000000000000000, 1.000000000000000000 ) ) ;
#21571 = CARTESIAN_POINT ( 'NONE',  ( -1.054774247047244540, 0.07405724077823318263, 0.4183070865604097133 ) ) ;
#21572 = ORIENTED_EDGE ( 'NONE', *, *, #32539, .T. ) ;
#21573 = ORIENTED_EDGE ( 'NONE', *, *, #16669, .F. ) ;
#21574 = CARTESIAN_POINT ( 'NONE',  ( -0.8759842519685039353, 0.1787899950787401882, 1.651082677111590513 ) ) ;
#21575 = ORIENTED_EDGE ( 'NONE', *, *, #429, .F. ) ;
#21576 = CARTESIAN_POINT ( 'NONE',  ( 1.054774247047244540, 0.07405724077823318263, 1.486220472387181690 ) ) ;
#21577 = CARTESIAN_POINT ( 'NONE',  ( -0.6971942568897626646, -0.07405724077823297447, 0.7972440944344250102 ) ) ;
#21578 = CARTESIAN_POINT ( 'NONE',  ( 1.002407869896990045, 0.1264236179284866091, 0.1500984251430867999 ) ) ;
#21579 = CARTESIAN_POINT ( 'NONE',  ( -0.9412147342319837628, -0.1574803149606297803, 1.685531495955465697 ) ) ;
#21580 = CARTESIAN_POINT ( 'NONE',  ( 0.6971942568897637749, 2.189545951927499583E-17, 0.7947834645131652831 ) ) ;
#21581 = CARTESIAN_POINT ( 'NONE',  ( -0.8759842519685039353, -0.1787899950787401882, 0.6815944881352126172 ) ) ;
#21582 = VECTOR ( 'NONE', #32122, 39.37007874015748143 ) ;
#21583 = DIRECTION ( 'NONE',  ( 1.000000000000000000, 0.000000000000000000, -1.822029033848725275E-16 ) ) ;
#21584 = AXIS2_PLACEMENT_3D ( 'NONE', #8168, #27136, #12030 ) ;
#21585 = CARTESIAN_POINT ( 'NONE',  ( 0.1574803149606300023, 1.126631386849004990, -3.440787370833234604 ) ) ;
#21586 = EDGE_CURVE ( 'NONE', #15079, #40089, #34604, .T. ) ;
#21587 = CARTESIAN_POINT ( 'NONE',  ( 0.1574803149606300301, -0.1530511809948351398, -0.06523048226347956391 ) ) ;
#21588 = CARTESIAN_POINT ( 'NONE',  ( -0.7185039370078746268, 0.06523048226347956391, 1.828248031388536310 ) ) ;
#21589 = ORIENTED_EDGE ( 'NONE', *, *, #44567, .T. ) ;
#21590 = LINE ( 'NONE', #14176, #27198 ) ;
#21591 = CARTESIAN_POINT ( 'NONE',  ( -1.033464566929133799, 0.000000000000000000, 1.505905511811023612 ) ) ;
#21592 = CARTESIAN_POINT ( 'NONE',  ( -0.7185039370078739607, 1.928577636452523993E-17, 0.4625984251968504046 ) ) ;
#21593 = ADVANCED_FACE ( 'NONE', ( #36605 ), #5515, .T. ) ;
#21594 = CARTESIAN_POINT ( 'NONE',  ( 0.7495606340400177148, -0.1264236179284866091, 1.508366141678519678 ) ) ;
#21595 = CARTESIAN_POINT ( 'NONE',  ( 0.03196715850396897318, -0.09851384192498563452, -0.1894913400051448926 ) ) ;
#21596 = DIRECTION ( 'NONE',  ( 1.000000000000000000, -0.000000000000000000, -0.000000000000000000 ) ) ;
#21597 = AXIS2_PLACEMENT_3D ( 'NONE', #23451, #12911, #44978 ) ;
#21598 = ORIENTED_EDGE ( 'NONE', *, *, #33900, .F. ) ;
#21599 = AXIS2_PLACEMENT_3D ( 'NONE', #20381, #12275, #27143 ) ;
#21600 = CARTESIAN_POINT ( 'NONE',  ( 0.07405724077823318263, -1.760950739882781502, -0.1787899950787401604 ) ) ;
#21601 = ORIENTED_EDGE ( 'NONE', *, *, #41303, .F. ) ;
#21602 = VERTEX_POINT ( 'NONE', #39695 ) ;
#21603 = EDGE_CURVE ( 'NONE', #14480, #23115, #43057, .T. ) ;
#21604 = LINE ( 'NONE', #6737, #23098 ) ;
#21605 = CARTESIAN_POINT ( 'NONE',  ( 0.1264236179284866091, -0.4237204723871811352, 0.1264236179284866091 ) ) ;
#21606 = CARTESIAN_POINT ( 'NONE',  ( 0.07405724077823318263, -0.9183070865604088251, -0.1787899950787401604 ) ) ;
#21607 = EDGE_CURVE ( 'NONE', #21900, #5382, #24884, .T. ) ;
#21608 = CARTESIAN_POINT ( 'NONE',  ( 0.2007874015748031815, 0.000000000000000000, 0.2047244094488188948 ) ) ;
#21609 = CARTESIAN_POINT ( 'NONE',  ( 0.1643970176812789008, -0.1622977831747160482, 1.011058549611711511E-12 ) ) ;
#21610 = CARTESIAN_POINT ( 'NONE',  ( 1.054774247047244540, 0.07405724077823318263, 0.3395669290800945039 ) ) ;
#21611 = CARTESIAN_POINT ( 'NONE',  ( -0.1797182628040039087, -0.1215989276932817470, -0.07444174185955065859 ) ) ;
#21612 = CARTESIAN_POINT ( 'NONE',  ( 0.1787899950787401604, -0.1910688501190024868, -0.07405724077823318263 ) ) ;
#21613 = CARTESIAN_POINT ( 'NONE',  ( 0.07405724077823318263, -0.2637795275052916555, 0.1787899950787401604 ) ) ;
#21614 = CARTESIAN_POINT ( 'NONE',  ( 3.284318927891251994E-17, -0.07431102356828367395, 0.1787899950787401882 ) ) ;
#21615 = CARTESIAN_POINT ( 'NONE',  ( 0.7185039370078739607, 1.928577636452523993E-17, 0.4527559054042842868 ) ) ;
#21616 = CARTESIAN_POINT ( 'NONE',  ( 0.9500414927467378812, -0.1787899950787401604, 0.6840551180564720113 ) ) ;
#21617 = CIRCLE ( 'NONE', #5535, 0.1574803149606299191 ) ;
#21618 = CARTESIAN_POINT ( 'NONE',  ( -0.8019270111902716547, -0.1787899950787401604, 0.9596456692375763264 ) ) ;
#21620 = CARTESIAN_POINT ( 'NONE',  ( 0.7646288533564489232, 0.1113553986120547346, 0.9990157479239685223 ) ) ;
#21619 = ( CONVERSION_BASED_UNIT ( 'INCH', #28605 ) LENGTH_UNIT ( ) NAMED_UNIT ( #16385 ) ) ;
#21621 = CARTESIAN_POINT ( 'NONE',  ( -0.1270800023317771588, -1.659492628480683019, -0.1270800023317771588 ) ) ;
#21622 = CARTESIAN_POINT ( 'NONE',  ( 0.9412147342319837628, -0.1574803149606297803, 1.695374015748031926 ) ) ;
#21623 = CARTESIAN_POINT ( 'NONE',  ( 1.002407869896990045, -0.1264236179284866091, 1.715059055064346527 ) ) ;
#21624 = CARTESIAN_POINT ( 'NONE',  ( -0.1766724065096720031, -0.08549467455868767218, 0.1834299084088460152 ) ) ;
#21625 = EDGE_LOOP ( 'NONE', ( #25371, #36176, #32578, #43915 ) ) ;
#21626 = AXIS2_PLACEMENT_3D ( 'NONE', #16566, #26892, #19675 ) ;
#21627 = DIRECTION ( 'NONE',  ( 0.000000000000000000, 1.000000000000000000, 0.000000000000000000 ) ) ;
#21628 = CARTESIAN_POINT ( 'NONE',  ( 0.1637325577037128943, -0.1604625459914955088, -0.002338731188024976374 ) ) ;
#21630 = CARTESIAN_POINT ( 'NONE',  ( 0.07405724077823318263, -0.1751968503399373434, -0.1787899950787401604 ) ) ;
#21629 = CARTESIAN_POINT ( 'NONE',  ( -0.1574803149606297803, -0.9207677164279066684, 0.06523048226347956391 ) ) ;
#21631 = CARTESIAN_POINT ( 'NONE',  ( -0.7495606340400177148, 0.1264236179284866091, 0.3961614172690708924 ) ) ;
#21632 = CARTESIAN_POINT ( 'NONE',  ( 0.8019270111902717657, 0.1787899950787401604, 0.5856299212060785964 ) ) ;
#21633 = CARTESIAN_POINT ( 'NONE',  ( 0.1264236179284866091, -1.078248031442299304, -0.1264236179284866091 ) ) ;
#21634 = CARTESIAN_POINT ( 'NONE',  ( 0.9500414927467378812, 0.1787899950787401604, 0.03444881884387430981 ) ) ;
#21635 = CARTESIAN_POINT ( 'NONE',  ( -0.7185039370078739607, 1.928577636452523993E-17, 1.161417322727118284 ) ) ;
#21636 = CARTESIAN_POINT ( 'NONE',  ( -0.6971942568897648851, 0.07405724077823318263, 1.653543307032850462 ) ) ;
#21637 = ORIENTED_EDGE ( 'NONE', *, *, #42977, .T. ) ;
#21638 = CIRCLE ( 'NONE', #38500, 0.09842519685039370636 ) ;
#21639 = CARTESIAN_POINT ( 'NONE',  ( -1.054774247047244540, -0.07405724077823318263, 1.166338582623402509 ) ) ;
#21640 = CARTESIAN_POINT ( 'NONE',  ( -0.3010010101267349136, -0.07503014570242684533, -1.025942700826908638 ) ) ;
#21642 = ORIENTED_EDGE ( 'NONE', *, *, #32450, .F. ) ;
#21641 = CARTESIAN_POINT ( 'NONE',  ( -0.1113553986120547346, -1.115157480207433105, 0.1113553986120547346 ) ) ;
#21643 = CARTESIAN_POINT ( 'NONE',  ( 0.1574803149606300023, 0.06851622550196635741, -0.1414889043096673460 ) ) ;
#21644 = CARTESIAN_POINT ( 'NONE',  ( 0.6971942568897648851, -0.07405724077823297447, 1.894685039316315489 ) ) ;
#21645 = CARTESIAN_POINT ( 'NONE',  ( -0.9412147342319837628, 0.1574803149606300301, 0.6077755905511815770 ) ) ;
#21646 = CARTESIAN_POINT ( 'NONE',  ( -0.7495606340400177148, 0.1264236179284866091, 0.9030511810485984947 ) ) ;
#21647 = ADVANCED_FACE ( 'NONE', ( #28488 ), #19257, .F. ) ;
#21648 = CARTESIAN_POINT ( 'NONE',  ( -0.1987795079023651490, -0.1807288298655959913, -0.05471869868084799915 ) ) ;
#21649 = CARTESIAN_POINT ( 'NONE',  ( 1.054774247047244540, -0.07405724077823318263, 0.3001968503399373711 ) ) ;
#21650 = CARTESIAN_POINT ( 'NONE',  ( -1.054774247047244540, 0.07405724077823318263, 0.1820866141194649179 ) ) ;
#21651 = CARTESIAN_POINT ( 'NONE',  ( -0.9500414927467378812, -0.1787899950787401604, 0.6840551180564720113 ) ) ;
#21652 = CARTESIAN_POINT ( 'NONE',  ( 1.033464566929134687, 0.06523048226347956391, 1.498523621939716444 ) ) ;
#21653 = ORIENTED_EDGE ( 'NONE', *, *, #92, .T. ) ;
#21654 = ADVANCED_FACE ( 'NONE', ( #17910 ), #3042, .F. ) ;
#21655 = CARTESIAN_POINT ( 'NONE',  ( 0.1787899950787401604, 0.01673228351833045899, -0.07405724077823318263 ) ) ;
#21656 = CARTESIAN_POINT ( 'NONE',  ( 1.002407869896990045, 0.1264236179284866091, 0.8587598424659212970 ) ) ;
#21657 = ADVANCED_FACE ( 'NONE', ( #43534, #47149 ), #14333, .F. ) ;
#21658 = CARTESIAN_POINT ( 'NONE',  ( 0.8759842519685039353, -0.1787899950787401882, 1.080216535379306952 ) ) ;
#21659 = CARTESIAN_POINT ( 'NONE',  ( -0.8759842519685039353, -0.1787899950787401882, 1.862696850339937038 ) ) ;
#21660 = EDGE_CURVE ( 'NONE', #34218, #32653, #2425, .T. ) ;
#21661 = ORIENTED_EDGE ( 'NONE', *, *, #36047, .F. ) ;
#21662 = CIRCLE ( 'NONE', #23163, 0.2204724409448818867 ) ;
#21663 = CARTESIAN_POINT ( 'NONE',  ( 0.7185039370078746268, 0.06523048226347956391, 1.326279527559055982 ) ) ;
#21664 = CARTESIAN_POINT ( 'NONE',  ( -1.094772975963752103E-17, -1.246679086339474551, -0.1787899950787401882 ) ) ;
#21665 = ORIENTED_EDGE ( 'NONE', *, *, #6091, .T. ) ;
#21666 = CARTESIAN_POINT ( 'NONE',  ( 0.1264236179284866091, -0.3302165353793074520, -0.1264236179284866091 ) ) ;
#21667 = ORIENTED_EDGE ( 'NONE', *, *, #41444, .T. ) ;
#21668 = CARTESIAN_POINT ( 'NONE',  ( 0.6971942568897648851, 0.07405724077823318263, 1.141732283410804349 ) ) ;
#21669 = CARTESIAN_POINT ( 'NONE',  ( -1.033464566929133799, 1.928577636452524610E-17, 2.869337061179095023E-17 ) ) ;
#21670 = CIRCLE ( 'NONE', #229, 0.09842519685039370636 ) ;
#21671 = DIRECTION ( 'NONE',  ( 0.000000000000000000, 1.000000000000000000, 0.000000000000000000 ) ) ;
#21672 = DIRECTION ( 'NONE',  ( -0.000000000000000000, 1.000000000000000000, -0.000000000000000000 ) ) ;
#21673 = ( BOUNDED_CURVE ( )  B_SPLINE_CURVE ( 2, ( #7444, #44103, #36689, #47233, #3850, #14889, #17761, #14417, #24958 ),
 .UNSPECIFIED., .F., .T. ) 
 B_SPLINE_CURVE_WITH_KNOTS ( ( 3, 2, 2, 2, 3 ),
 ( 0.7900000000000000355, 0.7924999999999999822, 0.7950000000000000400, 0.7974999999999999867, 0.8000000000000000444 ),
 .UNSPECIFIED. ) 
 CURVE ( )  GEOMETRIC_REPRESENTATION_ITEM ( )  RATIONAL_B_SPLINE_CURVE ( ( 1.000000000000000000, 0.9238795325112869605, 1.000000000000000000, 0.9238795325112869605, 1.000000000000000000, 0.9238795325112869605, 1.000000000000000000, 0.9238795325112869605, 1.000000000000000000 ) ) 
 REPRESENTATION_ITEM ( '' )  ) ;
#21674 = CARTESIAN_POINT ( 'NONE',  ( 1.054774247047244540, -0.07405724077823318263, 0.09842519679663024046 ) ) ;
#21675 = CARTESIAN_POINT ( 'NONE',  ( 0.1264236179284866091, -0.7780511810485984947, 0.1264236179284866091 ) ) ;
#21676 = CARTESIAN_POINT ( 'NONE',  ( -0.9500414927467377701, 0.1787899950787401604, 0.5068897637257642197 ) ) ;
#21677 = CARTESIAN_POINT ( 'NONE',  ( -0.7185039370078746268, 0.06523048226347956391, 0.6865157479239700766 ) ) ;
#21679 = CARTESIAN_POINT ( 'NONE',  ( -0.7236033548003161231, -0.07168286384238391207, 1.984649071003595999 ) ) ;
#21678 = CARTESIAN_POINT ( 'NONE',  ( 0.1797182628040039365, -1.280555620606667278, -2.200913952912460540E-17 ) ) ;
#21680 = DIRECTION ( 'NONE',  ( -9.420165495393842173E-15, -0.7880107536067199048, 0.6156614753256609562 ) ) ;
#21681 = CARTESIAN_POINT ( 'NONE',  ( 1.002407869896990045, -0.1264236179284866091, 1.281988188922614125 ) ) ;
#21682 = CARTESIAN_POINT ( 'NONE',  ( 1.002407869896990045, -0.1264236179284866091, 1.670767716481669440 ) ) ;
#21683 = CARTESIAN_POINT ( 'NONE',  ( -0.05116749466471032931, 0.1299212598425196763, 0.1641566192618154341 ) ) ;
#21685 = CARTESIAN_POINT ( 'NONE',  ( -0.7640189571129942792, 0.1165819918074077199, 1.980746850915923174 ) ) ;
#21684 = FACE_OUTER_BOUND ( 'NONE', #9437, .T. ) ;
#21686 = CARTESIAN_POINT ( 'NONE',  ( 0.1602931993194442739, -0.07955613945526357478, -0.1377952755905511861 ) ) ;
#21687 = CARTESIAN_POINT ( 'NONE',  ( 2.892866454678787531E-17, -0.7952755904436534795, 0.1574803149606299191 ) ) ;
#21688 = CARTESIAN_POINT ( 'NONE',  ( -0.8107537697050253289, -0.1574803149606297803, 1.680610236112946687 ) ) ;
#21689 = CARTESIAN_POINT ( 'NONE',  ( 0.9500414927467378812, 0.1787899950787401604, 0.1870078739619845387 ) ) ;
#21691 = DIRECTION ( 'NONE',  ( 1.822029033848725028E-16, 0.000000000000000000, 1.000000000000000000 ) ) ;
#21690 = CARTESIAN_POINT ( 'NONE',  ( 0.7495606340400177148, -0.1264236179284866091, 1.188484251914740275 ) ) ;
#21692 = DIRECTION ( 'NONE',  ( -1.000000000000000000, 0.000000000000000000, 0.000000000000000000 ) ) ;
#21693 = CARTESIAN_POINT ( 'NONE',  ( -0.7495606340400177148, 0.1264236179284866091, 1.218011810969858111 ) ) ;
#21694 = CARTESIAN_POINT ( 'NONE',  ( 0.8759842519685039353, -0.1574803149606299191, 0.5019685038294811052 ) ) ;
#21695 = EDGE_LOOP ( 'NONE', ( #27945, #46410, #15331, #30442 ) ) ;
#21696 = CARTESIAN_POINT ( 'NONE',  ( -0.7185039370078739607, 1.928577636452523993E-17, 1.397637795168062969 ) ) ;
#21697 = AXIS2_PLACEMENT_3D ( 'NONE', #19911, #42171, #19438 ) ;
#21698 = CARTESIAN_POINT ( 'NONE',  ( -0.8107537697050253289, -0.1574803149606297803, 0.3813976376877488139 ) ) ;
#21699 = ORIENTED_EDGE ( 'NONE', *, *, #35276, .T. ) ;
#21700 = CARTESIAN_POINT ( 'NONE',  ( 0.8759842519685039353, 0.1787899950787401882, 1.409940944828126153 ) ) ;
#21702 = CYLINDRICAL_SURFACE ( 'NONE', #46057, 0.1787899950787401049 ) ;
#21701 = CARTESIAN_POINT ( 'NONE',  ( -1.033464566929133799, 0.000000000000000000, 0.08858267716535432601 ) ) ;
#21703 = CARTESIAN_POINT ( 'NONE',  ( -0.1787899950787401604, 0.03641732288840918152, -0.07405724077823318263 ) ) ;
#21704 = ORIENTED_EDGE ( 'NONE', *, *, #5256, .T. ) ;
#21705 = DIRECTION ( 'NONE',  ( 0.000000000000000000, 1.000000000000000000, 0.000000000000000000 ) ) ;
#21706 = EDGE_CURVE ( 'NONE', #13443, #752, #39940, .T. ) ;
#21707 = ORIENTED_EDGE ( 'NONE', *, *, #35926, .T. ) ;
#21708 = FACE_OUTER_BOUND ( 'NONE', #43993, .T. ) ;
#21709 = DIRECTION ( 'NONE',  ( -0.000000000000000000, -0.000000000000000000, 1.000000000000000000 ) ) ;
#21710 = AXIS2_PLACEMENT_3D ( 'NONE', #31704, #35299, #46289 ) ;
#21711 = CARTESIAN_POINT ( 'NONE',  ( 1.002407869896990045, -0.1264236179284866091, 0.5733267715997795166 ) ) ;
#21713 = ADVANCED_FACE ( 'NONE', ( #21752 ), #36384, .T. ) ;
#21712 = ORIENTED_EDGE ( 'NONE', *, *, #4543, .T. ) ;
#21714 = CARTESIAN_POINT ( 'NONE',  ( -0.1113553986120547346, 0.1053149607374482266, 0.1113553986120547346 ) ) ;
#21715 = CARTESIAN_POINT ( 'NONE',  ( -1.002407869896990045, 0.1264236179284866091, 1.173720472387181246 ) ) ;
#21716 = CARTESIAN_POINT ( 'NONE',  ( -0.9873396505805591694, 0.1113553986120547346, 0.09350393700787401619 ) ) ;
#21717 = ORIENTED_EDGE ( 'NONE', *, *, #21029, .T. ) ;
#21718 = CARTESIAN_POINT ( 'NONE',  ( -0.7495606340400177148, 0.1264236179284866091, 1.021161417269070837 ) ) ;
#21719 = ADVANCED_FACE ( 'NONE', ( #44469 ), #34207, .F. ) ;
#21720 = CARTESIAN_POINT ( 'NONE',  ( -1.054774247047244540, 0.07405724077823318263, 0.8169291338045038264 ) ) ;
#21721 = CARTESIAN_POINT ( 'NONE',  ( -0.6971942568897626646, 0.07405724077823318263, 0.2411417322297011168 ) ) ;
#21722 = CARTESIAN_POINT ( 'NONE',  ( -1.033464566929134687, -0.06523048226347956391, 0.3617125984251969295 ) ) ;
#21723 = CARTESIAN_POINT ( 'NONE',  ( 0.5314960629921259283, 0.000000000000000000, 4.685039370078739829 ) ) ;
#21724 = CARTESIAN_POINT ( 'NONE',  ( -0.1264236179284866091, -0.8874271178355372935, -0.1264236179284866091 ) ) ;
#21725 = VERTEX_POINT ( 'NONE', #44940 ) ;
#21726 = CARTESIAN_POINT ( 'NONE',  ( 0.1787899950787401882, 0.1373031496600628232, -2.189545951927503898E-17 ) ) ;
#21727 = EDGE_LOOP ( 'NONE', ( #17082, #17293, #15613, #18265 ) ) ;
#21728 = ORIENTED_EDGE ( 'NONE', *, *, #7535, .T. ) ;
#21729 = CARTESIAN_POINT ( 'NONE',  ( -0.7185039370078739607, 0.000000000000000000, -2.869337061179095023E-17 ) ) ;
#21730 = CARTESIAN_POINT ( 'NONE',  ( -0.6971942568897626646, 0.07405724077823318263, 0.7480314960092282472 ) ) ;
#21731 = CARTESIAN_POINT ( 'NONE',  ( 0.7185039370078739607, 1.928577636452523993E-17, 0.8562992125984251190 ) ) ;
#21732 = ORIENTED_EDGE ( 'NONE', *, *, #35921, .F. ) ;
#21733 = EDGE_CURVE ( 'NONE', #40966, #5319, #22071, .T. ) ;
#21734 = CARTESIAN_POINT ( 'NONE',  ( 0.7185039370078746268, -0.06523048226347956391, 1.331200787401575436 ) ) ;
#21735 = CARTESIAN_POINT ( 'NONE',  ( -0.6971942568897626646, 0.07405724077823318263, 0.08366141726907130871 ) ) ;
#21736 = CARTESIAN_POINT ( 'NONE',  ( 0.7185039370078739607, 1.928577636452523993E-17, 0.6988188976377952555 ) ) ;
#21737 = CARTESIAN_POINT ( 'NONE',  ( 0.07444174185955046430, -0.8007327859609992826, -0.1797182628040039087 ) ) ;
#21738 = CARTESIAN_POINT ( 'NONE',  ( 0.09005431033085642412, -0.2435012976189759315, -0.3128573757127792176 ) ) ;
#21739 = CARTESIAN_POINT ( 'NONE',  ( -0.7646288533564489232, -0.1113553986120547346, 1.363188976270427455 ) ) ;
#21740 = AXIS2_PLACEMENT_3D ( 'NONE', #29330, #11539, #11078 ) ;
#21741 = CARTESIAN_POINT ( 'NONE',  ( 1.054774247047244540, -0.07405724077823318263, 0.7726377952218265177 ) ) ;
#21742 = CARTESIAN_POINT ( 'NONE',  ( -0.1574803149606300301, -0.5812007874015742148, -0.06523048226347956391 ) ) ;
#21743 = CARTESIAN_POINT ( 'NONE',  ( -0.1026092249587055166, 0.1299212598425196763, 0.1321676130798911386 ) ) ;
#21744 = ORIENTED_EDGE ( 'NONE', *, *, #22778, .T. ) ;
#21745 = DIRECTION ( 'NONE',  ( 0.000000000000000000, 0.000000000000000000, 1.000000000000000000 ) ) ;
#21746 = CARTESIAN_POINT ( 'NONE',  ( 0.9412147342319837628, 0.1574803149606300301, 1.198326771653543510 ) ) ;
#21748 = CARTESIAN_POINT ( 'NONE',  ( -0.02739131347899105909, -0.09752745740044843625, 0.1550798682808147422 ) ) ;
#21747 = CARTESIAN_POINT ( 'NONE',  ( 0.8638812610618022969, -0.1737634973235707980, 1.987989868856034681 ) ) ;
#21749 = CARTESIAN_POINT ( 'NONE',  ( 0.7185039370078739607, 1.928577636452523993E-17, 0.3346456691838114450 ) ) ;
#21750 = CARTESIAN_POINT ( 'NONE',  ( -0.1113553986120547346, -0.6427165353255432922, 0.1113553986120547346 ) ) ;
#21752 = FACE_OUTER_BOUND ( 'NONE', #46751, .T. ) ;
#21751 = CARTESIAN_POINT ( 'NONE',  ( 0.6971942568897648851, -0.07405724077823297447, 0.5954724408911187261 ) ) ;
#21753 = CARTESIAN_POINT ( 'NONE',  ( 0.07405724077823318263, -0.6574803149068665364, 0.1787899950787401604 ) ) ;
#21754 = CARTESIAN_POINT ( 'NONE',  ( -0.5555748031496058337, 0.2597269656108975311, 0.5511811023622046335 ) ) ;
#21755 = EDGE_LOOP ( 'NONE', ( #42662, #28128, #44270, #7087 ) ) ;
#21756 = DIRECTION ( 'NONE',  ( -1.000000000000000000, 0.000000000000000000, 0.000000000000000000 ) ) ;
#21757 = CARTESIAN_POINT ( 'NONE',  ( 1.002407869896990045, -0.1264236179284866091, 1.040846456639149764 ) ) ;
#21758 = DIRECTION ( 'NONE',  ( 1.000000000000000000, 0.000000000000000000, 0.000000000000000000 ) ) ;
#21759 = CARTESIAN_POINT ( 'NONE',  ( 0.07405724077823318263, -1.198818897584032150, -0.1787899950787401604 ) ) ;
#21760 = CARTESIAN_POINT ( 'NONE',  ( 1.181102362204724310, 0.000000000000000000, 0.9842519685039370358 ) ) ;
#21761 = ADVANCED_FACE ( 'NONE', ( #26540 ), #42974, .T. ) ;
#21762 = ORIENTED_EDGE ( 'NONE', *, *, #20354, .T. ) ;
#21763 = CARTESIAN_POINT ( 'NONE',  ( -1.054774247047244540, -0.07405724077823318263, 0.1377952755367876370 ) ) ;
#21764 = ORIENTED_EDGE ( 'NONE', *, *, #5153, .T. ) ;
#21765 = CARTESIAN_POINT ( 'NONE',  ( -0.1574803149606297803, 0.06348425207603099196, 0.06523048226347956391 ) ) ;
#21767 = CARTESIAN_POINT ( 'NONE',  ( 0.07405724077823318263, -1.410433070812377565, 0.1787899950787401604 ) ) ;
#21766 = CARTESIAN_POINT ( 'NONE',  ( -0.06523048226347956391, -0.3252952754830241155, 0.1574803149606297803 ) ) ;
#21769 = CARTESIAN_POINT ( 'NONE',  ( -0.8759842519685039353, 0.1787899950787401882, 1.887303149552535420 ) ) ;
#21768 = AXIS2_PLACEMENT_3D ( 'NONE', #28965, #40622, #11431 ) ;
#21770 = CARTESIAN_POINT ( 'NONE',  ( -0.6971942568897637749, 2.189545951927499583E-17, 1.734744094434425232 ) ) ;
#21771 = EDGE_CURVE ( 'NONE', #21060, #14891, #22443, .T. ) ;
#21772 = CARTESIAN_POINT ( 'NONE',  ( -0.6971942568897637749, 2.189545951927499583E-17, 0.4010826771115905687 ) ) ;
#21773 = CARTESIAN_POINT ( 'NONE',  ( 0.8759842519685039353, 0.000000000000000000, 4.498031496062992574 ) ) ;
#21774 = CARTESIAN_POINT ( 'NONE',  ( -1.002407869896990045, -0.1264236179284866091, 1.990649606245448844 ) ) ;
#21775 = CARTESIAN_POINT ( 'NONE',  ( 0.1235961452251413406, -0.09842519685039370636, -0.2140748031496062798 ) ) ;
#21776 = CARTESIAN_POINT ( 'NONE',  ( -0.8107537697050253289, 0.1574803149606300301, 1.872539370078740495 ) ) ;
#21777 = CIRCLE ( 'NONE', #42387, 0.7874015748031495399 ) ;
#21778 = CARTESIAN_POINT ( 'NONE',  ( -0.2617458567146319082, 0.1661939583519097263, -0.8535845443516340003 ) ) ;
#21779 = CARTESIAN_POINT ( 'NONE',  ( 0.1264236179284866091, -0.4248286926386873885, -0.1264236179284866091 ) ) ;
#21780 = DIRECTION ( 'NONE',  ( 0.000000000000000000, 0.000000000000000000, 1.000000000000000000 ) ) ;
#21781 = DIRECTION ( 'NONE',  ( -0.000000000000000000, -0.7880107536067214591, 0.6156614753256588468 ) ) ;
#21782 = CARTESIAN_POINT ( 'NONE',  ( -0.8759842519685039353, -0.1787899950787401882, 0.2485236219934806867 ) ) ;
#21783 = ( BOUNDED_CURVE ( )  B_SPLINE_CURVE ( 2, ( #37895, #44345, #33612, #23281, #8643, #26175, #33379, #22796, #15388 ),
 .UNSPECIFIED., .F., .T. ) 
 B_SPLINE_CURVE_WITH_KNOTS ( ( 3, 2, 2, 2, 3 ),
 ( 0.2200000000000000011, 0.2225000000000000033, 0.2250000000000000056, 0.2275000000000000078, 0.2300000000000000100 ),
 .UNSPECIFIED. ) 
 CURVE ( )  GEOMETRIC_REPRESENTATION_ITEM ( )  RATIONAL_B_SPLINE_CURVE ( ( 1.000000000000000000, 0.9238795325112869605, 1.000000000000000000, 0.9238795325112869605, 1.000000000000000000, 0.9238795325112869605, 1.000000000000000000, 0.9238795325112869605, 1.000000000000000000 ) ) 
 REPRESENTATION_ITEM ( '' )  ) ;
#21784 = ORIENTED_EDGE ( 'NONE', *, *, #18399, .T. ) ;
#21785 = VERTEX_POINT ( 'NONE', #11684 ) ;
#21786 = B_SPLINE_CURVE_WITH_KNOTS ( 'NONE', 3,
 ( #9395, #2413, #13460, #5791, #9631, #13677, #13923, #20396, #17511, #42651, #39548, #46026, #13238, #27866, #20632, #28568, #38844, #6721, #6012, #35968, #17753, #45787, #35277 ),
 .UNSPECIFIED., .F., .F.,
 ( 4, 2, 2, 1, 1, 1, 2, 2, 2, 1, 1, 2, 2, 4 ),
 ( 0.000000000000000000, 0.2500000000000004996, 0.3750000000000006661, 0.4375000000000008327, 0.4687500000000011657, 0.4843750000000014433, 0.4921875000000015543, 0.5000000000000015543, 0.6249999999999980016, 0.6874999999999958922, 0.7187499999999952260, 0.7343749999999952260, 0.7499999999999952260, 1.000000000000000000 ),
 .UNSPECIFIED. ) ;
#21787 = CARTESIAN_POINT ( 'NONE',  ( -0.8019270111902716547, -0.1787899950787401604, 1.432086614119464141 ) ) ;
#21788 = ORIENTED_EDGE ( 'NONE', *, *, #43210, .T. ) ;
#21789 = AXIS2_PLACEMENT_3D ( 'NONE', #14387, #29036, #43836 ) ;
#21790 = CARTESIAN_POINT ( 'NONE',  ( -0.1264236179284866091, -1.181594488135212506, 0.1264236179284866091 ) ) ;
#21791 = ADVANCED_FACE ( 'NONE', ( #19561 ), #15661, .F. ) ;
#21792 = CARTESIAN_POINT ( 'NONE',  ( -0.1264236179284866091, -1.422736220418677311, -0.1264236179284866091 ) ) ;
#21793 = ( CONVERSION_BASED_UNIT ( 'INCH', #7168 ) LENGTH_UNIT ( ) NAMED_UNIT ( #33833 ) ) ;
#21794 = DIRECTION ( 'NONE',  ( -0.9999965023344150605, -0.002644866525195953624, 6.595852336532814775E-15 ) ) ;
#21795 = CARTESIAN_POINT ( 'NONE',  ( 1.033464566929133799, 0.000000000000000000, 0.3248031496062992463 ) ) ;
#21796 = CARTESIAN_POINT ( 'NONE',  ( -0.6195511811023656223, 0.9842519685039370358, -0.7135826771653542844 ) ) ;
#21797 = CARTESIAN_POINT ( 'NONE',  ( -0.9412147342319837628, 0.1574803149606300301, 0.9522637794200313754 ) ) ;
#21798 = CARTESIAN_POINT ( 'NONE',  ( 1.002407869896990045, 0.1264236179284866091, 0.3863188975840318173 ) ) ;
#21799 = CARTESIAN_POINT ( 'NONE',  ( 0.06523048226347956391, -0.09399606299212612259, 0.1574803149606297803 ) ) ;
#21800 = AXIS2_PLACEMENT_3D ( 'NONE', #13094, #2507, #35129 ) ;
#21801 = CARTESIAN_POINT ( 'NONE',  ( 0.9873396505805591694, 0.1113553986120547346, 1.776574803042078488 ) ) ;
#21802 = ORIENTED_EDGE ( 'NONE', *, *, #11974, .T. ) ;
#21803 = DIRECTION ( 'NONE',  ( 0.000000000000000000, -0.7880107536067207930, 0.6156614753256598460 ) ) ;
#21804 = CARTESIAN_POINT ( 'NONE',  ( 0.8107537697050253289, 0.1574803149606300301, 0.8095472440944886383 ) ) ;
#21805 = CARTESIAN_POINT ( 'NONE',  ( -0.1534195868007021402, 0.9251089822459552803, -1.060267534067254935 ) ) ;
#21806 = ( BOUNDED_CURVE ( )  B_SPLINE_CURVE ( 2, ( #10798, #29026, #11027, #17484, #39517, #29281, #36428, #46705, #39281 ),
 .UNSPECIFIED., .F., .F. ) 
 B_SPLINE_CURVE_WITH_KNOTS ( ( 3, 2, 2, 2, 3 ),
 ( 0.08999999999999999667, 0.09249999999999999889, 0.09500000000000000111, 0.09750000000000000333, 0.1000000000000000056 ),
 .UNSPECIFIED. ) 
 CURVE ( )  GEOMETRIC_REPRESENTATION_ITEM ( )  RATIONAL_B_SPLINE_CURVE ( ( 1.000000000000000000, 0.9238795325112869605, 1.000000000000000000, 0.9238795325112869605, 1.000000000000000000, 0.9238795325112869605, 1.000000000000000000, 0.9238795325112869605, 1.000000000000000000 ) ) 
 REPRESENTATION_ITEM ( '' )  ) ;
#21807 = DIRECTION ( 'NONE',  ( 0.000000000000000000, -0.6156614753256599570, -0.7880107536067207930 ) ) ;
#21808 = CARTESIAN_POINT ( 'NONE',  ( 0.8759842519685039353, -0.1574803149606299191, 0.1476377951680635792 ) ) ;
#21809 = VERTEX_POINT ( 'NONE', #16914 ) ;
#21810 = ADVANCED_FACE ( 'NONE', ( #35835 ), #9963, .T. ) ;
#21811 = CARTESIAN_POINT ( 'NONE',  ( 0.7185039370078739607, 1.928577636452523993E-17, 1.909448818790110192 ) ) ;
#21812 = CARTESIAN_POINT ( 'NONE',  ( 0.07405724077823318263, -1.626968503883244876, -0.1787899950787401604 ) ) ;
#21813 = CARTESIAN_POINT ( 'NONE',  ( 0.06523048226347956391, -1.565452755797984263, -0.1574803149606300301 ) ) ;
#21814 = CARTESIAN_POINT ( 'NONE',  ( 0.1787899950787401604, -0.6919291338045056028, -0.07405724077823318263 ) ) ;
#21815 = CARTESIAN_POINT ( 'NONE',  ( -0.9873396505805591694, 0.1113553986120547346, 0.1624015746956226358 ) ) ;
#21816 = CARTESIAN_POINT ( 'NONE',  ( 0.06523048226347956391, -1.038877952755906442, 0.1574803149606297803 ) ) ;
#21817 = CARTESIAN_POINT ( 'NONE',  ( 1.033464566929134687, -0.06523048226347956391, 0.9817913384751510986 ) ) ;
#21818 = EDGE_CURVE ( 'NONE', #33977, #26206, #31787, .T. ) ;
#21819 = VERTEX_POINT ( 'NONE', #47079 ) ;
#21820 = ORIENTED_EDGE ( 'NONE', *, *, #45284, .F. ) ;
#21821 = CARTESIAN_POINT ( 'NONE',  ( -0.6971942568897637749, 2.189545951927499583E-17, 1.542814960576157413 ) ) ;
#21822 = CARTESIAN_POINT ( 'NONE',  ( 1.054774247047244096, 0.000000000000000000, 1.523129921206078707 ) ) ;
#21823 = CARTESIAN_POINT ( 'NONE',  ( 0.1113553986120547346, -1.292322834538141674, -0.1113553986120547346 ) ) ;
#21824 = CARTESIAN_POINT ( 'NONE',  ( -0.7495606340400177148, 0.1264236179284866091, 0.7898622046706456068 ) ) ;
#21825 = CARTESIAN_POINT ( 'NONE',  ( 1.002407869896990045, -0.1264236179284866091, 0.1402559054580474474 ) ) ;
#21826 = DIRECTION ( 'NONE',  ( -1.000000000000000000, -6.679788269418529283E-17, 0.000000000000000000 ) ) ;
#21827 = CARTESIAN_POINT ( 'NONE',  ( 0.6971942568897648851, 0.07405724077823318263, 0.7135826771115916234 ) ) ;
#21828 = CARTESIAN_POINT ( 'NONE',  ( -0.6971942568897648851, -0.07405724077823297447, 0.7529527558517473684 ) ) ;
#21829 = ADVANCED_FACE ( 'NONE', ( #46603 ), #13781, .T. ) ;
#21830 = CARTESIAN_POINT ( 'NONE',  ( 0.008396861977785833459, -0.08632935120555602915, 0.1260637287086050495 ) ) ;
#21831 = DIRECTION ( 'NONE',  ( 0.000000000000000000, -0.2126700594527834443, 0.9771240687918547607 ) ) ;
#21832 = CARTESIAN_POINT ( 'NONE',  ( -0.1574803149606297803, -0.1333661416247563514, 0.06523048226347956391 ) ) ;
#21833 = CARTESIAN_POINT ( 'NONE',  ( -0.8759842519685039353, -0.1574803149606299191, 1.919291338475149544 ) ) ;
#21834 = ORIENTED_EDGE ( 'NONE', *, *, #12201, .F. ) ;
#21835 = VECTOR ( 'NONE', #10050, 39.37007874015748143 ) ;
#21836 = CARTESIAN_POINT ( 'NONE',  ( -0.7185039370078746268, 0.06523048226347956391, 1.523129921259841923 ) ) ;
#21837 = DIRECTION ( 'NONE',  ( 0.000000000000000000, -1.000000000000000000, 0.000000000000000000 ) ) ;
#21838 = CARTESIAN_POINT ( 'NONE',  ( 0.7495606340400177148, 0.1264236179284866091, 1.419783464513165505 ) ) ;
#21839 = CARTESIAN_POINT ( 'NONE',  ( -0.1537669602759263732, -0.09851383235754725132, 0.06906785912561810847 ) ) ;
#21840 = DIRECTION ( 'NONE',  ( 0.000000000000000000, -0.6156614753256598460, -0.7880107536067207930 ) ) ;
#21841 = VERTEX_POINT ( 'NONE', #28428 ) ;
#21842 = CARTESIAN_POINT ( 'NONE',  ( 0.07405724077823318263, -1.721580661142623869, -0.1787899950787401604 ) ) ;
#21843 = ORIENTED_EDGE ( 'NONE', *, *, #3852, .F. ) ;
#21844 = ORIENTED_EDGE ( 'NONE', *, *, #2746, .F. ) ;
#21845 = DIRECTION ( 'NONE',  ( 0.000000000000000000, 1.000000000000000000, 0.000000000000000000 ) ) ;
#21846 = EDGE_CURVE ( 'NONE', #40728, #23847, #35255, .T. ) ;
#21847 = CARTESIAN_POINT ( 'NONE',  ( -0.1787899950787401604, -0.3966535432533230265, 0.07405724077823318263 ) ) ;
#21848 = CARTESIAN_POINT ( 'NONE',  ( -0.1787899950787401604, -0.9872047243556864027, -0.07405724077823318263 ) ) ;
#21849 = CARTESIAN_POINT ( 'NONE',  ( -0.2471922927914643187, -0.07821957050364394815, -0.07683452368279758415 ) ) ;
#21850 = CARTESIAN_POINT ( 'NONE',  ( 0.9500414927467378812, 0.1787899950787401604, 0.3051181101824569919 ) ) ;
#21851 = CARTESIAN_POINT ( 'NONE',  ( 0.07444174185955046430, -0.2101816048586362673, -0.1797182628040039087 ) ) ;
#21852 = PRODUCT_DEFINITION_SHAPE ( 'NONE', 'NONE',  #754 ) ;
#21853 = CARTESIAN_POINT ( 'NONE',  ( 0.07405724077823318263, -0.1615412910638844290, 0.1787899950787401604 ) ) ;
#21854 = CARTESIAN_POINT ( 'NONE',  ( 0.07405724077823318263, -0.09645669285962235606, -0.1787899950787401604 ) ) ;
#21855 = CYLINDRICAL_SURFACE ( 'NONE', #28055, 0.1574803149606299191 ) ;
#21856 = CARTESIAN_POINT ( 'NONE',  ( 0.8019270111902717657, -0.1787899950787401604, 0.5610236219934807700 ) ) ;
#21858 = CARTESIAN_POINT ( 'NONE',  ( 0.9412147342319837628, 0.1574803149606300301, 1.119586614173229577 ) ) ;
#21857 = CARTESIAN_POINT ( 'NONE',  ( -0.8340766383913040816, 0.1725986337945408233, 0.03937007874015843040 ) ) ;
#21859 = FACE_OUTER_BOUND ( 'NONE', #12249, .T. ) ;
#21860 = VECTOR ( 'NONE', #19113, 39.37007874015748143 ) ;
#21861 = CARTESIAN_POINT ( 'NONE',  ( 0.1787899950787401882, -0.4532480314422991929, -2.189545951927503898E-17 ) ) ;
#21862 = CARTESIAN_POINT ( 'NONE',  ( -0.9873396505805591694, 0.1113553986120547346, 1.304133858160188897 ) ) ;
#21863 = CARTESIAN_POINT ( 'NONE',  ( 0.6971942568897648851, -0.07405724077823297447, 1.663385826717890925 ) ) ;
#21864 = CARTESIAN_POINT ( 'NONE',  ( -0.1235961452251413406, -0.09842519685039370636, 0.2140748031496062798 ) ) ;
#21865 = CARTESIAN_POINT ( 'NONE',  ( 1.054774247047244096, 0.000000000000000000, 0.4945866141194645849 ) ) ;
#21866 = EDGE_CURVE ( 'NONE', #43609, #18913, #28494, .T. ) ;
#21867 = CIRCLE ( 'NONE', #37153, 0.01968503937007875723 ) ;
#21868 = VECTOR ( 'NONE', #16016, 39.37007874015748143 ) ;
#21869 = B_SPLINE_CURVE_WITH_KNOTS ( 'NONE', 3,
 ( #21257, #3755, #13596, #28234, #32313, #39686, #21493, #42797, #32787, #24626, #47382, #47142, #32064, #39463, #29224, #36125, #43771, #39933, #14326, #25591, #46652 ),
 .UNSPECIFIED., .F., .F.,
 ( 4, 1, 1, 1, 1, 2, 2, 1, 1, 1, 1, 1, 2, 2, 4 ),
 ( 0.000000000000000000, 0.1249999999999975298, 0.1874999999999962808, 0.2187499999999956701, 0.2343749999999953926, 0.2421874999999951983, 0.2499999999999949762, 0.3749999999999932832, 0.4374999999999924505, 0.4687499999999920064, 0.4843749999999918954, 0.4921874999999918399, 0.4960937499999916733, 0.4999999999999915623, 1.000000000000000000 ),
 .UNSPECIFIED. ) ;
#21870 = ORIENTED_EDGE ( 'NONE', *, *, #44289, .F. ) ;
#21871 = DIRECTION ( 'NONE',  ( 0.000000000000000000, 0.000000000000000000, -1.000000000000000000 ) ) ;
#21872 = CARTESIAN_POINT ( 'NONE',  ( 0.07405724077823318263, -0.2539370078202523584, -0.1787899950787401604 ) ) ;
#21874 = CARTESIAN_POINT ( 'NONE',  ( 0.7646288533564489232, 0.1113553986120547346, 0.4872047243019220208 ) ) ;
#21873 = CARTESIAN_POINT ( 'NONE',  ( -1.054774247047244540, 0.07405724077823318263, 0.4625984251430869665 ) ) ;
#21875 = CARTESIAN_POINT ( 'NONE',  ( -0.1787899950787401604, -1.105314960576158301, -0.07405724077823318263 ) ) ;
#21876 = CARTESIAN_POINT ( 'NONE',  ( 0.8759842519685039353, 0.1787899950787401882, 0.03690944876513417572 ) ) ;
#21877 = CARTESIAN_POINT ( 'NONE',  ( 0.2698848154395015464, 1.205361022782824954E-17, -0.09842519685039370636 ) ) ;
#21878 = EDGE_CURVE ( 'NONE', #37983, #41227, #39838, .T. ) ;
#21879 = CARTESIAN_POINT ( 'NONE',  ( -1.002407869896990045, -0.1264236179284866091, 1.552657480261196765 ) ) ;
#21880 = ORIENTED_EDGE ( 'NONE', *, *, #42977, .F. ) ;
#21881 = CARTESIAN_POINT ( 'NONE',  ( -0.6971942568897637749, 2.189545951927499583E-17, 1.109744094434425232 ) ) ;
#21882 = CARTESIAN_POINT ( 'NONE',  ( -0.9873396505805591694, 0.1113553986120547346, 0.3297244094488189226 ) ) ;
#21883 = CARTESIAN_POINT ( 'NONE',  ( 0.8759842519685039353, 0.1787899950787401882, 1.139271653489543290 ) ) ;
#21884 = CARTESIAN_POINT ( 'NONE',  ( 0.6971942568897648851, 0.07405724077823318263, 1.771653543253322249 ) ) ;
#21885 = CARTESIAN_POINT ( 'NONE',  ( -0.8759842519685039353, -0.1787899950787401882, 1.114665354276944909 ) ) ;
#21886 = DIRECTION ( 'NONE',  ( -0.000000000000000000, -0.000000000000000000, -1.000000000000000000 ) ) ;
#21887 = CARTESIAN_POINT ( 'NONE',  ( -0.1432458882847533199, -0.2127911801008985637, -0.02834147079957508031 ) ) ;
#21888 = CARTESIAN_POINT ( 'NONE',  ( 0.8019270111902716547, -0.1787899950787401604, 0.2509842519147403861 ) ) ;
#21889 = CARTESIAN_POINT ( 'NONE',  ( -0.8759842519685039353, -0.1787899950787401882, 0.2878937007336381804 ) ) ;
#21890 = CARTESIAN_POINT ( 'NONE',  ( -1.054774247047244096, 0.000000000000000000, 0.6914370078202519698 ) ) ;
#21891 = CARTESIAN_POINT ( 'NONE',  ( 0.8107537697050253289, -0.1574803149606297803, 1.641240157372788611 ) ) ;
#21892 = ORIENTED_EDGE ( 'NONE', *, *, #47187, .F. ) ;
#21893 = CARTESIAN_POINT ( 'NONE',  ( -0.1264236179284866091, 0.06840551186478720236, -0.1264236179284866091 ) ) ;
#21894 = CARTESIAN_POINT ( 'NONE',  ( 1.002407869896990045, -0.1264236179284866091, 0.7701771653005669016 ) ) ;
#21895 = CARTESIAN_POINT ( 'NONE',  ( 0.8759842519685039353, -0.1787899950787401882, 1.001476377898992132 ) ) ;
#21896 = CARTESIAN_POINT ( 'NONE',  ( -0.8759842519685039353, -0.1787899950787401882, 1.902066929080094448 ) ) ;
#21897 = CARTESIAN_POINT ( 'NONE',  ( 0.8019270111902717657, -0.1787899950787401604, 1.978346456639149320 ) ) ;
#21898 = CARTESIAN_POINT ( 'NONE',  ( 0.9412147342319837628, 0.1574803149606300301, 1.316437007874015519 ) ) ;
#21899 = CARTESIAN_POINT ( 'NONE',  ( 0.1787899950787401604, -1.337722393426090228, 0.07405724077823318263 ) ) ;
#21900 = VERTEX_POINT ( 'NONE', #28673 ) ;
#21901 = CARTESIAN_POINT ( 'NONE',  ( 0.1787899950787401882, -0.2170275590013547307, -2.189545951927503898E-17 ) ) ;
#21902 = CARTESIAN_POINT ( 'NONE',  ( -0.1574803149606297803, 0.02411417333587350526, 0.06523048226347956391 ) ) ;
#21903 = AXIS2_PLACEMENT_3D ( 'NONE', #1260, #12792, #9175 ) ;
#21904 = ORIENTED_EDGE ( 'NONE', *, *, #837, .T. ) ;
#21905 = CARTESIAN_POINT ( 'NONE',  ( 0.6971942568897648851, -0.07405724077823297447, 1.264763779473795813 ) ) ;
#21906 = CARTESIAN_POINT ( 'NONE',  ( 0.002094777259443145277, -0.1352690037933263756, -0.04129845016576910027 ) ) ;
#21907 = DIRECTION ( 'NONE',  ( 0.000000000000000000, 0.000000000000000000, 1.000000000000000000 ) ) ;
#21908 = CARTESIAN_POINT ( 'NONE',  ( 0.9500414927467378812, 0.1787899950787401604, 1.525590551127340433 ) ) ;
#21909 = CARTESIAN_POINT ( 'NONE',  ( 0.6971942568897626646, 0.07405724077823318263, 0.07874015742655145200 ) ) ;
#21910 = CARTESIAN_POINT ( 'NONE',  ( -0.07405724077823318263, -1.572834645615527327, 0.1787899950787401604 ) ) ;
#21911 = CARTESIAN_POINT ( 'NONE',  ( -0.1787899950787401604, -1.690944881836001334, 0.07405724077823318263 ) ) ;
#21912 = EDGE_CURVE ( 'NONE', #25198, #1966, #7064, .T. ) ;
#21913 = CARTESIAN_POINT ( 'NONE',  ( -1.054774247047244096, 0.000000000000000000, 0.4207677164816693294 ) ) ;
#21914 = DIRECTION ( 'NONE',  ( 0.000000000000000000, -1.000000000000000000, 0.000000000000000000 ) ) ;
#21916 = CARTESIAN_POINT ( 'NONE',  ( -0.7204869834275922091, -0.06397302528968762392, 1.984489880467943390 ) ) ;
#21915 = CARTESIAN_POINT ( 'NONE',  ( 0.1270800023317771588, -1.324846959189344364, 0.1270800023317771588 ) ) ;
#21917 = DIRECTION ( 'NONE',  ( -1.000000000000000000, 3.469446951953614189E-15, 1.144917494144692682E-16 ) ) ;
#21918 = CARTESIAN_POINT ( 'NONE',  ( 0.9500414927467378812, -0.1787899950787401604, 1.240157480261197431 ) ) ;
#21919 = CARTESIAN_POINT ( 'NONE',  ( 0.6971942568897648851, -0.07405724077823297447, 1.697834645615527771 ) ) ;
#21920 = EDGE_CURVE ( 'NONE', #23661, #5728, #2195, .T. ) ;
#21921 = DIRECTION ( 'NONE',  ( 0.5735764363510447161, 0.8191520442889925757, 0.000000000000000000 ) ) ;
#21922 = CARTESIAN_POINT ( 'NONE',  ( 0.1608764731649685309, -0.08278090606525061179, 0.1377952755905511861 ) ) ;
#21923 = DIRECTION ( 'NONE',  ( 0.000000000000000000, 0.000000000000000000, -1.000000000000000000 ) ) ;
#21924 = CARTESIAN_POINT ( 'NONE',  ( 1.181102362204724310, 0.000000000000000000, -0.9842519685039370358 ) ) ;
#21925 = PLANE ( 'NONE',  #44579 ) ;
#21926 = CARTESIAN_POINT ( 'NONE',  ( 1.054774247047244096, 0.000000000000000000, 0.1402559054580474474 ) ) ;
#21927 = CARTESIAN_POINT ( 'NONE',  ( 0.7026940052797937541, -0.01276303134770263512, 0.03936938617317344707 ) ) ;
#21928 = CARTESIAN_POINT ( 'NONE',  ( -1.033464566929133799, 0.000000000000000000, 0.5511811022546772021 ) ) ;
#21929 = FACE_OUTER_BOUND ( 'NONE', #1592, .T. ) ;
#21930 = CARTESIAN_POINT ( 'NONE',  ( -1.054774247047244096, 0.000000000000000000, 1.163877952702141672 ) ) ;
#21931 = CARTESIAN_POINT ( 'NONE',  ( 1.033464566929133799, 0.000000000000000000, 0.6299212597349921339 ) ) ;
#21932 = ORIENTED_EDGE ( 'NONE', *, *, #25154, .F. ) ;
#21933 = CARTESIAN_POINT ( 'NONE',  ( -0.7495606340400177148, 0.1264236179284866091, 1.065452755851747924 ) ) ;
#21934 = CARTESIAN_POINT ( 'NONE',  ( -1.033464566929134687, 0.06523048226347956391, 1.114665354330708125 ) ) ;
#21935 = CARTESIAN_POINT ( 'NONE',  ( 0.9040863184708680667, 0.1705322868731493358, 0.03937075118789555572 ) ) ;
#21936 = CARTESIAN_POINT ( 'NONE',  ( 0.7185039370078741827, 0.06523048226347841205, 0.8439960628845994961 ) ) ;
#21937 = CARTESIAN_POINT ( 'NONE',  ( -0.7646288533564489232, 0.1113553986120547346, 0.4478346455617645550 ) ) ;
#21938 = CARTESIAN_POINT ( 'NONE',  ( -1.033464566929133799, 0.000000000000000000, 0.04921259842519685318 ) ) ;
#21939 = CARTESIAN_POINT ( 'NONE',  ( 0.9500414927467378812, 0.1787899950787401604, 1.446850393647023614 ) ) ;
#21940 = CARTESIAN_POINT ( 'NONE',  ( -0.7185039370078739607, 1.928577636452523993E-17, 0.3346456691838114450 ) ) ;
#21941 = CARTESIAN_POINT ( 'NONE',  ( -1.002407869896990045, 0.1264236179284866091, 0.06643700782025216411 ) ) ;
#21942 = CARTESIAN_POINT ( 'NONE',  ( -0.1264236179284866091, -0.1924212597887563214, 0.1264236179284866091 ) ) ;
#21943 = VERTEX_POINT ( 'NONE', #6347 ) ;
#21944 = LINE ( 'NONE', #14756, #9216 ) ;
#21945 = CYLINDRICAL_SURFACE ( 'NONE', #8393, 0.1574803149606299191 ) ;
#21946 = ( CONVERSION_BASED_UNIT ( 'INCH', #39651 ) LENGTH_UNIT ( ) NAMED_UNIT ( #24046 ) ) ;
#21947 = CARTESIAN_POINT ( 'NONE',  ( 1.002407869896990045, -0.1264236179284866091, 0.6520669290800944484 ) ) ;
#21948 = EDGE_LOOP ( 'NONE', ( #1472, #21381, #31263, #36447, #4810 ) ) ;
#21949 = CARTESIAN_POINT ( 'NONE',  ( 0.06523048226347956391, 0.1274606300287869365, -0.1574803149606300301 ) ) ;
#21950 = CARTESIAN_POINT ( 'NONE',  ( -0.9500414927467378812, 0.1787899950787401604, 1.176181102308441417 ) ) ;
#21951 = CARTESIAN_POINT ( 'NONE',  ( -0.7495606340400177148, -0.1264236179284866091, 1.070374015694267600 ) ) ;
#21952 = CARTESIAN_POINT ( 'NONE',  ( -1.002407869896990045, 0.1264236179284866091, 0.7800196849856062542 ) ) ;
#21953 = CARTESIAN_POINT ( 'NONE',  ( -0.1495543973312470909, 0.2091518620004931273, -0.3144333452974443222 ) ) ;
#21954 = CARTESIAN_POINT ( 'NONE',  ( -0.7495606340400177148, 0.1264236179284866091, 0.1993110235682838682 ) ) ;
#21955 = CYLINDRICAL_SURFACE ( 'NONE', #11137, 0.02900000000000056352 ) ;
#21956 = LINE ( 'NONE', #15250, #27485 ) ;
#21957 = CARTESIAN_POINT ( 'NONE',  ( 3.284318927891251994E-17, -0.7545531020875060335, 0.1787899950787401882 ) ) ;
#21958 = VERTEX_POINT ( 'NONE', #25290 ) ;
#21959 = CARTESIAN_POINT ( 'NONE',  ( -0.8759842519685039353, 0.1574803149606299191, 1.466535432963338437 ) ) ;
#21960 = CARTESIAN_POINT ( 'NONE',  ( -0.1377952755905511861, 0.1574803149606320007, -0.8070866141732283561 ) ) ;
#21961 = ORIENTED_EDGE ( 'NONE', *, *, #32611, .T. ) ;
#21962 = CARTESIAN_POINT ( 'NONE',  ( 0.4453382816733590377, 4.766607801171850497E-17, 0.000000000000000000 ) ) ;
#21963 = CARTESIAN_POINT ( 'NONE',  ( -0.6971942568897626646, -0.07405724077823297447, 0.7135826771115916234 ) ) ;
#21964 = CARTESIAN_POINT ( 'NONE',  ( -0.1476377952755905387, 0.2573565155132548909, -0.3015174453633734930 ) ) ;
#21965 = CARTESIAN_POINT ( 'NONE',  ( -0.8019270111902716547, -0.1787899950787401604, 1.825787401521040243 ) ) ;
#21966 = EDGE_CURVE ( 'NONE', #27280, #26206, #35607, .T. ) ;
#21967 = ADVANCED_FACE ( 'NONE', ( #2517 ), #32011, .F. ) ;
#21968 = CARTESIAN_POINT ( 'NONE',  ( -0.7495606340400177148, -0.1264236179284866091, 0.09104330703285078152 ) ) ;
#21969 = CARTESIAN_POINT ( 'NONE',  ( -0.07444174185955065859, -0.8204178253310762114, 0.1797182628040039087 ) ) ;
#21970 = CARTESIAN_POINT ( 'NONE',  ( -0.8759842519685039353, 0.000000000000000000, 2.007874015640504162 ) ) ;
#21971 = CARTESIAN_POINT ( 'NONE',  ( -0.7185039370078746268, -0.06523048226347956391, 1.478838582569637294 ) ) ;
#21972 = CARTESIAN_POINT ( 'NONE',  ( 1.054774247047244096, 0.000000000000000000, 0.7750984251430865779 ) ) ;
#21973 = EDGE_CURVE ( 'NONE', #42574, #15230, #38423, .T. ) ;
#21974 = EDGE_CURVE ( 'NONE', #45730, #3713, #33683, .T. ) ;
#21975 = CARTESIAN_POINT ( 'NONE',  ( -0.2471922904502826812, -0.09842519685039370636, -0.1427165354330708902 ) ) ;
#21976 = CARTESIAN_POINT ( 'NONE',  ( 0.8759842519685039353, 0.1574803149606299191, 1.358267716535433323 ) ) ;
#21978 = DIRECTION ( 'NONE',  ( 0.000000000000000000, 0.000000000000000000, -1.000000000000000000 ) ) ;
#21977 = CARTESIAN_POINT ( 'NONE',  ( 0.7754090590921228765, -0.1384152968776324877, 1.986207984632974766 ) ) ;
#21979 = CARTESIAN_POINT ( 'NONE',  ( 1.033464566929134687, -0.06523048226347956391, 1.493602362097197211 ) ) ;
#21980 = ORIENTED_EDGE ( 'NONE', *, *, #45161, .F. ) ;
#21981 = VECTOR ( 'NONE', #45004, 39.37007874015748143 ) ;
#21983 = CARTESIAN_POINT ( 'NONE',  ( 0.000000000000000000, 0.000000000000000000, -0.3149606299212598381 ) ) ;
#21982 = CARTESIAN_POINT ( 'NONE',  ( 1.002407869896990045, 0.1264236179284866091, 0.7750984251430865779 ) ) ;
#21984 = CARTESIAN_POINT ( 'NONE',  ( -0.07405724077823318263, -0.8198818897100156322, 0.1787899950787401604 ) ) ;
#21985 = CARTESIAN_POINT ( 'NONE',  ( -0.8759842519685039353, 0.000000000000000000, 0.000000000000000000 ) ) ;
#21986 = VERTEX_POINT ( 'NONE', #1043 ) ;
#21987 = CARTESIAN_POINT ( 'NONE',  ( 0.1631287632117340569, 0.08016190229754059648, 0.1388454808432816601 ) ) ;
#21988 = DIRECTION ( 'NONE',  ( 1.000000000000000000, -0.000000000000000000, -0.000000000000000000 ) ) ;
#21989 = CARTESIAN_POINT ( 'NONE',  ( 1.054774247047244540, 0.07405724077823318263, 1.008858267662772423 ) ) ;
#21990 = DIRECTION ( 'NONE',  ( 0.000000000000000000, 1.000000000000000000, 0.000000000000000000 ) ) ;
#21991 = CARTESIAN_POINT ( 'NONE',  ( -0.1574803149606297803, -1.560531496062992574, 0.06523048226347956391 ) ) ;
#21992 = DIRECTION ( 'NONE',  ( 0.000000000000000000, 0.000000000000000000, -1.000000000000000000 ) ) ;
#21993 = CARTESIAN_POINT ( 'NONE',  ( -0.6971942568897637749, 2.189545951927499583E-17, 0.04183070860765386589 ) ) ;
#21994 = CARTESIAN_POINT ( 'NONE',  ( -1.033464566929133799, 0.000000000000000000, 0.7185039370078739607 ) ) ;
#21995 = EDGE_LOOP ( 'NONE', ( #2127, #710, #36847, #18871 ) ) ;
#21996 = CARTESIAN_POINT ( 'NONE',  ( -0.1787899950787401882, -1.422736220418677311, 0.000000000000000000 ) ) ;
#21997 = CARTESIAN_POINT ( 'NONE',  ( -0.6971942568897648851, 0.07405724077823318263, 1.614173228292692386 ) ) ;
#21998 = CARTESIAN_POINT ( 'NONE',  ( -0.7495606340400177148, 0.1264236179284866091, 1.099901574749385880 ) ) ;
#21999 = CARTESIAN_POINT ( 'NONE',  ( -0.6971942568897626646, 0.07405724077823318263, 0.3198818897100162983 ) ) ;
#22000 = CARTESIAN_POINT ( 'NONE',  ( -9.642888182262618425E-18, -0.02755905501058318954, -0.1574803149606299191 ) ) ;
#22001 = CARTESIAN_POINT ( 'NONE',  ( 0.1600813888245113392, 0.05392405859269203128, 0.1404791960285011465 ) ) ;
#22002 = CARTESIAN_POINT ( 'NONE',  ( 0.8019270111902717657, 0.1787899950787401604, 0.07381889758403178958 ) ) ;
#22003 = CARTESIAN_POINT ( 'NONE',  ( 0.000000000000000000, 1.086379535891621506, -0.03715491745705968435 ) ) ;
#22004 = CARTESIAN_POINT ( 'NONE',  ( 0.1787899950787401882, -0.4297499524812070648, -2.189545951927503898E-17 ) ) ;
#22005 = CARTESIAN_POINT ( 'NONE',  ( -0.1643603419142423416, -0.09842519685039370636, -0.06715674897764882523 ) ) ;
#22006 = DIRECTION ( 'NONE',  ( 6.944548107256202097E-15, 0.7880107536067212370, -0.6156614753256591799 ) ) ;
#22007 = DIRECTION ( 'NONE',  ( -1.000000000000000000, 0.000000000000000000, 0.000000000000000000 ) ) ;
#22008 = AXIS2_PLACEMENT_3D ( 'NONE', #10204, #39406, #6588 ) ;
#22009 = CARTESIAN_POINT ( 'NONE',  ( -0.6971942568897626646, -0.07405724077823297447, 0.3592519684501735977 ) ) ;
#22010 = ORIENTED_EDGE ( 'NONE', *, *, #14666, .F. ) ;
#22011 = VERTEX_POINT ( 'NONE', #44408 ) ;
#22012 = CARTESIAN_POINT ( 'NONE',  ( -0.7495606340400177148, -0.1264236179284866091, 1.429625984198204858 ) ) ;
#22013 = ORIENTED_EDGE ( 'NONE', *, *, #17520, .T. ) ;
#22014 = CARTESIAN_POINT ( 'NONE',  ( 0.1264236179284866091, -1.132381889710015743, 0.1264236179284866091 ) ) ;
#22015 = CARTESIAN_POINT ( 'NONE',  ( 0.1264236179284866091, -1.314468503883243988, -0.1264236179284866091 ) ) ;
#22016 = EDGE_CURVE ( 'NONE', #42193, #46242, #7105, .T. ) ;
#22017 = FILL_AREA_STYLE ('',( #432 ) ) ;
#22018 = CARTESIAN_POINT ( 'NONE',  ( 0.3761369780785432937, 0.9186225489821259194, 0.8759842519680709483 ) ) ;
#22019 = DIRECTION ( 'NONE',  ( -1.000000000000000000, 0.000000000000000000, 0.000000000000000000 ) ) ;
#22020 = CARTESIAN_POINT ( 'NONE',  ( -0.8759842519685039353, -0.1574803149606299191, 0.9350393699712126194 ) ) ;
#22021 = CARTESIAN_POINT ( 'NONE',  ( 0.8019270111902717657, -0.1787899950787401604, 0.4478346456155276045 ) ) ;
#22022 = CARTESIAN_POINT ( 'NONE',  ( -0.06523048226347956391, -0.09891732283464571562, 0.1574803149606297803 ) ) ;
#22023 = CARTESIAN_POINT ( 'NONE',  ( 0.9412147342319837628, 0.1574803149606300301, 1.779035432963339991 ) ) ;
#22024 = ORIENTED_EDGE ( 'NONE', *, *, #8756, .F. ) ;
#22025 = EDGE_CURVE ( 'NONE', #9878, #22983, #18331, .T. ) ;
#22026 = CARTESIAN_POINT ( 'NONE',  ( 0.1377952755905511861, 0.1564960629921262614, -0.8070866141732283561 ) ) ;
#22027 = CARTESIAN_POINT ( 'NONE',  ( 0.7185039370078739607, 1.928577636452523993E-17, 0.9350393700787401619 ) ) ;
#22028 = CARTESIAN_POINT ( 'NONE',  ( -0.1158283541424031532, -0.08956345598586890056, -0.1361971163587911426 ) ) ;
#22029 = CARTESIAN_POINT ( 'NONE',  ( 0.1113553986120547346, -0.5147637794200315975, 0.1113553986120547346 ) ) ;
#22030 = CIRCLE ( 'NONE', #43539, 0.1864803149606299171 ) ;
#22032 = CARTESIAN_POINT ( 'NONE',  ( -0.1574803149606299191, -0.2714884749021748145, -1.284167712019358198 ) ) ;
#22031 = DIRECTION ( 'NONE',  ( 0.5735764363510447161, -0.8191520442889925757, 1.003171929053525486E-16 ) ) ;
#22033 = CYLINDRICAL_SURFACE ( 'NONE', #12340, 0.04921259842519676991 ) ;
#22034 = CARTESIAN_POINT ( 'NONE',  ( -0.2833714012347087752, 0.1260629598319807643, 0.9865262584736159690 ) ) ;
#22035 = ORIENTED_EDGE ( 'NONE', *, *, #23605, .F. ) ;
#22036 = DIRECTION ( 'NONE',  ( 0.000000000000000000, -0.1045284632676499320, 0.9945218953682736229 ) ) ;
#22037 = CARTESIAN_POINT ( 'NONE',  ( -0.07405724077823318263, -1.528543307032852239, 0.1787899950787401604 ) ) ;
#22038 = CARTESIAN_POINT ( 'NONE',  ( 0.1113553986120547346, -1.577755905404283343, 0.1113553986120547346 ) ) ;
#22039 = CARTESIAN_POINT ( 'NONE',  ( 0.07405724077823318263, -0.6870078739619840391, -0.1787899950787401604 ) ) ;
#22040 = DIRECTION ( 'NONE',  ( 0.000000000000000000, -1.000000000000000000, 0.000000000000000000 ) ) ;
#22042 = AXIS2_PLACEMENT_3D ( 'NONE', #46798, #35095, #31743 ) ;
#22041 = CARTESIAN_POINT ( 'NONE',  ( -0.06523048226347956391, -1.058562992125983149, -0.1574803149606300301 ) ) ;
#22043 = CARTESIAN_POINT ( 'NONE',  ( 0.8759842519685039353, 0.1574803149606299191, 0.9940944880814488460 ) ) ;
#22044 = LINE ( 'NONE', #3598, #29844 ) ;
#22045 = CARTESIAN_POINT ( 'NONE',  ( -1.054774247047244540, -0.07405724077823318263, 0.3740157479777325711 ) ) ;
#22046 = ORIENTED_EDGE ( 'NONE', *, *, #28433, .F. ) ;
#22047 = ORIENTED_EDGE ( 'NONE', *, *, #28773, .F. ) ;
#22048 = CARTESIAN_POINT ( 'NONE',  ( -1.054774247047244540, 0.07405724077823318263, 1.683070866087970074 ) ) ;
#22049 = CARTESIAN_POINT ( 'NONE',  ( 1.002407869896990045, 0.1264236179284866091, 1.646161417269070837 ) ) ;
#22050 = CARTESIAN_POINT ( 'NONE',  ( -9.642888182262618425E-18, -1.326771653435779408, -0.1574803149606299191 ) ) ;
#22051 = CARTESIAN_POINT ( 'NONE',  ( -0.8019270111902717657, 0.1787899950787401604, 0.7480314960092282472 ) ) ;
#22052 = CARTESIAN_POINT ( 'NONE',  ( 0.6971942568897637749, 2.189545951927499583E-17, 0.3223425196312759144 ) ) ;
#22053 = CARTESIAN_POINT ( 'NONE',  ( -0.9873396505805591694, -0.1113553986120547346, 0.4675196849318432601 ) ) ;
#22054 = CARTESIAN_POINT ( 'NONE',  ( 0.8019270111902716547, 0.1787899950787401604, 0.7086614172690703928 ) ) ;
#22055 = CARTESIAN_POINT ( 'NONE',  ( -0.6971942568897648851, -0.07405724077823297447, 0.6742125983714336579 ) ) ;
#22056 = CARTESIAN_POINT ( 'NONE',  ( 0.1574803149606300301, -0.07923228335703978720, 0.06523048226347956391 ) ) ;
#22057 = ( BOUNDED_CURVE ( )  B_SPLINE_CURVE ( 2, ( #2068, #27274, #42539, #38956, #9025, #9743, #45661, #5668, #38496 ),
 .UNSPECIFIED., .F., .F. ) 
 B_SPLINE_CURVE_WITH_KNOTS ( ( 3, 2, 2, 2, 3 ),
 ( 0.9399999999999999467, 0.9425000000000000044, 0.9449999999999999512, 0.9475000000000000089, 0.9499999999999999556 ),
 .UNSPECIFIED. ) 
 CURVE ( )  GEOMETRIC_REPRESENTATION_ITEM ( )  RATIONAL_B_SPLINE_CURVE ( ( 1.000000000000000000, 0.9238795325112899581, 1.000000000000000000, 0.9238795325112869605, 1.000000000000000000, 0.9238795325112869605, 1.000000000000000000, 0.9238795325112829637, 1.000000000000000000 ) ) 
 REPRESENTATION_ITEM ( '' )  ) ;
#22058 = CARTESIAN_POINT ( 'NONE',  ( -0.8759842519685039353, -0.1787899950787401882, 1.592027559001354398 ) ) ;
#22059 = CARTESIAN_POINT ( 'NONE',  ( -0.8107537697050253289, 0.1574803149606300301, 1.862696850286174710 ) ) ;
#22060 = VERTEX_POINT ( 'NONE', #40808 ) ;
#22061 = CARTESIAN_POINT ( 'NONE',  ( -0.7185039370078739607, 1.928577636452523993E-17, 1.643700787401574992 ) ) ;
#22062 = DIRECTION ( 'NONE',  ( -1.000000000000000000, 0.000000000000000000, 0.000000000000000000 ) ) ;
#22063 = CARTESIAN_POINT ( 'NONE',  ( 0.8019270111902716547, -0.1787899950787401604, 1.392716535379308285 ) ) ;
#22064 = DIRECTION ( 'NONE',  ( 1.000000000000000000, 0.000000000000000000, 0.000000000000000000 ) ) ;
#22065 = ORIENTED_EDGE ( 'NONE', *, *, #16377, .F. ) ;
#22066 = AXIS2_PLACEMENT_3D ( 'NONE', #17204, #13386, #28731 ) ;
#22067 = VERTEX_POINT ( 'NONE', #4632 ) ;
#22068 = VERTEX_POINT ( 'NONE', #22868 ) ;
#22069 = CARTESIAN_POINT ( 'NONE',  ( -0.1968503937007874127, 0.1005108776172154716, -0.1165245190822937205 ) ) ;
#22070 = CIRCLE ( 'NONE', #29754, 0.1864803149606298893 ) ;
#22071 = ( BOUNDED_CURVE ( )  B_SPLINE_CURVE ( 2, ( #40403, #22686, #33271, #12152, #33974, #7590, #1100, #26775, #41335 ),
 .UNSPECIFIED., .F., .T. ) 
 B_SPLINE_CURVE_WITH_KNOTS ( ( 3, 2, 2, 2, 3 ),
 ( 0.7099999999999999645, 0.7125000000000000222, 0.7149999999999999689, 0.7175000000000000266, 0.7199999999999999734 ),
 .UNSPECIFIED. ) 
 CURVE ( )  GEOMETRIC_REPRESENTATION_ITEM ( )  RATIONAL_B_SPLINE_CURVE ( ( 1.000000000000000000, 0.9238795325112869605, 1.000000000000000000, 0.9238795325112869605, 1.000000000000000000, 0.9238795325112869605, 1.000000000000000000, 0.9238795325112869605, 1.000000000000000000 ) ) 
 REPRESENTATION_ITEM ( '' )  ) ;
#22072 = CARTESIAN_POINT ( 'NONE',  ( -0.1787899950787401604, -0.8690944881352120621, -0.07405724077823318263 ) ) ;
#22073 = VERTEX_POINT ( 'NONE', #8242 ) ;
#22074 = ADVANCED_FACE ( 'NONE', ( #4165 ), #37481, .T. ) ;
#22075 = CARTESIAN_POINT ( 'NONE',  ( 0.4736248074375818407, 0.9382165298418937427, -1.070508272602714639 ) ) ;
#22076 = CARTESIAN_POINT ( 'NONE',  ( 0.6971942568897637749, 2.189545951927502049E-17, 4.498031496062992574 ) ) ;
#22077 = CARTESIAN_POINT ( 'NONE',  ( 1.054774247047244540, -0.07405724077823318263, 1.791338582623401177 ) ) ;
#22078 = CARTESIAN_POINT ( 'NONE',  ( 0.1270800023317771588, -0.2520123135200535436, -0.1270800023317771588 ) ) ;
#22079 = CARTESIAN_POINT ( 'NONE',  ( -0.1787899950787401604, -0.1763050705914436245, -0.07405724077823318263 ) ) ;
#22080 = CARTESIAN_POINT ( 'NONE',  ( -0.1264236179284866091, -0.04970472435568527164, -0.1264236179284866091 ) ) ;
#22081 = CARTESIAN_POINT ( 'NONE',  ( 0.7185039370078746268, -0.06523048226347956391, 0.1402559054042841202 ) ) ;
#22082 = EDGE_CURVE ( 'NONE', #3381, #39582, #23099, .T. ) ;
#22083 = CARTESIAN_POINT ( 'NONE',  ( 0.9500414927467378812, 0.1787899950787401604, 0.6594488188438737408 ) ) ;
#22084 = ( NAMED_UNIT ( * ) PLANE_ANGLE_UNIT ( ) SI_UNIT ( $, .RADIAN. ) ) ;
#22085 = CARTESIAN_POINT ( 'NONE',  ( 0.7185039370078739607, 1.928577636452523993E-17, 0.6889763778452283605 ) ) ;
#22086 = CARTESIAN_POINT ( 'NONE',  ( 0.8107537697050254399, 0.1574803149606300301, 0.9571850392625507187 ) ) ;
#22087 = CARTESIAN_POINT ( 'NONE',  ( 0.6971942568897637749, 2.189545951927499583E-17, 1.897145669237574772 ) ) ;
#22089 = CARTESIAN_POINT ( 'NONE',  ( 0.8759842519685039353, 0.1574803149606299191, 0.1279527557979848462 ) ) ;
#22088 = CARTESIAN_POINT ( 'NONE',  ( -0.2362204724409471546, 2.422684756221294423E-15, -0.9891732283464564901 ) ) ;
#22090 = CARTESIAN_POINT ( 'NONE',  ( 0.1586955767088436831, -0.09170575825941058856, 0.1167515185291693181 ) ) ;
#22091 = CARTESIAN_POINT ( 'NONE',  ( -0.07405724077823318263, -0.3523622046706461619, 0.1787899950787401604 ) ) ;
#22092 = CARTESIAN_POINT ( 'NONE',  ( 0.1592537043533210628, 0.1452344447278379747, 0.02937400284934486849 ) ) ;
#22093 = CARTESIAN_POINT ( 'NONE',  ( -1.094772975963752103E-17, -1.033956692859621995, -0.1787899950787401882 ) ) ;
#22094 = CARTESIAN_POINT ( 'NONE',  ( 0.7495606340400177148, 0.1264236179284866091, 0.08120078734781142893 ) ) ;
#22095 = CARTESIAN_POINT ( 'NONE',  ( 0.2471922904502826812, -0.03219022224904106305, 0.1427165354330708902 ) ) ;
#22096 = AXIS2_PLACEMENT_3D ( 'NONE', #6103, #24802, #32003 ) ;
#22097 = CARTESIAN_POINT ( 'NONE',  ( -1.054774247047244540, -0.07405724077823318263, 1.673228346402929834 ) ) ;
#22098 = VERTEX_POINT ( 'NONE', #15701 ) ;
#22099 = CARTESIAN_POINT ( 'NONE',  ( -1.002407869896990045, 0.1264236179284866091, 1.173720472387181246 ) ) ;
#22100 = CARTESIAN_POINT ( 'NONE',  ( 0.7185039370078739607, 1.928577636452523993E-17, 0.2952755904436539236 ) ) ;
#22101 = CARTESIAN_POINT ( 'NONE',  ( 0.8019270111902717657, -0.1787899950787401604, 0.05413385821395302888 ) ) ;
#22102 = CARTESIAN_POINT ( 'NONE',  ( -0.7646288533564489232, -0.1113553986120547346, 0.6250000000000000000 ) ) ;
#22103 = CARTESIAN_POINT ( 'NONE',  ( -1.054774247047244540, 0.07405724077823318263, 1.126968503883244654 ) ) ;
#22104 = DIRECTION ( 'NONE',  ( -1.000000000000000000, 0.000000000000000000, 0.000000000000000000 ) ) ;
#22105 = CARTESIAN_POINT ( 'NONE',  ( -0.1154865254642846034, -0.2288180556978286484, -0.02742975588280020111 ) ) ;
#22106 = CARTESIAN_POINT ( 'NONE',  ( 0.8019270111902716547, 0.1787899950787401604, 0.3149606298674962890 ) ) ;
#22107 = CARTESIAN_POINT ( 'NONE',  ( -1.054774247047244540, 0.07405724077823318263, 0.3001968503399373711 ) ) ;
#22108 = PRODUCT_DEFINITION_CONTEXT ( 'detailed design', #12884, 'design' ) ;
#22109 = CARTESIAN_POINT ( 'NONE',  ( -1.002407869896990045, -0.1264236179284866091, 0.7652559054580472253 ) ) ;
#22110 = CARTESIAN_POINT ( 'NONE',  ( 0.8107537697050253289, -0.1574803149606297803, 1.719980314853102321 ) ) ;
#22111 = ORIENTED_EDGE ( 'NONE', *, *, #40129, .F. ) ;
#22112 = VECTOR ( 'NONE', #3791, 39.37007874015748854 ) ;
#22113 = CARTESIAN_POINT ( 'NONE',  ( -0.1787899950787401604, 0.03641732288840918152, 0.07405724077823318263 ) ) ;
#22114 = VERTEX_POINT ( 'NONE', #30336 ) ;
#22115 = CARTESIAN_POINT ( 'NONE',  ( 1.002407869896990045, 0.1264236179284866091, 0.7800196849856062542 ) ) ;
#22116 = AXIS2_PLACEMENT_3D ( 'NONE', #14748, #37247, #4399 ) ;
#22117 = CARTESIAN_POINT ( 'NONE',  ( -0.7495606340400177148, 0.1264236179284866091, 1.887303149552535420 ) ) ;
#22118 = ORIENTED_EDGE ( 'NONE', *, *, #27522, .F. ) ;
#22119 = CARTESIAN_POINT ( 'NONE',  ( 0.9500414927467378812, 0.1787899950787401604, 1.879921259788756016 ) ) ;
#22120 = CARTESIAN_POINT ( 'NONE',  ( 0.8070866141732283561, -0.0009842519685049383633, 0.6590551181102368705 ) ) ;
#22121 = CARTESIAN_POINT ( 'NONE',  ( -0.1787899950787401604, -1.234375936733175916, 0.07405724077823318263 ) ) ;
#22122 = ORIENTED_EDGE ( 'NONE', *, *, #23171, .F. ) ;
#22123 = CARTESIAN_POINT ( 'NONE',  ( 0.07405724077823318263, -0.2490157479777327099, -0.1787899950787401604 ) ) ;
#22124 = ADVANCED_FACE ( 'NONE', ( #26483 ), #39917, .T. ) ;
#22125 = CARTESIAN_POINT ( 'NONE',  ( -9.642888182262618425E-18, 0.01181102372957427288, -0.1574803149606299191 ) ) ;
#22126 = EDGE_LOOP ( 'NONE', ( #45946, #30891, #4709, #4126 ) ) ;
#22127 = CARTESIAN_POINT ( 'NONE',  ( 1.002407869896990045, 0.1264236179284866091, 1.168799212544661348 ) ) ;
#22128 = PLANE ( 'NONE',  #23303 ) ;
#22129 = DIRECTION ( 'NONE',  ( 0.000000000000000000, 1.000000000000000000, 0.000000000000000000 ) ) ;
#22130 = EDGE_CURVE ( 'NONE', #29781, #2057, #40344, .T. ) ;
#22131 = CIRCLE ( 'NONE', #25185, 0.09842519685039370636 ) ;
#22132 = CARTESIAN_POINT ( 'NONE',  ( 0.6971942568897626646, -0.07405724077823297447, 0.08366141726907129483 ) ) ;
#22133 = CARTESIAN_POINT ( 'NONE',  ( -0.1264236179284866091, -1.624507873961984261, -0.1264236179284866091 ) ) ;
#22134 = ADVANCED_FACE ( 'NONE', ( #37240 ), #18790, .T. ) ;
#22135 = AXIS2_PLACEMENT_3D ( 'NONE', #7144, #2355, #6895 ) ;
#22136 = CARTESIAN_POINT ( 'NONE',  ( -0.8019270111902716547, 0.1787899950787401604, 0.4724409448281262636 ) ) ;
#22137 = CARTESIAN_POINT ( 'NONE',  ( 0.9412147342319837628, -0.1574803149606297803, 0.3075787400499532809 ) ) ;
#22139 = CARTESIAN_POINT ( 'NONE',  ( -0.7103339159022584726, 0.006824654076337659594, 1.983144407867949655 ) ) ;
#22138 = CARTESIAN_POINT ( 'NONE',  ( -0.1797182628040039087, -1.494630423756273085, 0.07444174185955065859 ) ) ;
#22140 = CARTESIAN_POINT ( 'NONE',  ( 0.8759842519685039353, 0.1574803149606299191, 1.437007874015747921 ) ) ;
#22141 = CARTESIAN_POINT ( 'NONE',  ( 0.7495606340400177148, -0.1264236179284866091, 1.193405511757259951 ) ) ;
#22142 = CARTESIAN_POINT ( 'NONE',  ( 0.7495606340400177148, 0.1264236179284866091, 1.611712598371433103 ) ) ;
#22143 = CARTESIAN_POINT ( 'NONE',  ( -0.006597203818611992697, 0.1299212598425198428, 0.1741786893156897775 ) ) ;
#22144 = CARTESIAN_POINT ( 'NONE',  ( 0.9412147342319837628, -0.1574803149606297803, 0.8981299211523156023 ) ) ;
#22145 = CARTESIAN_POINT ( 'NONE',  ( -1.033464566929133799, 0.000000000000000000, 1.938976377952756014 ) ) ;
#22146 = CARTESIAN_POINT ( 'NONE',  ( 0.9412147342319837628, -0.1574803149606297803, 0.5437992124908980207 ) ) ;
#22147 = CARTESIAN_POINT ( 'NONE',  ( -1.033464566929134687, -0.06523048226347956391, 1.729822834538142784 ) ) ;
#22148 = LINE ( 'NONE', #563, #44431 ) ;
#22149 = CARTESIAN_POINT ( 'NONE',  ( -0.8019270111902717657, 0.1787899950787401604, 1.254921259788757348 ) ) ;
#22150 = CARTESIAN_POINT ( 'NONE',  ( 0.7185039370078739607, 1.928577636452523993E-17, 0.7283464565853858819 ) ) ;
#22151 = EDGE_LOOP ( 'NONE', ( #20417, #11069, #17181, #30915 ) ) ;
#22152 = CARTESIAN_POINT ( 'NONE',  ( 0.1574803149606299191, -0.5708661417322835607, 0.9783464566929134243 ) ) ;
#22153 = CARTESIAN_POINT ( 'NONE',  ( 0.8857703219174262177, 0.1737007691241557183, 0.03937007805475359334 ) ) ;
#22154 = CARTESIAN_POINT ( 'NONE',  ( -1.033464566929134687, 0.06523048226347956391, 1.587106299212598604 ) ) ;
#22155 = CARTESIAN_POINT ( 'NONE',  ( 1.054774247047244540, 0.07405724077823318263, 1.638779527505292988 ) ) ;
#22156 = CARTESIAN_POINT ( 'NONE',  ( -0.7185039370078739607, 1.928577636452523993E-17, 1.171259842519684957 ) ) ;
#22157 = CARTESIAN_POINT ( 'NONE',  ( 0.7185039370078746268, 0.06523048226347956391, 1.916830708661418026 ) ) ;
#22158 = CARTESIAN_POINT ( 'NONE',  ( -0.07405724077823318263, -0.2047244093950554844, -0.1787899950787401604 ) ) ;
#22159 = CARTESIAN_POINT ( 'NONE',  ( 1.033464566929134687, -0.06523048226347956391, 1.336122047136566904 ) ) ;
#22160 = ORIENTED_EDGE ( 'NONE', *, *, #19536, .F. ) ;
#22161 = CARTESIAN_POINT ( 'NONE',  ( 0.2471922904502826812, -0.03219022224904102836, -0.1427165354330708902 ) ) ;
#22162 = CARTESIAN_POINT ( 'NONE',  ( 0.9500414927467378812, 0.1787899950787401604, 0.5856299212060785964 ) ) ;
#22163 = VERTEX_POINT ( 'NONE', #41276 ) ;
#22164 = CARTESIAN_POINT ( 'NONE',  ( -1.054774247047244540, 0.07405724077823318263, 1.441929133804504604 ) ) ;
#22165 = CARTESIAN_POINT ( 'NONE',  ( -0.06523048226347956391, 0.1077755906587081480, 0.1574803149606297803 ) ) ;
#22166 = CARTESIAN_POINT ( 'NONE',  ( -0.8759842519685039353, -0.1787899950787401882, 1.198326771599779628 ) ) ;
#22167 = EDGE_LOOP ( 'NONE', ( #2588, #26151, #42026, #46031 ) ) ;
#22168 = EDGE_CURVE ( 'NONE', #33889, #29837, #94, .T. ) ;
#22169 = CARTESIAN_POINT ( 'NONE',  ( -0.2559055118110236116, -0.1477471161312049197, -0.1122047244094488277 ) ) ;
#22170 = CIRCLE ( 'NONE', #7627, 0.09842519685039370636 ) ;
#22171 = CARTESIAN_POINT ( 'NONE',  ( -0.6971942568897626646, -0.07405724077823297447, 0.8366141731745828647 ) ) ;
#22172 = EDGE_CURVE ( 'NONE', #17741, #19150, #31535, .T. ) ;
#22173 = CARTESIAN_POINT ( 'NONE',  ( -0.7495606340400177148, 0.1264236179284866091, 0.2386811023084413619 ) ) ;
#22174 = DIRECTION ( 'NONE',  ( 0.000000000000000000, 0.000000000000000000, -1.000000000000000000 ) ) ;
#22175 = CARTESIAN_POINT ( 'NONE',  ( 1.033464566929136907, -0.06523048226347749612, 1.651082677057827519 ) ) ;
#22176 = CARTESIAN_POINT ( 'NONE',  ( 0.1787899950787401604, -0.8603601887016788519, -0.07405724077823318263 ) ) ;
#22177 = ORIENTED_EDGE ( 'NONE', *, *, #25029, .T. ) ;
#22178 = AXIS2_PLACEMENT_3D ( 'NONE', #15720, #23837, #38449 ) ;
#22179 = CARTESIAN_POINT ( 'NONE',  ( 0.07405724077823318263, 0.1446850394238423654, -0.1787899950787401604 ) ) ;
#22180 = VERTEX_POINT ( 'NONE', #14740 ) ;
#22181 = EDGE_CURVE ( 'NONE', #18659, #23819, #40577, .T. ) ;
#22182 = ORIENTED_EDGE ( 'NONE', *, *, #32939, .F. ) ;
#22183 = CARTESIAN_POINT ( 'NONE',  ( 0.8759842519685039353, -0.1574803149606299191, 1.210629921152315047 ) ) ;
#22184 = CARTESIAN_POINT ( 'NONE',  ( -1.054774247047244540, -0.07405724077823318263, 0.7677165353793073965 ) ) ;
#22185 = ( BOUNDED_CURVE ( )  B_SPLINE_CURVE ( 2, ( #13422, #32353, #10537, #28520, #39033, #35917, #13638, #35695, #35464 ),
 .UNSPECIFIED., .F., .T. ) 
 B_SPLINE_CURVE_WITH_KNOTS ( ( 3, 2, 2, 2, 3 ),
 ( 0.5100000000000000089, 0.5124999999999999556, 0.5150000000000000133, 0.5174999999999999600, 0.5200000000000000178 ),
 .UNSPECIFIED. ) 
 CURVE ( )  GEOMETRIC_REPRESENTATION_ITEM ( )  RATIONAL_B_SPLINE_CURVE ( ( 1.000000000000000000, 0.9238795325112869605, 1.000000000000000000, 0.9238795325112869605, 1.000000000000000000, 0.9238795325112869605, 1.000000000000000000, 0.9238795325112869605, 1.000000000000000000 ) ) 
 REPRESENTATION_ITEM ( '' )  ) ;
#22186 = ORIENTED_EDGE ( 'NONE', *, *, #29670, .F. ) ;
#22187 = CARTESIAN_POINT ( 'NONE',  ( -1.054774247047244540, -0.07405724077823318263, 1.835629921206078485 ) ) ;
#22188 = EDGE_CURVE ( 'NONE', #13130, #8550, #13133, .T. ) ;
#22189 = AXIS2_PLACEMENT_3D ( 'NONE', #39245, #6419, #35901 ) ;
#22190 = ADVANCED_FACE ( 'NONE', ( #42245 ), #41435, .F. ) ;
#22191 = CARTESIAN_POINT ( 'NONE',  ( -0.9500414927467377701, 0.1787899950787401604, 0.07381889758403178958 ) ) ;
#22192 = CARTESIAN_POINT ( 'NONE',  ( 0.1797182628040039365, -0.9655949906854075504, -2.200913952912460540E-17 ) ) ;
#22193 = DIRECTION ( 'NONE',  ( -1.000000000000000000, 3.469446951953613794E-15, 1.144917494144692682E-16 ) ) ;
#22194 = CARTESIAN_POINT ( 'NONE',  ( -0.7646288533564489232, -0.1113553986120547346, 1.481299212490897466 ) ) ;
#22195 = CARTESIAN_POINT ( 'NONE',  ( 1.054774247047244540, 0.07405724077823318263, 0.8169291338045038264 ) ) ;
#22196 = CARTESIAN_POINT ( 'NONE',  ( 0.8759842519685039353, -0.1787899950787401882, 1.350885826717889815 ) ) ;
#22197 = DIRECTION ( 'NONE',  ( -0.000000000000000000, 0.6156614753256597350, 0.7880107536067206819 ) ) ;
#22198 = CARTESIAN_POINT ( 'NONE',  ( 0.7646288533564489232, 0.1113553986120547346, 1.441929133858267598 ) ) ;
#22200 = LINE ( 'NONE', #4213, #8593 ) ;
#22199 = CARTESIAN_POINT ( 'NONE',  ( 0.7836433926840684627, -0.1444537073663495208, 1.986395014210853738 ) ) ;
#22201 = VECTOR ( 'NONE', #41591, 39.37007874015748143 ) ;
#22202 = CARTESIAN_POINT ( 'NONE',  ( -1.033464566929133799, 0.000000000000000000, 0.9055118109160944506 ) ) ;
#22203 = CARTESIAN_POINT ( 'NONE',  ( -0.1574803149606297803, -0.6845472439869605408, 0.06523048226347956391 ) ) ;
#22205 = DIRECTION ( 'NONE',  ( 0.000000000000000000, 0.000000000000000000, -1.000000000000000000 ) ) ;
#22204 = CARTESIAN_POINT ( 'NONE',  ( 0.7495606340400177148, 0.1264236179284866091, 0.9030511810485984947 ) ) ;
#22206 = CARTESIAN_POINT ( 'NONE',  ( -0.07405724077823318263, -0.7017716534895438452, 0.1787899950787401604 ) ) ;
#22207 = DIRECTION ( 'NONE',  ( 0.000000000000000000, -1.020425574104001164E-16, 1.000000000000000000 ) ) ;
#22208 = CARTESIAN_POINT ( 'NONE',  ( -1.033464566929133799, 0.000000000000000000, 0.8366141732283465249 ) ) ;
#22209 = DIRECTION ( 'NONE',  ( 1.822029033848725028E-16, 0.000000000000000000, 1.000000000000000000 ) ) ;
#22210 = CARTESIAN_POINT ( 'NONE',  ( 0.6971942568897648851, -0.07405724077823297447, 1.028543307032851795 ) ) ;
#22211 = CARTESIAN_POINT ( 'NONE',  ( 0.1574803149606299191, -0.5708661417322835607, -6.991093932140394160E-17 ) ) ;
#22212 = CARTESIAN_POINT ( 'NONE',  ( -0.06523048226347956391, -1.649114173228347413, -0.1574803149606300301 ) ) ;
#22213 = CARTESIAN_POINT ( 'NONE',  ( 0.2395294000716133853, 0.1968503937007874127, 0.4921259842519685179 ) ) ;
#22214 = EDGE_LOOP ( 'NONE', ( #2375, #25891, #36622, #35348 ) ) ;
#22215 = DIRECTION ( 'NONE',  ( 0.000000000000000000, 0.000000000000000000, -1.000000000000000000 ) ) ;
#22216 = CARTESIAN_POINT ( 'NONE',  ( -0.9500414927467378812, 0.1787899950787401604, 0.06889763774151215492 ) ) ;
#22217 = EDGE_LOOP ( 'NONE', ( #34827, #27613, #8011 ) ) ;
#22218 = CARTESIAN_POINT ( 'NONE',  ( -0.8107537697050254399, -0.1574803149606297803, 0.7062007874015745479 ) ) ;
#22219 = CARTESIAN_POINT ( 'NONE',  ( 1.033464566929134687, -0.06523048226347956391, 0.3518700786326304231 ) ) ;
#22220 = CARTESIAN_POINT ( 'NONE',  ( -1.054774247047244540, -0.07405724077823318263, 1.751968503883245765 ) ) ;
#22221 = EDGE_CURVE ( 'NONE', #40227, #42395, #35357, .T. ) ;
#22222 = CARTESIAN_POINT ( 'NONE',  ( -1.002407869896990045, 0.1264236179284866091, 1.050688976324189117 ) ) ;
#22223 = ADVANCED_FACE ( 'NONE', ( #16853 ), #3973, .T. ) ;
#22224 = DIRECTION ( 'NONE',  ( -1.000000000000000000, 3.469446951953614189E-15, 0.000000000000000000 ) ) ;
#22225 = CARTESIAN_POINT ( 'NONE',  ( 0.8759842519685039353, -0.1574803149606299191, 0.9842519685039370358 ) ) ;
#22226 = CARTESIAN_POINT ( 'NONE',  ( 0.05275482926409180012, 0.07559918600399875843, -0.2549750559894655155 ) ) ;
#22227 = CARTESIAN_POINT ( 'NONE',  ( -0.2802144182493689351, 0.1328525842424026215, -0.7736900671310529276 ) ) ;
#22228 = CARTESIAN_POINT ( 'NONE',  ( -0.1264236179284866091, -0.4051436532686086833, 0.1264236179284866091 ) ) ;
#22229 = CARTESIAN_POINT ( 'NONE',  ( -0.2247554567094850464, -0.08955974650949173610, -0.08956146268411240008 ) ) ;
#22230 = DIRECTION ( 'NONE',  ( 1.000000000000000000, -3.469446951953614189E-15, -0.000000000000000000 ) ) ;
#22231 = CARTESIAN_POINT ( 'NONE',  ( -0.4620708661417322616, 0.9842519685039375910, -0.5511811023622041894 ) ) ;
#22232 = EDGE_CURVE ( 'NONE', #12067, #10459, #16202, .T. ) ;
#22233 = VECTOR ( 'NONE', #35075, 39.37007874015748143 ) ;
#22234 = EDGE_CURVE ( 'NONE', #21841, #44803, #26950, .T. ) ;
#22235 = VECTOR ( 'NONE', #16633, 39.37007874015748143 ) ;
#22236 = CARTESIAN_POINT ( 'NONE',  ( -0.8019270111902717657, -0.1787899950787401604, 0.2854330708123783422 ) ) ;
#22237 = ORIENTED_EDGE ( 'NONE', *, *, #7951, .T. ) ;
#22238 = CARTESIAN_POINT ( 'NONE',  ( 0.7646288533564489232, 0.1113553986120547346, 0.8120078740157481434 ) ) ;
#22239 = EDGE_LOOP ( 'NONE', ( #43258, #7452, #33006, #26870, #6170, #47116 ) ) ;
#22240 = CARTESIAN_POINT ( 'NONE',  ( -0.9500414927467377701, -0.1787899950787401604, 1.397637795221827517 ) ) ;
#22241 = ORIENTED_EDGE ( 'NONE', *, *, #34217, .F. ) ;
#22242 = CARTESIAN_POINT ( 'NONE',  ( -0.1264236179284866091, -1.299704724355684959, 0.1264236179284866091 ) ) ;
#22243 = CARTESIAN_POINT ( 'NONE',  ( -0.1787899950787401882, -1.614665354276944909, 0.000000000000000000 ) ) ;
#22244 = DIRECTION ( 'NONE',  ( 1.000000000000000000, 0.000000000000000000, 0.000000000000000000 ) ) ;
#22245 = CARTESIAN_POINT ( 'NONE',  ( 0.8107537697050253289, -0.1574803149606297803, 0.3518700787401576324 ) ) ;
#22246 = CARTESIAN_POINT ( 'NONE',  ( 0.1270800023317771588, -0.6161855418665097561, 0.1270800023317771588 ) ) ;
#22247 = LINE ( 'NONE', #36421, #29419 ) ;
#22248 = CARTESIAN_POINT ( 'NONE',  ( -0.7185039370078746268, -0.06523048226347956391, 1.085137795168063413 ) ) ;
#22249 = CARTESIAN_POINT ( 'NONE',  ( 0.7495606340400177148, -0.1264236179284866091, 0.4060039369541102450 ) ) ;
#22250 = CARTESIAN_POINT ( 'NONE',  ( -0.9873396505805591694, -0.1113553986120547346, 1.491141732175936818 ) ) ;
#22251 = CARTESIAN_POINT ( 'NONE',  ( -0.1574803149606299191, -0.2637795275590551491, 0.000000000000000000 ) ) ;
#22252 = CARTESIAN_POINT ( 'NONE',  ( 0.7185039370078746268, -0.06523048226347956391, 1.951279527451529772 ) ) ;
#22253 = ORIENTED_EDGE ( 'NONE', *, *, #2433, .T. ) ;
#22254 = CARTESIAN_POINT ( 'NONE',  ( 0.2066929133858268486, -0.5175744617845222662, -0.9076376772307633845 ) ) ;
#22255 = CARTESIAN_POINT ( 'NONE',  ( 0.7646288533564489232, 0.1113553986120547346, 1.008858267716535417 ) ) ;
#22256 = CARTESIAN_POINT ( 'NONE',  ( -1.033464566929133799, 0.000000000000000000, 1.850393700679873854 ) ) ;
#22257 = VECTOR ( 'NONE', #19791, 39.37007874015748143 ) ;
#22258 = CARTESIAN_POINT ( 'NONE',  ( -0.2362204724409466272, 0.1574803149606323616, -1.186023622047243986 ) ) ;
#22259 = CARTESIAN_POINT ( 'NONE',  ( -0.1796295154119676718, -0.08412760742784908263, -0.1817225848796409637 ) ) ;
#22260 = CARTESIAN_POINT ( 'NONE',  ( -0.2644617891023673395, 0.1618364700813163526, 0.8320631914506742000 ) ) ;
#22261 = VERTEX_POINT ( 'NONE', #37963 ) ;
#22262 = DIRECTION ( 'NONE',  ( 0.000000000000000000, 0.000000000000000000, -1.000000000000000000 ) ) ;
#22263 = CARTESIAN_POINT ( 'NONE',  ( -1.033464566929134687, -0.06523048226347956391, 0.9916338582677169944 ) ) ;
#22264 = CARTESIAN_POINT ( 'NONE',  ( 0.1264236179284866091, -1.599901574749385880, 0.1264236179284866091 ) ) ;
#22265 = CARTESIAN_POINT ( 'NONE',  ( -0.1787899950787401882, -0.7140748030958424808, 0.000000000000000000 ) ) ;
#22266 = AXIS2_PLACEMENT_3D ( 'NONE', #34324, #42177, #45307 ) ;
#22267 = CARTESIAN_POINT ( 'NONE',  ( -0.06523048226347956391, -1.216043307086613012, -0.1574803149606300301 ) ) ;
#22268 = CARTESIAN_POINT ( 'NONE',  ( 0.9412147342319837628, 0.1574803149606300301, 1.031003936900347639 ) ) ;
#22269 = CARTESIAN_POINT ( 'NONE',  ( 1.033464566929134687, 0.06523048226347956391, 1.823326771653542178 ) ) ;
#22270 = CARTESIAN_POINT ( 'NONE',  ( -0.8019270111902717657, 0.1787899950787401604, 0.3887795275052913224 ) ) ;
#22271 = ORIENTED_EDGE ( 'NONE', *, *, #1994, .T. ) ;
#22272 = ORIENTED_EDGE ( 'NONE', *, *, #14131, .F. ) ;
#22273 = VERTEX_POINT ( 'NONE', #26959 ) ;
#22274 = CARTESIAN_POINT ( 'NONE',  ( -1.054774247047244540, 0.07405724077823318263, 1.643700787347811998 ) ) ;
#22275 = VECTOR ( 'NONE', #26246, 39.37007874015748143 ) ;
#22276 = CARTESIAN_POINT ( 'NONE',  ( 1.054774247047244540, -0.07405724077823318263, 1.717519684985606476 ) ) ;
#22277 = CARTESIAN_POINT ( 'NONE',  ( -0.6971942568897626646, -0.07405724077823297447, 0.7578740156942689321 ) ) ;
#22278 = DIRECTION ( 'NONE',  ( 0.000000000000000000, -1.000000000000000000, -0.000000000000000000 ) ) ;
#22279 = CARTESIAN_POINT ( 'NONE',  ( 0.8759842519685039353, -0.1787899950787401882, 0.2534448818360003908 ) ) ;
#22280 = DIRECTION ( 'NONE',  ( 0.000000000000000000, 0.000000000000000000, 1.000000000000000000 ) ) ;
#22281 = CARTESIAN_POINT ( 'NONE',  ( -1.054774247047244096, 0.000000000000000000, 1.203248031442299304 ) ) ;
#22282 = CARTESIAN_POINT ( 'NONE',  ( -1.054774247047244540, -0.07405724077823318263, 0.8070866141194653620 ) ) ;
#22283 = CARTESIAN_POINT ( 'NONE',  ( 0.9412147342319837628, 0.1574803149606300301, 0.9128937006798734100 ) ) ;
#22284 = EDGE_CURVE ( 'NONE', #27712, #32411, #18512, .T. ) ;
#22285 = LINE ( 'NONE', #45022, #16833 ) ;
#22286 = CARTESIAN_POINT ( 'NONE',  ( -1.002407869896990045, 0.1264236179284866091, 1.567421259788755794 ) ) ;
#22287 = CARTESIAN_POINT ( 'NONE',  ( -0.7185039370078746268, -0.06523048226347956391, 1.951279527451529772 ) ) ;
#22288 = EDGE_LOOP ( 'NONE', ( #31628, #23686, #28885, #15925 ) ) ;
#22289 = DIRECTION ( 'NONE',  ( 0.000000000000000000, 1.000000000000000000, 3.662381193212024518E-16 ) ) ;
#22290 = CARTESIAN_POINT ( 'NONE',  ( -0.9412147342319837628, 0.1574803149606300301, 1.552657480314961536 ) ) ;
#22291 = CARTESIAN_POINT ( 'NONE',  ( 0.8759842519685039353, 0.000000000000000000, 4.498031496062992574 ) ) ;
#22292 = CARTESIAN_POINT ( 'NONE',  ( 0.6971942568897648851, 0.07405724077823318263, 1.422244094434425898 ) ) ;
#22293 = CARTESIAN_POINT ( 'NONE',  ( -0.1400282309210590381, -0.09851383267563169899, 0.09116504983989133504 ) ) ;
#22294 = CARTESIAN_POINT ( 'NONE',  ( -0.2066929133858267931, -0.2714884749021748145, -1.284167712019358198 ) ) ;
#22295 = ORIENTED_EDGE ( 'NONE', *, *, #1614, .T. ) ;
#22296 = EDGE_CURVE ( 'NONE', #12706, #39516, #34150, .T. ) ;
#22297 = VECTOR ( 'NONE', #46771, 39.37007874015748854 ) ;
#22298 = ORIENTED_EDGE ( 'NONE', *, *, #19148, .F. ) ;
#22299 = ORIENTED_EDGE ( 'NONE', *, *, #40328, .F. ) ;
#22300 = AXIS2_PLACEMENT_3D ( 'NONE', #15741, #27001, #33725 ) ;
#22301 = AXIS2_PLACEMENT_3D ( 'NONE', #26302, #37775, #4928 ) ;
#22302 = CARTESIAN_POINT ( 'NONE',  ( 0.1264236179284866091, -0.9650590550643465271, -0.1264236179284866091 ) ) ;
#22303 = CARTESIAN_POINT ( 'NONE',  ( 0.1264236179284866091, -0.3843503936470239468, 0.1264236179284866091 ) ) ;
#22304 = CARTESIAN_POINT ( 'NONE',  ( 0.07405724077823318263, -0.9724409448281265966, 0.1787899950787401604 ) ) ;
#22305 = ORIENTED_EDGE ( 'NONE', *, *, #44446, .T. ) ;
#22306 = SURFACE_STYLE_USAGE ( .BOTH. , #26164 ) ;
#22307 = CARTESIAN_POINT ( 'NONE',  ( 3.301370929368692659E-17, -0.1880359355672976407, 0.1797182628040039365 ) ) ;
#22308 = DIRECTION ( 'NONE',  ( 0.000000000000000000, 0.000000000000000000, 1.000000000000000000 ) ) ;
#22309 = CARTESIAN_POINT ( 'NONE',  ( -0.1264236179284866091, -0.1284448818360001965, -0.1264236179284866091 ) ) ;
#22310 = CARTESIAN_POINT ( 'NONE',  ( 0.8759842519685039353, -0.1574803149606299191, 0.1476377951680635792 ) ) ;
#22311 = CARTESIAN_POINT ( 'NONE',  ( 1.054774247047244096, 0.000000000000000000, 0.7308070865604093802 ) ) ;
#22313 = CARTESIAN_POINT ( 'NONE',  ( 0.7646288533564489232, -0.1113553986120547346, 1.126968503829480328 ) ) ;
#22312 = CARTESIAN_POINT ( 'NONE',  ( -1.011560127499680828, 0.09259506503980204084, 0.03937007874015843734 ) ) ;
#22315 = CARTESIAN_POINT ( 'NONE',  ( 0.2642359194686346169, 1.205361022782824954E-17, -0.09842519685039370636 ) ) ;
#22314 = CARTESIAN_POINT ( 'NONE',  ( -0.1377952755905511584, -1.331775896911328393E-15, -0.9074803149606294195 ) ) ;
#22316 = CARTESIAN_POINT ( 'NONE',  ( 0.8107537697050254399, -0.1574803149606297803, 1.690452755905512916 ) ) ;
#22317 = CARTESIAN_POINT ( 'NONE',  ( 0.6971942568897637749, 2.189545951927499583E-17, 1.779035433017102319 ) ) ;
#22318 = DIRECTION ( 'NONE',  ( -1.000000000000000000, 0.000000000000000000, 0.000000000000000000 ) ) ;
#22319 = VERTEX_POINT ( 'NONE', #34612 ) ;
#22320 = VECTOR ( 'NONE', #35308, 39.37007874015748143 ) ;
#22321 = CARTESIAN_POINT ( 'NONE',  ( 0.7185039370078739607, 1.928577636452523993E-17, 1.318897637687747926 ) ) ;
#22323 = CARTESIAN_POINT ( 'NONE',  ( -0.1787899950787401604, -0.2834645668753703052, -0.07405724077823318263 ) ) ;
#22322 = CARTESIAN_POINT ( 'NONE',  ( 0.1113553986120547346, -0.9379921258767245362, -0.1113553986120547346 ) ) ;
#22324 = CARTESIAN_POINT ( 'NONE',  ( 0.7185039370078739607, 1.928577636452523993E-17, 0.06889763779527559306 ) ) ;
#22325 = CARTESIAN_POINT ( 'NONE',  ( -0.1787899950787401604, -1.061023621993481214, 0.07405724077823318263 ) ) ;
#22326 = CARTESIAN_POINT ( 'NONE',  ( 0.7495606340400177148, -0.1264236179284866091, 0.1697834645131657827 ) ) ;
#22327 = ( BOUNDED_CURVE ( )  B_SPLINE_CURVE ( 2, ( #7297, #29150, #14491, #15206, #44397, #36054, #10912, #40103, #3697 ),
 .UNSPECIFIED., .F., .F. ) 
 B_SPLINE_CURVE_WITH_KNOTS ( ( 3, 2, 2, 2, 3 ),
 ( 0.5999999999999999778, 0.6025000000000000355, 0.6049999999999999822, 0.6075000000000000400, 0.6099999999999999867 ),
 .UNSPECIFIED. ) 
 CURVE ( )  GEOMETRIC_REPRESENTATION_ITEM ( )  RATIONAL_B_SPLINE_CURVE ( ( 1.000000000000000000, 0.9238795325112869605, 1.000000000000000000, 0.9238795325112869605, 1.000000000000000000, 0.9238795325112869605, 1.000000000000000000, 0.9238795325112869605, 1.000000000000000000 ) ) 
 REPRESENTATION_ITEM ( '' )  ) ;
#22328 = CARTESIAN_POINT ( 'NONE',  ( 0.3551574803149606385, 2.613864355459500179E-17, 0.000000000000000000 ) ) ;
#22329 = CARTESIAN_POINT ( 'NONE',  ( -0.6971942568897648851, -0.07405724077823297447, 1.619094488135213838 ) ) ;
#22330 = VERTEX_POINT ( 'NONE', #20448 ) ;
#22331 = CARTESIAN_POINT ( 'NONE',  ( -1.002407869896990045, -0.1264236179284866091, 1.124507873961984261 ) ) ;
#22332 = CARTESIAN_POINT ( 'NONE',  ( 0.9500414927467378812, 0.1787899950787401604, 1.294291338528912982 ) ) ;
#22333 = CARTESIAN_POINT ( 'NONE',  ( 0.1574803149606300301, -1.216043306979087468, -0.06523048226347956391 ) ) ;
#22334 = AXIS2_PLACEMENT_3D ( 'NONE', #3542, #19074, #41100 ) ;
#22335 = CARTESIAN_POINT ( 'NONE',  ( 0.9500414927467378812, -0.1787899950787401604, 0.05905511805647267048 ) ) ;
#22336 = CARTESIAN_POINT ( 'NONE',  ( -0.6971942568897637749, 2.189545951927499583E-17, 1.065452755851747924 ) ) ;
#22337 = CARTESIAN_POINT ( 'NONE',  ( -0.6971942568897637749, -2.189545951927502049E-17, 1.990649606245448844 ) ) ;
#22338 = CARTESIAN_POINT ( 'NONE',  ( 0.4755220087074803481, -3.032960542342102697E-32, 0.09842519685039370636 ) ) ;
#22339 = CARTESIAN_POINT ( 'NONE',  ( 0.8019270111902716547, 0.1787899950787401604, 0.3937007873478114983 ) ) ;
#22340 = CARTESIAN_POINT ( 'NONE',  ( -0.9500414927467377701, -0.1787899950787401604, 0.2509842519147403861 ) ) ;
#22341 = CARTESIAN_POINT ( 'NONE',  ( -0.6971942568897637749, 2.189545951927499583E-17, 0.7898622046706456068 ) ) ;
#22342 = CARTESIAN_POINT ( 'NONE',  ( 0.9412147342319837628, -0.1574803149606297803, 1.724901574695621553 ) ) ;
#22343 = ORIENTED_EDGE ( 'NONE', *, *, #19902, .F. ) ;
#22344 = ADVANCED_FACE ( 'NONE', ( #27681 ), #35086, .T. ) ;
#22345 = DIRECTION ( 'NONE',  ( -1.000000000000000000, 0.000000000000000000, 0.000000000000000000 ) ) ;
#22346 = CARTESIAN_POINT ( 'NONE',  ( 0.7495606340400177148, -0.1264236179284866091, 0.8784448818360000022 ) ) ;
#22347 = CARTESIAN_POINT ( 'NONE',  ( 0.6971942568897637749, 2.189545951927499583E-17, 0.9916338582139527791 ) ) ;
#22348 = CARTESIAN_POINT ( 'NONE',  ( -0.6971942568897648851, 0.07405724077823318263, 1.850393700733638624 ) ) ;
#22349 = VERTEX_POINT ( 'NONE', #31495 ) ;
#22350 = EDGE_CURVE ( 'NONE', #1825, #18854, #9389, .T. ) ;
#22351 = ( BOUNDED_CURVE ( )  B_SPLINE_CURVE ( 2, ( #34389, #26737, #8493, #11874, #15237, #26262, #23126, #40824, #41527, #4407, #1529, #45383, #19036, #15475, #20927, #35568, #31275, #9461, #35335, #19987, #5856, #42708, #34627, #9926, #38908, #28385, #45853, #28148, #2245, #6304, #31745, #6069, #24533, #42006, #13744, #31043, #24079, #5368, #42953, #31975, #1776, #12829, #2476, #9210, #20693, #17102, #34870, #46331, #27923, #13515, #2713, #2017, #42486, #17340, #45611, #39133, #38687, #46559, #16416, #27460, #38445, #23831, #5614, #9693, #20221, #16865, #16645, #10161, #38206, #13061, #27698, #20463, #42262, #35098, #31508, #46090, #13294, #24307, #40304, #17572, #32461, #39832, #21400, #10640, #14939, #43192, #36025, #21888, #7270, #28635, #11113, #43432, #29601, #10882, #14697, #10404, #36509, #25733, #3664, #47040, #18287, #29371, #39604, #6781, #32929, #3186, #25006, #21649, #17814, #24770, #39367, #43911, #25245, #22106, #7487, #14232, #6548, #29120, #28874, #7024, #36282, #18519, #21160, #3433, #32212, #25502, #50, #35793, #18047, #32692, #36734, #46800, #47283, #14460, #3892, #33171, #293, #2935, #13984, #43671, #40070, #33402, #7722, #18744, #19450, #22339, #12286, #15409, #748, #37195, #16121, #36967, #41001, #25954, #4581, #519, #45071, #4827, #40533, #30510, #41465, #30743, #11341, #30056, #26438, #22813, #4120, #15886, #15177, #26905, #12051, #1461, #4339, #1232, #37427, #8663, #11573, #8189, #5071, #29820, #44366, #18972, #23299, #26200, #33634, #37916, #19216, #30289, #994, #19687, #40766, #7962, #34331, #8427, #22581, #44598, #11814, #33875, #15651, #44841, #26673, #41223, #23055, #37675, #34105, #9392, #12534, #9861, #1706, #16803, #42649, #24473, #35033, #17042, #27634, #1952, #5548, #35506, #17279, #45316, #16583, #27154, #12992, #2411, #41709, #13458, #34554, #41940, #8909, #31211, #45784, #23540, #9147, #2181, #28088, #38141, #6009, #42187, #39068, #5305, #19922, #6238, #16353, #30976, #31443, #45542, #24010, #12765, #20629, #38842, #27396, #31683, #38611, #20863, #23765, #5789, #38374, #2646, #20394, #20158, #34808, #46024, #13236, #27864, #42421, #9629, #24246, #46263, #29056, #14406, #35737, #32869, #17750, #22054, #17983, #21827, #17509, #43612, #23997, #40010, #6719, #32398, #36454, #13919, #28566, #7205, #43134, #32143, #28812, #2874, #31915, #42881, #14637, #46975, #29306, #11057, #21334, #10091, #3374, #35965, #43374, #24703, #21099, #10586, #39769, #40247, #6960, #7435, #21580, #39304, #32636, #47223, #7790, #15012, #37033, #22655, #43323, #33236, #10284, #4183, #363, #40833, #46676, #32341, #44432, #10525, #37260, #35908, #3063, #26022, #24892, #39491, #29888, #39715, #43079, #35687, #24659, #39253, #8026, #17692, #17928, #18810, #46922, #22407, #11648, #13867, #28755, #6427, #29666, #25123, #33467, #15242, #21521, #14111, #36158, #3312, #11404, #40597, #4412, #19042, #26270, #818, #15480, #12118, #23375, #5621, #8264, #26740, #19286, #41778, #8979, #16653, #41532, #5137, #23600, #41299, #34395, #8499, #38212, #31051, #20229, #22888, #11881, #1304, #15960, #19993, #37502, #39842, #22347, #28882, #33410, #36517, #21895, #10890, #37203, #10648, #14703, #47048, #25740, #7031, #18752, #29378, #3672, #40080, #22590, #4346, #32469, #18295, #57, #43918, #43443, #36973, #14241, #4128, #33179, #25253, #25510, #15184, #11123, #29830, #44373, #11581, #36290, #7969, #21658, #300, #3442, #7277, #26208, #40313, #40773, #18054, #14946, #32701, #47291, #14471, #29127, #32936, #43681, #7496, #36741, #3899, #18524, #44150, #11350, #30753, #45324, #15657, #12540, #8672, #41715, #30983, #37682, #26914, #4588, #8917, #41468, #5312, #45550, #34563, #38381, #4835, #12770, #12057, #26681, #19696, #19224, #33881, #1715, #34111, #22822, #26443, #18981, #33644, #41948, #37439, #12291, #37922, #9154, #41008, #19457, #8199, #23064, #15894, #23305, #45080, #5076, #34337, #24254, #45793, #20638, #38851, #9402, #6016, #35746, #32154, #24017, #35283, #39314, #17517, #35515, #46742, #34816, #38619, #12999, #6248, #2656, #43141, #2420, #17050, #17287, #27642, #13466, #2189, #31922, #24714, #21107, #13687, #46506, #28095, #28323, #42196, #1958, #5796, #42892, #16591, #6489, #9636, #42429, #31449, #10347, #31216, #31692, #20163, #46272, #20402, #2881, #10102, #35042, #13931, #28576, #24956, #5554, #9871, #39076, #20873, #16811, #46033, #27870, #11295, #43383, #22063, #3848, #36231, #36688, #29317, #18469, #36927, #10830, #4808, #25192, #18695, #21838, #22292, #32409, #47231, #25907, #25445, #4079, #3384, #17992, #40256, #39778, #6970, #44101, #7214, #10594, #3132, #44325, #11528, #33356, #33120, #477, #245, #14416, #14888, #15131, #46984, #43623, #39554, #43864, #36461, #29550, #29776, #3618, #14178, #18235, #32879, #21594, #14645, #6727, #21345, #11066, #32646, #29065, #25684, #7443, #35973, #17760, #28821, #18931, #26866, #37877, #30943, #12009, #41182, #5030, #33590, #1190, #22770, #19652, #16080, #34296, #37150, #26148, #948, #8146, #703, #22532, #15361, #1421, #4298, #27117, #30245, #15607, #4534, #45504, #30011, #8385, #40718, #19411, #15849, #45271, #23014, #44796, #26630, #44557, #11775, #26393, #37627, #4785, #30472, #40956, #30705, #37379, #12491, #41427, #19171, #45028, #41664, #12243, #8624, #23502, #38104, #5268, #19886, #1667, #27830, #12728, #38334, #20121, #31173, #31410, #23730, #34998, #42390, #23973, #45986, #27594, #45746, #16546, #24209, #42144, #9352, #2143, #27358, #38576, #13194, #41901, #9110, #5745, #20359, #5507, #16769, #34768, #1910, #4694, #12400, #23636, #857, #16225, #15516, #26777, #22687, #12869, #1817, #37291, #11918, #27021, #41101, #34208, #4442, #30857, #1573, #22922, #27261, #37784, #38247, #37535, #41336, #44700, #4936, #5408, #26541, #15758, #41813, #8535, #20029, #19326, #33975, #8775, #8295, #1101, #12637, #23167, #30392, #19076, #27502, #33748, #34670, #44941, #9014, #34427, #12153, #5175, #16454, #19562, #1336, #15992, #45179, #30615, #38014, #45420, #41570, #23410, #19793, #31087, #45651, #13332, #24808, #21202, #46371, #20505, #16915, #9499, #38944, #35836, #38485, #13107, #34912, #42747, #39175, #32260, #27961, #9730, #6348, #2055, #2518, #38725, #20962, #13783, #35608, #5655, #42053, #31554, #24120, #16688, #27738, #5893, #2749, #35142, #42994, #46132, #42528, #24347 ),
 .UNSPECIFIED., .F., .T. ) 
 B_SPLINE_CURVE_WITH_KNOTS ( ( 3, 2, 2, 2, 2, 2, 2, 2, 2, 2, 2, 2, 2, 2, 2, 2, 2, 2, 2, 2, 2, 2, 2, 2, 2, 2, 2, 2, 2, 2, 2, 2, 2, 2, 2, 2, 2, 2, 2, 2, 2, 2, 2, 2, 2, 2, 2, 2, 2, 2, 2, 2, 2, 2, 2, 2, 2, 2, 2, 2, 2, 2, 2, 2, 2, 2, 2, 2, 2, 2, 2, 2, 2, 2, 2, 2, 2, 2, 2, 2, 2, 2, 2, 2, 2, 2, 2, 2, 2, 2, 2, 2, 2, 2, 2, 2, 2, 2, 2, 2, 2, 2, 2, 2, 2, 2, 2, 2, 2, 2, 2, 2, 2, 2, 2, 2, 2, 2, 2, 2, 2, 2, 2, 2, 2, 2, 2, 2, 2, 2, 2, 2, 2, 2, 2, 2, 2, 2, 2, 2, 2, 2, 2, 2, 2, 2, 2, 2, 2, 2, 2, 2, 2, 2, 2, 2, 2, 2, 2, 2, 2, 2, 2, 2, 2, 2, 2, 2, 2, 2, 2, 2, 2, 2, 2, 2, 2, 2, 2, 2, 2, 2, 2, 2, 2, 2, 2, 2, 2, 2, 2, 2, 2, 2, 2, 2, 2, 2, 2, 2, 2, 2, 2, 2, 2, 2, 2, 2, 2, 2, 2, 2, 2, 2, 2, 2, 2, 2, 2, 2, 2, 2, 2, 2, 2, 2, 2, 2, 2, 2, 2, 2, 2, 2, 2, 2, 2, 2, 2, 2, 2, 2, 2, 2, 2, 2, 2, 2, 2, 2, 2, 2, 2, 2, 2, 2, 2, 2, 2, 2, 2, 2, 2, 2, 2, 2, 2, 2, 2, 2, 2, 2, 2, 2, 2, 2, 2, 2, 2, 2, 2, 2, 2, 2, 2, 2, 2, 2, 2, 2, 2, 2, 2, 2, 2, 2, 2, 2, 2, 2, 2, 2, 2, 2, 2, 2, 2, 2, 2, 2, 2, 2, 2, 2, 2, 2, 2, 2, 2, 2, 2, 2, 2, 2, 2, 2, 2, 2, 2, 2, 2, 2, 2, 2, 2, 2, 2, 2, 2, 2, 2, 2, 2, 2, 2, 2, 2, 2, 2, 2, 2, 2, 2, 2, 2, 2, 2, 2, 2, 2, 2, 2, 2, 2, 2, 2, 2, 2, 2, 2, 2, 2, 2, 2, 2, 2, 2, 2, 2, 2, 2, 2, 2, 2, 2, 2, 2, 2, 2, 2, 2, 2, 2, 2, 2, 2, 2, 3 ),
 ( 0.006249999973727609834, 0.007499999999999999722, 0.01000000000000000021, 0.01250000000000000069, 0.01499999999999999944, 0.01750000000000000167, 0.02000000000000000042, 0.02249999999999999917, 0.02500000000000000139, 0.02750000000000000361, 0.02999999999999999889, 0.03249999999999999417, 0.03500000000000000333, 0.03749999999999999861, 0.04000000000000000083, 0.04250000000000000305, 0.04499999999999999833, 0.04750000000000000056, 0.05000000000000000278, 0.05249999999999999806, 0.05500000000000000028, 0.05750000000000000250, 0.05999999999999999778, 0.06250000000000000000, 0.06500000000000000222, 0.06750000000000000444, 0.07000000000000000666, 0.07249999999999999500, 0.07500000000000001110, 0.07749999999999999944, 0.08000000000000000167, 0.08250000000000000389, 0.08500000000000000611, 0.08749999999999999445, 0.08999999999999999667, 0.09249999999999999889, 0.09500000000000000111, 0.09750000000000000333, 0.1000000000000000056, 0.1024999999999999939, 0.1049999999999999961, 0.1074999999999999983, 0.1100000000000000006, 0.1125000000000000028, 0.1150000000000000050, 0.1174999999999999933, 0.1199999999999999956, 0.1224999999999999978, 0.1250000000000000000, 0.1275000000000000022, 0.1300000000000000044, 0.1325000000000000067, 0.1350000000000000089, 0.1374999999999999833, 0.1400000000000000133, 0.1424999999999999878, 0.1449999999999999900, 0.1474999999999999922, 0.1499999999999999944, 0.1524999999999999967, 0.1549999999999999989, 0.1575000000000000011, 0.1600000000000000033, 0.1625000000000000056, 0.1650000000000000078, 0.1675000000000000100, 0.1700000000000000122, 0.1724999999999999867, 0.1749999999999999889, 0.1774999999999999911, 0.1799999999999999933, 0.1824999999999999956, 0.1849999999999999978, 0.1875000000000000000, 0.1900000000000000022, 0.1925000000000000044, 0.1950000000000000067, 0.1975000000000000089, 0.2000000000000000111, 0.2025000000000000133, 0.2049999999999999878, 0.2074999999999999900, 0.2099999999999999922, 0.2124999999999999944, 0.2149999999999999967, 0.2174999999999999989, 0.2200000000000000011, 0.2225000000000000033, 0.2250000000000000056, 0.2275000000000000078, 0.2300000000000000100, 0.2325000000000000122, 0.2349999999999999867, 0.2374999999999999889, 0.2399999999999999911, 0.2424999999999999933, 0.2449999999999999956, 0.2474999999999999978, 0.2500000000000000000, 0.2525000000000000022, 0.2550000000000000044, 0.2575000000000000067, 0.2600000000000000089, 0.2625000000000000111, 0.2650000000000000133, 0.2675000000000000155, 0.2700000000000000178, 0.2725000000000000200, 0.2750000000000000222, 0.2775000000000000244, 0.2800000000000000266, 0.2824999999999999734, 0.2849999999999999756, 0.2874999999999999778, 0.2899999999999999800, 0.2924999999999999822, 0.2949999999999999845, 0.2974999999999999867, 0.2999999999999999889, 0.3024999999999999911, 0.3049999999999999933, 0.3074999999999999956, 0.3099999999999999978, 0.3125000000000000000, 0.3150000000000000022, 0.3175000000000000044, 0.3200000000000000067, 0.3225000000000000089, 0.3250000000000000111, 0.3275000000000000133, 0.3300000000000000155, 0.3325000000000000178, 0.3350000000000000200, 0.3375000000000000222, 0.3400000000000000244, 0.3425000000000000266, 0.3449999999999999734, 0.3474999999999999756, 0.3499999999999999778, 0.3524999999999999800, 0.3549999999999999822, 0.3574999999999999845, 0.3599999999999999867, 0.3624999999999999889, 0.3649999999999999911, 0.3674999999999999933, 0.3699999999999999956, 0.3724999999999999978, 0.3750000000000000000, 0.3775000000000000022, 0.3800000000000000044, 0.3825000000000000067, 0.3850000000000000089, 0.3875000000000000111, 0.3900000000000000133, 0.3925000000000000155, 0.3950000000000000178, 0.3975000000000000200, 0.4000000000000000222, 0.4025000000000000244, 0.4050000000000000266, 0.4074999999999999734, 0.4099999999999999756, 0.4124999999999999778, 0.4149999999999999800, 0.4174999999999999822, 0.4199999999999999845, 0.4224999999999999867, 0.4249999999999999889, 0.4274999999999999911, 0.4299999999999999933, 0.4324999999999999956, 0.4349999999999999978, 0.4375000000000000000, 0.4400000000000000022, 0.4425000000000000044, 0.4450000000000000067, 0.4475000000000000089, 0.4500000000000000111, 0.4525000000000000133, 0.4550000000000000155, 0.4575000000000000178, 0.4600000000000000200, 0.4625000000000000222, 0.4650000000000000244, 0.4675000000000000266, 0.4699999999999999734, 0.4724999999999999756, 0.4749999999999999778, 0.4774999999999999800, 0.4799999999999999822, 0.4824999999999999845, 0.4849999999999999867, 0.4874999999999999889, 0.4899999999999999911, 0.4924999999999999933, 0.4949999999999999956, 0.4974999999999999978, 0.5000000000000000000, 0.5024999999999999467, 0.5050000000000000044, 0.5074999999999999512, 0.5100000000000000089, 0.5124999999999999556, 0.5150000000000000133, 0.5174999999999999600, 0.5200000000000000178, 0.5224999999999999645, 0.5250000000000000222, 0.5274999999999999689, 0.5300000000000000266, 0.5324999999999999734, 0.5350000000000000311, 0.5374999999999999778, 0.5400000000000000355, 0.5424999999999999822, 0.5450000000000000400, 0.5474999999999999867, 0.5500000000000000444, 0.5524999999999999911, 0.5550000000000000488, 0.5574999999999999956, 0.5600000000000000533, 0.5625000000000000000, 0.5649999999999999467, 0.5675000000000000044, 0.5699999999999999512, 0.5725000000000000089, 0.5749999999999999556, 0.5775000000000000133, 0.5799999999999999600, 0.5825000000000000178, 0.5849999999999999645, 0.5875000000000000222, 0.5899999999999999689, 0.5925000000000000266, 0.5949999999999999734, 0.5975000000000000311, 0.5999999999999999778, 0.6025000000000000355, 0.6049999999999999822, 0.6075000000000000400, 0.6099999999999999867, 0.6125000000000000444, 0.6149999999999999911, 0.6175000000000000488, 0.6199999999999999956, 0.6225000000000000533, 0.6250000000000000000, 0.6274999999999999467, 0.6300000000000000044, 0.6324999999999999512, 0.6350000000000000089, 0.6374999999999999556, 0.6400000000000000133, 0.6424999999999999600, 0.6450000000000000178, 0.6474999999999999645, 0.6500000000000000222, 0.6524999999999999689, 0.6550000000000000266, 0.6574999999999999734, 0.6600000000000000311, 0.6624999999999999778, 0.6650000000000000355, 0.6674999999999999822, 0.6700000000000000400, 0.6724999999999999867, 0.6750000000000000444, 0.6774999999999999911, 0.6800000000000000488, 0.6824999999999999956, 0.6850000000000000533, 0.6875000000000000000, 0.6899999999999999467, 0.6925000000000000044, 0.6949999999999999512, 0.6975000000000000089, 0.6999999999999999556, 0.7025000000000000133, 0.7049999999999999600, 0.7075000000000000178, 0.7099999999999999645, 0.7125000000000000222, 0.7149999999999999689, 0.7175000000000000266, 0.7199999999999999734, 0.7225000000000000311, 0.7249999999999999778, 0.7275000000000000355, 0.7299999999999999822, 0.7325000000000000400, 0.7349999999999999867, 0.7375000000000000444, 0.7399999999999999911, 0.7425000000000000488, 0.7449999999999999956, 0.7475000000000000533, 0.7500000000000000000, 0.7524999999999999467, 0.7550000000000000044, 0.7574999999999999512, 0.7600000000000000089, 0.7624999999999999556, 0.7650000000000000133, 0.7674999999999999600, 0.7700000000000000178, 0.7724999999999999645, 0.7750000000000000222, 0.7774999999999999689, 0.7799999999999999156, 0.7824999999999999734, 0.7850000000000000311, 0.7874999999999999778, 0.7900000000000000355, 0.7924999999999999822, 0.7950000000000000400, 0.7975000000000000977, 0.8000000000000000444, 0.8024999999999999911, 0.8050000000000000488, 0.8074999999999999956, 0.8100000000000000533, 0.8125000000000000000, 0.8150000000000000577, 0.8175000000000000044, 0.8199999999999999512, 0.8225000000000000089, 0.8249999999999999556, 0.8275000000000000133, 0.8299999999999999600, 0.8325000000000000178, 0.8349999999999999645, 0.8375000000000000222, 0.8399999999999999689, 0.8425000000000000266, 0.8449999999999999734, 0.8475000000000000311, 0.8499999999999999778, 0.8525000000000000355, 0.8549999999999999822, 0.8575000000000000400, 0.8599999999999999867, 0.8625000000000000444, 0.8649999999999999911, 0.8675000000000000488, 0.8699999999999999956, 0.8725000000000000533, 0.8750000000000000000, 0.8774999999999999467, 0.8800000000000000044, 0.8824999999999999512, 0.8850000000000000089, 0.8874999999999999556, 0.8900000000000000133, 0.8924999999999999600, 0.8950000000000000178, 0.8974999999999999645, 0.9000000000000000222, 0.9024999999999999689, 0.9050000000000000266, 0.9074999999999999734, 0.9100000000000000311, 0.9124999999999999778, 0.9150000000000000355, 0.9174999999999999822, 0.9200000000000000400, 0.9224999999999999867, 0.9250000000000000444, 0.9274999999999999911, 0.9300000000000000488, 0.9324999999999999956, 0.9350000000000000533, 0.9375000000000000000, 0.9399999999999999467, 0.9425000000000000044, 0.9449999999999999512, 0.9475000000000000089, 0.9499999999999999556, 0.9525000000000000133, 0.9549999999999999600, 0.9575000000000000178, 0.9599999999999999645, 0.9625000000000000222, 0.9649999999999999689, 0.9675000000000000266, 0.9699999999999999734, 0.9725000000000000311, 0.9749999999999999778, 0.9775000000000000355, 0.9799999999999999822, 0.9825000000000000400, 0.9849999999999999867, 0.9875000000000000444, 0.9899999999999999911, 0.9925000000000000488, 0.9949999999999999956, 0.9975000000000000533 ),
 .UNSPECIFIED. ) 
 CURVE ( )  GEOMETRIC_REPRESENTATION_ITEM ( )  RATIONAL_B_SPLINE_CURVE ( ( 0.9619397662556429252, 0.9619397654556960386, 1.000000000000000000, 0.9238795325112869605, 1.000000000000000000, 0.9238795325112869605, 1.000000000000000000, 0.9238795325112869605, 1.000000000000000000, 0.9238795325112869605, 1.000000000000000000, 0.9238795325112869605, 1.000000000000000000, 0.9238795325112869605, 1.000000000000000000, 0.9238795325112869605, 1.000000000000000000, 0.9238795325112869605, 1.000000000000000000, 0.9238795325112869605, 1.000000000000000000, 0.9238795325112869605, 1.000000000000000000, 0.9238795325112869605, 1.000000000000000000, 0.9238795325112869605, 1.000000000000000000, 0.9238795325112869605, 1.000000000000000000, 0.9238795325112869605, 1.000000000000000000, 0.9238795325112869605, 1.000000000000000000, 0.9238795325112869605, 1.000000000000000000, 0.9238795325112869605, 1.000000000000000000, 0.9238795325112869605, 1.000000000000000000, 0.9238795325112869605, 1.000000000000000000, 0.9238795325112869605, 1.000000000000000000, 0.9238795325112869605, 1.000000000000000000, 0.9238795325112869605, 1.000000000000000000, 0.9238795325112869605, 1.000000000000000000, 0.9238795325112869605, 1.000000000000000000, 0.9238795325112869605, 1.000000000000000000, 0.9238795325112869605, 1.000000000000000000, 0.9238795325112869605, 1.000000000000000000, 0.9238795325112869605, 1.000000000000000000, 0.9238795325112869605, 1.000000000000000000, 0.9238795325112869605, 1.000000000000000000, 0.9238795325112869605, 1.000000000000000000, 0.9238795325112869605, 1.000000000000000000, 0.9238795325112869605, 1.000000000000000000, 0.9238795325112869605, 1.000000000000000000, 0.9238795325112869605, 1.000000000000000000, 0.9238795325112869605, 1.000000000000000000, 0.9238795325112869605, 1.000000000000000000, 0.9238795325112869605, 1.000000000000000000, 0.9238795325112869605, 1.000000000000000000, 0.9238795325112869605, 1.000000000000000000, 0.9238795325112869605, 1.000000000000000000, 0.9238795325112869605, 1.000000000000000000, 0.9238795325112869605, 1.000000000000000000, 0.9238795325112869605, 1.000000000000000000, 0.9238795325112869605, 1.000000000000000000, 0.9238795325112869605, 1.000000000000000000, 0.9238795325112869605, 1.000000000000000000, 0.9238795325112869605, 1.000000000000000000, 0.9238795325112869605, 1.000000000000000000, 0.9238795325112869605, 1.000000000000000000, 0.9238795325112869605, 1.000000000000000000, 0.9238795325112869605, 1.000000000000000000, 0.9238795325112869605, 1.000000000000000000, 0.9238795325112869605, 1.000000000000000000, 0.9238795325112869605, 1.000000000000000000, 0.9238795325112869605, 1.000000000000000000, 0.9238795325112869605, 1.000000000000000000, 0.9238795325112869605, 1.000000000000000000, 0.9238795325112869605, 1.000000000000000000, 0.9238795325112869605, 1.000000000000000000, 0.9238795325112869605, 1.000000000000000000, 0.9238795325112869605, 1.000000000000000000, 0.9238795325112869605, 1.000000000000000000, 0.9238795325112869605, 1.000000000000000000, 0.9238795325112869605, 1.000000000000000000, 0.9238795325112869605, 1.000000000000000000, 0.9238795325112869605, 1.000000000000000000, 0.9238795325112869605, 1.000000000000000000, 0.9238795325112869605, 1.000000000000000000, 0.9238795325112869605, 1.000000000000000000, 0.9238795325112869605, 1.000000000000000000, 0.9238795325112869605, 1.000000000000000000, 0.9238795325112869605, 1.000000000000000000, 0.9238795325112869605, 1.000000000000000000, 0.9238795325112869605, 1.000000000000000000, 0.9238795325112869605, 1.000000000000000000, 0.9238795325112869605, 1.000000000000000000, 0.9238795325112869605, 1.000000000000000000, 0.9238795325112869605, 1.000000000000000000, 0.9238795325112869605, 1.000000000000000000, 0.9238795325112869605, 1.000000000000000000, 0.9238795325112869605, 1.000000000000000000, 0.9238795325112869605, 1.000000000000000000, 0.9238795325112869605, 1.000000000000000000, 0.9238795325112869605, 1.000000000000000000, 0.9238795325112869605, 1.000000000000000000, 0.9238795325112869605, 1.000000000000000000, 0.9238795325112869605, 1.000000000000000000, 0.9238795325112869605, 1.000000000000000000, 0.9238795325112869605, 1.000000000000000000, 0.9238795325112869605, 1.000000000000000000, 0.9238795325112869605, 1.000000000000000000, 0.9238795325112869605, 1.000000000000000000, 0.9238795325112869605, 1.000000000000000000, 0.9238795325112869605, 1.000000000000000000, 0.9238795325112869605, 1.000000000000000000, 0.9238795325112869605, 1.000000000000000000, 0.9238795325112869605, 1.000000000000000000, 0.9238795325112869605, 1.000000000000000000, 0.9238795325112869605, 1.000000000000000000, 0.9238795325112869605, 1.000000000000000000, 0.9238795325112869605, 1.000000000000000000, 0.9238795325112869605, 1.000000000000000000, 0.9238795325112869605, 1.000000000000000000, 0.9238795325112869605, 1.000000000000000000, 0.9238795325112869605, 1.000000000000000000, 0.9238795325112869605, 1.000000000000000000, 0.9238795325112869605, 1.000000000000000000, 0.9238795325112869605, 1.000000000000000000, 0.9238795325112869605, 1.000000000000000000, 0.9238795325112869605, 1.000000000000000000, 0.9238795325112869605, 1.000000000000000000, 0.9238795325112869605, 1.000000000000000000, 0.9238795325112869605, 1.000000000000000000, 0.9238795325112869605, 1.000000000000000000, 0.9238795325112869605, 1.000000000000000000, 0.9238795325112869605, 1.000000000000000000, 0.9238795325112869605, 1.000000000000000000, 0.9238795325112869605, 1.000000000000000000, 0.9238795325112869605, 1.000000000000000000, 0.9238795325112869605, 1.000000000000000000, 0.9238795325112869605, 1.000000000000000000, 0.9238795325112869605, 1.000000000000000000, 0.9238795325112869605, 1.000000000000000000, 0.9238795325112869605, 1.000000000000000000, 0.9238795325112869605, 1.000000000000000000, 0.9238795325112869605, 1.000000000000000000, 0.9238795325112869605, 1.000000000000000000, 0.9238795325112869605, 1.000000000000000000, 0.9238795325112869605, 1.000000000000000000, 0.9238795325112869605, 1.000000000000000000, 0.9238795325112869605, 1.000000000000000000, 0.9238795325112869605, 1.000000000000000000, 0.9238795325112869605, 1.000000000000000000, 0.9238795325112869605, 1.000000000000000000, 0.9238795325112869605, 1.000000000000000000, 0.9238795325112869605, 1.000000000000000000, 0.9238795325112869605, 1.000000000000000000, 0.9238795325112869605, 1.000000000000000000, 0.9238795325112869605, 1.000000000000000000, 0.9238795325112869605, 1.000000000000000000, 0.9238795325112869605, 1.000000000000000000, 0.9238795325112869605, 1.000000000000000000, 0.9238795325112869605, 1.000000000000000000, 0.9238795325112869605, 1.000000000000000000, 0.9238795325112869605, 1.000000000000000000, 0.9238795325112869605, 1.000000000000000000, 0.9238795325112869605, 1.000000000000000000, 0.9238795325112869605, 1.000000000000000000, 0.9238795325112869605, 1.000000000000000000, 0.9238795325112869605, 1.000000000000000000, 0.9238795325112869605, 1.000000000000000000, 0.9238795325112869605, 1.000000000000000000, 0.9238795325112869605, 1.000000000000000000, 0.9238795325112869605, 1.000000000000000000, 0.9238795325112869605, 1.000000000000000000, 0.9238795325112869605, 1.000000000000000000, 0.9238795325112869605, 1.000000000000000000, 0.9238795325112869605, 1.000000000000000000, 0.9238795325112869605, 1.000000000000000000, 0.9238795325112869605, 1.000000000000000000, 0.9238795325112869605, 1.000000000000000000, 0.9238795325112869605, 1.000000000000000000, 0.9238795325112869605, 1.000000000000000000, 0.9238795325112869605, 1.000000000000000000, 0.9238795325112869605, 1.000000000000000000, 0.9238795325112869605, 1.000000000000000000, 0.9238795325112869605, 1.000000000000000000, 0.9238795325112869605, 1.000000000000000000, 0.9238795325112869605, 1.000000000000000000, 0.9238795325112869605, 1.000000000000000000, 0.9238795325112869605, 1.000000000000000000, 0.9238795325112869605, 1.000000000000000000, 0.9238795325112869605, 1.000000000000000000, 0.9238795325112869605, 1.000000000000000000, 0.9238795325112869605, 1.000000000000000000, 0.9238795325112869605, 1.000000000000000000, 0.9238795325112869605, 1.000000000000000000, 0.9238795325112869605, 1.000000000000000000, 0.9238795325112869605, 1.000000000000000000, 0.9238795325112869605, 1.000000000000000000, 0.9238795325112869605, 1.000000000000000000, 0.9238795325112869605, 1.000000000000000000, 0.9238795325112869605, 1.000000000000000000, 0.9238795325112869605, 1.000000000000000000, 0.9238795325112869605, 1.000000000000000000, 0.9238795325112869605, 1.000000000000000000, 0.9238795325112869605, 1.000000000000000000, 0.9238795325112869605, 1.000000000000000000, 0.9238795325112869605, 1.000000000000000000, 0.9238795325112869605, 1.000000000000000000, 0.9238795325112869605, 1.000000000000000000, 0.9238795325112869605, 1.000000000000000000, 0.9238795325112869605, 1.000000000000000000, 0.9238795325112869605, 1.000000000000000000, 0.9238795325112869605, 1.000000000000000000, 0.9238795325112869605, 1.000000000000000000, 0.9238795325112869605, 1.000000000000000000, 0.9238795325112869605, 1.000000000000000000, 0.9238795325112869605, 1.000000000000000000, 0.9238795325112869605, 1.000000000000000000, 0.9238795325112869605, 1.000000000000000000, 0.9238795325112869605, 1.000000000000000000, 0.9238795325112869605, 1.000000000000000000, 0.9238795325112869605, 1.000000000000000000, 0.9238795325112869605, 1.000000000000000000, 0.9238795325112869605, 1.000000000000000000, 0.9238795325112869605, 1.000000000000000000, 0.9238795325112869605, 1.000000000000000000, 0.9238795325112869605, 1.000000000000000000, 0.9238795325112869605, 1.000000000000000000, 0.9238795325112869605, 1.000000000000000000, 0.9238795325112869605, 1.000000000000000000, 0.9238795325112869605, 1.000000000000000000, 0.9238795325112869605, 1.000000000000000000, 0.9238795325112869605, 1.000000000000000000, 0.9238795325112869605, 1.000000000000000000, 0.9238795325112869605, 1.000000000000000000, 0.9238795325112869605, 1.000000000000000000, 0.9238795325112869605, 1.000000000000000000, 0.9238795325112869605, 1.000000000000000000, 0.9238795325112869605, 1.000000000000000000, 0.9238795325112869605, 1.000000000000000000, 0.9238795325112869605, 1.000000000000000000, 0.9238795325112869605, 1.000000000000000000, 0.9238795325112869605, 1.000000000000000000, 0.9238795325112869605, 1.000000000000000000, 0.9238795325112869605, 1.000000000000000000, 0.9238795325112869605, 1.000000000000000000, 0.9238795325112869605, 1.000000000000000000, 0.9238795325112869605, 1.000000000000000000, 0.9238795325112869605, 1.000000000000000000, 0.9238795325112869605, 1.000000000000000000, 0.9238795325112869605, 1.000000000000000000, 0.9238795325112869605, 1.000000000000000000, 0.9238795325112869605, 1.000000000000000000, 0.9238795325112869605, 1.000000000000000000, 0.9238795325112869605, 1.000000000000000000, 0.9238795325112869605, 1.000000000000000000, 0.9238795325112869605, 1.000000000000000000, 0.9238795325112869605, 1.000000000000000000, 0.9238795325112869605, 1.000000000000000000, 0.9238795325112869605, 1.000000000000000000, 0.9238795325112869605, 1.000000000000000000, 0.9238795325112869605, 1.000000000000000000, 0.9238795325112869605, 1.000000000000000000, 0.9238795325112869605, 1.000000000000000000, 0.9238795325112869605, 1.000000000000000000, 0.9238795325112869605, 1.000000000000000000, 0.9238795325112869605, 1.000000000000000000, 0.9238795325112869605, 1.000000000000000000, 0.9238795325112869605, 1.000000000000000000, 0.9238795325112869605, 1.000000000000000000, 0.9238795325112869605, 1.000000000000000000, 0.9238795325112869605, 1.000000000000000000, 0.9238795325112869605, 1.000000000000000000, 0.9238795325112869605, 1.000000000000000000, 0.9238795325112869605, 1.000000000000000000, 0.9238795325112869605, 1.000000000000000000, 0.9238795325112869605, 1.000000000000000000, 0.9238795325112869605, 1.000000000000000000, 0.9238795325112869605, 1.000000000000000000, 0.9238795325112869605, 1.000000000000000000, 0.9238795325112869605, 1.000000000000000000, 0.9238795325112869605, 1.000000000000000000, 0.9238795325112869605, 1.000000000000000000, 0.9238795325112869605, 1.000000000000000000, 0.9238795325112869605, 1.000000000000000000, 0.9238795325112869605, 1.000000000000000000, 0.9238795325112869605, 1.000000000000000000, 0.9238795325112869605, 1.000000000000000000, 0.9238795325112869605, 1.000000000000000000, 0.9238795325112869605, 1.000000000000000000, 0.9238795325112869605, 1.000000000000000000, 0.9238795325112869605, 1.000000000000000000, 0.9238795325112869605, 1.000000000000000000, 0.9238795325112869605, 1.000000000000000000, 0.9238795325112869605, 1.000000000000000000, 0.9238795325112869605, 1.000000000000000000, 0.9238795325112869605, 1.000000000000000000, 0.9238795325112869605, 1.000000000000000000, 0.9238795325112869605, 1.000000000000000000, 0.9238795325112869605, 1.000000000000000000, 0.9238795325112869605, 1.000000000000000000, 0.9238795325112869605, 1.000000000000000000, 0.9238795325112869605, 1.000000000000000000, 0.9238795325112869605, 1.000000000000000000, 0.9238795325112869605, 1.000000000000000000, 0.9238795325112869605, 1.000000000000000000, 0.9238795325112869605, 1.000000000000000000, 0.9238795325112869605, 1.000000000000000000, 0.9238795325112869605, 1.000000000000000000, 0.9238795325112869605, 1.000000000000000000, 0.9238795325112869605, 1.000000000000000000, 0.9238795325112869605, 1.000000000000000000, 0.9238795325112869605, 1.000000000000000000, 0.9238795325112869605, 1.000000000000000000, 0.9238795325112869605, 1.000000000000000000, 0.9238795325112869605, 1.000000000000000000, 0.9238795325112869605, 1.000000000000000000, 0.9238795325112869605, 1.000000000000000000, 0.9238795325112869605, 1.000000000000000000, 0.9238795325112869605, 1.000000000000000000, 0.9238795325112869605, 1.000000000000000000, 0.9238795325112869605, 1.000000000000000000, 0.9238795325112869605, 1.000000000000000000, 0.9238795325112869605, 1.000000000000000000, 0.9238795325112869605, 1.000000000000000000, 0.9238795325112869605, 1.000000000000000000, 0.9238795325112869605, 1.000000000000000000, 0.9238795325112869605, 1.000000000000000000, 0.9238795325112869605, 1.000000000000000000, 0.9238795325112869605, 1.000000000000000000, 0.9238795325112869605, 1.000000000000000000, 0.9238795325112869605, 1.000000000000000000, 0.9238795325112869605, 1.000000000000000000, 0.9238795325112869605, 1.000000000000000000, 0.9238795325112869605, 1.000000000000000000, 0.9238795325112869605, 1.000000000000000000, 0.9238795325112869605, 1.000000000000000000, 0.9238795325112869605, 1.000000000000000000, 0.9238795325112869605, 1.000000000000000000, 0.9238795325112869605, 1.000000000000000000, 0.9238795325112869605, 1.000000000000000000, 0.9238795325112869605, 1.000000000000000000, 0.9238795325112869605, 1.000000000000000000, 0.9238795325112869605, 1.000000000000000000, 0.9238795325112869605, 1.000000000000000000, 0.9238795325112869605, 1.000000000000000000, 0.9238795325112869605, 1.000000000000000000, 0.9238795325112869605, 1.000000000000000000, 0.9238795325112869605, 1.000000000000000000, 0.9238795325112869605, 1.000000000000000000, 0.9238795325112869605, 1.000000000000000000, 0.9238795325112869605, 1.000000000000000000, 0.9238795325112869605, 1.000000000000000000, 0.9238795325112869605, 1.000000000000000000, 0.9238795325112869605, 1.000000000000000000, 0.9238795325112869605, 1.000000000000000000, 0.9238795325112869605, 1.000000000000000000, 0.9238795325112869605, 1.000000000000000000, 0.9238795325112869605, 1.000000000000000000, 0.9238795325112869605, 1.000000000000000000, 0.9238795325112869605, 1.000000000000000000, 0.9238795325112869605, 1.000000000000000000, 0.9238795325112869605, 1.000000000000000000, 0.9238795325112869605, 1.000000000000000000, 0.9238795325112869605, 1.000000000000000000, 0.9238795325112869605, 1.000000000000000000, 0.9238795325112869605, 1.000000000000000000, 0.9238795325112869605, 1.000000000000000000, 0.9238795325112869605, 1.000000000000000000, 0.9238795325112869605, 1.000000000000000000, 0.9238795325112869605, 1.000000000000000000, 0.9238795325112869605, 1.000000000000000000, 0.9238795325112869605, 1.000000000000000000, 0.9238795325112869605, 1.000000000000000000, 0.9238795325112869605, 1.000000000000000000, 0.9238795325112869605, 1.000000000000000000, 0.9238795325112869605, 1.000000000000000000, 0.9238795325112869605, 1.000000000000000000, 0.9238795325112869605, 1.000000000000000000, 0.9238795325112869605, 1.000000000000000000, 0.9238795325112869605, 1.000000000000000000, 0.9238795325112869605, 1.000000000000000000, 0.9238795325112869605, 1.000000000000000000, 0.9238795325112869605, 1.000000000000000000, 0.9238795325112869605, 1.000000000000000000, 0.9238795325112869605, 1.000000000000000000, 0.9238795325112869605, 1.000000000000000000, 0.9238795325112869605, 1.000000000000000000, 0.9238795325112869605, 1.000000000000000000, 0.9238795325112869605, 1.000000000000000000, 0.9238795325112869605, 1.000000000000000000, 0.9238795325112869605, 1.000000000000000000, 0.9238795325112869605, 1.000000000000000000, 0.9238795325112869605, 1.000000000000000000, 0.9238795325112869605, 1.000000000000000000, 0.9238795325112869605, 1.000000000000000000, 0.9238795325112869605, 1.000000000000000000, 0.9238795325112869605, 1.000000000000000000, 0.9238795325112869605, 1.000000000000000000, 0.9238795325112869605, 1.000000000000000000, 0.9238795325112869605, 1.000000000000000000, 0.9238795325112869605, 1.000000000000000000, 0.9238795325112869605, 1.000000000000000000, 0.9238795325112869605, 1.000000000000000000, 0.9238795325112869605, 1.000000000000000000, 0.9238795325112869605, 1.000000000000000000, 0.9238795325112869605, 1.000000000000000000, 0.9238795325112869605, 1.000000000000000000, 0.9238795325112869605, 1.000000000000000000, 0.9238795325112869605, 1.000000000000000000, 0.9238795325112869605, 1.000000000000000000, 0.9238795325112869605, 1.000000000000000000, 0.9238795325112869605, 1.000000000000000000 ) ) 
 REPRESENTATION_ITEM ( '' )  ) ;
#22352 = CARTESIAN_POINT ( 'NONE',  ( 0.8070866141732283561, 0.000000000000000000, 0.7574803149606299524 ) ) ;
#22353 = CARTESIAN_POINT ( 'NONE',  ( -0.1264236179284866091, -1.428765700512702796, 0.1264236179284866091 ) ) ;
#22354 = ORIENTED_EDGE ( 'NONE', *, *, #34217, .T. ) ;
#22355 = DIRECTION ( 'NONE',  ( 1.822029033848725028E-16, 0.000000000000000000, 1.000000000000000000 ) ) ;
#22356 = CARTESIAN_POINT ( 'NONE',  ( 3.284318927891251994E-17, -0.3449803149068665364, 0.1787899950787401882 ) ) ;
#22357 = CARTESIAN_POINT ( 'NONE',  ( 0.7185039370078739607, 1.928577636452523993E-17, 0.5019685039370078705 ) ) ;
#22358 = EDGE_LOOP ( 'NONE', ( #5793, #2491, #767, #30804, #37213 ) ) ;
#22359 = CARTESIAN_POINT ( 'NONE',  ( 0.6971942568897637749, 2.189545951927499583E-17, 1.183562992072220599 ) ) ;
#22360 = STYLED_ITEM ( 'NONE', ( #11550 ), #36588 ) ;
#22361 = DIRECTION ( 'NONE',  ( -1.000000000000000000, 0.000000000000000000, 0.000000000000000000 ) ) ;
#22362 = CARTESIAN_POINT ( 'NONE',  ( -0.2471913174571636063, -0.07307272215568164087, 0.08638584879643394776 ) ) ;
#22363 = CARTESIAN_POINT ( 'NONE',  ( 0.8019270111902717657, -0.1787899950787401604, 1.505905511757261284 ) ) ;
#22364 = CARTESIAN_POINT ( 'NONE',  ( 1.054774247047244540, 0.07405724077823318263, 0.1820866141194649179 ) ) ;
#22365 = AXIS2_PLACEMENT_3D ( 'NONE', #21005, #35874, #39453 ) ;
#22366 = AXIS2_PLACEMENT_3D ( 'NONE', #22328, #11805, #7476 ) ;
#22367 = CARTESIAN_POINT ( 'NONE',  ( -0.07405724077823318263, -1.587598425143086800, -0.1787899950787401604 ) ) ;
#22368 = CARTESIAN_POINT ( 'NONE',  ( 0.07405724077823318263, -1.745078740103716886, -0.1787899950787401604 ) ) ;
#22369 = DIRECTION ( 'NONE',  ( 0.000000000000000000, -1.000000000000000000, 0.000000000000000000 ) ) ;
#22370 = EDGE_CURVE ( 'NONE', #22319, #31526, #35397, .T. ) ;
#22371 = CARTESIAN_POINT ( 'NONE',  ( -1.054774247047244540, -0.07405724077823318263, 0.4576771653005669016 ) ) ;
#22372 = CARTESIAN_POINT ( 'NONE',  ( 0.8759842519685039353, 0.1574803149606299191, 0.3740157480314960647 ) ) ;
#22374 = CARTESIAN_POINT ( 'NONE',  ( -0.7123958336783836609, -0.03406646599270943959, 1.983899093309475781 ) ) ;
#22373 = CARTESIAN_POINT ( 'NONE',  ( 0.07444174185955046430, -1.391283967063361215, -0.1797182628040039087 ) ) ;
#22375 = CARTESIAN_POINT ( 'NONE',  ( -0.03889724126169491480, 0.2730368995492339357, -0.06846571731931054561 ) ) ;
#22376 = CARTESIAN_POINT ( 'NONE',  ( 0.6971942568897637749, 2.189545951927499583E-17, 1.345964566875370139 ) ) ;
#22377 = CARTESIAN_POINT ( 'NONE',  ( 0.6971942568897648851, 0.07405724077823318263, 1.614173228292692386 ) ) ;
#22378 = PLANE ( 'NONE',  #46802 ) ;
#22379 = DIRECTION ( 'NONE',  ( -2.891205793294680298E-16, 1.000000000000000000, 0.000000000000000000 ) ) ;
#22380 = CARTESIAN_POINT ( 'NONE',  ( 1.033464566929133799, 0.000000000000000000, 0.8267716534357796299 ) ) ;
#22381 = DIRECTION ( 'NONE',  ( 0.000000000000000000, -1.000000000000000000, 0.000000000000000000 ) ) ;
#22382 = DIRECTION ( 'NONE',  ( 0.000000000000000000, 0.9699617890481186944, 0.2432573283306645462 ) ) ;
#22383 = CARTESIAN_POINT ( 'NONE',  ( 0.9500414927467378812, -0.1787899950787401604, 0.2903543306548980185 ) ) ;
#22384 = CARTESIAN_POINT ( 'NONE',  ( -0.9412147342319837628, -0.1574803149606297803, 1.724901574695621775 ) ) ;
#22385 = DIRECTION ( 'NONE',  ( 1.000000000000000000, 0.000000000000000000, -1.144917494144692682E-16 ) ) ;
#22386 = LINE ( 'NONE', #19021, #4659 ) ;
#22387 = CARTESIAN_POINT ( 'NONE',  ( -0.6971942568897648851, 0.07405724077823318263, 1.181102362150960428 ) ) ;
#22388 = CARTESIAN_POINT ( 'NONE',  ( 0.8107537697050253289, -0.1574803149606297803, 0.5782480313885360879 ) ) ;
#22389 = ORIENTED_EDGE ( 'NONE', *, *, #6070, .F. ) ;
#22390 = SURFACE_STYLE_USAGE ( .BOTH. , #30341 ) ;
#22391 = CARTESIAN_POINT ( 'NONE',  ( -0.1805243946129686250, -0.4175072877304116248, -0.9858187220043870269 ) ) ;
#22392 = ORIENTED_EDGE ( 'NONE', *, *, #30909, .F. ) ;
#22393 = CARTESIAN_POINT ( 'NONE',  ( 0.7185039370078746268, 0.06523048226347956391, 0.2632874015748031260 ) ) ;
#22394 = CARTESIAN_POINT ( 'NONE',  ( -0.1797182628040039365, -0.001028061551549484288, 0.000000000000000000 ) ) ;
#22395 = CARTESIAN_POINT ( 'NONE',  ( -0.7185039370078746268, 0.06523048226347956391, 1.601870078740158077 ) ) ;
#22396 = CARTESIAN_POINT ( 'NONE',  ( 0.8759842519685039353, 0.1787899950787401882, 1.567421259788755794 ) ) ;
#22398 = CARTESIAN_POINT ( 'NONE',  ( 0.8759842519685039353, 0.1574803149606299191, 1.673228346456693050 ) ) ;
#22397 = CARTESIAN_POINT ( 'NONE',  ( -0.8107537697050254399, 0.1574803149606300301, 1.833169291338582640 ) ) ;
#22399 = CARTESIAN_POINT ( 'NONE',  ( -1.284448818897637956, 0.000000000000000000, -1.181102362204724310 ) ) ;
#22400 = CARTESIAN_POINT ( 'NONE',  ( -0.1787899950787401604, -0.1998031495525358359, -0.07405724077823318263 ) ) ;
#22401 = ORIENTED_EDGE ( 'NONE', *, *, #3254, .T. ) ;
#22402 = AXIS2_PLACEMENT_3D ( 'NONE', #5547, #46023, #13235 ) ;
#22403 = EDGE_CURVE ( 'NONE', #27881, #28992, #35509, .T. ) ;
#22404 = EDGE_CURVE ( 'NONE', #43583, #12067, #1199, .T. ) ;
#22405 = CARTESIAN_POINT ( 'NONE',  ( 0.2759478392031653460, 0.3740157480314960647, 2.185526306663015728 ) ) ;
#22406 = CARTESIAN_POINT ( 'NONE',  ( 0.1807077244537487193, -0.08350519546663393022, -0.1811005174359491543 ) ) ;
#22407 = CARTESIAN_POINT ( 'NONE',  ( 0.8019270111902716547, -0.1787899950787401604, 0.8809055117572600624 ) ) ;
#22408 = CARTESIAN_POINT ( 'NONE',  ( -0.6971942568897648851, -0.07405724077823297447, 1.461614173174583753 ) ) ;
#22409 = CARTESIAN_POINT ( 'NONE',  ( -0.1574803149606297803, 0.06348425207603099196, 0.06523048226347956391 ) ) ;
#22410 = CARTESIAN_POINT ( 'NONE',  ( -1.054774247047244096, 0.000000000000000000, 1.326279527505291433 ) ) ;
#22411 = ( GEOMETRIC_REPRESENTATION_CONTEXT ( 3 ) GLOBAL_UNCERTAINTY_ASSIGNED_CONTEXT ( ( #16866 ) ) GLOBAL_UNIT_ASSIGNED_CONTEXT ( ( #6683, #39509, #10546 ) ) REPRESENTATION_CONTEXT ( 'NONE', 'WORKASPACE' ) ) ;
#22412 = VECTOR ( 'NONE', #5710, 39.37007874015747433 ) ;
#22413 = ORIENTED_EDGE ( 'NONE', *, *, #45284, .T. ) ;
#22414 = EDGE_CURVE ( 'NONE', #39665, #45117, #9359, .T. ) ;
#22415 = CARTESIAN_POINT ( 'NONE',  ( -0.9500414927467378812, -0.1787899950787401604, 0.3346456692375748831 ) ) ;
#22416 = DIRECTION ( 'NONE',  ( 0.000000000000000000, 1.000000000000000000, 0.000000000000000000 ) ) ;
#22417 = DIRECTION ( 'NONE',  ( -0.000000000000000000, 1.000000000000000000, -0.000000000000000000 ) ) ;
#22418 = CARTESIAN_POINT ( 'NONE',  ( -0.07405724077823318263, -0.9292578264969543200, -0.1787899950787401604 ) ) ;
#22419 = VECTOR ( 'NONE', #18827, 39.37007874015748143 ) ;
#22420 = ORIENTED_EDGE ( 'NONE', *, *, #12375, .T. ) ;
#22421 = CARTESIAN_POINT ( 'NONE',  ( 0.7670496988260933069, 0.1418927192561055817, 0.03937512220365226023 ) ) ;
#22422 = ORIENTED_EDGE ( 'NONE', *, *, #8615, .T. ) ;
#22423 = DIRECTION ( 'NONE',  ( 0.000000000000000000, 0.000000000000000000, 1.000000000000000000 ) ) ;
#22424 = CARTESIAN_POINT ( 'NONE',  ( 0.03901279071809810040, -0.5708661417322835607, 1.713085361781127913 ) ) ;
#22425 = CARTESIAN_POINT ( 'NONE',  ( -0.1787899950787401604, -0.4803149605761579677, -0.07405724077823318263 ) ) ;
#22426 = VERTEX_POINT ( 'NONE', #17326 ) ;
#22427 = AXIS2_PLACEMENT_3D ( 'NONE', #3695, #28901, #10911 ) ;
#22428 = CARTESIAN_POINT ( 'NONE',  ( -0.6971942568897626646, -0.07405724077823297447, 0.08858267711159095725 ) ) ;
#22429 = CARTESIAN_POINT ( 'NONE',  ( -1.033464566929133799, 0.000000000000000000, 0.9547244094488189781 ) ) ;
#22430 = DIRECTION ( 'NONE',  ( 1.000000000000000000, -0.000000000000000000, -0.000000000000000000 ) ) ;
#22431 = CARTESIAN_POINT ( 'NONE',  ( 0.1797182628040039087, -0.9631343607641484894, -0.07444174185955065859 ) ) ;
#22432 = CARTESIAN_POINT ( 'NONE',  ( 0.1008439437011256906, -0.2372714618124188435, -0.3138705397960864785 ) ) ;
#22433 = CARTESIAN_POINT ( 'NONE',  ( -1.033464566929134687, -0.06523048226347956391, 1.532972440837355066 ) ) ;
#22434 = CARTESIAN_POINT ( 'NONE',  ( 0.8019270111902717657, 0.1787899950787401604, 0.9842519684501742638 ) ) ;
#22435 = PRODUCT_DEFINITION_FORMATION_WITH_SPECIFIED_SOURCE ( 'ANY', '', #29172, .NOT_KNOWN. ) ;
#22436 = AXIS2_PLACEMENT_3D ( 'NONE', #33916, #40573, #36544 ) ;
#22437 = CARTESIAN_POINT ( 'NONE',  ( 0.4330708661417322913, 0.1574803149606299191, 1.186023622047243986 ) ) ;
#22438 = CARTESIAN_POINT ( 'NONE',  ( 0.9873396505805591694, 0.1113553986120547346, 1.432086614173228245 ) ) ;
#22440 = CARTESIAN_POINT ( 'NONE',  ( 0.1113553986120547346, 0.1151574804224878013, 0.1113553986120547346 ) ) ;
#22439 = CARTESIAN_POINT ( 'NONE',  ( 0.7125671091357160813, -0.03503208222838762737, 1.983917631934041026 ) ) ;
#22441 = LINE ( 'NONE', #44467, #26676 ) ;
#22443 = LINE ( 'NONE', #37783, #1677 ) ;
#22442 = CARTESIAN_POINT ( 'NONE',  ( 0.8759842519685039353, -0.1787899950787401882, 0.7603346456155274380 ) ) ;
#22444 = CARTESIAN_POINT ( 'NONE',  ( -0.1264236179284866091, -0.8321850393163149340, -0.1264236179284866091 ) ) ;
#22445 = VERTEX_POINT ( 'NONE', #2463 ) ;
#22446 = ADVANCED_FACE ( 'NONE', ( #17559, #47025, #32197 ), #28621, .F. ) ;
#22447 = CARTESIAN_POINT ( 'NONE',  ( 0.7185039370078746268, 0.06523048226347956391, 1.090059055118109965 ) ) ;
#22448 = CARTESIAN_POINT ( 'NONE',  ( 1.054774247047244540, 0.07405724077823318263, 1.087598425143086578 ) ) ;
#22449 = DIRECTION ( 'NONE',  ( 0.000000000000000000, 1.000000000000000000, 0.000000000000000000 ) ) ;
#22450 = CARTESIAN_POINT ( 'NONE',  ( 0.1574803149606300301, -1.624507874015748810, 0.06523048226347956391 ) ) ;
#22451 = PLANE ( 'NONE',  #14544 ) ;
#22452 = ORIENTED_EDGE ( 'NONE', *, *, #25107, .F. ) ;
#22453 = CARTESIAN_POINT ( 'NONE',  ( 0.8759842519685039353, -0.1574803149606300579, 0.03937007874015747977 ) ) ;
#22454 = CARTESIAN_POINT ( 'NONE',  ( -1.054774247047244096, 0.000000000000000000, 0.2189960629383626012 ) ) ;
#22455 = ORIENTED_EDGE ( 'NONE', *, *, #14578, .T. ) ;
#22456 = CARTESIAN_POINT ( 'NONE',  ( -1.033464566929134687, -0.06523048226347956391, 0.7160433070866151217 ) ) ;
#22457 = CARTESIAN_POINT ( 'NONE',  ( -9.642888182262618425E-18, -0.3031496061916854612, -0.1574803149606299191 ) ) ;
#22458 = CARTESIAN_POINT ( 'NONE',  ( 0.7185039370078746268, -0.06523048226347956391, 0.3371062991050715607 ) ) ;
#22459 = CARTESIAN_POINT ( 'NONE',  ( -0.6971942568897648851, -0.07405724077823297447, 1.619094488135213838 ) ) ;
#22460 = CARTESIAN_POINT ( 'NONE',  ( -0.9500414927467377701, -0.1787899950787401604, 0.9202755904974182499 ) ) ;
#22461 = AXIS2_PLACEMENT_3D ( 'NONE', #17025, #1927, #46238 ) ;
#22462 = EDGE_CURVE ( 'NONE', #34892, #42619, #17090, .T. ) ;
#22463 = CARTESIAN_POINT ( 'NONE',  ( -0.9500414927467378812, -0.1787899950787401604, 0.5708661416785201226 ) ) ;
#22464 = ( BOUNDED_CURVE ( )  B_SPLINE_CURVE ( 2, ( #27531, #42083, #26572, #27048, #11951, #41127, #8324, #34002, #1131 ),
 .UNSPECIFIED., .F., .T. ) 
 B_SPLINE_CURVE_WITH_KNOTS ( ( 3, 2, 2, 2, 3 ),
 ( 0.9699999999999999734, 0.9725000000000000311, 0.9749999999999999778, 0.9775000000000000355, 0.9799999999999999822 ),
 .UNSPECIFIED. ) 
 CURVE ( )  GEOMETRIC_REPRESENTATION_ITEM ( )  RATIONAL_B_SPLINE_CURVE ( ( 1.000000000000000000, 0.9238795325112869605, 1.000000000000000000, 0.9238795325112869605, 1.000000000000000000, 0.9238795325112869605, 1.000000000000000000, 0.9238795325112869605, 1.000000000000000000 ) ) 
 REPRESENTATION_ITEM ( '' )  ) ;
#22465 = EDGE_CURVE ( 'NONE', #4124, #35796, #30087, .T. ) ;
#22466 = CARTESIAN_POINT ( 'NONE',  ( 0.5113546317124669782, 4.466152701071653354E-17, 0.000000000000000000 ) ) ;
#22467 = CARTESIAN_POINT ( 'NONE',  ( 1.033464566929133799, 0.000000000000000000, 0.9940944881889764995 ) ) ;
#22468 = CYLINDRICAL_SURFACE ( 'NONE', #20317, 0.1574803149606299191 ) ;
#22469 = CARTESIAN_POINT ( 'NONE',  ( 0.7495606340400177148, -0.1264236179284866091, 0.08612204719033110523 ) ) ;
#22470 = LINE ( 'NONE', #40196, #22112 ) ;
#22471 = CARTESIAN_POINT ( 'NONE',  ( 0.1264236179284866091, -0.4346712123237267966, 0.1264236179284866091 ) ) ;
#22472 = CARTESIAN_POINT ( 'NONE',  ( 0.08190613820814231227, -0.09842519685039370636, 0.1253801239223421293 ) ) ;
#22473 = FACE_OUTER_BOUND ( 'NONE', #3901, .T. ) ;
#22474 = DIRECTION ( 'NONE',  ( 0.000000000000000000, 1.000000000000000000, 0.000000000000000000 ) ) ;
#22475 = AXIS2_PLACEMENT_3D ( 'NONE', #9061, #41376, #41857 ) ;
#22476 = CARTESIAN_POINT ( 'NONE',  ( 0.2559054921376553993, -0.04463177124945857249, -0.03568053490012755569 ) ) ;
#22477 = CARTESIAN_POINT ( 'NONE',  ( -0.6971942568897637749, 2.189545951927499583E-17, 0.3174212597887562382 ) ) ;
#22478 = ORIENTED_EDGE ( 'NONE', *, *, #32542, .T. ) ;
#22479 = VERTEX_POINT ( 'NONE', #24296 ) ;
#22480 = CARTESIAN_POINT ( 'NONE',  ( -0.6971942568897637749, 2.189545951927499583E-17, 1.424704724355685181 ) ) ;
#22481 = ORIENTED_EDGE ( 'NONE', *, *, #3021, .F. ) ;
#22482 = CARTESIAN_POINT ( 'NONE',  ( 0.1264236179284866091, -1.280019684985606254, -0.1264236179284866091 ) ) ;
#22483 = CARTESIAN_POINT ( 'NONE',  ( 0.1787899950787401882, -1.555610236166708571, -2.189545951927503898E-17 ) ) ;
#22484 = DIRECTION ( 'NONE',  ( 1.000000000000000000, -1.000000000000000078E-15, 0.000000000000000000 ) ) ;
#22485 = CARTESIAN_POINT ( 'NONE',  ( 0.7185039370078746268, -0.06523048226347956391, 0.3469488188976379561 ) ) ;
#22486 = DIRECTION ( 'NONE',  ( 3.385139170096289319E-15, 1.000000000000000000, 0.000000000000000000 ) ) ;
#22487 = CARTESIAN_POINT ( 'NONE',  ( -0.9873396505805591694, -0.1113553986120547346, 1.097440944774362270 ) ) ;
#22488 = CARTESIAN_POINT ( 'NONE',  ( 0.6971942568897626646, 0.07405724077823318263, 0.5167322834108034613 ) ) ;
#22489 = CARTESIAN_POINT ( 'NONE',  ( 1.033464566929133799, 0.000000000000000000, 0.5511811022546778682 ) ) ;
#22490 = CARTESIAN_POINT ( 'NONE',  ( -0.06523048226347956391, -0.2957677165354329341, 0.1574803149606297803 ) ) ;
#22491 = CARTESIAN_POINT ( 'NONE',  ( 0.4453382816733590377, -0.09842519685039370636, 1.205361022782828805E-17 ) ) ;
#22492 = ORIENTED_EDGE ( 'NONE', *, *, #42976, .F. ) ;
#22493 = EDGE_CURVE ( 'NONE', #6130, #9939, #39352, .T. ) ;
#22494 = CARTESIAN_POINT ( 'NONE',  ( -0.1158283541424031532, -0.08956345598586890056, -0.1361971163587911426 ) ) ;
#22495 = CARTESIAN_POINT ( 'NONE',  ( -1.054774247047244096, 0.000000000000000000, 0.9325787401037164415 ) ) ;
#22496 = CARTESIAN_POINT ( 'NONE',  ( 0.9873396505805591694, 0.1113553986120547346, 0.9990157480314961758 ) ) ;
#22497 = CARTESIAN_POINT ( 'NONE',  ( 0.2642359194686346169, 0.09842519685039370636, 0.000000000000000000 ) ) ;
#22498 = EDGE_CURVE ( 'NONE', #39149, #42397, #43181, .T. ) ;
#22500 = CARTESIAN_POINT ( 'NONE',  ( 0.8759842519685039353, -0.1574803149606299191, 1.535433070866141669 ) ) ;
#22499 = LINE ( 'NONE', #4498, #14851 ) ;
#22501 = CARTESIAN_POINT ( 'NONE',  ( -0.07885344035849289890, -0.08956334183977000818, 0.1372477332191901489 ) ) ;
#22502 = ORIENTED_EDGE ( 'NONE', *, *, #37774, .T. ) ;
#22503 = ADVANCED_FACE ( 'NONE', ( #24756 ), #44562, .F. ) ;
#22504 = CARTESIAN_POINT ( 'NONE',  ( 0.1637325661183565428, 0.08225671873206810703, -0.1377952755905511306 ) ) ;
#22505 = VERTEX_POINT ( 'NONE', #3170 ) ;
#22506 = CARTESIAN_POINT ( 'NONE',  ( 0.4736248074375818407, 1.101950626536848388, -0.8609381856333149230 ) ) ;
#22507 = CARTESIAN_POINT ( 'NONE',  ( 0.1574803149606299191, 0.6241017553149685870, 0.3240160679609074834 ) ) ;
#22508 = CARTESIAN_POINT ( 'NONE',  ( 0.1264236179284866091, -1.511318897584031484, -0.1264236179284866091 ) ) ;
#22509 = CARTESIAN_POINT ( 'NONE',  ( 3.284318927891251994E-17, -0.7042322834108031282, 0.1787899950787401882 ) ) ;
#22510 = CARTESIAN_POINT ( 'NONE',  ( -0.1574803149606297803, -1.284940944881890923, 0.06523048226347956391 ) ) ;
#22511 = CARTESIAN_POINT ( 'NONE',  ( 0.9873396505805591694, -0.1113553986120547346, 1.097440944774362270 ) ) ;
#22512 = PLANE ( 'NONE',  #26020 ) ;
#22513 = UNCERTAINTY_MEASURE_WITH_UNIT (LENGTH_MEASURE( 1.000000000000000082E-05 ), #7227, 'distance_accuracy_value', 'NONE') ;
#22514 = ORIENTED_EDGE ( 'NONE', *, *, #2373, .F. ) ;
#22515 = ORIENTED_EDGE ( 'NONE', *, *, #4092, .F. ) ;
#22516 = ORIENTED_EDGE ( 'NONE', *, *, #43595, .T. ) ;
#22517 = CARTESIAN_POINT ( 'NONE',  ( -0.7495606340400177148, 0.1264236179284866091, 1.813484251914740053 ) ) ;
#22518 = CARTESIAN_POINT ( 'NONE',  ( 0.9500414927467378812, 0.1787899950787401604, 1.648622047190331230 ) ) ;
#22519 = CARTESIAN_POINT ( 'NONE',  ( -0.8759842519685039353, 0.1787899950787401882, 0.8636811023084409733 ) ) ;
#22520 = CARTESIAN_POINT ( 'NONE',  ( 1.229559056033039366E-16, 0.000000000000000000, 0.3937007874015748254 ) ) ;
#22521 = CARTESIAN_POINT ( 'NONE',  ( 0.9500414927467378812, -0.1787899950787401604, 0.2559055117572600624 ) ) ;
#22522 = CARTESIAN_POINT ( 'NONE',  ( -1.033464566929134687, 0.06523048226347956391, 1.498523621939716444 ) ) ;
#22523 = CARTESIAN_POINT ( 'NONE',  ( -0.8019270111902716547, -0.1787899950787401604, 1.309055118056473122 ) ) ;
#22524 = CARTESIAN_POINT ( 'NONE',  ( -0.6971942568897637749, 2.189545951927499583E-17, 0.7898622046706456068 ) ) ;
#22525 = CARTESIAN_POINT ( 'NONE',  ( -0.9500414927467378812, 0.1787899950787401604, 0.9350393700249758355 ) ) ;
#22526 = CARTESIAN_POINT ( 'NONE',  ( 0.07600661141694387002, 0.08819060268787905221, 0.2415506333043779541 ) ) ;
#22527 = CARTESIAN_POINT ( 'NONE',  ( -0.8019270111902717657, 0.1787899950787401604, 1.653543307032850462 ) ) ;
#22528 = CARTESIAN_POINT ( 'NONE',  ( -0.8759842519685039353, -0.1574803149606299191, 1.879921259734992134 ) ) ;
#22529 = ORIENTED_EDGE ( 'NONE', *, *, #5913, .F. ) ;
#22530 = CARTESIAN_POINT ( 'NONE',  ( -1.033464566929133799, 0.000000000000000000, 1.624015748031496287 ) ) ;
#22531 = CARTESIAN_POINT ( 'NONE',  ( 0.1647351823960283845, -0.4387500173593407160, -0.9692220826775356235 ) ) ;
#22532 = CARTESIAN_POINT ( 'NONE',  ( 0.6971942568897637749, 2.189545951927499583E-17, 1.582185039316315045 ) ) ;
#22533 = CARTESIAN_POINT ( 'NONE',  ( -0.2118147889498118164, -0.09842519685039370636, 0.1047082926952616067 ) ) ;
#22534 = CARTESIAN_POINT ( 'NONE',  ( 0.7646288533564489232, -0.1113553986120547346, 1.008858267609007875 ) ) ;
#22535 = ORIENTED_EDGE ( 'NONE', *, *, #33520, .F. ) ;
#22536 = ORIENTED_EDGE ( 'NONE', *, *, #4010, .F. ) ;
#22537 = CIRCLE ( 'NONE', #16438, 0.09842519685039370636 ) ;
#22538 = LENGTH_MEASURE_WITH_UNIT ( LENGTH_MEASURE( 0.02539999999999999897 ), #36695 ) ;
#22539 = ORIENTED_EDGE ( 'NONE', *, *, #6034, .F. ) ;
#22540 = AXIS2_PLACEMENT_3D ( 'NONE', #16212, #11429, #7814 ) ;
#22541 = VECTOR ( 'NONE', #26765, 39.37007874015748143 ) ;
#22542 = CARTESIAN_POINT ( 'NONE',  ( -0.07405724077823318263, -0.8789370078202529690, -0.1787899950787401604 ) ) ;
#22543 = CARTESIAN_POINT ( 'NONE',  ( 3.284318927891251994E-17, -0.4680118109698582773, 0.1787899950787401882 ) ) ;
#22544 = CARTESIAN_POINT ( 'NONE',  ( -0.1264236179284866091, -0.9896653542769447975, -0.1264236179284866091 ) ) ;
#22545 = EDGE_LOOP ( 'NONE', ( #3969, #5037, #21442, #45586, #45700 ) ) ;
#22546 = CARTESIAN_POINT ( 'NONE',  ( -0.3161444924769509779, 2.177585298233989164, -3.731703755406937439 ) ) ;
#22547 = CARTESIAN_POINT ( 'NONE',  ( 0.8759842519685039353, -0.1787899950787401882, 1.783956692859621995 ) ) ;
#22548 = CARTESIAN_POINT ( 'NONE',  ( 0.1270800023317771588, -0.3701225497405259968, -0.1270800023317771588 ) ) ;
#22549 = CARTESIAN_POINT ( 'NONE',  ( -0.1574803149606297803, 0.1323818897637794312, 0.06523048226347956391 ) ) ;
#22550 = EDGE_CURVE ( 'NONE', #8098, #829, #41460, .T. ) ;
#22551 = CARTESIAN_POINT ( 'NONE',  ( 0.6971942568897637749, 2.189545951927499583E-17, 0.8292322834108031282 ) ) ;
#22552 = EDGE_CURVE ( 'NONE', #29529, #42873, #9911, .T. ) ;
#22554 = CARTESIAN_POINT ( 'NONE',  ( 0.7646288533564489232, 0.1113553986120547346, 1.126968503937007871 ) ) ;
#22553 = DIRECTION ( 'NONE',  ( 0.000000000000000000, 0.000000000000000000, -1.000000000000000000 ) ) ;
#22556 = DIRECTION ( 'NONE',  ( 0.000000000000000000, 0.000000000000000000, 1.000000000000000000 ) ) ;
#22555 = FACE_OUTER_BOUND ( 'NONE', #31589, .T. ) ;
#22557 = CARTESIAN_POINT ( 'NONE',  ( 0.8759842519685039353, -0.1574803149606299191, 1.259842519685039353 ) ) ;
#22558 = CARTESIAN_POINT ( 'NONE',  ( 1.054774247047244540, -0.07405724077823318263, 1.835629921206078485 ) ) ;
#22559 = DIRECTION ( 'NONE',  ( -1.000000000000000000, 0.000000000000000000, 0.000000000000000000 ) ) ;
#22560 = EDGE_CURVE ( 'NONE', #41698, #41647, #32720, .T. ) ;
#22561 = EDGE_CURVE ( 'NONE', #33076, #36696, #24177, .T. ) ;
#22562 = CARTESIAN_POINT ( 'NONE',  ( 1.033464566929134687, 0.06523048226347956391, 0.1304133858267717272 ) ) ;
#22563 = DIRECTION ( 'NONE',  ( 0.000000000000000000, 0.000000000000000000, -1.000000000000000000 ) ) ;
#22565 = CARTESIAN_POINT ( 'NONE',  ( 0.1787899950787401604, -0.2637795275052916555, 0.07405724077823318263 ) ) ;
#22564 = CARTESIAN_POINT ( 'NONE',  ( -0.1574803149606299191, -0.9625984250893229177, 0.000000000000000000 ) ) ;
#22567 = CARTESIAN_POINT ( 'NONE',  ( 0.1588779435336218349, 0.1435649425735163465, 0.03225083113271716428 ) ) ;
#22566 = CARTESIAN_POINT ( 'NONE',  ( -0.8759842519685039353, -0.1787899950787401882, 0.4109251967966299213 ) ) ;
#22568 = CARTESIAN_POINT ( 'NONE',  ( 0.1264236179284866091, -1.235728346402928945, -0.1264236179284866091 ) ) ;
#22569 = CARTESIAN_POINT ( 'NONE',  ( 0.7495606340400177148, 0.1264236179284866091, 0.2780511810485988278 ) ) ;
#22570 = CARTESIAN_POINT ( 'NONE',  ( 0.8107537697050254399, 0.1574803149606300301, 1.114665354223180804 ) ) ;
#22571 = CARTESIAN_POINT ( 'NONE',  ( -0.9500414927467378812, -0.1787899950787401604, 1.786417322780882388 ) ) ;
#22572 = ORIENTED_EDGE ( 'NONE', *, *, #42184, .T. ) ;
#22573 = CARTESIAN_POINT ( 'NONE',  ( 0.8019270111902717657, -0.1787899950787401604, 1.313976377898992132 ) ) ;
#22574 = CIRCLE ( 'NONE', #34071, 0.3100393700787401619 ) ;
#22575 = CIRCLE ( 'NONE', #15737, 0.009842519685039378616 ) ;
#22576 = CARTESIAN_POINT ( 'NONE',  ( 0.1574803149606300301, -1.181594488081448846, 0.06523048226347956391 ) ) ;
#22577 = CARTESIAN_POINT ( 'NONE',  ( 1.054774247047244096, 0.000000000000000000, 0.02706692908009476414 ) ) ;
#22578 = CARTESIAN_POINT ( 'NONE',  ( -0.8759842519685039353, 0.1787899950787401882, 1.016240157426551161 ) ) ;
#22579 = CARTESIAN_POINT ( 'NONE',  ( 0.1599045142068303837, 0.1486426375328276928, -0.02349808476882435729 ) ) ;
#22580 = CARTESIAN_POINT ( 'NONE',  ( 0.1184675242425088648, -0.09842519685039370636, 1.555605046820498050 ) ) ;
#22581 = CARTESIAN_POINT ( 'NONE',  ( 0.7495606340400177148, 0.1264236179284866091, 0.5142716534895434011 ) ) ;
#22582 = CARTESIAN_POINT ( 'NONE',  ( -0.6971942568897626646, 0.07405724077823318263, 0.3149606298674962890 ) ) ;
#22583 = CARTESIAN_POINT ( 'NONE',  ( -0.9500414927467378812, 0.1787899950787401604, 0.6988188975840318173 ) ) ;
#22584 = CARTESIAN_POINT ( 'NONE',  ( 0.9873396505805591694, 0.1113553986120547346, 1.697834645561763889 ) ) ;
#22585 = ORIENTED_EDGE ( 'NONE', *, *, #23019, .T. ) ;
#22586 = VERTEX_POINT ( 'NONE', #21635 ) ;
#22587 = CYLINDRICAL_SURFACE ( 'NONE', #47426, 0.1574803149606299191 ) ;
#22588 = ORIENTED_EDGE ( 'NONE', *, *, #36491, .F. ) ;
#22589 = CARTESIAN_POINT ( 'NONE',  ( -1.033464566929133799, 0.000000000000000000, 0.1673228346456692994 ) ) ;
#22590 = CARTESIAN_POINT ( 'NONE',  ( 0.6971942568897637749, 2.189545951927499583E-17, 1.031003936954110189 ) ) ;
#22591 = DIRECTION ( 'NONE',  ( 0.000000000000000000, 0.7880107536067203489, -0.6156614753256602901 ) ) ;
#22592 = ORIENTED_EDGE ( 'NONE', *, *, #3528, .T. ) ;
#22593 = CARTESIAN_POINT ( 'NONE',  ( 0.8759842519685039353, -0.1787899950787401882, 1.862696850339937038 ) ) ;
#22594 = CARTESIAN_POINT ( 'NONE',  ( -0.6971942568897626646, -0.07405724077823297447, 0.8759842519147408302 ) ) ;
#22595 = B_SPLINE_CURVE_WITH_KNOTS ( 'NONE', 3,
 ( #10234, #6380, #43278, #13362, #28215, #42779 ),
 .UNSPECIFIED., .F., .F.,
 ( 4, 2, 4 ),
 ( 0.000000000000000000, 0.5000000000000000000, 1.000000000000000000 ),
 .UNSPECIFIED. ) ;
#22596 = CARTESIAN_POINT ( 'NONE',  ( -0.6971942568897626646, 0.07405724077823318263, 0.07874015742655145200 ) ) ;
#22597 = CARTESIAN_POINT ( 'NONE',  ( 0.07405724077823318263, -1.421383810748923393, 0.1787899950787401604 ) ) ;
#22598 = ORIENTED_EDGE ( 'NONE', *, *, #44107, .F. ) ;
#22599 = CARTESIAN_POINT ( 'NONE',  ( -0.1787899950787401604, -0.3966535432533230265, -0.07405724077823318263 ) ) ;
#22600 = CARTESIAN_POINT ( 'NONE',  ( -0.2896304277639954461, -0.1109299681405384735, 0.7502625622129650562 ) ) ;
#22601 = ORIENTED_EDGE ( 'NONE', *, *, #34924, .T. ) ;
#22602 = CARTESIAN_POINT ( 'NONE',  ( 0.8019270111902717657, -0.1787899950787401604, 1.230314960576156746 ) ) ;
#22603 = CARTESIAN_POINT ( 'NONE',  ( 1.033464566929133799, 0.000000000000000000, 1.978346456692913646 ) ) ;
#22604 = CARTESIAN_POINT ( 'NONE',  ( 0.7185039370078739607, 1.928577636452523993E-17, 0.7283464565853858819 ) ) ;
#22605 = CARTESIAN_POINT ( 'NONE',  ( -0.9412147342319837628, 0.1574803149606300301, 1.434547244094487972 ) ) ;
#22606 = CARTESIAN_POINT ( 'NONE',  ( 1.054774247047244540, -0.07405724077823318263, 1.515748031442299526 ) ) ;
#22607 = AXIS2_PLACEMENT_3D ( 'NONE', #885, #44734, #11950 ) ;
#22608 = AXIS2_PLACEMENT_3D ( 'NONE', #16429, #46103, #2028 ) ;
#22609 = CARTESIAN_POINT ( 'NONE',  ( 0.1787899950787401882, -1.757381889710015965, -2.189545951927503898E-17 ) ) ;
#22610 = CARTESIAN_POINT ( 'NONE',  ( 3.284318927891251994E-17, -1.644192913332062966, 0.1787899950787401882 ) ) ;
#22611 = PRODUCT_CONTEXT ( 'NONE', #15052, 'mechanical' ) ;
#22612 = CARTESIAN_POINT ( 'NONE',  ( 0.7646288533564489232, -0.1113553986120547346, 1.333661417322834719 ) ) ;
#22613 = ( BOUNDED_CURVE ( )  B_SPLINE_CURVE ( 2, ( #32791, #30157, #18383, #18148, #7587, #44696, #47386, #14559, #14803 ),
 .UNSPECIFIED., .F., .T. ) 
 B_SPLINE_CURVE_WITH_KNOTS ( ( 3, 2, 2, 2, 3 ),
 ( 0.8499999999999999778, 0.8525000000000000355, 0.8549999999999999822, 0.8575000000000000400, 0.8599999999999999867 ),
 .UNSPECIFIED. ) 
 CURVE ( )  GEOMETRIC_REPRESENTATION_ITEM ( )  RATIONAL_B_SPLINE_CURVE ( ( 1.000000000000000000, 0.9238795325112939549, 1.000000000000000000, 0.9238795325112869605, 1.000000000000000000, 0.9238795325112869605, 1.000000000000000000, 0.9238795325112869605, 1.000000000000000000 ) ) 
 REPRESENTATION_ITEM ( '' )  ) ;
#22614 = EDGE_CURVE ( 'NONE', #14891, #5868, #19246, .T. ) ;
#22615 = CARTESIAN_POINT ( 'NONE',  ( -0.6971942568897648851, 0.07405724077823318263, 0.6742125983714336579 ) ) ;
#22617 = CARTESIAN_POINT ( 'NONE',  ( 0.7646288533564489232, 0.1113553986120547346, 0.3789370078740157410 ) ) ;
#22616 = CARTESIAN_POINT ( 'NONE',  ( 0.1113553986120547346, -0.8001968503937008093, 0.1113553986120547346 ) ) ;
#22618 = CARTESIAN_POINT ( 'NONE',  ( 0.07444174185955065859, -1.445417825331076767, 0.1797182628040039087 ) ) ;
#22619 = DIRECTION ( 'NONE',  ( 0.000000000000000000, 1.000000000000000000, 0.000000000000000000 ) ) ;
#22620 = CARTESIAN_POINT ( 'NONE',  ( 0.2471922904502826812, 0.09842519685039370636, -5.914624404477007554E-17 ) ) ;
#22621 = CARTESIAN_POINT ( 'NONE',  ( 0.8759842519685039353, -0.1787899950787401882, 1.316437007820252081 ) ) ;
#22622 = CARTESIAN_POINT ( 'NONE',  ( 0.7495606340400177148, 0.1264236179284866091, 1.729822834591905556 ) ) ;
#22623 = CARTESIAN_POINT ( 'NONE',  ( 0.8759842519685039353, 0.1787899950787401882, 0.2682086613635594752 ) ) ;
#22624 = DIRECTION ( 'NONE',  ( 1.885568995626964040E-16, 0.6156614753256598460, 0.7880107536067206819 ) ) ;
#22625 = EDGE_CURVE ( 'NONE', #19741, #34889, #43396, .T. ) ;
#22626 = CARTESIAN_POINT ( 'NONE',  ( 0.2362204724409449064, 0.3740157480314960647, 0.9783464566929134243 ) ) ;
#22627 = CARTESIAN_POINT ( 'NONE',  ( 0.9412147342319837628, -0.1574803149606297803, 0.8193897636719996713 ) ) ;
#22628 = CARTESIAN_POINT ( 'NONE',  ( 0.1574803149606299191, 0.4668427075568346574, -0.7022306805398661478 ) ) ;
#22629 = CARTESIAN_POINT ( 'NONE',  ( 0.9873396505805591694, -0.1113553986120547346, 0.5462598424121581919 ) ) ;
#22630 = CARTESIAN_POINT ( 'NONE',  ( 1.054774247047244096, 0.000000000000000000, 0.3371062991588349989 ) ) ;
#22632 = CARTESIAN_POINT ( 'NONE',  ( -0.8759842519685039353, 0.1574803149606299191, 1.712598425196850238 ) ) ;
#22631 = CARTESIAN_POINT ( 'NONE',  ( 0.9500414927467377701, 0.1787899950787401604, 1.289370078686393750 ) ) ;
#22633 = CARTESIAN_POINT ( 'NONE',  ( -1.033464566929134687, -0.06523048226347956391, 1.336122047136566904 ) ) ;
#22634 = CARTESIAN_POINT ( 'NONE',  ( -0.7646288533564489232, 0.1113553986120547346, 0.9596456691838111119 ) ) ;
#22635 = CARTESIAN_POINT ( 'NONE',  ( -0.8019270111902717657, -0.1787899950787401604, 1.348425196796630976 ) ) ;
#22636 = CARTESIAN_POINT ( 'NONE',  ( 0.8759842519685039353, -0.1574803149606299191, 0.6988188975302678241 ) ) ;
#22637 = VERTEX_POINT ( 'NONE', #7255 ) ;
#22638 = CARTESIAN_POINT ( 'NONE',  ( 0.7185039370078739607, 1.928577636452523993E-17, 1.407480314960629864 ) ) ;
#22639 = CARTESIAN_POINT ( 'NONE',  ( -0.1925018001412950874, -0.3879436464012143704, -1.008916370042088673 ) ) ;
#22640 = ORIENTED_EDGE ( 'NONE', *, *, #44884, .T. ) ;
#22641 = CARTESIAN_POINT ( 'NONE',  ( 3.301370929368692659E-17, -0.06992569934682500710, 0.1797182628040039365 ) ) ;
#22642 = PLANE ( 'NONE',  #12968 ) ;
#22643 = PRODUCT_DEFINITION_SHAPE ( 'NONE', 'NONE',  #47479 ) ;
#22644 = CARTESIAN_POINT ( 'NONE',  ( 0.1264236179284866091, -1.201279527505291433, -0.1264236179284866091 ) ) ;
#22645 = CARTESIAN_POINT ( 'NONE',  ( -0.6195511811023656223, 1.354170115732555191, -0.4197102375732078561 ) ) ;
#22646 = CARTESIAN_POINT ( 'NONE',  ( 0.9500414927467378812, -0.1787899950787401604, 1.589566929080094448 ) ) ;
#22647 = CARTESIAN_POINT ( 'NONE',  ( -1.033464566929134687, -0.06523048226347956391, 1.227854330708661124 ) ) ;
#22648 = AXIS2_PLACEMENT_3D ( 'NONE', #14098, #17443, #7137 ) ;
#22649 = CARTESIAN_POINT ( 'NONE',  ( 0.000000000000000000, 0.000000000000000000, -0.1828167807439035619 ) ) ;
#22650 = CARTESIAN_POINT ( 'NONE',  ( -0.08091701073424910351, -0.5708661417322835607, 1.112073044918589382 ) ) ;
#22651 = CARTESIAN_POINT ( 'NONE',  ( 0.1787899950787401882, -0.1382874015210395768, -2.189545951927503898E-17 ) ) ;
#22652 = ORIENTED_EDGE ( 'NONE', *, *, #39484, .F. ) ;
#22653 = ( BOUNDED_CURVE ( )  B_SPLINE_CURVE ( 2, ( #42424, #38614, #20633, #12995, #46029, #23768, #5308, #27638, #19925 ),
 .UNSPECIFIED., .F., .F. ) 
 B_SPLINE_CURVE_WITH_KNOTS ( ( 3, 2, 2, 2, 3 ),
 ( 0.8199999999999999512, 0.8225000000000000089, 0.8249999999999999556, 0.8275000000000000133, 0.8299999999999999600 ),
 .UNSPECIFIED. ) 
 CURVE ( )  GEOMETRIC_REPRESENTATION_ITEM ( )  RATIONAL_B_SPLINE_CURVE ( ( 1.000000000000000000, 0.9238795325112899581, 1.000000000000000000, 0.9238795325112869605, 1.000000000000000000, 0.9238795325112869605, 1.000000000000000000, 0.9238795325112799661, 1.000000000000000000 ) ) 
 REPRESENTATION_ITEM ( '' )  ) ;
#22654 = SURFACE_STYLE_FILL_AREA ( #40830 ) ;
#22655 = CARTESIAN_POINT ( 'NONE',  ( 1.054774247047244540, -0.07405724077823318263, 0.8120078739619844832 ) ) ;
#22656 = CARTESIAN_POINT ( 'NONE',  ( 0.1113553986120547346, -0.1112204723334179052, -0.1113553986120547346 ) ) ;
#22657 = CARTESIAN_POINT ( 'NONE',  ( -0.8019270111902717657, -0.1787899950787401604, 1.353346456639149986 ) ) ;
#22658 = AXIS2_PLACEMENT_3D ( 'NONE', #2674, #2903, #16831 ) ;
#22659 = EDGE_LOOP ( 'NONE', ( #2631, #7989, #36081, #19498 ) ) ;
#22660 = ADVANCED_FACE ( 'NONE', ( #25723 ), #40522, .F. ) ;
#22661 = CARTESIAN_POINT ( 'NONE',  ( -0.9500414927467378812, -0.1787899950787401604, 0.2952755904974176393 ) ) ;
#22662 = CARTESIAN_POINT ( 'NONE',  ( 0.3246033735368759610, 4.766607801171850497E-17, 0.000000000000000000 ) ) ;
#22663 = CARTESIAN_POINT ( 'NONE',  ( 0.1787899950787401882, -1.020301133583568776, -2.189545951927503898E-17 ) ) ;
#22664 = ORIENTED_EDGE ( 'NONE', *, *, #31147, .F. ) ;
#22665 = CARTESIAN_POINT ( 'NONE',  ( 3.284318927891251994E-17, 0.08809055123486594918, 0.1787899950787401882 ) ) ;
#22666 = VERTEX_POINT ( 'NONE', #22095 ) ;
#22667 = CARTESIAN_POINT ( 'NONE',  ( 0.7185039370078739607, 1.928577636452523993E-17, 1.131889763779527547 ) ) ;
#22668 = DIRECTION ( 'NONE',  ( 0.000000000000000000, -1.000000000000000000, 0.000000000000000000 ) ) ;
#22669 = CARTESIAN_POINT ( 'NONE',  ( 1.033464566929131356, 0.06523048226348168721, 1.419783464459401845 ) ) ;
#22670 = CIRCLE ( 'NONE', #2014, 0.4404574800679669777 ) ;
#22671 = CARTESIAN_POINT ( 'NONE',  ( 0.1787899950787401604, -0.4950787401037172186, -0.07405724077823318263 ) ) ;
#22672 = EDGE_CURVE ( 'NONE', #44801, #5491, #46863, .T. ) ;
#22673 = ADVANCED_FACE ( 'NONE', ( #33862 ), #11563, .T. ) ;
#22674 = CARTESIAN_POINT ( 'NONE',  ( -0.6971942568897637749, 2.189545951927499583E-17, 0.1648622046706460786 ) ) ;
#22675 = CARTESIAN_POINT ( 'NONE',  ( -0.8107537697050253289, -0.1574803149606297803, 0.8636811023622045225 ) ) ;
#22676 = CARTESIAN_POINT ( 'NONE',  ( 0.1270800023317771588, -1.000043809583045284, -0.1270800023317771588 ) ) ;
#22677 = CARTESIAN_POINT ( 'NONE',  ( 0.07669050334470198238, -0.2512157378938873475, -0.3110703821947682357 ) ) ;
#22678 = CARTESIAN_POINT ( 'NONE',  ( -0.8759842519685039353, 0.1574803149606299191, 1.505905511703495847 ) ) ;
#22679 = CARTESIAN_POINT ( 'NONE',  ( 0.6971942568897626646, -0.07405724077823297447, 0.8759842519147408302 ) ) ;
#22680 = CARTESIAN_POINT ( 'NONE',  ( 0.6971942568897648851, 0.07405724077823318263, 1.338582677111590069 ) ) ;
#22681 = CARTESIAN_POINT ( 'NONE',  ( 0.8759842519685039353, 0.1574803149606299191, 1.476377952755905554 ) ) ;
#22683 = CARTESIAN_POINT ( 'NONE',  ( 0.1574803149606299191, 0.1200787401574803237, 2.850509043694854679E-09 ) ) ;
#22682 = CARTESIAN_POINT ( 'NONE',  ( 0.7140868796910422311, 0.03190629090790177841, 1.982670689315033652 ) ) ;
#22684 = CARTESIAN_POINT ( 'NONE',  ( 0.9412147342319837628, 0.1574803149606300301, 0.3223425195775121432 ) ) ;
#22686 = CARTESIAN_POINT ( 'NONE',  ( -0.7185039370078746268, -0.06523048226347956391, 1.409940944881891367 ) ) ;
#22685 = CARTESIAN_POINT ( 'NONE',  ( 1.002407869896990045, 0.1264236179284866091, 0.8538385826234016207 ) ) ;
#22687 = CARTESIAN_POINT ( 'NONE',  ( 0.9500414927467377701, 0.1787899950787401604, 1.766732283410803239 ) ) ;
#22688 = CARTESIAN_POINT ( 'NONE',  ( 0.1264236179284866091, -0.7337598424659212970, 0.1264236179284866091 ) ) ;
#22689 = ORIENTED_EDGE ( 'NONE', *, *, #10414, .F. ) ;
#22690 = CARTESIAN_POINT ( 'NONE',  ( 0.9412147342319837628, -0.1574803149606297803, 0.4256889762704256230 ) ) ;
#22691 = CARTESIAN_POINT ( 'NONE',  ( -0.3161444924769509779, 2.559880088878760951, -3.648497683167374550 ) ) ;
#22692 = CARTESIAN_POINT ( 'NONE',  ( 1.002407869896990045, -0.1264236179284866091, 1.080216535379306952 ) ) ;
#22693 = DIRECTION ( 'NONE',  ( 1.000000000000000000, -4.402590611634445055E-17, 0.000000000000000000 ) ) ;
#22694 = CARTESIAN_POINT ( 'NONE',  ( 0.1574803149606300301, -1.698326771653543510, -0.06523048226347956391 ) ) ;
#22695 = CYLINDRICAL_SURFACE ( 'NONE', #35228, 0.02900000000000001882 ) ;
#22696 = VERTEX_POINT ( 'NONE', #30043 ) ;
#22697 = CYLINDRICAL_SURFACE ( 'NONE', #15258, 0.4724409448818900348 ) ;
#22698 = CARTESIAN_POINT ( 'NONE',  ( -0.8019270111902717657, 0.1787899950787401604, 0.2312992125446618197 ) ) ;
#22699 = CARTESIAN_POINT ( 'NONE',  ( -1.033464566929133799, 0.000000000000000000, 0.6003937007874016185 ) ) ;
#22700 = EDGE_LOOP ( 'NONE', ( #20240, #38225, #4759, #12717 ) ) ;
#22701 = CARTESIAN_POINT ( 'NONE',  ( 0.1264236179284866091, -1.486712598371433103, 0.1264236179284866091 ) ) ;
#22702 = CARTESIAN_POINT ( 'NONE',  ( -0.8759842519685039353, 0.1787899950787401882, 1.882381889710015743 ) ) ;
#22703 = CARTESIAN_POINT ( 'NONE',  ( -0.9500414927467377701, 0.1787899950787401604, 0.9350393700249758355 ) ) ;
#22704 = CARTESIAN_POINT ( 'NONE',  ( -1.054774247047244540, 0.07405724077823318263, 1.126968503883244654 ) ) ;
#22705 = CARTESIAN_POINT ( 'NONE',  ( -0.8019270111902717657, -0.1787899950787401604, 0.4478346456155276045 ) ) ;
#22706 = CARTESIAN_POINT ( 'NONE',  ( -0.7646288533564489232, -0.1113553986120547346, 0.1525590551181102428 ) ) ;
#22707 = DIRECTION ( 'NONE',  ( 0.000000000000000000, 0.000000000000000000, 1.000000000000000000 ) ) ;
#22708 = CARTESIAN_POINT ( 'NONE',  ( 0.1380782811756038342, 0.1289404906632452552, -0.09318370980563837891 ) ) ;
#22709 = CARTESIAN_POINT ( 'NONE',  ( 0.8019270111902717657, -0.1787899950787401604, 0.04921259837143338034 ) ) ;
#22710 = CARTESIAN_POINT ( 'NONE',  ( 0.1574803149606299191, 0.9876813667277579700, 0.7893767492247204531 ) ) ;
#22711 = CARTESIAN_POINT ( 'NONE',  ( -0.07405724077823318263, -0.5355570390953806603, -0.1787899950787401604 ) ) ;
#22712 = CARTESIAN_POINT ( 'NONE',  ( -0.002407869453279200614, -0.08955980254238483929, 0.2209030018291311126 ) ) ;
#22713 = FACE_OUTER_BOUND ( 'NONE', #32271, .T. ) ;
#22714 = CARTESIAN_POINT ( 'NONE',  ( -1.033464566929133799, 0.000000000000000000, 1.968503936900346529 ) ) ;
#22715 = CARTESIAN_POINT ( 'NONE',  ( -0.8759842519685039353, 0.1787899950787401882, 0.3075787401037169411 ) ) ;
#22716 = DIRECTION ( 'NONE',  ( 1.822029033848725028E-16, 0.000000000000000000, 1.000000000000000000 ) ) ;
#22717 = CARTESIAN_POINT ( 'NONE',  ( 0.2471915046495881119, -0.08339338023400436062, 0.06619788746988974903 ) ) ;
#22718 = ORIENTED_EDGE ( 'NONE', *, *, #8665, .T. ) ;
#22719 = EDGE_CURVE ( 'NONE', #43976, #40723, #25449, .T. ) ;
#22720 = CARTESIAN_POINT ( 'NONE',  ( -1.054774247047244540, -0.07405724077823318263, 1.560039370024976835 ) ) ;
#22721 = VERTEX_POINT ( 'NONE', #44588 ) ;
#22722 = CARTESIAN_POINT ( 'NONE',  ( -0.07405724077823318263, -1.336614173174582865, 0.1787899950787401604 ) ) ;
#22723 = CARTESIAN_POINT ( 'NONE',  ( -0.07405724077823318263, -1.567913385773008095, 0.1787899950787401604 ) ) ;
#22724 = VECTOR ( 'NONE', #10719, 39.37007874015748854 ) ;
#22725 = EDGE_CURVE ( 'NONE', #5360, #5716, #13203, .T. ) ;
#22726 = CARTESIAN_POINT ( 'NONE',  ( 0.7185039370078739607, 0.000000000000000000, 4.498031496062992574 ) ) ;
#22727 = FACE_OUTER_BOUND ( 'NONE', #35732, .T. ) ;
#22728 = CARTESIAN_POINT ( 'NONE',  ( 0.8107537697050253289, 0.1574803149606300301, 0.4945866141732282451 ) ) ;
#22729 = FACE_OUTER_BOUND ( 'NONE', #7274, .T. ) ;
#22730 = CARTESIAN_POINT ( 'NONE',  ( -0.8107537697050253289, -0.1574803149606297803, 1.090059055010582423 ) ) ;
#22731 = CARTESIAN_POINT ( 'NONE',  ( 0.6971942568897626646, 0.07405724077823318263, 0.5561023621509617598 ) ) ;
#22732 = CARTESIAN_POINT ( 'NONE',  ( 0.4736248074375818407, 0.4457451269443653552, -1.671447902550338815 ) ) ;
#22733 = CARTESIAN_POINT ( 'NONE',  ( -0.1574803149606299191, -0.3031496062992126150, 0.000000000000000000 ) ) ;
#22734 = CARTESIAN_POINT ( 'NONE',  ( 0.9873396505805591694, -0.1113553986120547346, 1.963582677057826853 ) ) ;
#22735 = ORIENTED_EDGE ( 'NONE', *, *, #43445, .F. ) ;
#22736 = DIRECTION ( 'NONE',  ( 0.000000000000000000, 0.000000000000000000, 1.000000000000000000 ) ) ;
#22737 = CARTESIAN_POINT ( 'NONE',  ( -1.054774247047244540, -0.07405724077823318263, 0.8907480314422985268 ) ) ;
#22738 = CARTESIAN_POINT ( 'NONE',  ( 0.7185039370078746268, 0.06523048226347956391, 0.8932086614173218031 ) ) ;
#22739 = CARTESIAN_POINT ( 'NONE',  ( -0.4620708661417322616, 0.000000000000000000, -1.186023622047243986 ) ) ;
#22741 = CARTESIAN_POINT ( 'NONE',  ( 1.033464566929133799, 0.000000000000000000, 1.545275590551181244 ) ) ;
#22740 = LINE ( 'NONE', #16046, #19418 ) ;
#22742 = CARTESIAN_POINT ( 'NONE',  ( -0.1677420379284152441, -0.08956119648846384840, 0.01551656620580007390 ) ) ;
#22743 = ORIENTED_EDGE ( 'NONE', *, *, #20943, .T. ) ;
#22744 = DIRECTION ( 'NONE',  ( 0.000000000000000000, 0.000000000000000000, 1.000000000000000000 ) ) ;
#22745 = ORIENTED_EDGE ( 'NONE', *, *, #20363, .F. ) ;
#22746 = CARTESIAN_POINT ( 'NONE',  ( -0.1179171413540952840, 0.09842519685039383126, -0.2173535775632838007 ) ) ;
#22747 = CARTESIAN_POINT ( 'NONE',  ( 0.7185039370078714072, 0.06523048226347728795, 1.158956692805858779 ) ) ;
#22748 = CARTESIAN_POINT ( 'NONE',  ( 0.1264236179284866091, -1.521161417269070837, 0.1264236179284866091 ) ) ;
#22749 = CARTESIAN_POINT ( 'NONE',  ( -0.1787899950787401882, -0.8321850393163149340, 0.000000000000000000 ) ) ;
#22750 = CARTESIAN_POINT ( 'NONE',  ( -0.1574803149606297803, -1.206200787401574770, 0.06523048226347956391 ) ) ;
#22751 = CARTESIAN_POINT ( 'NONE',  ( 0.8107537697050253289, -0.1574803149606297803, 1.090059055010582423 ) ) ;
#22752 = ( BOUNDED_CURVE ( )  B_SPLINE_CURVE ( 2, ( #42672, #16826, #17062, #31467, #31703, #23789, #12785, #35531, #30776 ),
 .UNSPECIFIED., .F., .T. ) 
 B_SPLINE_CURVE_WITH_KNOTS ( ( 3, 2, 2, 2, 3 ),
 ( 0.07000000000000000666, 0.07249999999999999500, 0.07499999999999999722, 0.07749999999999999944, 0.08000000000000000167 ),
 .UNSPECIFIED. ) 
 CURVE ( )  GEOMETRIC_REPRESENTATION_ITEM ( )  RATIONAL_B_SPLINE_CURVE ( ( 1.000000000000000000, 0.9238795325112869605, 1.000000000000000000, 0.9238795325112869605, 1.000000000000000000, 0.9238795325112869605, 1.000000000000000000, 0.9238795325112869605, 1.000000000000000000 ) ) 
 REPRESENTATION_ITEM ( '' )  ) ;
#22753 = CARTESIAN_POINT ( 'NONE',  ( -0.9873396505805591694, -0.1113553986120547346, 1.658464566929134021 ) ) ;
#22754 = CARTESIAN_POINT ( 'NONE',  ( -1.054774247047244540, -0.07405724077823318263, 0.4921259841982048577 ) ) ;
#22755 = ORIENTED_EDGE ( 'NONE', *, *, #37677, .T. ) ;
#22756 = VERTEX_POINT ( 'NONE', #18274 ) ;
#22757 = CARTESIAN_POINT ( 'NONE',  ( -0.6971942568897648851, 0.07405724077823318263, 1.737204724355685848 ) ) ;
#22758 = CARTESIAN_POINT ( 'NONE',  ( 0.6971942568897637749, 2.189545951927499583E-17, 1.660925196796630088 ) ) ;
#22759 = CARTESIAN_POINT ( 'NONE',  ( -0.09011016336854826836, -0.2434714151301908824, -0.3128311589625485389 ) ) ;
#22760 = CARTESIAN_POINT ( 'NONE',  ( 0.9500414927467378812, 0.1787899950787401604, 0.2706692912848194243 ) ) ;
#22761 = FACE_OUTER_BOUND ( 'NONE', #17169, .T. ) ;
#22762 = CARTESIAN_POINT ( 'NONE',  ( -1.002407869896990045, -0.1264236179284866091, 1.277066929080094448 ) ) ;
#22763 = VECTOR ( 'NONE', #37255, 39.37007874015748143 ) ;
#22764 = CARTESIAN_POINT ( 'NONE',  ( -0.8019270111902717657, 0.1787899950787401604, 0.1181102361667090567 ) ) ;
#22765 = CARTESIAN_POINT ( 'NONE',  ( 0.000000000000000000, 0.9876813667277579700, 0.7893767492247204531 ) ) ;
#22766 = CARTESIAN_POINT ( 'NONE',  ( -1.054774247047244096, 0.000000000000000000, 1.523129921206078707 ) ) ;
#22767 = ORIENTED_EDGE ( 'NONE', *, *, #37009, .T. ) ;
#22768 = CARTESIAN_POINT ( 'NONE',  ( -0.8759842519685039353, -0.1574803149606299191, 1.535433070866141669 ) ) ;
#22769 = CARTESIAN_POINT ( 'NONE',  ( 0.7185039370078739607, 1.928577636452523993E-17, 0.8858267715460158565 ) ) ;
#22770 = CARTESIAN_POINT ( 'NONE',  ( 1.054774247047244540, -0.07405724077823318263, 1.560039370024976835 ) ) ;
#22771 = CARTESIAN_POINT ( 'NONE',  ( -0.2160651621502015785, -0.09842519685039370636, -0.1192374171493116308 ) ) ;
#22772 = DIRECTION ( 'NONE',  ( 0.000000000000000000, 0.000000000000000000, -1.000000000000000000 ) ) ;
#22773 = CARTESIAN_POINT ( 'NONE',  ( -0.2559098255137246536, 0.02501923667458835418, -0.3142646454376785137 ) ) ;
#22774 = ORIENTED_EDGE ( 'NONE', *, *, #38591, .F. ) ;
#22775 = EDGE_CURVE ( 'NONE', #30092, #39149, #18731, .T. ) ;
#22776 = DIMENSIONAL_EXPONENTS ( 1.000000000000000000, 0.000000000000000000, 0.000000000000000000, 0.000000000000000000, 0.000000000000000000, 0.000000000000000000, 0.000000000000000000 ) ;
#22777 = EDGE_LOOP ( 'NONE', ( #25350, #21113, #9747, #34688 ) ) ;
#22778 = EDGE_CURVE ( 'NONE', #1638, #23930, #8195, .T. ) ;
#22779 = CARTESIAN_POINT ( 'NONE',  ( -0.9500414927467377701, -0.1787899950787401604, 1.161417322780881278 ) ) ;
#22780 = VERTEX_POINT ( 'NONE', #21877 ) ;
#22781 = CARTESIAN_POINT ( 'NONE',  ( -0.1787899950787401604, -0.8297244093950564281, 0.07405724077823318263 ) ) ;
#22782 = CARTESIAN_POINT ( 'NONE',  ( -0.1787899950787401604, -1.065944881836000224, -0.07405724077823318263 ) ) ;
#22783 = AXIS2_PLACEMENT_3D ( 'NONE', #22626, #22379, #333 ) ;
#22784 = LINE ( 'NONE', #10845, #10252 ) ;
#22785 = SHAPE_REPRESENTATION_RELATIONSHIP ( 'NONE' , 'NONE' ,  #43589, #7828 ) ;
#22786 = CARTESIAN_POINT ( 'NONE',  ( 0.6971942568897648851, -0.07405724077823297447, 1.815944881835999558 ) ) ;
#22787 = CARTESIAN_POINT ( 'NONE',  ( 0.07444174185955065859, -0.3430556206066676106, 0.1797182628040039087 ) ) ;
#22788 = CARTESIAN_POINT ( 'NONE',  ( -0.1574803149606300301, 0.08809055118110237226, -0.06523048226347956391 ) ) ;
#22789 = CARTESIAN_POINT ( 'NONE',  ( 3.284318927891251994E-17, -0.1530511810485986057, 0.1787899950787401882 ) ) ;
#22790 = LINE ( 'NONE', #33844, #14624 ) ;
#22791 = CARTESIAN_POINT ( 'NONE',  ( 0.8019270111902717657, -0.1787899950787401604, 0.7185039369541108556 ) ) ;
#22792 = CIRCLE ( 'NONE', #18948, 0.1013779527559039162 ) ;
#22794 = PLANE ( 'NONE',  #17752 ) ;
#22793 = CARTESIAN_POINT ( 'NONE',  ( -0.8759842519685039353, -0.1574803149606299191, 1.564960629813732185 ) ) ;
#22795 = CARTESIAN_POINT ( 'NONE',  ( -0.1184675242425147629, 0.3740157480314960647, 1.713085361781126803 ) ) ;
#22796 = CARTESIAN_POINT ( 'NONE',  ( 0.7185039370078746268, 0.06523048226347956391, 0.4601377952755902889 ) ) ;
#22797 = CARTESIAN_POINT ( 'NONE',  ( 0.9500414927467378812, 0.1787899950787401604, 1.766732283410803461 ) ) ;
#22798 = DIRECTION ( 'NONE',  ( 1.822029033848725028E-16, 0.000000000000000000, 1.000000000000000000 ) ) ;
#22799 = CARTESIAN_POINT ( 'NONE',  ( -1.094772975963752103E-17, -0.2121062991588350544, -0.1787899950787401882 ) ) ;
#22800 = CARTESIAN_POINT ( 'NONE',  ( 1.033464566929134687, 0.06523048226347956391, 0.4749015746956221085 ) ) ;
#22801 = CARTESIAN_POINT ( 'NONE',  ( -0.1264236179284866091, -1.225885826717889815, -0.1264236179284866091 ) ) ;
#22802 = CARTESIAN_POINT ( 'NONE',  ( 0.8019270111902717657, 0.1787899950787401604, 0.2362204723871814960 ) ) ;
#22803 = CARTESIAN_POINT ( 'NONE',  ( 0.9873396505805591694, 0.1113553986120547346, 0.05413385826771653642 ) ) ;
#22804 = CARTESIAN_POINT ( 'NONE',  ( -0.8019270111902717657, -0.1787899950787401604, 1.820866141678520789 ) ) ;
#22805 = ORIENTED_EDGE ( 'NONE', *, *, #35133, .T. ) ;
#22806 = CARTESIAN_POINT ( 'NONE',  ( -0.6971942568897648851, 0.07405724077823318263, 1.264763779473795813 ) ) ;
#22807 = DIRECTION ( 'NONE',  ( 0.000000000000000000, -0.2432573283306819767, 0.9699617890481142535 ) ) ;
#22808 = CARTESIAN_POINT ( 'NONE',  ( 0.9500414927467378812, 0.1787899950787401604, 0.03444881884387430981 ) ) ;
#22809 = CARTESIAN_POINT ( 'NONE',  ( -0.7495606340400177148, 0.1264236179284866091, 1.060531496009228247 ) ) ;
#22810 = DIRECTION ( 'NONE',  ( 1.000000000000000000, 0.000000000000000000, 0.000000000000000000 ) ) ;
#22811 = CARTESIAN_POINT ( 'NONE',  ( 0.1582120475477782062, 0.1402876732178915120, -0.03788922412827557679 ) ) ;
#22812 = DIRECTION ( 'NONE',  ( 0.000000000000000000, 0.000000000000000000, 1.000000000000000000 ) ) ;
#22813 = CARTESIAN_POINT ( 'NONE',  ( 0.6971942568897648851, -0.07405724077823297447, 0.4429133857730084833 ) ) ;
#22814 = CARTESIAN_POINT ( 'NONE',  ( -0.8759842519685039353, 0.1787899950787401882, 0.4650590550643464716 ) ) ;
#22815 = CARTESIAN_POINT ( 'NONE',  ( 0.8759842519685039353, 0.1574803149606299191, 1.702755905404283565 ) ) ;
#22816 = ORIENTED_EDGE ( 'NONE', *, *, #34489, .F. ) ;
#22817 = VECTOR ( 'NONE', #27797, 39.37007874015748854 ) ;
#22818 = DIRECTION ( 'NONE',  ( 0.000000000000000000, 0.1045284632676499320, -0.9945218953682736229 ) ) ;
#22819 = ORIENTED_EDGE ( 'NONE', *, *, #7149, .F. ) ;
#22820 = CARTESIAN_POINT ( 'NONE',  ( 0.7495606340400177148, -0.1264236179284866091, 0.9178149605761574126 ) ) ;
#22821 = CARTESIAN_POINT ( 'NONE',  ( -1.033464566929133799, 0.000000000000000000, 0.08858267716535432601 ) ) ;
#22822 = CARTESIAN_POINT ( 'NONE',  ( 0.7495606340400177148, -0.1264236179284866091, 1.193405511757259951 ) ) ;
#22823 = CARTESIAN_POINT ( 'NONE',  ( -0.2246256911002503798, -0.09851385142897184366, -0.1004183578296887897 ) ) ;
#22824 = ORIENTED_EDGE ( 'NONE', *, *, #39682, .T. ) ;
#22825 = EDGE_CURVE ( 'NONE', #44147, #13283, #32917, .T. ) ;
#22826 = CARTESIAN_POINT ( 'NONE',  ( 0.5660731898098425585, -0.09842519685039370636, 1.205361022782828805E-17 ) ) ;
#22827 = CARTESIAN_POINT ( 'NONE',  ( -1.054774247047244096, 0.000000000000000000, 0.8932086613635591421 ) ) ;
#22828 = EDGE_CURVE ( 'NONE', #1170, #18061, #33160, .T. ) ;
#22829 = CARTESIAN_POINT ( 'NONE',  ( 0.1588150004738562715, -0.09138854459949809217, -0.1173009487050077904 ) ) ;
#22830 = CARTESIAN_POINT ( 'NONE',  ( 1.033464566929133799, 0.000000000000000000, 0.7972440944881890035 ) ) ;
#22831 = CARTESIAN_POINT ( 'NONE',  ( 0.1787899950787401882, -1.492742078465458810, -2.189545951927503898E-17 ) ) ;
#22832 = ORIENTED_EDGE ( 'NONE', *, *, #30191, .F. ) ;
#22833 = CARTESIAN_POINT ( 'NONE',  ( -0.4330708661417356775, 0.000000000000000000, -1.186023622047243986 ) ) ;
#22834 = CARTESIAN_POINT ( 'NONE',  ( 0.07405724077823318263, -0.4852362204186770889, -0.1787899950787401604 ) ) ;
#22835 = EDGE_CURVE ( 'NONE', #23380, #5132, #33125, .T. ) ;
#22836 = CYLINDRICAL_SURFACE ( 'NONE', #42235, 0.8366141732283466359 ) ;
#22837 = VERTEX_POINT ( 'NONE', #34795 ) ;
#22838 = CARTESIAN_POINT ( 'NONE',  ( 1.054774247047244540, 0.07405724077823318263, 1.284448818843874740 ) ) ;
#22839 = ADVANCED_FACE ( 'NONE', ( #45060 ), #1935, .T. ) ;
#22840 = PLANE ( 'NONE',  #19491 ) ;
#22841 = CARTESIAN_POINT ( 'NONE',  ( -0.1377952755905511861, 0.1574803149606320007, 0.8070866141732283561 ) ) ;
#22842 = B_SPLINE_CURVE_WITH_KNOTS ( 'NONE', 3,
 ( #14727, #25031, #29400, #25535, #7519 ),
 .UNSPECIFIED., .F., .F.,
 ( 4, 1, 4 ),
 ( 0.000000000000000000, 0.002020725942163694843, 0.004041451884327384482 ),
 .UNSPECIFIED. ) ;
#22843 = CARTESIAN_POINT ( 'NONE',  ( 0.01035225325197390578, -0.08294251416999544324, -0.1319299025311632956 ) ) ;
#22844 = CARTESIAN_POINT ( 'NONE',  ( 0.7495606340400177148, -0.1264236179284866091, 0.1648622046706460786 ) ) ;
#22845 = CARTESIAN_POINT ( 'NONE',  ( -0.1787899950787401604, -1.735236220418678643, 0.07405724077823318263 ) ) ;
#22846 = CARTESIAN_POINT ( 'NONE',  ( -0.1264236179284866091, -1.737696850339937038, -0.1264236179284866091 ) ) ;
#22847 = DIRECTION ( 'NONE',  ( -0.5938482344758516662, -2.107288435035759121E-16, 0.8045770779794275684 ) ) ;
#22848 = CARTESIAN_POINT ( 'NONE',  ( 1.181102362204724310, -0.3937007874015748254, 0.9842519685039370358 ) ) ;
#22849 = CARTESIAN_POINT ( 'NONE',  ( -0.8759842519685039353, 0.1787899950787401882, 0.5880905511273386566 ) ) ;
#22850 = AXIS2_PLACEMENT_3D ( 'NONE', #2512, #35601, #13327 ) ;
#22851 = CARTESIAN_POINT ( 'NONE',  ( -0.1574803149606300301, -0.6993110236220480003, -0.06523048226347956391 ) ) ;
#22852 = CARTESIAN_POINT ( 'NONE',  ( 0.1270800023317771588, -1.403587116669659407, 0.1270800023317771588 ) ) ;
#22853 = CARTESIAN_POINT ( 'NONE',  ( 0.8759842519685039353, 0.000000000000000000, 4.498031496062992574 ) ) ;
#22854 = LINE ( 'NONE', #19725, #37589 ) ;
#22855 = CARTESIAN_POINT ( 'NONE',  ( 1.054774247047244540, 0.07405724077823318263, 1.407480314906865981 ) ) ;
#22856 = CARTESIAN_POINT ( 'NONE',  ( 0.8759842519685039353, -0.1787899950787401882, 1.862696850339937038 ) ) ;
#22857 = CARTESIAN_POINT ( 'NONE',  ( 0.6971942568897626646, 0.07405724077823318263, 0.2755905511273391006 ) ) ;
#22858 = CIRCLE ( 'NONE', #13685, 0.08090551181102362266 ) ;
#22860 = EDGE_LOOP ( 'NONE', ( #11159, #9999, #8267, #10275 ) ) ;
#22859 = FACE_OUTER_BOUND ( 'NONE', #34603, .T. ) ;
#22861 = CARTESIAN_POINT ( 'NONE',  ( 0.000000000000000000, 0.000000000000000000, 0.09842519685039370636 ) ) ;
#22862 = CARTESIAN_POINT ( 'NONE',  ( 1.033464566929133799, 1.928577636452524610E-17, 2.007874015640504162 ) ) ;
#22863 = CARTESIAN_POINT ( 'NONE',  ( -0.8759842519685039353, -0.1574803149606299191, 1.023622047244094446 ) ) ;
#22864 = CARTESIAN_POINT ( 'NONE',  ( 0.2397010884053811242, 4.466152701071653354E-17, 0.000000000000000000 ) ) ;
#22865 = VECTOR ( 'NONE', #12664, 39.37007874015748143 ) ;
#22866 = CARTESIAN_POINT ( 'NONE',  ( 0.6971942568897626646, 0.07405724077823318263, 0.3543307086076538659 ) ) ;
#22867 = CARTESIAN_POINT ( 'NONE',  ( 0.7328829063313654357, -0.08888254389784847054, 0.03937018366421114746 ) ) ;
#22868 = CARTESIAN_POINT ( 'NONE',  ( 1.033464566929133799, 0.000000000000000000, 0.8661417321759370402 ) ) ;
#22869 = CARTESIAN_POINT ( 'NONE',  ( 1.033464566929133799, 0.000000000000000000, 0.03937007863263043694 ) ) ;
#22870 = CARTESIAN_POINT ( 'NONE',  ( -0.7185039370078739607, 1.928577636452523993E-17, 1.289370078740157632 ) ) ;
#22871 = CARTESIAN_POINT ( 'NONE',  ( -1.054774247047244540, -0.07405724077823318263, 1.279527559001355286 ) ) ;
#22872 = CARTESIAN_POINT ( 'NONE',  ( 0.9873396505805591694, 0.1113553986120547346, 0.5954724408373543998 ) ) ;
#22873 = EDGE_LOOP ( 'NONE', ( #15535, #30967, #13994, #38016 ) ) ;
#22874 = CARTESIAN_POINT ( 'NONE',  ( 0.8107537697050254399, 0.1574803149606300301, 1.400098425196850904 ) ) ;
#22875 = CARTESIAN_POINT ( 'NONE',  ( 0.7185039370078739607, 1.928577636452523993E-17, 0.6988188976377952555 ) ) ;
#22876 = VERTEX_POINT ( 'NONE', #12522 ) ;
#22877 = CARTESIAN_POINT ( 'NONE',  ( 0.1270800023317771588, 0.01373571797600956802, 0.1270800023317771588 ) ) ;
#22878 = CARTESIAN_POINT ( 'NONE',  ( -0.1264236179284866091, -1.181594488135212506, 0.1264236179284866091 ) ) ;
#22879 = DIRECTION ( 'NONE',  ( 0.000000000000000000, 1.000000000000000000, 0.000000000000000000 ) ) ;
#22880 = CARTESIAN_POINT ( 'NONE',  ( -0.9873396505805591694, 0.1113553986120547346, 1.195866141732283561 ) ) ;
#22881 = CARTESIAN_POINT ( 'NONE',  ( 0.1574803149606299746, -0.09842519685039370636, 1.713085361781126803 ) ) ;
#22883 = CARTESIAN_POINT ( 'NONE',  ( -0.8759842519685039353, 0.1574803149606299191, 0.7578740156405039397 ) ) ;
#22882 = CARTESIAN_POINT ( 'NONE',  ( -0.06523048226347956391, 0.04379921259842517456, -0.1574803149606300301 ) ) ;
#22884 = CARTESIAN_POINT ( 'NONE',  ( 0.7185039370078739607, 1.928577636452523993E-17, 1.318897637687747926 ) ) ;
#22885 = EDGE_LOOP ( 'NONE', ( #16962, #19816, #2114, #42175 ) ) ;
#22886 = CARTESIAN_POINT ( 'NONE',  ( -0.03837864586579538273, -0.06712557525760225186, -0.2632749781601607109 ) ) ;
#22887 = CARTESIAN_POINT ( 'NONE',  ( 0.6971942568897626646, 0.07405724077823318263, 0.6742125983714335469 ) ) ;
#22888 = CARTESIAN_POINT ( 'NONE',  ( 1.054774247047244540, 0.07405724077823318263, 0.9744094487651340231 ) ) ;
#22889 = CARTESIAN_POINT ( 'NONE',  ( -0.8759842519685039353, -0.1787899950787401882, 1.508366141678519678 ) ) ;
#22890 = CARTESIAN_POINT ( 'NONE',  ( 0.1113553986120547346, -0.03248031485310291788, -0.1113553986120547346 ) ) ;
#22891 = CARTESIAN_POINT ( 'NONE',  ( -0.9500414927467378812, 0.1787899950787401604, 1.215551181048599272 ) ) ;
#22892 = ORIENTED_EDGE ( 'NONE', *, *, #19482, .F. ) ;
#22893 = ADVANCED_FACE ( 'NONE', ( #15874 ), #9382, .F. ) ;
#22894 = VECTOR ( 'NONE', #40517, 39.37007874015748143 ) ;
#22895 = CARTESIAN_POINT ( 'NONE',  ( -0.7495606340400177148, 0.1264236179284866091, 0.3567913385289137596 ) ) ;
#22896 = FACE_OUTER_BOUND ( 'NONE', #34458, .T. ) ;
#22897 = CARTESIAN_POINT ( 'NONE',  ( 0.3425196850393700809, -0.08090551181102362266, 0.000000000000000000 ) ) ;
#22898 = CARTESIAN_POINT ( 'NONE',  ( 0.1787899950787401604, -0.9391003461819946718, -0.07405724077823318263 ) ) ;
#22899 = ORIENTED_EDGE ( 'NONE', *, *, #45207, .F. ) ;
#22900 = VERTEX_POINT ( 'NONE', #24002 ) ;
#22901 = ADVANCED_FACE ( 'NONE', ( #41696 ), #5775, .T. ) ;
#22902 = CARTESIAN_POINT ( 'NONE',  ( 0.004714672091284868166, -0.04816527795631998093, 0.1377938255964467340 ) ) ;
#22903 = CONICAL_SURFACE ( 'NONE', #30595, 0.09842519685039370636, 0.9599310885968824758 ) ;
#22904 = LINE ( 'NONE', #4916, #37595 ) ;
#22905 = ( BOUNDED_CURVE ( )  B_SPLINE_CURVE ( 2, ( #30106, #12095, #37006, #44640, #7529, #22146, #22629, #14984, #29637 ),
 .UNSPECIFIED., .F., .T. ) 
 B_SPLINE_CURVE_WITH_KNOTS ( ( 3, 2, 2, 2, 3 ),
 ( 0.2500000000000000000, 0.2525000000000000022, 0.2550000000000000044, 0.2575000000000000067, 0.2600000000000000089 ),
 .UNSPECIFIED. ) 
 CURVE ( )  GEOMETRIC_REPRESENTATION_ITEM ( )  RATIONAL_B_SPLINE_CURVE ( ( 1.000000000000000000, 0.9238795325112859613, 1.000000000000000000, 0.9238795325112869605, 1.000000000000000000, 0.9238795325112869605, 1.000000000000000000, 0.9238795325112869605, 1.000000000000000000 ) ) 
 REPRESENTATION_ITEM ( '' )  ) ;
#22906 = CARTESIAN_POINT ( 'NONE',  ( -0.2066929133858267931, 0.7443365962042343131, -3.964450923140766303 ) ) ;
#22907 = CARTESIAN_POINT ( 'NONE',  ( 0.1787899950787401882, -0.5369094487651339120, -2.189545951927503898E-17 ) ) ;
#22908 = CARTESIAN_POINT ( 'NONE',  ( -1.002407869896990045, -0.1264236179284866091, 0.2583661416785200671 ) ) ;
#22909 = CARTESIAN_POINT ( 'NONE',  ( -0.8107537697050253289, 0.1574803149606300301, 0.8095472440944886383 ) ) ;
#22910 = CARTESIAN_POINT ( 'NONE',  ( -0.1797182628040039365, -0.9459099513153288452, 0.000000000000000000 ) ) ;
#22911 = CARTESIAN_POINT ( 'NONE',  ( 0.2066929133858268486, 0.07021257666614924564, -0.1553045758542777877 ) ) ;
#22912 = CARTESIAN_POINT ( 'NONE',  ( -0.7185039370078739607, 1.928577636452523993E-17, 1.555118110128692832 ) ) ;
#22913 = CARTESIAN_POINT ( 'NONE',  ( 0.6971942568897637749, 2.189545951927499583E-17, 0.9522637794737952577 ) ) ;
#22914 = CARTESIAN_POINT ( 'NONE',  ( 1.054774247047244540, -0.07405724077823318263, 1.358267716481669662 ) ) ;
#22915 = LINE ( 'NONE', #22437, #33050 ) ;
#22916 = CARTESIAN_POINT ( 'NONE',  ( 1.033464566929134687, -0.06523048226347956391, 1.424704724409449064 ) ) ;
#22917 = CARTESIAN_POINT ( 'NONE',  ( 0.7395153858165040006, 0.08906846876865334717, 1.981445972419700885 ) ) ;
#22918 = CARTESIAN_POINT ( 'NONE',  ( 0.1476377952755906220, 0.2512968553230415791, -0.3092734567177705673 ) ) ;
#22919 = ( BOUNDED_CURVE ( )  B_SPLINE_CURVE ( 2, ( #12782, #12313, #41482, #34352, #1484, #16141, #15596, #44782, #29764 ),
 .UNSPECIFIED., .F., .T. ) 
 B_SPLINE_CURVE_WITH_KNOTS ( ( 3, 2, 2, 2, 3 ),
 ( 0.7199999999999999734, 0.7225000000000000311, 0.7249999999999999778, 0.7275000000000000355, 0.7299999999999999822 ),
 .UNSPECIFIED. ) 
 CURVE ( )  GEOMETRIC_REPRESENTATION_ITEM ( )  RATIONAL_B_SPLINE_CURVE ( ( 1.000000000000000000, 0.9238795325112869605, 1.000000000000000000, 0.9238795325112869605, 1.000000000000000000, 0.9238795325112869605, 1.000000000000000000, 0.9238795325112799661, 1.000000000000000000 ) ) 
 REPRESENTATION_ITEM ( '' )  ) ;
#22920 = DIRECTION ( 'NONE',  ( -1.000000000000000000, 3.469446951953614189E-15, 1.144917494144692682E-16 ) ) ;
#22921 = CARTESIAN_POINT ( 'NONE',  ( 1.002407869896990045, -0.1264236179284866091, 0.8833661416785196785 ) ) ;
#22922 = CARTESIAN_POINT ( 'NONE',  ( 1.002407869896990045, -0.1264236179284866091, 1.793799212544661348 ) ) ;
#22923 = CARTESIAN_POINT ( 'NONE',  ( -0.1787899950787401882, -0.7878937007336378473, 0.000000000000000000 ) ) ;
#22925 = ( BOUNDED_CURVE ( )  B_SPLINE_CURVE ( 2, ( #46097, #31749, #17579, #46806, #42491, #13519, #35798, #32221, #31978 ),
 .UNSPECIFIED., .F., .T. ) 
 B_SPLINE_CURVE_WITH_KNOTS ( ( 3, 2, 2, 2, 3 ),
 ( 0.8800000000000000044, 0.8824999999999999512, 0.8850000000000000089, 0.8874999999999999556, 0.8900000000000000133 ),
 .UNSPECIFIED. ) 
 CURVE ( )  GEOMETRIC_REPRESENTATION_ITEM ( )  RATIONAL_B_SPLINE_CURVE ( ( 1.000000000000000000, 0.9238795325112869605, 1.000000000000000000, 0.9238795325112869605, 1.000000000000000000, 0.9238795325112869605, 1.000000000000000000, 0.9238795325112829637, 1.000000000000000000 ) ) 
 REPRESENTATION_ITEM ( '' )  ) ;
#22924 = CARTESIAN_POINT ( 'NONE',  ( -0.6195511811023656223, 0.6102362204724408601, 0.5167322834645649010 ) ) ;
#22926 = ORIENTED_EDGE ( 'NONE', *, *, #33834, .F. ) ;
#22927 = CARTESIAN_POINT ( 'NONE',  ( 1.033464566929133799, 0.000000000000000000, 0.4330708660342047489 ) ) ;
#22928 = FACE_OUTER_BOUND ( 'NONE', #42544, .T. ) ;
#22929 = CARTESIAN_POINT ( 'NONE',  ( 0.06523048226347956391, -1.604822834538142784, -0.1574803149606300301 ) ) ;
#22930 = CARTESIAN_POINT ( 'NONE',  ( -1.033464566929133799, 0.000000000000000000, 0.1181102361129454797 ) ) ;
#22931 = CARTESIAN_POINT ( 'NONE',  ( 0.8019270111902717657, 0.1787899950787401604, 1.215551181048599272 ) ) ;
#22932 = FACE_OUTER_BOUND ( 'NONE', #16934, .T. ) ;
#22934 = VECTOR ( 'NONE', #16871, 39.37007874015748143 ) ;
#22933 = CARTESIAN_POINT ( 'NONE',  ( 0.1574803149606299191, -1.700787401574803237, -1.928577636452523993E-17 ) ) ;
#22935 = CARTESIAN_POINT ( 'NONE',  ( 0.4330708661417329020, 0.1864803149606300281, -1.186023622047243986 ) ) ;
#22936 = EDGE_LOOP ( 'NONE', ( #29475, #44565, #32044, #37156, #14543, #20534 ) ) ;
#22937 = DIRECTION ( 'NONE',  ( -1.000000000000000000, 0.000000000000000000, -0.000000000000000000 ) ) ;
#22938 = CARTESIAN_POINT ( 'NONE',  ( -1.002407869896990045, 0.1264236179284866091, 0.2239173227808822775 ) ) ;
#22939 = ORIENTED_EDGE ( 'NONE', *, *, #34652, .F. ) ;
#22940 = CARTESIAN_POINT ( 'NONE',  ( 0.1574803149606299191, 1.928577636452524610E-17, -0.2748405511811023438 ) ) ;
#22941 = ( REPRESENTATION_RELATIONSHIP ('NONE','NONE', #9609, #14237 ) REPRESENTATION_RELATIONSHIP_WITH_TRANSFORMATION ( #17068 )SHAPE_REPRESENTATION_RELATIONSHIP( ) ) ;
#22943 = CARTESIAN_POINT ( 'NONE',  ( -0.1787899950787401882, -1.580216535379306952, 0.000000000000000000 ) ) ;
#22942 = CARTESIAN_POINT ( 'NONE',  ( 0.1574803149606300301, -0.3499015746956224415, -0.06523048226347956391 ) ) ;
#22944 = CARTESIAN_POINT ( 'NONE',  ( -0.8019270111902717657, 0.1787899950787401604, 1.766732283410803461 ) ) ;
#22945 = CARTESIAN_POINT ( 'NONE',  ( -1.002407869896990045, -0.1264236179284866091, 0.9621062991588346103 ) ) ;
#22946 = CARTESIAN_POINT ( 'NONE',  ( -0.7495606340400177148, -0.1264236179284866091, 0.5634842519147401640 ) ) ;
#22947 = ADVANCED_FACE ( 'NONE', ( #34724 ), #12445, .F. ) ;
#22948 = DIRECTION ( 'NONE',  ( 1.000000000000000000, 0.000000000000000000, -0.000000000000000000 ) ) ;
#22949 = DIRECTION ( 'NONE',  ( 0.000000000000000000, 0.000000000000000000, 1.000000000000000000 ) ) ;
#22950 = FACE_OUTER_BOUND ( 'NONE', #38338, .T. ) ;
#22951 = DIRECTION ( 'NONE',  ( 0.000000000000000000, 0.000000000000000000, 1.000000000000000000 ) ) ;
#22952 = CARTESIAN_POINT ( 'NONE',  ( 0.07405724077823318263, -0.6192184564182152684, -0.1787899950787401604 ) ) ;
#22953 = CARTESIAN_POINT ( 'NONE',  ( 0.07190187720976377872, -0.08956013875575118133, 0.2047185321618893994 ) ) ;
#22954 = DIRECTION ( 'NONE',  ( 0.000000000000000000, -0.9771240687918556489, -0.2126700594527800303 ) ) ;
#22955 = LINE ( 'NONE', #19349, #38652 ) ;
#22956 = EDGE_CURVE ( 'NONE', #7313, #42075, #23500, .T. ) ;
#22957 = CARTESIAN_POINT ( 'NONE',  ( 0.000000000000000000, -0.09842519685039370636, 0.000000000000000000 ) ) ;
#22958 = CARTESIAN_POINT ( 'NONE',  ( -0.9500414927467378812, 0.1787899950787401604, 0.4625984251430869665 ) ) ;
#22959 = CARTESIAN_POINT ( 'NONE',  ( 2.892866454678787531E-17, -0.007874015640504449659, 0.1574803149606299191 ) ) ;
#22960 = AXIS2_PLACEMENT_3D ( 'NONE', #13120, #9510, #20517 ) ;
#22961 = DIRECTION ( 'NONE',  ( -1.000000000000000000, 0.000000000000000000, 0.000000000000000000 ) ) ;
#22962 = CARTESIAN_POINT ( 'NONE',  ( -0.7495606340400177148, 0.1264236179284866091, 1.537893700733637736 ) ) ;
#22963 = ORIENTED_EDGE ( 'NONE', *, *, #24304, .T. ) ;
#22964 = CARTESIAN_POINT ( 'NONE',  ( -0.07405724077823318263, -1.272637795221826629, -0.1787899950787401604 ) ) ;
#22965 = CARTESIAN_POINT ( 'NONE',  ( 0.1787899950787401604, -1.474409448765133801, -0.07405724077823318263 ) ) ;
#22966 = CARTESIAN_POINT ( 'NONE',  ( 1.033464566929134687, -0.06523048226347956391, 0.2042322834645668717 ) ) ;
#22967 = LINE ( 'NONE', #12192, #44518 ) ;
#22968 = CARTESIAN_POINT ( 'NONE',  ( 0.5555748031496109407, 0.9100161909011688088, 0.01858545845903165558 ) ) ;
#22969 = CARTESIAN_POINT ( 'NONE',  ( -1.033464566929134687, -0.06523048226347956391, 1.021161417215306955 ) ) ;
#22970 = CARTESIAN_POINT ( 'NONE',  ( 0.9500414927467378812, 0.1787899950787401604, 0.5068897637257642197 ) ) ;
#22971 = CARTESIAN_POINT ( 'NONE',  ( 0.6971942568897637749, 2.189545951927499583E-17, 0.04183070860765386589 ) ) ;
#22973 = LINE ( 'NONE', #38061, #27053 ) ;
#22972 = CARTESIAN_POINT ( 'NONE',  ( -0.1113553986120547346, -0.2588582677165354173, 0.1113553986120547346 ) ) ;
#22974 = CARTESIAN_POINT ( 'NONE',  ( 0.9412147342319837628, -0.1574803149606297803, 1.921751968396409493 ) ) ;
#22975 = VERTEX_POINT ( 'NONE', #13495 ) ;
#22976 = CARTESIAN_POINT ( 'NONE',  ( 0.8759842519685039353, 0.000000000000000000, 4.498031496062992574 ) ) ;
#22977 = CARTESIAN_POINT ( 'NONE',  ( 0.8759842519685039353, -0.1574803149606299191, 0.9055118110236221041 ) ) ;
#22978 = DIRECTION ( 'NONE',  ( 1.000000000000000000, 0.000000000000000000, 0.000000000000000000 ) ) ;
#22979 = CARTESIAN_POINT ( 'NONE',  ( 0.1574803149606300301, -0.5467519683964097155, -0.06523048226347956391 ) ) ;
#22980 = CARTESIAN_POINT ( 'NONE',  ( -0.1564674760227699191, -0.09340956239926194449, 0.1950964973271945568 ) ) ;
#22981 = DIRECTION ( 'NONE',  ( -0.8191520442889989040, 0.000000000000000000, -0.5735764363510359454 ) ) ;
#22982 = CARTESIAN_POINT ( 'NONE',  ( -0.1288387865083106543, -0.08955301800084583541, 0.09875942480506787191 ) ) ;
#22983 = VERTEX_POINT ( 'NONE', #17550 ) ;
#22984 = DIRECTION ( 'NONE',  ( 0.000000000000000000, 0.000000000000000000, 1.000000000000000000 ) ) ;
#22985 = CARTESIAN_POINT ( 'NONE',  ( -0.2927386332256519674, 0.1025512834716171690, 1.008637609646301447 ) ) ;
#22986 = CARTESIAN_POINT ( 'NONE',  ( 0.8759842519685039353, -0.1787899950787401882, 0.7209645668753701386 ) ) ;
#22987 = ORIENTED_EDGE ( 'NONE', *, *, #8556, .F. ) ;
#22988 = CARTESIAN_POINT ( 'NONE',  ( 0.1574803149606300023, -0.2237541348899639571, -1.272196386806235813 ) ) ;
#22989 = DIRECTION ( 'NONE',  ( 1.000000000000000000, 0.000000000000000000, 0.000000000000000000 ) ) ;
#22990 = CARTESIAN_POINT ( 'NONE',  ( -0.1264236179284866091, -1.658956692859621995, -0.1264236179284866091 ) ) ;
#22991 = CARTESIAN_POINT ( 'NONE',  ( -0.1787899950787401604, -0.8690944881352120621, 0.07405724077823318263 ) ) ;
#22992 = CARTESIAN_POINT ( 'NONE',  ( 0.1113553986120547346, -1.223425196850393748, -0.1113553986120547346 ) ) ;
#22993 = CARTESIAN_POINT ( 'NONE',  ( 0.7185039370078746268, -0.06523048226347956391, 1.163877952648379344 ) ) ;
#22994 = CARTESIAN_POINT ( 'NONE',  ( -0.7646288533564489232, -0.1113553986120547346, 1.648622047244094668 ) ) ;
#22995 = AXIS2_PLACEMENT_3D ( 'NONE', #11733, #26352, #23217 ) ;
#22996 = ORIENTED_EDGE ( 'NONE', *, *, #15932, .T. ) ;
#22997 = ORIENTED_EDGE ( 'NONE', *, *, #22016, .T. ) ;
#22998 = EDGE_CURVE ( 'NONE', #30008, #11246, #34877, .T. ) ;
#22999 = CARTESIAN_POINT ( 'NONE',  ( 1.054774247047244540, -0.07405724077823318263, 1.756889763725764553 ) ) ;
#23000 = CARTESIAN_POINT ( 'NONE',  ( -0.9500414927467378812, 0.1787899950787401604, 0.9005905511273389896 ) ) ;
#23001 = CARTESIAN_POINT ( 'NONE',  ( -0.1279527559055118058, -0.2216206741968047289, -0.3149606299212598381 ) ) ;
#23002 = CARTESIAN_POINT ( 'NONE',  ( 0.8019270111902717657, -0.1787899950787401604, 0.4478346456155276045 ) ) ;
#23003 = CARTESIAN_POINT ( 'NONE',  ( -0.6971942568897648851, 0.07405724077823318263, 1.338582677111590069 ) ) ;
#23004 = CARTESIAN_POINT ( 'NONE',  ( -0.9873396505805591694, 0.1113553986120547346, 1.500984251860976171 ) ) ;
#23005 = CARTESIAN_POINT ( 'NONE',  ( -0.8019270111902716547, 0.1787899950787401604, 1.254921259788757348 ) ) ;
#23006 = CARTESIAN_POINT ( 'NONE',  ( -0.9500414927467378812, -0.1787899950787401604, 0.9202755904974182499 ) ) ;
#23007 = CARTESIAN_POINT ( 'NONE',  ( -1.002407869896990045, 0.1264236179284866091, 0.1500984251430867999 ) ) ;
#23008 = EDGE_CURVE ( 'NONE', #34485, #25630, #46070, .T. ) ;
#23009 = FACE_OUTER_BOUND ( 'NONE', #41775, .T. ) ;
#23010 = CARTESIAN_POINT ( 'NONE',  ( -1.054774247047244096, 0.000000000000000000, 1.798720472387181024 ) ) ;
#23011 = CARTESIAN_POINT ( 'NONE',  ( -0.6971942568897626646, 0.07405724077823318263, 0.1230314960092287191 ) ) ;
#23012 = CARTESIAN_POINT ( 'NONE',  ( -1.033464566929134687, -0.06523048226347956391, 1.542814960629920851 ) ) ;
#23013 = CARTESIAN_POINT ( 'NONE',  ( -1.181102362204724310, -0.3937007874015748254, 0.9842519685039370358 ) ) ;
#23014 = CARTESIAN_POINT ( 'NONE',  ( 0.6971942568897648851, 0.07405724077823318263, 1.619094488135213838 ) ) ;
#23015 = CARTESIAN_POINT ( 'NONE',  ( -0.1946994858204661449, -0.09842519685039370636, -0.1548548131872939104 ) ) ;
#23016 = DIRECTION ( 'NONE',  ( 0.000000000000000000, 0.000000000000000000, -1.000000000000000000 ) ) ;
#23017 = CARTESIAN_POINT ( 'NONE',  ( 0.9412147342319837628, 0.1574803149606300301, 0.2829724408373550104 ) ) ;
#23018 = ORIENTED_EDGE ( 'NONE', *, *, #17008, .F. ) ;
#23019 = EDGE_CURVE ( 'NONE', #4424, #18622, #46307, .T. ) ;
#23020 = EDGE_CURVE ( 'NONE', #5132, #12211, #14209, .T. ) ;
#23021 = VERTEX_POINT ( 'NONE', #46538 ) ;
#23022 = ORIENTED_EDGE ( 'NONE', *, *, #12457, .F. ) ;
#23023 = CARTESIAN_POINT ( 'NONE',  ( -0.1264236179284866091, -0.9552165353793071745, -0.1264236179284866091 ) ) ;
#23024 = CARTESIAN_POINT ( 'NONE',  ( -0.1264236179284866091, -1.068405511757259951, -0.1264236179284866091 ) ) ;
#23025 = CONICAL_SURFACE ( 'NONE', #36820, 0.1377952755905509363, 0.9599310885968960205 ) ;
#23026 = CARTESIAN_POINT ( 'NONE',  ( 0.000000000000000000, 0.000000000000000000, 0.000000000000000000 ) ) ;
#23027 = ( NAMED_UNIT ( * ) SI_UNIT ( $, .STERADIAN. ) SOLID_ANGLE_UNIT ( ) ) ;
#23028 = CARTESIAN_POINT ( 'NONE',  ( -0.1797182628040039087, -0.2790792426539118187, -0.07444174185955065859 ) ) ;
#23029 = CARTESIAN_POINT ( 'NONE',  ( 0.1113553986120547346, 0.1151574803149606335, -0.1113553986120547346 ) ) ;
#23030 = VECTOR ( 'NONE', #33925, 39.37007874015748143 ) ;
#23031 = CARTESIAN_POINT ( 'NONE',  ( 0.8019270111902717657, -0.1787899950787401604, 0.7972440944344250102 ) ) ;
#23032 = AXIS2_PLACEMENT_3D ( 'NONE', #19613, #29974, #26357 ) ;
#23033 = ( BOUNDED_CURVE ( )  B_SPLINE_CURVE ( 2, ( #42115, #23949, #38555, #23703, #20336, #16748, #5945, #17217, #39239 ),
 .UNSPECIFIED., .F., .T. ) 
 B_SPLINE_CURVE_WITH_KNOTS ( ( 3, 2, 2, 2, 3 ),
 ( 0.7299999999999999822, 0.7325000000000000400, 0.7349999999999999867, 0.7375000000000000444, 0.7399999999999999911 ),
 .UNSPECIFIED. ) 
 CURVE ( )  GEOMETRIC_REPRESENTATION_ITEM ( )  RATIONAL_B_SPLINE_CURVE ( ( 1.000000000000000000, 0.9238795325112869605, 1.000000000000000000, 0.9238795325112869605, 1.000000000000000000, 0.9238795325112869605, 1.000000000000000000, 0.9238795325112869605, 1.000000000000000000 ) ) 
 REPRESENTATION_ITEM ( '' )  ) ;
#23034 = CARTESIAN_POINT ( 'NONE',  ( 1.033464566929133799, 0.000000000000000000, 1.141732283357039357 ) ) ;
#23035 = PLANE ( 'NONE',  #24405 ) ;
#23036 = CARTESIAN_POINT ( 'NONE',  ( -0.9412147342319837628, -0.1574803149606297803, 0.07135826760900840227 ) ) ;
#23037 = CARTESIAN_POINT ( 'NONE',  ( 0.8759842519685039353, 0.1787899950787401882, 1.808562992072220377 ) ) ;
#23038 = CARTESIAN_POINT ( 'NONE',  ( 1.033464566929133799, 0.000000000000000000, 0.04921259842519685318 ) ) ;
#23039 = LINE ( 'NONE', #5289, #43568 ) ;
#23040 = CARTESIAN_POINT ( 'NONE',  ( -0.1264236179284866091, -0.4335629920722205433, 0.1264236179284866091 ) ) ;
#23041 = CARTESIAN_POINT ( 'NONE',  ( 0.7185039370078732945, -0.06523048226347920309, 0.1107283464566930498 ) ) ;
#23042 = CARTESIAN_POINT ( 'NONE',  ( 0.07405724077823318263, -1.208661417269070393, 0.1787899950787401604 ) ) ;
#23043 = CARTESIAN_POINT ( 'NONE',  ( 0.6971942568897637749, 2.189545951927499583E-17, 0.1648622046706460786 ) ) ;
#23044 = CARTESIAN_POINT ( 'NONE',  ( -1.054774247047244540, 0.07405724077823318263, 1.796259842465923073 ) ) ;
#23045 = ORIENTED_EDGE ( 'NONE', *, *, #9595, .T. ) ;
#23046 = CARTESIAN_POINT ( 'NONE',  ( -1.054774247047244540, 0.07405724077823318263, 1.289370078686393750 ) ) ;
#23047 = DIRECTION ( 'NONE',  ( 1.000000000000000000, 0.000000000000000000, 0.000000000000000000 ) ) ;
#23048 = EDGE_CURVE ( 'NONE', #43073, #37122, #9900, .T. ) ;
#23049 = CARTESIAN_POINT ( 'NONE',  ( 0.1113553986120547346, -1.184055118002708795, 0.1113553986120547346 ) ) ;
#23050 = CARTESIAN_POINT ( 'NONE',  ( 0.8019270111902717657, 0.1787899950787401604, 0.03937007868639399305 ) ) ;
#23051 = CARTESIAN_POINT ( 'NONE',  ( -1.054774247047244540, 0.07405724077823318263, 1.166338582623402509 ) ) ;
#23052 = DIRECTION ( 'NONE',  ( 1.822029033848725028E-16, 0.000000000000000000, 1.000000000000000000 ) ) ;
#23053 = CARTESIAN_POINT ( 'NONE',  ( 0.04026256913104946100, -0.09842715401333676506, -0.1741995584308680955 ) ) ;
#23054 = CARTESIAN_POINT ( 'NONE',  ( 0.7646288533564489232, 0.1113553986120547346, 0.05413385816018952829 ) ) ;
#23055 = CARTESIAN_POINT ( 'NONE',  ( 1.002407869896990045, -0.1264236179284866091, 0.5339566928596221063 ) ) ;
#23056 = CARTESIAN_POINT ( 'NONE',  ( -0.6971942568897648851, -0.07405724077823297447, 0.4379921259304883074 ) ) ;
#23057 = CARTESIAN_POINT ( 'NONE',  ( -0.9500414927467378812, 0.1787899950787401604, 0.8169291338045038264 ) ) ;
#23058 = ORIENTED_EDGE ( 'NONE', *, *, #24381, .F. ) ;
#23059 = VECTOR ( 'NONE', #16393, 39.37007874015748143 ) ;
#23060 = CARTESIAN_POINT ( 'NONE',  ( -0.2559055118110236116, -0.1477471161312043368, -0.3149606299212598381 ) ) ;
#23061 = ORIENTED_EDGE ( 'NONE', *, *, #36589, .F. ) ;
#23062 = CARTESIAN_POINT ( 'NONE',  ( 1.054774247047244096, 0.000000000000000000, 0.8932086613635591421 ) ) ;
#23063 = CARTESIAN_POINT ( 'NONE',  ( -0.8107537697050234415, -0.1574803149606297803, 0.1550196850393702197 ) ) ;
#23064 = CARTESIAN_POINT ( 'NONE',  ( 0.7495606340400177148, 0.1264236179284866091, 1.222933070812378009 ) ) ;
#23065 = CARTESIAN_POINT ( 'NONE',  ( -1.054774247047244540, -0.07405724077823318263, 1.988188976324191781 ) ) ;
#23066 = CARTESIAN_POINT ( 'NONE',  ( -0.2559055118110236671, -0.08665008082093515751, -0.05796767012934854468 ) ) ;
#23067 = CIRCLE ( 'NONE', #46003, 0.1003937007874011050 ) ;
#23068 = VERTEX_POINT ( 'NONE', #46774 ) ;
#23069 = VECTOR ( 'NONE', #31103, 39.37007874015748143 ) ;
#23070 = EDGE_CURVE ( 'NONE', #8749, #46267, #24746, .T. ) ;
#23071 = CYLINDRICAL_SURFACE ( 'NONE', #7998, 0.1377952755905510751 ) ;
#23072 = AXIS2_PLACEMENT_3D ( 'NONE', #389, #44230, #30153 ) ;
#23073 = CARTESIAN_POINT ( 'NONE',  ( 0.1574803149606299746, 0.3740157480314960647, 0.9783464566929134243 ) ) ;
#23074 = CARTESIAN_POINT ( 'NONE',  ( -0.9500414927467378812, 0.1787899950787401604, 0.02952755900135462311 ) ) ;
#23075 = CARTESIAN_POINT ( 'NONE',  ( -0.1264236179284866091, -1.517348377678057192, -0.1264236179284866091 ) ) ;
#23076 = VERTEX_POINT ( 'NONE', #20671 ) ;
#23077 = CARTESIAN_POINT ( 'NONE',  ( 3.284318927891251994E-17, -0.4237204723871811352, 0.1787899950787401882 ) ) ;
#23078 = CARTESIAN_POINT ( 'NONE',  ( -0.4330708661417356775, 0.1864803149606299171, -1.186023622047243986 ) ) ;
#23079 = ORIENTED_EDGE ( 'NONE', *, *, #1300, .F. ) ;
#23080 = CARTESIAN_POINT ( 'NONE',  ( 0.7185039370078739607, 1.928577636452523993E-17, 1.604330708661417360 ) ) ;
#23081 = CYLINDRICAL_SURFACE ( 'NONE', #1676, 0.1003937007874010356 ) ;
#23082 = CARTESIAN_POINT ( 'NONE',  ( 0.8019270111902717657, -0.1787899950787401604, 0.1279527558517483676 ) ) ;
#23083 = CARTESIAN_POINT ( 'NONE',  ( 0.07405724077823318263, -1.725393700733637958, 0.1787899950787401604 ) ) ;
#23084 = CARTESIAN_POINT ( 'NONE',  ( 0.1264236179284866091, 0.1274606299750234428, 0.1264236179284866091 ) ) ;
#23085 = DIRECTION ( 'NONE',  ( 0.000000000000000000, 0.000000000000000000, 1.000000000000000000 ) ) ;
#23086 = CYLINDRICAL_SURFACE ( 'NONE', #5033, 0.1574803149606299191 ) ;
#23087 = VECTOR ( 'NONE', #43537, 39.37007874015748143 ) ;
#23088 = CARTESIAN_POINT ( 'NONE',  ( -0.9500414927467377701, 0.1787899950787401604, 0.6643700786863929730 ) ) ;
#23089 = CARTESIAN_POINT ( 'NONE',  ( 0.1113553986120547346, -0.7214566929133858775, 0.1113553986120547346 ) ) ;
#23090 = CARTESIAN_POINT ( 'NONE',  ( 0.07444174185955046430, -1.470024124543674926, -0.1797182628040039087 ) ) ;
#23091 = CARTESIAN_POINT ( 'NONE',  ( -0.7185039370078739607, 1.928577636452523993E-17, 1.594488188868850242 ) ) ;
#23092 = CARTESIAN_POINT ( 'NONE',  ( -0.1113553986120547346, -0.4458661416247566289, 0.1113553986120547346 ) ) ;
#23093 = CARTESIAN_POINT ( 'NONE',  ( 0.2471922904502825702, 0.06774690380563494485, -0.09545378441111782020 ) ) ;
#23094 = CARTESIAN_POINT ( 'NONE',  ( 0.6971942568897637749, 2.189545951927499583E-17, 1.385334645615527549 ) ) ;
#23095 = CARTESIAN_POINT ( 'NONE',  ( 0.8759842519685039353, 0.1787899950787401882, 1.921751968450173376 ) ) ;
#23096 = CARTESIAN_POINT ( 'NONE',  ( 0.6971942568897626646, -0.07405724077823297447, 0.2805118109698587214 ) ) ;
#23097 = B_SPLINE_CURVE_WITH_KNOTS ( 'NONE', 3,
 ( #37960, #19733, #34367, #1508, #2694, #24059, #6527, #38888, #10384, #6290, #10142, #5834, #17321, #21141, #46542, #27908, #31958, #24751, #42239 ),
 .UNSPECIFIED., .F., .F.,
 ( 4, 2, 2, 1, 2, 2, 2, 2, 2, 4 ),
 ( 0.000000000000000000, 0.2500000000000028311, 0.3750000000000042188, 0.4375000000000049960, 0.4687500000000051625, 0.5000000000000052180, 0.6250000000000036637, 0.6875000000000028866, 0.7500000000000021094, 1.000000000000000000 ),
 .UNSPECIFIED. ) ;
#23098 = VECTOR ( 'NONE', #24966, 39.37007874015748143 ) ;
#23099 = CIRCLE ( 'NONE', #3179, 0.1003937007874010356 ) ;
#23102 = EDGE_LOOP ( 'NONE', ( #2453, #18976, #28802, #24320 ) ) ;
#23101 = EDGE_CURVE ( 'NONE', #38861, #23202, #2451, .T. ) ;
#23100 = CARTESIAN_POINT ( 'NONE',  ( -0.7185039370078739607, 1.928577636452523993E-17, 0.1377952754830242266 ) ) ;
#23103 = CARTESIAN_POINT ( 'NONE',  ( 0.000000000000000000, 0.000000000000000000, -0.1966003937007873570 ) ) ;
#23104 = FACE_OUTER_BOUND ( 'NONE', #6047, .T. ) ;
#23106 = CARTESIAN_POINT ( 'NONE',  ( 3.284318927891251994E-17, -0.03494094482812622193, 0.1787899950787401882 ) ) ;
#23105 = CARTESIAN_POINT ( 'NONE',  ( -0.06523048226347956391, -0.8371062991050713942, 0.1574803149606297803 ) ) ;
#23107 = CARTESIAN_POINT ( 'NONE',  ( 0.1574803149606299191, -0.5708661417322835607, 0.9783464566929134243 ) ) ;
#23108 = CARTESIAN_POINT ( 'NONE',  ( 0.8019270111902717657, 0.1787899950787401604, 0.3494094487651343006 ) ) ;
#23109 = EDGE_CURVE ( 'NONE', #25373, #38468, #19541, .T. ) ;
#23110 = CARTESIAN_POINT ( 'NONE',  ( -0.7185039370078746268, -0.06523048226347956391, 0.7406496062992133922 ) ) ;
#23111 = CARTESIAN_POINT ( 'NONE',  ( -0.9412147342319837628, -0.1574803149606297803, 1.331200787294047672 ) ) ;
#23112 = CARTESIAN_POINT ( 'NONE',  ( 0.9873396505805591694, 0.1113553986120547346, 0.8415354330708662012 ) ) ;
#23113 = CARTESIAN_POINT ( 'NONE',  ( -0.8759842519685039353, 0.1574803149606299191, 0.7677165354330708347 ) ) ;
#23114 = CARTESIAN_POINT ( 'NONE',  ( 0.9412147342319837628, -0.1574803149606297803, 0.8587598424121576368 ) ) ;
#23115 = VERTEX_POINT ( 'NONE', #21138 ) ;
#23116 = EDGE_CURVE ( 'NONE', #23380, #14480, #10139, .T. ) ;
#23117 = DIRECTION ( 'NONE',  ( -0.000000000000000000, 1.000000000000000000, -0.000000000000000000 ) ) ;
#23118 = ORIENTED_EDGE ( 'NONE', *, *, #2269, .F. ) ;
#23119 = CARTESIAN_POINT ( 'NONE',  ( 0.1797182628040039087, -0.02317373084288805798, 0.07444174185955046430 ) ) ;
#23121 = ORIENTED_EDGE ( 'NONE', *, *, #27183, .T. ) ;
#23120 = CARTESIAN_POINT ( 'NONE',  ( 0.1787899950787401604, -1.203740157426551383, -0.07405724077823318263 ) ) ;
#23122 = CARTESIAN_POINT ( 'NONE',  ( 0.6971942568897648851, -0.07405724077823297447, 1.619094488135213838 ) ) ;
#23123 = CARTESIAN_POINT ( 'NONE',  ( -0.8759842519685039353, -0.1574803149606299191, 1.259842519685039353 ) ) ;
#23125 = CARTESIAN_POINT ( 'NONE',  ( -1.033464566929134687, 0.06523048226347956391, 0.7504921258767240921 ) ) ;
#23124 = DIRECTION ( 'NONE',  ( -1.000000000000000000, 0.000000000000000000, 0.000000000000000000 ) ) ;
#23126 = CARTESIAN_POINT ( 'NONE',  ( 0.7495606340400177148, -0.1264236179284866091, 0.05167322829269323931 ) ) ;
#23127 = CARTESIAN_POINT ( 'NONE',  ( 0.9873396505805591694, -0.1113553986120547346, 1.333661417215306955 ) ) ;
#23128 = ORIENTED_EDGE ( 'NONE', *, *, #19766, .T. ) ;
#23129 = LINE ( 'NONE', #8737, #20637 ) ;
#23130 = CARTESIAN_POINT ( 'NONE',  ( -0.8759842519685039353, 0.1787899950787401882, 1.567421259788755794 ) ) ;
#23131 = CARTESIAN_POINT ( 'NONE',  ( -0.1574803149606300301, 0.01919291349335381161, -0.06523048226347956391 ) ) ;
#23132 = CARTESIAN_POINT ( 'NONE',  ( -0.8019270111902717657, 0.1787899950787401604, 1.259842519631276359 ) ) ;
#23133 = ORIENTED_EDGE ( 'NONE', *, *, #5244, .T. ) ;
#23134 = VECTOR ( 'NONE', #46611, 39.37007874015748143 ) ;
#23135 = CARTESIAN_POINT ( 'NONE',  ( 0.04756641494945763188, 0.3740157480314960647, 1.120507485783946766 ) ) ;
#23136 = CARTESIAN_POINT ( 'NONE',  ( -0.9500414927467378812, 0.1787899950787401604, 0.3887795275052913224 ) ) ;
#23137 = LINE ( 'NONE', #16879, #31832 ) ;
#23138 = CARTESIAN_POINT ( 'NONE',  ( -0.8107537697050254399, -0.1574803149606297803, 1.877460629813732407 ) ) ;
#23139 = CARTESIAN_POINT ( 'NONE',  ( 0.1787899950787401604, -1.062131842244986135, 0.07405724077823318263 ) ) ;
#23140 = ORIENTED_EDGE ( 'NONE', *, *, #14732, .F. ) ;
#23141 = CARTESIAN_POINT ( 'NONE',  ( -0.1787899950787401882, -0.0004921259304884630223, 0.000000000000000000 ) ) ;
#23142 = ORIENTED_EDGE ( 'NONE', *, *, #1193, .F. ) ;
#23143 = CONICAL_SURFACE ( 'NONE', #1701, 0.1003937007874010356, 0.7853981633978647237 ) ;
#23144 = CIRCLE ( 'NONE', #5544, 0.1787899950787401049 ) ;
#23145 = CARTESIAN_POINT ( 'NONE',  ( -0.7185039370078746268, -0.06523048226347956391, 0.2583661416247562959 ) ) ;
#23146 = DIRECTION ( 'NONE',  ( -1.000000000000000000, 0.000000000000000000, 0.000000000000000000 ) ) ;
#23147 = FACE_OUTER_BOUND ( 'NONE', #30987, .T. ) ;
#23148 = CARTESIAN_POINT ( 'NONE',  ( -0.1787899950787401882, -0.5959645668753701386, 0.000000000000000000 ) ) ;
#23149 = CARTESIAN_POINT ( 'NONE',  ( -0.9500414927467377701, 0.1787899950787401604, 0.1919291338045042705 ) ) ;
#23150 = CARTESIAN_POINT ( 'NONE',  ( -0.7185039370078746268, 0.06523048226347956391, 0.8932086614173218031 ) ) ;
#23151 = CARTESIAN_POINT ( 'NONE',  ( -0.1184675242425147629, 0.3740157480314960647, 1.161904259418922836 ) ) ;
#23152 = LINE ( 'NONE', #11671, #24844 ) ;
#23153 = CARTESIAN_POINT ( 'NONE',  ( -0.1270800023317771588, -1.019728848953123990, 0.1270800023317771588 ) ) ;
#23154 = CYLINDRICAL_SURFACE ( 'NONE', #40148, 0.1574803149606299191 ) ;
#23155 = CARTESIAN_POINT ( 'NONE',  ( 0.8019270111902717657, -0.1787899950787401604, 0.9596456692375764375 ) ) ;
#23156 = CARTESIAN_POINT ( 'NONE',  ( -0.1377952755905511861, 1.808041534174241898E-17, -0.01478361295688420882 ) ) ;
#23157 = CARTESIAN_POINT ( 'NONE',  ( 1.033464566929134687, -0.06523048226347956391, 1.582185039370078927 ) ) ;
#23159 = FACE_OUTER_BOUND ( 'NONE', #43197, .T. ) ;
#23158 = CARTESIAN_POINT ( 'NONE',  ( 0.7102849092615979298, 0.006128682583928486173, 1.983157089510096949 ) ) ;
#23160 = CARTESIAN_POINT ( 'NONE',  ( 0.1564141481333313488, -0.4043448265461809243, -0.9276852126764746354 ) ) ;
#23161 = CARTESIAN_POINT ( 'NONE',  ( 0.1574803149606299191, -0.6673228345381416737, -1.928577636452523993E-17 ) ) ;
#23162 = EDGE_CURVE ( 'NONE', #27640, #32335, #47399, .T. ) ;
#23163 = AXIS2_PLACEMENT_3D ( 'NONE', #31974, #38907, #13983 ) ;
#23164 = CARTESIAN_POINT ( 'NONE',  ( 0.1377952755905510751, 0.000000000000000000, -0.02633646578327370619 ) ) ;
#23166 = DIRECTION ( 'NONE',  ( 0.000000000000000000, 0.000000000000000000, -1.000000000000000000 ) ) ;
#23165 = CARTESIAN_POINT ( 'NONE',  ( 1.002407869896990045, 0.1264236179284866091, 1.011318897584031484 ) ) ;
#23167 = CARTESIAN_POINT ( 'NONE',  ( 1.002407869896990045, 0.1264236179284866091, 1.843011810969858333 ) ) ;
#23168 = CARTESIAN_POINT ( 'NONE',  ( -0.1264236179284866091, -0.9798228345919054449, 0.1264236179284866091 ) ) ;
#23169 = ORIENTED_EDGE ( 'NONE', *, *, #28163, .F. ) ;
#23170 = DIRECTION ( 'NONE',  ( 0.000000000000000000, 0.000000000000000000, 1.000000000000000000 ) ) ;
#23171 = EDGE_CURVE ( 'NONE', #3412, #41311, #39194, .T. ) ;
#23172 = DIRECTION ( 'NONE',  ( 0.000000000000000000, 0.7880107536067175733, -0.6156614753256638428 ) ) ;
#23173 = CARTESIAN_POINT ( 'NONE',  ( -0.06523048226347956391, -1.757381889656251195, -0.1574803149606300301 ) ) ;
#23174 = CARTESIAN_POINT ( 'NONE',  ( -0.7646288533564489232, -0.1113553986120547346, 0.1033464565853864231 ) ) ;
#23175 = CARTESIAN_POINT ( 'NONE',  ( -0.1264236179284866091, -0.08415354325332302654, -0.1264236179284866091 ) ) ;
#23176 = CARTESIAN_POINT ( 'NONE',  ( 0.8019270111902717657, 0.1787899950787401604, 1.176181102308441417 ) ) ;
#23177 = EDGE_CURVE ( 'NONE', #26106, #31809, #23144, .T. ) ;
#23178 = DIRECTION ( 'NONE',  ( 1.000000000000000000, 0.000000000000000000, -0.000000000000000000 ) ) ;
#23179 = CARTESIAN_POINT ( 'NONE',  ( -0.1113553986120547346, -1.686023622047244208, -0.1113553986120547346 ) ) ;
#23180 = DIRECTION ( 'NONE',  ( -1.000000000000000000, 0.000000000000000000, 0.000000000000000000 ) ) ;
#23181 = DIRECTION ( 'NONE',  ( 1.000000000000000000, 0.000000000000000000, 0.000000000000000000 ) ) ;
#23182 = CARTESIAN_POINT ( 'NONE',  ( -1.054774247047244540, 0.07405724077823318263, 0.1820866141194649179 ) ) ;
#23183 = ORIENTED_EDGE ( 'NONE', *, *, #28056, .T. ) ;
#23185 = ORIENTED_EDGE ( 'NONE', *, *, #36437, .T. ) ;
#23184 = STYLED_ITEM ( 'NONE', ( #14086 ), #3862 ) ;
#23186 = ORIENTED_EDGE ( 'NONE', *, *, #35719, .F. ) ;
#23187 = CARTESIAN_POINT ( 'NONE',  ( 0.1787899950787401604, -1.523622047190330564, 0.07405724077823318263 ) ) ;
#23188 = CARTESIAN_POINT ( 'NONE',  ( -1.054774247047244540, 0.07405724077823318263, 1.874999999946236784 ) ) ;
#23189 = CARTESIAN_POINT ( 'NONE',  ( -1.054774247047244540, -0.07405724077823318263, 0.9645669290800954476 ) ) ;
#23190 = CARTESIAN_POINT ( 'NONE',  ( -0.9500414927467378812, -0.1787899950787401604, 0.4921259841982048577 ) ) ;
#23191 = CARTESIAN_POINT ( 'NONE',  ( 0.7185039370078739607, 1.928577636452523993E-17, 0.5314960628845992741 ) ) ;
#23192 = DIRECTION ( 'NONE',  ( 0.000000000000000000, 0.000000000000000000, 1.000000000000000000 ) ) ;
#23193 = DIRECTION ( 'NONE',  ( 0.000000000000000000, 0.000000000000000000, -1.000000000000000000 ) ) ;
#23194 = CARTESIAN_POINT ( 'NONE',  ( -1.033464566929134687, 0.06523048226347956391, 1.665846456692914312 ) ) ;
#23195 = CARTESIAN_POINT ( 'NONE',  ( 0.1264236179284866091, -0.6216790863394745514, -0.1264236179284866091 ) ) ;
#23196 = CARTESIAN_POINT ( 'NONE',  ( 0.06715823863710629338, -0.08956012741285963863, 0.2065986400649870158 ) ) ;
#23197 = CARTESIAN_POINT ( 'NONE',  ( 0.7646288533564489232, -0.1113553986120547346, 0.4675196850393700809 ) ) ;
#23198 = CARTESIAN_POINT ( 'NONE',  ( -0.7185039370078739607, 1.928577636452523993E-17, 1.161417322727118284 ) ) ;
#23199 = CARTESIAN_POINT ( 'NONE',  ( -0.8019270111902717657, -0.1787899950787401604, 0.4429133857730075952 ) ) ;
#23200 = CARTESIAN_POINT ( 'NONE',  ( 1.033464566929134687, 0.06523048226347956391, 1.183562992018456272 ) ) ;
#23201 = AXIS2_PLACEMENT_3D ( 'NONE', #1497, #42459, #9664 ) ;
#23202 = VERTEX_POINT ( 'NONE', #36490 ) ;
#23203 = CARTESIAN_POINT ( 'NONE',  ( 0.000000000000000000, 0.000000000000000000, -0.09302377043719921301 ) ) ;
#23204 = CARTESIAN_POINT ( 'NONE',  ( -0.8759842519685039353, 0.1787899950787401882, 1.572342519631275692 ) ) ;
#23205 = CARTESIAN_POINT ( 'NONE',  ( -0.8759842519685039353, 0.1787899950787401882, 0.7406496062454487328 ) ) ;
#23206 = VECTOR ( 'NONE', #38131, 39.37007874015748143 ) ;
#23207 = CARTESIAN_POINT ( 'NONE',  ( 3.284318927891251994E-17, -1.373523621993480326, 0.1787899950787401882 ) ) ;
#23208 = CARTESIAN_POINT ( 'NONE',  ( -0.07405724077823318263, -1.503937007820251637, -0.1787899950787401604 ) ) ;
#23209 = ( BOUNDED_CURVE ( )  B_SPLINE_CURVE ( 2, ( #42987, #28667, #10436, #39168, #32252, #2281, #35600, #42740, #17367 ),
 .UNSPECIFIED., .F., .F. ) 
 B_SPLINE_CURVE_WITH_KNOTS ( ( 3, 2, 2, 2, 3 ),
 ( 0.5500000000000000444, 0.5524999999999999911, 0.5550000000000000488, 0.5574999999999999956, 0.5600000000000000533 ),
 .UNSPECIFIED. ) 
 CURVE ( )  GEOMETRIC_REPRESENTATION_ITEM ( )  RATIONAL_B_SPLINE_CURVE ( ( 1.000000000000000000, 0.9238795325112869605, 1.000000000000000000, 0.9238795325112869605, 1.000000000000000000, 0.9238795325112869605, 1.000000000000000000, 0.9238795325112869605, 1.000000000000000000 ) ) 
 REPRESENTATION_ITEM ( '' )  ) ;
#23210 = VECTOR ( 'NONE', #7019, 39.37007874015748143 ) ;
#23211 = CARTESIAN_POINT ( 'NONE',  ( 0.9412147342319837628, -0.1574803149606297803, 0.1993110236220472509 ) ) ;
#23212 = CARTESIAN_POINT ( 'NONE',  ( 0.7646288533564489232, 0.1113553986120547346, 0.9694881889763780070 ) ) ;
#23213 = CARTESIAN_POINT ( 'NONE',  ( 0.8107537697050253289, -0.1574803149606297803, 0.4306102362204725642 ) ) ;
#23214 = DIRECTION ( 'NONE',  ( 0.000000000000000000, -1.000000000000000000, 0.000000000000000000 ) ) ;
#23215 = CARTESIAN_POINT ( 'NONE',  ( -0.8759842519685039353, -0.1574803149606299191, 1.053149606191685184 ) ) ;
#23216 = CARTESIAN_POINT ( 'NONE',  ( 0.9500414927467378812, 0.1787899950787401604, 0.6249999999462356737 ) ) ;
#23217 = DIRECTION ( 'NONE',  ( 0.000000000000000000, 0.000000000000000000, -1.000000000000000000 ) ) ;
#23219 = CARTESIAN_POINT ( 'NONE',  ( 0.9412147342319837628, -0.1574803149606297803, 0.3567913385826773087 ) ) ;
#23218 = CARTESIAN_POINT ( 'NONE',  ( 0.1574803149606300301, -0.2859251968503936370, 0.06523048226347956391 ) ) ;
#23220 = CARTESIAN_POINT ( 'NONE',  ( 0.9412147342319837628, -0.1574803149606297803, 2.000492125876725424 ) ) ;
#23221 = ORIENTED_EDGE ( 'NONE', *, *, #16944, .T. ) ;
#23222 = DIRECTION ( 'NONE',  ( 0.000000000000000000, -0.9699617890481251337, -0.2432573283306392609 ) ) ;
#23223 = CARTESIAN_POINT ( 'NONE',  ( -0.6971942568897648851, -0.07405724077823297447, 1.151574803095843036 ) ) ;
#23224 = CARTESIAN_POINT ( 'NONE',  ( 0.8107537697050253289, 0.1574803149606300301, 1.163877952755904666 ) ) ;
#23225 = CARTESIAN_POINT ( 'NONE',  ( -0.8759842519685039353, 0.1574803149606299191, 0.7185039369003465293 ) ) ;
#23226 = CARTESIAN_POINT ( 'NONE',  ( 0.06523048226347956391, -0.5565944880814488460, 0.1574803149606297803 ) ) ;
#23227 = EDGE_CURVE ( 'NONE', #26427, #12403, #2454, .T. ) ;
#23228 = FACE_OUTER_BOUND ( 'NONE', #42265, .T. ) ;
#23229 = DIRECTION ( 'NONE',  ( 1.822029033848725028E-16, 0.000000000000000000, 1.000000000000000000 ) ) ;
#23230 = CARTESIAN_POINT ( 'NONE',  ( 0.1574803149606300023, 0.2573565155132531701, -0.3015174453633727714 ) ) ;
#23231 = CARTESIAN_POINT ( 'NONE',  ( -0.1264236179284866091, -0.5467519684501732646, 0.1264236179284866091 ) ) ;
#23232 = EDGE_LOOP ( 'NONE', ( #8335, #15556, #30298, #8201 ) ) ;
#23233 = DIRECTION ( 'NONE',  ( 0.000000000000000000, 0.000000000000000000, 1.000000000000000000 ) ) ;
#23234 = CARTESIAN_POINT ( 'NONE',  ( 1.002407869896990045, -0.1264236179284866091, 0.6865157479777322935 ) ) ;
#23235 = CARTESIAN_POINT ( 'NONE',  ( -1.033464566929133799, 0.000000000000000000, 1.112204724409448842 ) ) ;
#23236 = EDGE_CURVE ( 'NONE', #40379, #19512, #27275, .T. ) ;
#23237 = VERTEX_POINT ( 'NONE', #4321 ) ;
#23238 = CARTESIAN_POINT ( 'NONE',  ( -0.09934514972680209832, 0.09575019180979019162, -0.2280761219286889518 ) ) ;
#23239 = CARTESIAN_POINT ( 'NONE',  ( 0.07405724077823318263, -1.745078740103716886, -0.1787899950787401604 ) ) ;
#23240 = CARTESIAN_POINT ( 'NONE',  ( 0.07405724077823318263, -0.8592519684501739308, 0.1787899950787401604 ) ) ;
#23241 = CARTESIAN_POINT ( 'NONE',  ( 0.1574803149606299191, -1.188976377952756014, -1.928577636452523993E-17 ) ) ;
#23242 = CARTESIAN_POINT ( 'NONE',  ( 0.7646288533564489232, 0.1113553986120547346, 1.195866141624756018 ) ) ;
#23243 = DIRECTION ( 'NONE',  ( -1.217491584052838080E-15, -0.6156614753256588468, -0.7880107536067214591 ) ) ;
#23244 = ORIENTED_EDGE ( 'NONE', *, *, #8398, .T. ) ;
#23245 = VERTEX_POINT ( 'NONE', #18723 ) ;
#23246 = CARTESIAN_POINT ( 'NONE',  ( -0.6971942568897637749, 2.189545951927499583E-17, 1.779035433017102319 ) ) ;
#23247 = CARTESIAN_POINT ( 'NONE',  ( 1.002407869896990045, -0.1264236179284866091, 1.793799212544661348 ) ) ;
#23248 = EDGE_LOOP ( 'NONE', ( #133, #7539, #23386, #14518, #27857, #29840, #26490, #23584, #373, #41503, #1594, #21980, #46030, #24589, #7686, #14281, #20640 ) ) ;
#23249 = CARTESIAN_POINT ( 'NONE',  ( 0.03901279071809810040, -0.09842519685039370636, 1.713085361781127913 ) ) ;
#23250 = CARTESIAN_POINT ( 'NONE',  ( 0.8759842519685039353, 0.1787899950787401882, 0.4306102361667086820 ) ) ;
#23251 = CARTESIAN_POINT ( 'NONE',  ( -0.8019270111902717657, -0.1787899950787401604, 1.309055118056472899 ) ) ;
#23252 = CARTESIAN_POINT ( 'NONE',  ( -0.7185039370078739607, 1.928577636452523993E-17, 0.7283464565853858819 ) ) ;
#23253 = CARTESIAN_POINT ( 'NONE',  ( -0.6971942568897637749, 2.189545951927499583E-17, 1.301673228292692830 ) ) ;
#23254 = CARTESIAN_POINT ( 'NONE',  ( -1.054774247047244540, -0.07405724077823318263, 0.8858267715997791836 ) ) ;
#23255 = CARTESIAN_POINT ( 'NONE',  ( -0.6971942568897626646, 0.07405724077823318263, 0.04429133852891373180 ) ) ;
#23256 = DIRECTION ( 'NONE',  ( -3.494233027178531125E-15, -1.000000000000000000, 0.000000000000000000 ) ) ;
#23257 = CARTESIAN_POINT ( 'NONE',  ( -1.054774247047244540, 0.07405724077823318263, 1.801181102308441861 ) ) ;
#23258 = CARTESIAN_POINT ( 'NONE',  ( -0.8019270111902717657, 0.1787899950787401604, 0.07874015742655145200 ) ) ;
#23259 = CARTESIAN_POINT ( 'NONE',  ( -0.7185039370078739607, 1.928577636452523993E-17, 1.830708661309795149 ) ) ;
#23260 = CARTESIAN_POINT ( 'NONE',  ( -0.9873396505805591694, -0.1113553986120547346, 1.776574803149606252 ) ) ;
#23261 = CARTESIAN_POINT ( 'NONE',  ( -1.033464566929134687, 0.06523048226347956391, 0.2878937007874017850 ) ) ;
#23262 = CARTESIAN_POINT ( 'NONE',  ( -0.004818628365293897708, -0.09851383159603781248, 0.1563573961146315083 ) ) ;
#23263 = CARTESIAN_POINT ( 'NONE',  ( 0.9873396505805591694, 0.1113553986120547346, 0.2017716534357799352 ) ) ;
#23264 = EDGE_CURVE ( 'NONE', #2549, #43655, #8581, .T. ) ;
#23265 = VERTEX_POINT ( 'NONE', #12459 ) ;
#23266 = ORIENTED_EDGE ( 'NONE', *, *, #12899, .F. ) ;
#23267 = CARTESIAN_POINT ( 'NONE',  ( 0.1264236179284866091, -0.8567913385289133155, 0.1264236179284866091 ) ) ;
#23268 = CARTESIAN_POINT ( 'NONE',  ( 0.1264236179284866091, -1.127460629867496067, 0.1264236179284866091 ) ) ;
#23269 = DIRECTION ( 'NONE',  ( 0.000000000000000000, 0.9699617890481186944, 0.2432573283306645462 ) ) ;
#23270 = CARTESIAN_POINT ( 'NONE',  ( -0.1270800023317771588, -0.3602800300554865887, -0.1270800023317771588 ) ) ;
#23271 = CARTESIAN_POINT ( 'NONE',  ( 0.06523048226347956391, -1.801673228238930946, -0.1574803149606300301 ) ) ;
#23272 = CYLINDRICAL_SURFACE ( 'NONE', #46359, 0.09842519685039317900 ) ;
#23273 = CIRCLE ( 'NONE', #2593, 0.1574803149606291142 ) ;
#23274 = CARTESIAN_POINT ( 'NONE',  ( -0.1787899950787401604, -0.1604330708123782034, 0.07405724077823318263 ) ) ;
#23275 = EDGE_CURVE ( 'NONE', #16796, #18657, #3994, .T. ) ;
#23277 = ADVANCED_FACE ( 'NONE', ( #7244 ), #25935, .T. ) ;
#23276 = CARTESIAN_POINT ( 'NONE',  ( 0.9500414927467378812, 0.1787899950787401604, 0.6988188975840318173 ) ) ;
#23278 = EDGE_CURVE ( 'NONE', #35809, #827, #25479, .T. ) ;
#23279 = CARTESIAN_POINT ( 'NONE',  ( 0.1598936088129108701, -0.05389714384564588123, 0.1404773021332396676 ) ) ;
#23280 = PRESENTATION_LAYER_ASSIGNMENT (  '', '', ( #12604 ) ) ;
#23281 = CARTESIAN_POINT ( 'NONE',  ( 0.9412147342319837628, 0.1574803149606300301, 0.4502952755905510474 ) ) ;
#23282 = CARTESIAN_POINT ( 'NONE',  ( 0.7495606340400177148, 0.1264236179284866091, 1.931594488135212728 ) ) ;
#23283 = ADVANCED_FACE ( 'NONE', ( #33147 ), #43892, .T. ) ;
#23284 = CARTESIAN_POINT ( 'NONE',  ( 0.8107537697050234415, -0.1574803149606297803, 0.1156496062992125873 ) ) ;
#23285 = DIRECTION ( 'NONE',  ( 0.000000000000000000, 0.000000000000000000, 1.000000000000000000 ) ) ;
#23286 = CARTESIAN_POINT ( 'NONE',  ( -0.07405724077823318263, -0.4704724408911186706, 0.1787899950787401604 ) ) ;
#23287 = CARTESIAN_POINT ( 'NONE',  ( 0.7646288533564489232, -0.1113553986120547346, 0.1131889763779527630 ) ) ;
#23288 = CARTESIAN_POINT ( 'NONE',  ( 0.1787899950787401604, -1.282480314906867314, 0.07405724077823318263 ) ) ;
#23289 = CARTESIAN_POINT ( 'NONE',  ( 0.9500414927467378812, 0.1787899950787401604, 0.1919291338045042428 ) ) ;
#23290 = CARTESIAN_POINT ( 'NONE',  ( -0.7495606340400177148, -0.1264236179284866091, 1.700295275536787498 ) ) ;
#23291 = ORIENTED_EDGE ( 'NONE', *, *, #20397, .T. ) ;
#23292 = CARTESIAN_POINT ( 'NONE',  ( -1.002407869896990045, 0.1264236179284866091, 1.370570866087968520 ) ) ;
#23293 = CARTESIAN_POINT ( 'NONE',  ( 0.8759842519685039353, 0.1787899950787401882, 1.454232283410803017 ) ) ;
#23294 = CARTESIAN_POINT ( 'NONE',  ( 0.9500414927467378812, 0.1787899950787401604, 0.1131889763241892138 ) ) ;
#23295 = CARTESIAN_POINT ( 'NONE',  ( -1.054774247047244540, -0.07405724077823318263, 1.161417322780881278 ) ) ;
#23296 = DIRECTION ( 'NONE',  ( -0.7986355100472959379, -2.891205793294678326E-16, 0.6018150231520442706 ) ) ;
#23297 = CARTESIAN_POINT ( 'NONE',  ( 0.06597690942901487943, -0.09842519659738405147, -0.1661715391456292656 ) ) ;
#23298 = CARTESIAN_POINT ( 'NONE',  ( 0.7185039370078739607, 1.928577636452523993E-17, 1.210629921259842590 ) ) ;
#23299 = CARTESIAN_POINT ( 'NONE',  ( 0.7495606340400177148, -0.1264236179284866091, 0.4847440944344252323 ) ) ;
#23300 = CARTESIAN_POINT ( 'NONE',  ( -1.002407869896990045, 0.1264236179284866091, 0.4207677164816693294 ) ) ;
#23301 = CARTESIAN_POINT ( 'NONE',  ( -0.7646288533564489232, 0.1113553986120547346, 0.8809055117034961802 ) ) ;
#23302 = ORIENTED_EDGE ( 'NONE', *, *, #34435, .F. ) ;
#23303 = AXIS2_PLACEMENT_3D ( 'NONE', #18308, #7981, #29622 ) ;
#23304 = CARTESIAN_POINT ( 'NONE',  ( -0.8107537697050253289, 0.1574803149606300301, 0.2977362204724410821 ) ) ;
#23305 = CARTESIAN_POINT ( 'NONE',  ( 0.6971942568897637749, 2.189545951927499583E-17, 1.227854330654897685 ) ) ;
#23306 = CARTESIAN_POINT ( 'NONE',  ( -1.002407869896990045, 0.1264236179284866091, 1.956200787347811110 ) ) ;
#23307 = CARTESIAN_POINT ( 'NONE',  ( -0.2559055118110236116, -0.1194803229784886650, -0.08356133691647003869 ) ) ;
#23308 = CIRCLE ( 'NONE', #39359, 0.09842519685039370636 ) ;
#23309 = VECTOR ( 'NONE', #14382, 39.37007874015748143 ) ;
#23310 = EDGE_LOOP ( 'NONE', ( #40471, #31354, #31650 ) ) ;
#23311 = LINE ( 'NONE', #33884, #27164 ) ;
#23312 = CARTESIAN_POINT ( 'NONE',  ( -0.6971942568897626646, 0.07405724077823318263, 0.9891732282926934960 ) ) ;
#23313 = EDGE_CURVE ( 'NONE', #8746, #15113, #15156, .T. ) ;
#23314 = CARTESIAN_POINT ( 'NONE',  ( -0.7646288533564489232, 0.1113553986120547346, 1.471456692805858113 ) ) ;
#23315 = CARTESIAN_POINT ( 'NONE',  ( 0.1574803149606300023, 0.3743908788525358022, -3.616772362661642592 ) ) ;
#23316 = CARTESIAN_POINT ( 'NONE',  ( -0.1264236179284866091, -1.507505857993017839, 0.1264236179284866091 ) ) ;
#23317 = AXIS2_PLACEMENT_3D ( 'NONE', #20690, #10398, #17097 ) ;
#23318 = ORIENTED_EDGE ( 'NONE', *, *, #45386, .F. ) ;
#23319 = CARTESIAN_POINT ( 'NONE',  ( 0.7646288533564489232, 0.1113553986120547346, 1.008858267716535417 ) ) ;
#23320 = CARTESIAN_POINT ( 'NONE',  ( -0.1787899950787401604, -0.4311023621509605386, 0.07405724077823318263 ) ) ;
#23321 = CARTESIAN_POINT ( 'NONE',  ( -0.1673228346456692994, 0.05639690512153998359, -0.1570009270184610506 ) ) ;
#23322 = CARTESIAN_POINT ( 'NONE',  ( 0.9873396505805591694, 0.1113553986120547346, 0.8809055118110236116 ) ) ;
#23323 = CARTESIAN_POINT ( 'NONE',  ( 1.033464566929133799, 0.000000000000000000, 0.7480314959554645871 ) ) ;
#23324 = CARTESIAN_POINT ( 'NONE',  ( 0.07405724077823318263, -0.2293307086076536994, 0.1787899950787401604 ) ) ;
#23325 = ( BOUNDED_SURFACE ( )  B_SPLINE_SURFACE ( 1, 2, ( 
 ( #21431, #25282, #36314, #24750, #43412, #17553, #39345, #10621, #39812, #25481, #46778, #26180, #15866, #30037, #37897, #4323, #23038, #499, #15158, #15632, #29802, #33384, #44580, #4105, #5054, #33153, #37656, #18955, #30494, #4812, #18724, #274, #37404, #40748, #11799, #12034, #14918, #44349, #29583, #7945, #40516, #33856, #30270, #23284, #731, #15393, #44822, #7705, #40986, #22562, #44125, #37179, #8647, #26417, #8170, #4562, #26657, #19197, #975, #41204, #8410, #19435, #34085, #1215, #45053, #12265, #26888, #41445, #30729, #24233, #45298, #17029, #2166, #24454, #12751, #41923, #16563, #27139, #45766, #27614, #31667, #12516, #41690, #45527, #8893, #5288, #23524, #34538, #1690, #42168, #10078, #35947, #21563, #23879, #38489, #45896, #13337, #27745, #20738, #35379, #43483, #14508, #14278, #22393, #32976, #11392, #36073, #14747, #7070, #348, #43247, #18096, #29170, #14997, #28919, #26005, #25049, #15143, #36476, #18251, #29333, #11, #962, #12020, #17477, #33308, #47430, #7869, #21795, #40444, #17945, #32604, #194, #47191, #14373, #14601, #21546, #22485, #46943, #22245, #36419, #434, #36877, #36184, #14133, #36644, #10790, #25636, #29506, #28778, #6922, #10547, #25400, #25145, #18420, #14841, #40672, #3577, #18195, #44053, #7170, #11251, #32835, #25862, #4031, #26100, #18651, #15086, #29733, #44274, #11478, #23213, #15564, #26348, #34017, #40907, #38056, #27063, #1141, #41855, #19604, #30428, #9059, #34466, #1616, #26818, #8816, #41375, #41612, #37575, #44512, #4736, #44980, #8106, #8575, #19838, #16266, #22728, #37827, #4982, #30659, #23453, #4483, #5210, #18887, #45219, #30203, #15311, #11729, #11966, #26587, #12441, #42567, #13374, #42790, #34950, #39218, #12912, #35418, #42345, #9775, #46177, #34719, #45692, #1858, #9299, #13589, #20309, #35652, #9541, #13150, #17419, #10005, #31360, #45940, #38289, #16956, #20544, #13831, #31596, #24386, #43042, #38985, #6154, #20777, #17191, #7356, #21249, #39926, #137, #3027, #40389, #46885, #6865, #14073, #3523, #36827, #33015, #36593, #28721, #14790, #36118, #43290, #47374, #29451, #10490, #3750, #28963, #7113, #43764, #10734, #18373, #25088, #40157, #7578, #21486, #3273, #14546, #32545, #47133, #21736, #18135, #36368, #32780, #29216, #10966, #25584, #29027, #29282, #39518, #35712, #24925, #43827, #10067, #2848, #36192, #21555, #42856, #25411, #39987, #14380, #6694, #28294, #20842, #17485, #39047, #36429, #46706, #3348, #43586, #46474, #43108, #6216, #28786, #21310, #17956, #10799, #35939, #11028, #24685, #32119, #32613, #47200, #39282, #7179, #21804, #3585, #3098, #6457, #35483, #13896, #2622, #18204, #28540, #32845, #47440, #13657, #10314, #17255, #43352, #17724, #14608, #31893, #32373, #21074, #46951, #14146, #10556, #25155, #39745, #6932, #44063, #40686, #40920, #11739, #26597, #29516, #41149, #37586, #22738, #18661, #4748, #30438, #33320, #22977, #37116, #44524, #15323, #30214, #36889, #8351, #14853, #37343, #44285, #29976, #668, #22027, #204, #36652, #33081, #33796, #3811, #19375, #29742, #15096, #34028, #914, #11261, #443, #40220, #18897, #25871, #1154, #7879, #18427, #44991, #15575, #15809, #11490, #26111, #4494, #40455, #22496, #44759, #25645, #7640, #22255, #4043, #4264, #33552, #26359, #19132, #23933, #4996, #34960, #38066, #41385, #1869, #2105, #12203, #5705, #30906, #41867, #45704, #45467, #9310, #16041, #42104, #38540, #8831, #20321, #16507, #16735, #9552, #12693, #20085, #45230, #31371, #34731, #45948, #24173, #13160, #2338, #27318, #23464, #19850, #27795, #42356, #19614, #16278, #26829, #31136, #9070, #38774, #5934, #23689, #34252, #38300, #5468, #30670, #12922, #20552, #35193, #12454, #27552, #16964, #31605, #8587, #27074, #23224, #37838, #1385, #5221, #41622, #34477, #1629, #17905, #10499, #38994, #6639, #42798, #28014, #24395, #21746, #10013, #20785, #3534, #39687, #32315, #46893, #24628, #35428, #28480, #2565, #47143, #36127, #10258, #36377, #28729, #43052, #18145, #43529, #10744, #35883, #32555, #3036, #3283, #39228, #6401, #46186, #13383, #17428, #13837, #24862, #42576, #14327, #9785, #28972, #14084, #6165, #21014, #35662, #2797, #17200, #32065, #39464, #17667, #25353, #31836, #46653, #43299, #46420, #39935, #25097, #7123, #13597, #28236, #21258, #6874, #21494, #8055, #40860, #144, #4437, #15040, #850, #14799, #18606, #21976, #11911, #29690, #15510, #25592, #44231, #29459, #15267, #4687, #44004, #11207, #33495, #33021, #25819, #37283, #11437, #36599, #30154, #33265, #40398, #26054, #4211, #7584, #44693, #40625, #29918, #7821, #22916, #26533, #41093, #22438, #19068, #37058, #33739, #22198, #36834, #32788, #47383, #3985, #18840, #611, #29225, #37529, #14555, #43773, #44464, #10976, #11677, #22681, #40164, #7364, #3756, #18379, #23630, #34905, #9492, #45171, #5398, #37776, #23865, #38240, #20258, #5647, #26769, #4929, #45415, #15750, #42044, #12860, #34200, #38477, #1565, #2046, #1327, #5167, #8527, #45886, #16218, #16681, #12146, #30848, #15984, #1810, #38718, #30606, #12393, #20022, #19553, #27014, #31308, #34419, #23157, #13098, #19786, #41560, #12629, #34662, #8767, #27731, #27254, #24112, #38006, #9247, #23403, #41806, #16448, #9005, #31079, #45643, #27493, #19317, #33966, #42295, #1093, #30385, #44931, #41327, #35136, #39394, #46362, #42985, #32249, #2279, #24338, #16907, #6100, #20723, #6579, #17603, #21190, #31546, #25035, #46829, #35367, #35824, #28178, #42738, #9954, #5888, #24565, #39166, #2972, #14017, #28664, #43230, #21430, #17845, #47073, #14266, #31849, #28247, #10509, #24639, #46903, #6884, #35672, #2809, #28492, #43062, #31295, #30839, #35586, #38925, #46349, #9236, #34895, #13313, #45406, #45876, #6087, #16205, #31764, #5389, #12850, #12617, #9483, #42729, #20713, #27941, #8996, #35354, #42033, #27241, #5878, #2500, #41796, #9715, #2036, #13088, #2267, #16666, #42510, #20008, #46115, #24327, #27482, #17124, #20484, #13533, #28168, #27718, #24098, #1801, #9943, #38708, #24549, #39157, #6327, #20946, #42284, #23853, #35120, #23619, #34650, #38466, #38230, #16437, #31068, #45631, #5637, #20247, #16890, #31533, #31993, #43216, #2729, #73, #10426, #47309, #7288, #10182, #6801, #17358, #39857, #3207, #32717, #25530, #21421, #42972, #17837, #36049, #6570, #32481, #32952, #29392, #21180, #47060, #18069, #36304, #36531, #35812, #3688, #14719 ),
 ( #39385, #18312, #40095, #14255, #40326, #14483, #24788, #10661, #14006, #46584, #28404, #25756, #25027, #2959, #7510, #43696, #3455, #29143, #39623, #17596, #28897, #32238, #43938, #21909, #43456, #22132, #10906, #25268, #13764, #11134, #7047, #21674, #8453, #41024, #41251, #29846, #33428, #8693, #36760, #7984, #4367, #773, #33195, #23082, #18540, #37699, #37458, #26935, #44388, #11603, #26223, #44164, #37220, #18998, #8217, #4853, #3916, #15197, #22844, #7749, #1256, #4608, #15911, #30536, #11365, #22364, #15432, #316, #12072, #30312, #4145, #45098, #33659, #14965, #18768, #44622, #25973, #29625, #19240, #40558, #36990, #33899, #541, #1019, #40790, #15677, #44863, #26696, #12787, #27423, #27888, #13259, #13705, #40034, #43156, #17536, #24971, #28838, #35758, #7230, #6743, #14660, #28593, #47246, #6507, #21125, #39793, #2898, #10120, #21361, #28341, #29332, #9886, #14428, #10366, #21850, #29080, #42912, #24500, #43395, #32170, #35989, #3394, #39093, #46760, #20892, #13946, #2671, #10607, #21610, #25206, #17302, #43637, #3150, #10, #36475, #3629, #6986, #10847, #18005, #32893, #39566, #17775, #31936, #46525, #32660, #12739, #23739, #19663, #16782, #12503, #45999, #9363, #20601, #23516, #34525, #27369, #27126, #1920, #23986, #5762, #9601, #5981, #23794, #31472, #16384, #2441, #2213, #46295, #31710, #5329, #31004, #24045, #8942, #20657, #38872, #27429, #13487, #42223, #28116, #38408, #31239, #1740, #24504, #38646, #9891, #19949, #5820, #5581, #27893, #17307, #34837, #1982, #46056, #45816, #13024, #39098, #20428, #35062, #6271, #13264, #42456, #9660, #24276, #6036, #35536, #35305, #2677, #45347, #12559, #27185, #46766, #14433, #13950, #32178, #28842, #2906, #36706, #3869, #21856, #3155, #29341, #3637, #17541, #46529, #36250, #24977, #10612, #10855, #13711, #35764, #28347, #28602, #24736, #32665, #43645, #47252, #10127, #18257, #25467, #39333, #39800, #43164, #42917, #6511, #7460, #39572, #21131, #31943, #40039, #18012, #29086, #6748, #21369, #14198, #35996, #32899, #36482, #43401, #22083, #7236, #3401, #17779, #14667, #25209, #32428, #47006, #17, #6991, #21616, #43884, #11084, #25704, #40275, #36941, #23276, #37892, #8404, #37170, #15862, #37647, #4093, #33137, #22791, #44340, #44573, #44815, #265, #22311, #14909, #18716, #11312, #19188, #30264, #33846, #44117, #4800, #12025, #25926, #26410, #15148, #29571, #40508, #8639, #29793, #7697, #18487, #26650, #4553, #967, #11548, #33373, #722, #492, #19429, #23031, #30031, #26170, #15625, #15383, #40739, #30486, #45046, #8164, #34081, #37398, #1209, #7935, #22551, #4314, #18947, #11793, #40976, #41198, #12260, #26883, #34309, #24229, #5767, #42631, #45522, #27376, #41916, #12508, #23742, #20139, #9369, #20608, #9838, #30956, #38592, #23520, #9608, #23993, #5987, #38824, #27133, #38123, #31188, #1439, #27846, #46005, #19901, #35253, #34785, #2389, #34531, #38351, #41681, #31660, #1926, #17023, #45292, #16558, #1686, #35012, #24448, #16333, #12745, #20372, #5283, #9127, #46235, #45761, #8888, #13438, #5525, #12972, #27608, #28068, #42163, #5050, #2160, #16788, #31426, #19669, #13211, #16099, #42407, #30722, #374, #15255, #47368, #44217, #26035, #33480, #40611, #18824, #19056, #598, #44445, #30138, #44678, #41078, #37515, #40150, #7350, #17832, #31989, #10656, #39151, #43212, #46346, #13529, #35810, #28165, #42724, #46579, #6322, #25264, #20481, #25022, #20942, #32477, #6798, #35582, #2263, #2954, #28401, #42968, #32235, #16887, #17592, #31528, #21416, #13310, #47056, #4142, #40553, #18065, #11596, #18763, #32712, #312, #36527, #21668, #47304, #15428, #3683, #29138, #44615, #33423, #25969, #7745, #18306, #43693, #22127, #10899, #40785, #29841, #3912, #30078, #22359, #36754, #11831, #37214, #4361, #29621, #26219, #44161, #44384, #32948, #68, #39853, #7043, #11131, #7507, #18534, #36300, #7980, #3452, #22602, #537, #25523, #14713, #29387, #43934, #40090, #25753, #33188, #11361, #18995, #7285, #40322, #15193, #21905, #33653, #768, #14959, #12781, #33893, #12068, #5088, #22838, #1729, #19940, #41244, #30772, #45561, #27175, #30998, #12310, #37694, #45804, #26455, #26930, #41481, #37936, #37452, #27417, #8210, #41960, #41727, #31227, #8687, #34351, #23555, #44858, #5322, #34575, #16373, #9168, #41020, #38397, #20178, #34828, #1971, #4602, #13941, #46752, #20418, #27882, #39086, #9412, #35753, #21117, #2432, #32161, #42667, #43148, #46285, #13474, #2202, #6736, #24493, #21353, #35053, #20885, #28107, #24723, #32415, #35527, #2666, #13699, #17297, #31930, #17530, #46519, #16820, #35983, #28333, #2889, #3139, #17767, #13011, #27654, #42209, #24030, #38635, #32596, #36759, #3915, #44387, #18539, #14718, #11364, #72, #29142, #43695, #33658, #40557, #11835, #30085, #22363, #10905, #11602, #7983, #22606, #37219, #40094, #18311, #21908, #44621, #3687, #26462, #41023, #8216, #37457, #4607, #12786, #41250, #23561, #45097, #30311, #8452, #24039, #12317, #37698, #5815, #41966, #34582, #1735, #26934, #4852, #45342, #19477, #1976, #38402, #27179, #38642, #9171, #5325, #20424, #45811, #13019, #19945, #16607, #30535, #34354, #41486, #42217, #23790, #31233, #8692, #20184, #23327, #34832, #1018, #37941, #5092, #9420, #19715, #16145, #15676, #44862, #46290, #17774, #17301, #42674, #46524, #6506, #24499, #14192, #13704, #46051, #28340, #28837, #42911, #10119, #17535, #32169, #10365, #27887, #42448, #40969, #32659, #11540, #40270, #33604, #40734, #40033, #47245, #25921, #9, #257, #487, #14427, #25461, #29079, #7229, #43636, #33368, #15142, #29790, #10846, #7928, #44336, #36474, #29566, #18250, #32892, #29331, #11788, #43877, #25698, #7456, #22547, #7690, #37163, #22077, #36702, #3863, #18483, #4310, #717, #33131, #14904, #15377, #19662, #22786, #37394, #4549, #45287, #9123, #23515, #19182, #1204, #45041, #15620, #30260, #41439, #34305, #1432, #8635, #16093, #30714, #38119, #18527, #22593, #10892, #40082, #7279, #25256, #36519, #32940, #22119, #33415, #37207, #43684, #3904, #3444, #36976, #36745, #18755, #4132, #39845, #18057, #43924, #14243, #40543, #11353, #32703, #530, #29833, #29612, #10650, #44376, #25513, #28884, #7499, #11586, #17824, #25962, #3674, #14706, #304, #18297, #14950, #47294, #44153, #26211, #14474, #43446, #7034, #29129, #21897, #25744, #12296, #4591, #16130, #26920 ) ),
 .UNSPECIFIED., .F., .F., .T. ) 
 B_SPLINE_SURFACE_WITH_KNOTS ( ( 2, 2 ),
 ( 3, 2, 2, 2, 2, 2, 2, 2, 2, 2, 2, 2, 2, 2, 2, 2, 2, 2, 2, 2, 2, 2, 2, 2, 2, 2, 2, 2, 2, 2, 2, 2, 2, 2, 2, 2, 2, 2, 2, 2, 2, 2, 2, 2, 2, 2, 2, 2, 2, 2, 2, 2, 2, 2, 2, 2, 2, 2, 2, 2, 2, 2, 2, 2, 2, 2, 2, 2, 2, 2, 2, 2, 2, 2, 2, 2, 2, 2, 2, 2, 2, 2, 2, 2, 2, 2, 2, 2, 2, 2, 2, 2, 2, 2, 2, 2, 2, 2, 2, 2, 2, 2, 2, 2, 2, 2, 2, 2, 2, 2, 2, 2, 2, 2, 2, 2, 2, 2, 2, 2, 2, 2, 2, 2, 2, 2, 2, 2, 2, 2, 2, 2, 2, 2, 2, 2, 2, 2, 2, 2, 2, 2, 2, 2, 2, 2, 2, 2, 2, 2, 2, 2, 2, 2, 2, 2, 2, 2, 2, 2, 2, 2, 2, 2, 2, 2, 2, 2, 2, 2, 2, 2, 2, 2, 2, 2, 2, 2, 2, 2, 2, 2, 2, 2, 2, 2, 2, 2, 2, 2, 2, 2, 2, 2, 2, 2, 2, 2, 2, 2, 2, 2, 2, 2, 2, 2, 2, 2, 2, 2, 2, 2, 2, 2, 2, 2, 2, 2, 2, 2, 2, 2, 2, 2, 2, 2, 2, 2, 2, 2, 2, 2, 2, 2, 2, 2, 2, 2, 2, 2, 2, 2, 2, 2, 2, 2, 2, 2, 2, 2, 2, 2, 2, 2, 2, 2, 2, 2, 2, 2, 2, 2, 2, 2, 2, 2, 2, 2, 2, 2, 2, 2, 2, 2, 2, 2, 2, 2, 2, 2, 2, 2, 2, 2, 2, 2, 2, 2, 2, 2, 2, 2, 2, 2, 2, 2, 2, 2, 2, 2, 2, 2, 2, 2, 2, 2, 2, 2, 2, 2, 2, 2, 2, 2, 2, 2, 2, 2, 2, 2, 2, 2, 2, 2, 2, 2, 2, 2, 2, 2, 2, 2, 2, 2, 2, 2, 2, 2, 2, 2, 2, 2, 2, 2, 2, 2, 2, 2, 2, 2, 2, 2, 2, 2, 2, 2, 2, 2, 2, 2, 2, 2, 2, 2, 2, 2, 2, 2, 2, 2, 2, 2, 2, 2, 2, 2, 2, 2, 2, 2, 2, 2, 2, 2, 2, 2, 2, 2, 2, 2, 2, 2, 2, 2, 2, 2, 2, 2, 2, 2, 3 ),
 ( 0.000000000000000000, 1.000000000000000000 ),
 ( 0.000000000000000000, 0.002500000000000000052, 0.005000000000000000104, 0.007499999999999999722, 0.01000000000000000021, 0.01250000000000000069, 0.01499999999999999944, 0.01750000000000000167, 0.02000000000000000042, 0.02249999999999999917, 0.02500000000000000139, 0.02750000000000000014, 0.02999999999999999889, 0.03250000000000000111, 0.03500000000000000333, 0.03749999999999999861, 0.04000000000000000083, 0.04250000000000000305, 0.04499999999999999833, 0.04750000000000000056, 0.05000000000000000278, 0.05249999999999999806, 0.05500000000000000028, 0.05750000000000000250, 0.05999999999999999778, 0.06250000000000000000, 0.06500000000000000222, 0.06750000000000000444, 0.07000000000000000666, 0.07249999999999999500, 0.07499999999999999722, 0.07749999999999999944, 0.08000000000000000167, 0.08250000000000000389, 0.08500000000000000611, 0.08749999999999999445, 0.08999999999999999667, 0.09249999999999999889, 0.09500000000000000111, 0.09750000000000000333, 0.1000000000000000056, 0.1024999999999999939, 0.1049999999999999961, 0.1074999999999999983, 0.1100000000000000006, 0.1125000000000000028, 0.1150000000000000050, 0.1174999999999999933, 0.1199999999999999956, 0.1224999999999999978, 0.1250000000000000000, 0.1275000000000000022, 0.1300000000000000044, 0.1325000000000000067, 0.1350000000000000089, 0.1375000000000000111, 0.1400000000000000133, 0.1424999999999999878, 0.1449999999999999900, 0.1474999999999999922, 0.1499999999999999944, 0.1524999999999999967, 0.1549999999999999989, 0.1575000000000000011, 0.1600000000000000033, 0.1625000000000000056, 0.1650000000000000078, 0.1675000000000000100, 0.1700000000000000122, 0.1724999999999999867, 0.1749999999999999889, 0.1774999999999999911, 0.1799999999999999933, 0.1824999999999999956, 0.1849999999999999978, 0.1875000000000000000, 0.1900000000000000022, 0.1925000000000000044, 0.1950000000000000067, 0.1975000000000000089, 0.2000000000000000111, 0.2025000000000000133, 0.2049999999999999878, 0.2074999999999999900, 0.2099999999999999922, 0.2124999999999999944, 0.2149999999999999967, 0.2174999999999999989, 0.2200000000000000011, 0.2225000000000000033, 0.2250000000000000056, 0.2275000000000000078, 0.2300000000000000100, 0.2325000000000000122, 0.2349999999999999867, 0.2374999999999999889, 0.2399999999999999911, 0.2424999999999999933, 0.2449999999999999956, 0.2474999999999999978, 0.2500000000000000000, 0.2525000000000000022, 0.2550000000000000044, 0.2575000000000000067, 0.2600000000000000089, 0.2625000000000000111, 0.2650000000000000133, 0.2675000000000000155, 0.2700000000000000178, 0.2725000000000000200, 0.2750000000000000222, 0.2775000000000000244, 0.2800000000000000266, 0.2824999999999999734, 0.2849999999999999756, 0.2874999999999999778, 0.2899999999999999800, 0.2924999999999999822, 0.2949999999999999845, 0.2974999999999999867, 0.2999999999999999889, 0.3024999999999999911, 0.3049999999999999933, 0.3074999999999999956, 0.3099999999999999978, 0.3125000000000000000, 0.3150000000000000022, 0.3175000000000000044, 0.3200000000000000067, 0.3225000000000000089, 0.3250000000000000111, 0.3275000000000000133, 0.3300000000000000155, 0.3325000000000000178, 0.3350000000000000200, 0.3375000000000000222, 0.3400000000000000244, 0.3425000000000000266, 0.3449999999999999734, 0.3474999999999999756, 0.3499999999999999778, 0.3524999999999999800, 0.3549999999999999822, 0.3574999999999999845, 0.3599999999999999867, 0.3624999999999999889, 0.3649999999999999911, 0.3674999999999999933, 0.3699999999999999956, 0.3724999999999999978, 0.3750000000000000000, 0.3775000000000000022, 0.3800000000000000044, 0.3825000000000000067, 0.3850000000000000089, 0.3875000000000000111, 0.3900000000000000133, 0.3925000000000000155, 0.3950000000000000178, 0.3975000000000000200, 0.4000000000000000222, 0.4025000000000000244, 0.4050000000000000266, 0.4074999999999999734, 0.4099999999999999756, 0.4124999999999999778, 0.4149999999999999800, 0.4174999999999999822, 0.4199999999999999845, 0.4224999999999999867, 0.4249999999999999889, 0.4274999999999999911, 0.4299999999999999933, 0.4324999999999999956, 0.4349999999999999978, 0.4375000000000000000, 0.4400000000000000022, 0.4425000000000000044, 0.4450000000000000067, 0.4475000000000000089, 0.4500000000000000111, 0.4525000000000000133, 0.4550000000000000155, 0.4575000000000000178, 0.4600000000000000200, 0.4625000000000000222, 0.4650000000000000244, 0.4675000000000000266, 0.4699999999999999734, 0.4724999999999999756, 0.4749999999999999778, 0.4774999999999999800, 0.4799999999999999822, 0.4824999999999999845, 0.4849999999999999867, 0.4874999999999999889, 0.4899999999999999911, 0.4924999999999999933, 0.4949999999999999956, 0.4974999999999999978, 0.5000000000000000000, 0.5024999999999999467, 0.5050000000000000044, 0.5074999999999999512, 0.5100000000000000089, 0.5124999999999999556, 0.5150000000000000133, 0.5174999999999999600, 0.5200000000000000178, 0.5224999999999999645, 0.5250000000000000222, 0.5274999999999999689, 0.5300000000000000266, 0.5324999999999999734, 0.5350000000000000311, 0.5374999999999999778, 0.5400000000000000355, 0.5424999999999999822, 0.5450000000000000400, 0.5474999999999999867, 0.5500000000000000444, 0.5524999999999999911, 0.5550000000000000488, 0.5574999999999999956, 0.5600000000000000533, 0.5625000000000000000, 0.5649999999999999467, 0.5675000000000000044, 0.5699999999999999512, 0.5725000000000000089, 0.5749999999999999556, 0.5775000000000000133, 0.5799999999999999600, 0.5825000000000000178, 0.5849999999999999645, 0.5875000000000000222, 0.5899999999999999689, 0.5925000000000000266, 0.5949999999999999734, 0.5975000000000000311, 0.5999999999999999778, 0.6025000000000000355, 0.6049999999999999822, 0.6075000000000000400, 0.6099999999999999867, 0.6125000000000000444, 0.6149999999999999911, 0.6175000000000000488, 0.6199999999999999956, 0.6225000000000000533, 0.6250000000000000000, 0.6274999999999999467, 0.6300000000000000044, 0.6324999999999999512, 0.6350000000000000089, 0.6374999999999999556, 0.6400000000000000133, 0.6424999999999999600, 0.6450000000000000178, 0.6474999999999999645, 0.6500000000000000222, 0.6524999999999999689, 0.6550000000000000266, 0.6574999999999999734, 0.6600000000000000311, 0.6624999999999999778, 0.6650000000000000355, 0.6674999999999999822, 0.6700000000000000400, 0.6724999999999999867, 0.6750000000000000444, 0.6774999999999999911, 0.6800000000000000488, 0.6824999999999999956, 0.6850000000000000533, 0.6875000000000000000, 0.6899999999999999467, 0.6925000000000000044, 0.6949999999999999512, 0.6975000000000000089, 0.6999999999999999556, 0.7025000000000000133, 0.7049999999999999600, 0.7075000000000000178, 0.7099999999999999645, 0.7125000000000000222, 0.7149999999999999689, 0.7175000000000000266, 0.7199999999999999734, 0.7225000000000000311, 0.7249999999999999778, 0.7275000000000000355, 0.7299999999999999822, 0.7325000000000000400, 0.7349999999999999867, 0.7375000000000000444, 0.7399999999999999911, 0.7425000000000000488, 0.7449999999999999956, 0.7475000000000000533, 0.7500000000000000000, 0.7524999999999999467, 0.7550000000000000044, 0.7574999999999999512, 0.7600000000000000089, 0.7624999999999999556, 0.7650000000000000133, 0.7674999999999999600, 0.7700000000000000178, 0.7724999999999999645, 0.7750000000000000222, 0.7774999999999999689, 0.7800000000000000266, 0.7824999999999999734, 0.7850000000000000311, 0.7874999999999999778, 0.7900000000000000355, 0.7924999999999999822, 0.7950000000000000400, 0.7974999999999999867, 0.8000000000000000444, 0.8024999999999999911, 0.8050000000000000488, 0.8074999999999999956, 0.8100000000000000533, 0.8125000000000000000, 0.8149999999999999467, 0.8175000000000000044, 0.8199999999999999512, 0.8225000000000000089, 0.8249999999999999556, 0.8275000000000000133, 0.8299999999999999600, 0.8325000000000000178, 0.8349999999999999645, 0.8375000000000000222, 0.8399999999999999689, 0.8425000000000000266, 0.8449999999999999734, 0.8475000000000000311, 0.8499999999999999778, 0.8525000000000000355, 0.8549999999999999822, 0.8575000000000000400, 0.8599999999999999867, 0.8625000000000000444, 0.8649999999999999911, 0.8675000000000000488, 0.8699999999999999956, 0.8725000000000000533, 0.8750000000000000000, 0.8774999999999999467, 0.8800000000000000044, 0.8824999999999999512, 0.8850000000000000089, 0.8874999999999999556, 0.8900000000000000133, 0.8924999999999999600, 0.8950000000000000178, 0.8974999999999999645, 0.9000000000000000222, 0.9024999999999999689, 0.9050000000000000266, 0.9074999999999999734, 0.9100000000000000311, 0.9124999999999999778, 0.9150000000000000355, 0.9174999999999999822, 0.9200000000000000400, 0.9224999999999999867, 0.9250000000000000444, 0.9274999999999999911, 0.9300000000000000488, 0.9324999999999999956, 0.9350000000000000533, 0.9375000000000000000, 0.9399999999999999467, 0.9425000000000000044, 0.9449999999999999512, 0.9475000000000000089, 0.9499999999999999556, 0.9525000000000000133, 0.9549999999999999600, 0.9575000000000000178, 0.9599999999999999645, 0.9625000000000000222, 0.9649999999999999689, 0.9675000000000000266, 0.9699999999999999734, 0.9725000000000000311, 0.9749999999999999778, 0.9775000000000000355, 0.9799999999999999822, 0.9825000000000000400, 0.9849999999999999867, 0.9875000000000000444, 0.9899999999999999911, 0.9925000000000000488, 0.9949999999999999956, 0.9975000000000000533, 1.000000000000000000 ),
 .UNSPECIFIED. ) 
 GEOMETRIC_REPRESENTATION_ITEM ( )  RATIONAL_B_SPLINE_SURFACE ( (
 ( 1.000000000000000000, 0.9238795325112869605, 1.000000000000000000, 0.9238795325112869605, 1.000000000000000000, 0.9238795325112869605, 1.000000000000000000, 0.9238795325112869605, 1.000000000000000000, 0.9238795325112869605, 1.000000000000000000, 0.9238795325112869605, 1.000000000000000000, 0.9238795325112869605, 1.000000000000000000, 0.9238795325112869605, 1.000000000000000000, 0.9238795325112869605, 1.000000000000000000, 0.9238795325112869605, 1.000000000000000000, 0.9238795325112869605, 1.000000000000000000, 0.9238795325112869605, 1.000000000000000000, 0.9238795325112869605, 1.000000000000000000, 0.9238795325112869605, 1.000000000000000000, 0.9238795325112869605, 1.000000000000000000, 0.9238795325112869605, 1.000000000000000000, 0.9238795325112869605, 1.000000000000000000, 0.9238795325112869605, 1.000000000000000000, 0.9238795325112869605, 1.000000000000000000, 0.9238795325112869605, 1.000000000000000000, 0.9238795325112869605, 1.000000000000000000, 0.9238795325112869605, 1.000000000000000000, 0.9238795325112869605, 1.000000000000000000, 0.9238795325112869605, 1.000000000000000000, 0.9238795325112869605, 1.000000000000000000, 0.9238795325112869605, 1.000000000000000000, 0.9238795325112869605, 1.000000000000000000, 0.9238795325112869605, 1.000000000000000000, 0.9238795325112869605, 1.000000000000000000, 0.9238795325112869605, 1.000000000000000000, 0.9238795325112869605, 1.000000000000000000, 0.9238795325112869605, 1.000000000000000000, 0.9238795325112869605, 1.000000000000000000, 0.9238795325112869605, 1.000000000000000000, 0.9238795325112869605, 1.000000000000000000, 0.9238795325112869605, 1.000000000000000000, 0.9238795325112869605, 1.000000000000000000, 0.9238795325112869605, 1.000000000000000000, 0.9238795325112869605, 1.000000000000000000, 0.9238795325112869605, 1.000000000000000000, 0.9238795325112869605, 1.000000000000000000, 0.9238795325112869605, 1.000000000000000000, 0.9238795325112869605, 1.000000000000000000, 0.9238795325112869605, 1.000000000000000000, 0.9238795325112869605, 1.000000000000000000, 0.9238795325112869605, 1.000000000000000000, 0.9238795325112869605, 1.000000000000000000, 0.9238795325112869605, 1.000000000000000000, 0.9238795325112869605, 1.000000000000000000, 0.9238795325112869605, 1.000000000000000000, 0.9238795325112869605, 1.000000000000000000, 0.9238795325112869605, 1.000000000000000000, 0.9238795325112869605, 1.000000000000000000, 0.9238795325112869605, 1.000000000000000000, 0.9238795325112869605, 1.000000000000000000, 0.9238795325112869605, 1.000000000000000000, 0.9238795325112869605, 1.000000000000000000, 0.9238795325112869605, 1.000000000000000000, 0.9238795325112869605, 1.000000000000000000, 0.9238795325112869605, 1.000000000000000000, 0.9238795325112869605, 1.000000000000000000, 0.9238795325112869605, 1.000000000000000000, 0.9238795325112869605, 1.000000000000000000, 0.9238795325112869605, 1.000000000000000000, 0.9238795325112869605, 1.000000000000000000, 0.9238795325112869605, 1.000000000000000000, 0.9238795325112869605, 1.000000000000000000, 0.9238795325112869605, 1.000000000000000000, 0.9238795325112869605, 1.000000000000000000, 0.9238795325112869605, 1.000000000000000000, 0.9238795325112869605, 1.000000000000000000, 0.9238795325112869605, 1.000000000000000000, 0.9238795325112869605, 1.000000000000000000, 0.9238795325112869605, 1.000000000000000000, 0.9238795325112869605, 1.000000000000000000, 0.9238795325112869605, 1.000000000000000000, 0.9238795325112869605, 1.000000000000000000, 0.9238795325112869605, 1.000000000000000000, 0.9238795325112869605, 1.000000000000000000, 0.9238795325112869605, 1.000000000000000000, 0.9238795325112869605, 1.000000000000000000, 0.9238795325112869605, 1.000000000000000000, 0.9238795325112869605, 1.000000000000000000, 0.9238795325112869605, 1.000000000000000000, 0.9238795325112869605, 1.000000000000000000, 0.9238795325112869605, 1.000000000000000000, 0.9238795325112869605, 1.000000000000000000, 0.9238795325112869605, 1.000000000000000000, 0.9238795325112869605, 1.000000000000000000, 0.9238795325112869605, 1.000000000000000000, 0.9238795325112869605, 1.000000000000000000, 0.9238795325112869605, 1.000000000000000000, 0.9238795325112869605, 1.000000000000000000, 0.9238795325112869605, 1.000000000000000000, 0.9238795325112869605, 1.000000000000000000, 0.9238795325112869605, 1.000000000000000000, 0.9238795325112869605, 1.000000000000000000, 0.9238795325112869605, 1.000000000000000000, 0.9238795325112869605, 1.000000000000000000, 0.9238795325112869605, 1.000000000000000000, 0.9238795325112869605, 1.000000000000000000, 0.9238795325112869605, 1.000000000000000000, 0.9238795325112869605, 1.000000000000000000, 0.9238795325112869605, 1.000000000000000000, 0.9238795325112869605, 1.000000000000000000, 0.9238795325112869605, 1.000000000000000000, 0.9238795325112869605, 1.000000000000000000, 0.9238795325112869605, 1.000000000000000000, 0.9238795325112869605, 1.000000000000000000, 0.9238795325112869605, 1.000000000000000000, 0.9238795325112869605, 1.000000000000000000, 0.9238795325112869605, 1.000000000000000000, 0.9238795325112869605, 1.000000000000000000, 0.9238795325112869605, 1.000000000000000000, 0.9238795325112869605, 1.000000000000000000, 0.9238795325112869605, 1.000000000000000000, 0.9238795325112869605, 1.000000000000000000, 0.9238795325112869605, 1.000000000000000000, 0.9238795325112869605, 1.000000000000000000, 0.9238795325112869605, 1.000000000000000000, 0.9238795325112869605, 1.000000000000000000, 0.9238795325112869605, 1.000000000000000000, 0.9238795325112869605, 1.000000000000000000, 0.9238795325112869605, 1.000000000000000000, 0.9238795325112869605, 1.000000000000000000, 0.9238795325112869605, 1.000000000000000000, 0.9238795325112869605, 1.000000000000000000, 0.9238795325112869605, 1.000000000000000000, 0.9238795325112869605, 1.000000000000000000, 0.9238795325112869605, 1.000000000000000000, 0.9238795325112869605, 1.000000000000000000, 0.9238795325112869605, 1.000000000000000000, 0.9238795325112869605, 1.000000000000000000, 0.9238795325112869605, 1.000000000000000000, 0.9238795325112869605, 1.000000000000000000, 0.9238795325112869605, 1.000000000000000000, 0.9238795325112869605, 1.000000000000000000, 0.9238795325112869605, 1.000000000000000000, 0.9238795325112869605, 1.000000000000000000, 0.9238795325112869605, 1.000000000000000000, 0.9238795325112869605, 1.000000000000000000, 0.9238795325112869605, 1.000000000000000000, 0.9238795325112869605, 1.000000000000000000, 0.9238795325112869605, 1.000000000000000000, 0.9238795325112869605, 1.000000000000000000, 0.9238795325112869605, 1.000000000000000000, 0.9238795325112869605, 1.000000000000000000, 0.9238795325112869605, 1.000000000000000000, 0.9238795325112869605, 1.000000000000000000, 0.9238795325112869605, 1.000000000000000000, 0.9238795325112869605, 1.000000000000000000, 0.9238795325112869605, 1.000000000000000000, 0.9238795325112869605, 1.000000000000000000, 0.9238795325112869605, 1.000000000000000000, 0.9238795325112869605, 1.000000000000000000, 0.9238795325112869605, 1.000000000000000000, 0.9238795325112869605, 1.000000000000000000, 0.9238795325112869605, 1.000000000000000000, 0.9238795325112869605, 1.000000000000000000, 0.9238795325112869605, 1.000000000000000000, 0.9238795325112869605, 1.000000000000000000, 0.9238795325112869605, 1.000000000000000000, 0.9238795325112869605, 1.000000000000000000, 0.9238795325112869605, 1.000000000000000000, 0.9238795325112869605, 1.000000000000000000, 0.9238795325112869605, 1.000000000000000000, 0.9238795325112869605, 1.000000000000000000, 0.9238795325112869605, 1.000000000000000000, 0.9238795325112869605, 1.000000000000000000, 0.9238795325112869605, 1.000000000000000000, 0.9238795325112869605, 1.000000000000000000, 0.9238795325112869605, 1.000000000000000000, 0.9238795325112869605, 1.000000000000000000, 0.9238795325112869605, 1.000000000000000000, 0.9238795325112869605, 1.000000000000000000, 0.9238795325112869605, 1.000000000000000000, 0.9238795325112869605, 1.000000000000000000, 0.9238795325112869605, 1.000000000000000000, 0.9238795325112869605, 1.000000000000000000, 0.9238795325112869605, 1.000000000000000000, 0.9238795325112869605, 1.000000000000000000, 0.9238795325112869605, 1.000000000000000000, 0.9238795325112869605, 1.000000000000000000, 0.9238795325112869605, 1.000000000000000000, 0.9238795325112869605, 1.000000000000000000, 0.9238795325112869605, 1.000000000000000000, 0.9238795325112869605, 1.000000000000000000, 0.9238795325112869605, 1.000000000000000000, 0.9238795325112869605, 1.000000000000000000, 0.9238795325112869605, 1.000000000000000000, 0.9238795325112869605, 1.000000000000000000, 0.9238795325112869605, 1.000000000000000000, 0.9238795325112869605, 1.000000000000000000, 0.9238795325112869605, 1.000000000000000000, 0.9238795325112869605, 1.000000000000000000, 0.9238795325112869605, 1.000000000000000000, 0.9238795325112869605, 1.000000000000000000, 0.9238795325112869605, 1.000000000000000000, 0.9238795325112869605, 1.000000000000000000, 0.9238795325112869605, 1.000000000000000000, 0.9238795325112869605, 1.000000000000000000, 0.9238795325112869605, 1.000000000000000000, 0.9238795325112869605, 1.000000000000000000, 0.9238795325112869605, 1.000000000000000000, 0.9238795325112869605, 1.000000000000000000, 0.9238795325112869605, 1.000000000000000000, 0.9238795325112869605, 1.000000000000000000, 0.9238795325112869605, 1.000000000000000000, 0.9238795325112869605, 1.000000000000000000, 0.9238795325112869605, 1.000000000000000000, 0.9238795325112869605, 1.000000000000000000, 0.9238795325112869605, 1.000000000000000000, 0.9238795325112869605, 1.000000000000000000, 0.9238795325112869605, 1.000000000000000000, 0.9238795325112869605, 1.000000000000000000, 0.9238795325112869605, 1.000000000000000000, 0.9238795325112869605, 1.000000000000000000, 0.9238795325112869605, 1.000000000000000000, 0.9238795325112869605, 1.000000000000000000, 0.9238795325112869605, 1.000000000000000000, 0.9238795325112869605, 1.000000000000000000, 0.9238795325112869605, 1.000000000000000000, 0.9238795325112869605, 1.000000000000000000, 0.9238795325112869605, 1.000000000000000000, 0.9238795325112869605, 1.000000000000000000, 0.9238795325112869605, 1.000000000000000000, 0.9238795325112869605, 1.000000000000000000, 0.9238795325112869605, 1.000000000000000000, 0.9238795325112869605, 1.000000000000000000, 0.9238795325112869605, 1.000000000000000000, 0.9238795325112869605, 1.000000000000000000, 0.9238795325112869605, 1.000000000000000000, 0.9238795325112869605, 1.000000000000000000, 0.9238795325112869605, 1.000000000000000000, 0.9238795325112869605, 1.000000000000000000, 0.9238795325112869605, 1.000000000000000000, 0.9238795325112869605, 1.000000000000000000, 0.9238795325112869605, 1.000000000000000000, 0.9238795325112869605, 1.000000000000000000, 0.9238795325112869605, 1.000000000000000000, 0.9238795325112869605, 1.000000000000000000, 0.9238795325112869605, 1.000000000000000000, 0.9238795325112869605, 1.000000000000000000, 0.9238795325112869605, 1.000000000000000000, 0.9238795325112869605, 1.000000000000000000, 0.9238795325112869605, 1.000000000000000000, 0.9238795325112869605, 1.000000000000000000, 0.9238795325112869605, 1.000000000000000000, 0.9238795325112869605, 1.000000000000000000, 0.9238795325112869605, 1.000000000000000000, 0.9238795325112869605, 1.000000000000000000, 0.9238795325112869605, 1.000000000000000000, 0.9238795325112869605, 1.000000000000000000, 0.9238795325112869605, 1.000000000000000000, 0.9238795325112869605, 1.000000000000000000, 0.9238795325112869605, 1.000000000000000000, 0.9238795325112869605, 1.000000000000000000, 0.9238795325112869605, 1.000000000000000000, 0.9238795325112869605, 1.000000000000000000, 0.9238795325112869605, 1.000000000000000000, 0.9238795325112869605, 1.000000000000000000, 0.9238795325112869605, 1.000000000000000000, 0.9238795325112869605, 1.000000000000000000, 0.9238795325112869605, 1.000000000000000000, 0.9238795325112869605, 1.000000000000000000, 0.9238795325112869605, 1.000000000000000000, 0.9238795325112869605, 1.000000000000000000, 0.9238795325112869605, 1.000000000000000000, 0.9238795325112869605, 1.000000000000000000, 0.9238795325112869605, 1.000000000000000000, 0.9238795325112869605, 1.000000000000000000, 0.9238795325112869605, 1.000000000000000000, 0.9238795325112869605, 1.000000000000000000, 0.9238795325112869605, 1.000000000000000000, 0.9238795325112869605, 1.000000000000000000, 0.9238795325112869605, 1.000000000000000000, 0.9238795325112869605, 1.000000000000000000, 0.9238795325112869605, 1.000000000000000000, 0.9238795325112869605, 1.000000000000000000, 0.9238795325112869605, 1.000000000000000000, 0.9238795325112869605, 1.000000000000000000, 0.9238795325112869605, 1.000000000000000000, 0.9238795325112869605, 1.000000000000000000, 0.9238795325112869605, 1.000000000000000000, 0.9238795325112869605, 1.000000000000000000, 0.9238795325112869605, 1.000000000000000000, 0.9238795325112869605, 1.000000000000000000, 0.9238795325112869605, 1.000000000000000000, 0.9238795325112869605, 1.000000000000000000, 0.9238795325112869605, 1.000000000000000000, 0.9238795325112869605, 1.000000000000000000, 0.9238795325112869605, 1.000000000000000000, 0.9238795325112869605, 1.000000000000000000, 0.9238795325112869605, 1.000000000000000000, 0.9238795325112869605, 1.000000000000000000, 0.9238795325112869605, 1.000000000000000000, 0.9238795325112869605, 1.000000000000000000, 0.9238795325112869605, 1.000000000000000000, 0.9238795325112869605, 1.000000000000000000, 0.9238795325112869605, 1.000000000000000000, 0.9238795325112869605, 1.000000000000000000, 0.9238795325112869605, 1.000000000000000000, 0.9238795325112869605, 1.000000000000000000, 0.9238795325112869605, 1.000000000000000000, 0.9238795325112869605, 1.000000000000000000, 0.9238795325112869605, 1.000000000000000000, 0.9238795325112869605, 1.000000000000000000, 0.9238795325112869605, 1.000000000000000000, 0.9238795325112869605, 1.000000000000000000, 0.9238795325112869605, 1.000000000000000000, 0.9238795325112869605, 1.000000000000000000, 0.9238795325112869605, 1.000000000000000000, 0.9238795325112869605, 1.000000000000000000, 0.9238795325112869605, 1.000000000000000000, 0.9238795325112869605, 1.000000000000000000, 0.9238795325112869605, 1.000000000000000000, 0.9238795325112869605, 1.000000000000000000, 0.9238795325112869605, 1.000000000000000000, 0.9238795325112869605, 1.000000000000000000, 0.9238795325112869605, 1.000000000000000000, 0.9238795325112869605, 1.000000000000000000, 0.9238795325112869605, 1.000000000000000000, 0.9238795325112869605, 1.000000000000000000, 0.9238795325112869605, 1.000000000000000000, 0.9238795325112869605, 1.000000000000000000, 0.9238795325112869605, 1.000000000000000000, 0.9238795325112869605, 1.000000000000000000, 0.9238795325112869605, 1.000000000000000000, 0.9238795325112869605, 1.000000000000000000, 0.9238795325112869605, 1.000000000000000000, 0.9238795325112869605, 1.000000000000000000, 0.9238795325112869605, 1.000000000000000000, 0.9238795325112869605, 1.000000000000000000, 0.9238795325112869605, 1.000000000000000000, 0.9238795325112869605, 1.000000000000000000, 0.9238795325112869605, 1.000000000000000000, 0.9238795325112869605, 1.000000000000000000, 0.9238795325112869605, 1.000000000000000000, 0.9238795325112869605, 1.000000000000000000, 0.9238795325112869605, 1.000000000000000000, 0.9238795325112869605, 1.000000000000000000, 0.9238795325112869605, 1.000000000000000000, 0.9238795325112869605, 1.000000000000000000, 0.9238795325112869605, 1.000000000000000000, 0.9238795325112869605, 1.000000000000000000, 0.9238795325112869605, 1.000000000000000000, 0.9238795325112869605, 1.000000000000000000, 0.9238795325112869605, 1.000000000000000000, 0.9238795325112869605, 1.000000000000000000, 0.9238795325112869605, 1.000000000000000000, 0.9238795325112869605, 1.000000000000000000, 0.9238795325112869605, 1.000000000000000000, 0.9238795325112869605, 1.000000000000000000, 0.9238795325112869605, 1.000000000000000000, 0.9238795325112869605, 1.000000000000000000, 0.9238795325112869605, 1.000000000000000000, 0.9238795325112869605, 1.000000000000000000, 0.9238795325112869605, 1.000000000000000000, 0.9238795325112869605, 1.000000000000000000, 0.9238795325112869605, 1.000000000000000000, 0.9238795325112869605, 1.000000000000000000, 0.9238795325112869605, 1.000000000000000000, 0.9238795325112869605, 1.000000000000000000, 0.9238795325112869605, 1.000000000000000000, 0.9238795325112869605, 1.000000000000000000, 0.9238795325112869605, 1.000000000000000000, 0.9238795325112869605, 1.000000000000000000, 0.9238795325112869605, 1.000000000000000000, 0.9238795325112869605, 1.000000000000000000, 0.9238795325112869605, 1.000000000000000000, 0.9238795325112869605, 1.000000000000000000, 0.9238795325112869605, 1.000000000000000000, 0.9238795325112869605, 1.000000000000000000, 0.9238795325112869605, 1.000000000000000000, 0.9238795325112869605, 1.000000000000000000, 0.9238795325112869605, 1.000000000000000000, 0.9238795325112869605, 1.000000000000000000, 0.9238795325112869605, 1.000000000000000000, 0.9238795325112869605, 1.000000000000000000, 0.9238795325112869605, 1.000000000000000000, 0.9238795325112869605, 1.000000000000000000, 0.9238795325112869605, 1.000000000000000000, 0.9238795325112869605, 1.000000000000000000, 0.9238795325112869605, 1.000000000000000000, 0.9238795325112869605, 1.000000000000000000, 0.9238795325112869605, 1.000000000000000000, 0.9238795325112869605, 1.000000000000000000, 0.9238795325112869605, 1.000000000000000000, 0.9238795325112869605, 1.000000000000000000, 0.9238795325112869605, 1.000000000000000000, 0.9238795325112869605, 1.000000000000000000, 0.9238795325112869605, 1.000000000000000000, 0.9238795325112869605, 1.000000000000000000, 0.9238795325112869605, 1.000000000000000000, 0.9238795325112869605, 1.000000000000000000, 0.9238795325112869605, 1.000000000000000000, 0.9238795325112869605, 1.000000000000000000, 0.9238795325112869605, 1.000000000000000000, 0.9238795325112869605, 1.000000000000000000, 0.9238795325112869605, 1.000000000000000000),
 ( 1.000000000000000000, 0.9238795325112869605, 1.000000000000000000, 0.9238795325112869605, 1.000000000000000000, 0.9238795325112869605, 1.000000000000000000, 0.9238795325112869605, 1.000000000000000000, 0.9238795325112869605, 1.000000000000000000, 0.9238795325112869605, 1.000000000000000000, 0.9238795325112869605, 1.000000000000000000, 0.9238795325112869605, 1.000000000000000000, 0.9238795325112869605, 1.000000000000000000, 0.9238795325112869605, 1.000000000000000000, 0.9238795325112869605, 1.000000000000000000, 0.9238795325112869605, 1.000000000000000000, 0.9238795325112869605, 1.000000000000000000, 0.9238795325112869605, 1.000000000000000000, 0.9238795325112869605, 1.000000000000000000, 0.9238795325112869605, 1.000000000000000000, 0.9238795325112869605, 1.000000000000000000, 0.9238795325112869605, 1.000000000000000000, 0.9238795325112869605, 1.000000000000000000, 0.9238795325112869605, 1.000000000000000000, 0.9238795325112869605, 1.000000000000000000, 0.9238795325112869605, 1.000000000000000000, 0.9238795325112869605, 1.000000000000000000, 0.9238795325112869605, 1.000000000000000000, 0.9238795325112869605, 1.000000000000000000, 0.9238795325112869605, 1.000000000000000000, 0.9238795325112869605, 1.000000000000000000, 0.9238795325112869605, 1.000000000000000000, 0.9238795325112869605, 1.000000000000000000, 0.9238795325112869605, 1.000000000000000000, 0.9238795325112869605, 1.000000000000000000, 0.9238795325112869605, 1.000000000000000000, 0.9238795325112869605, 1.000000000000000000, 0.9238795325112869605, 1.000000000000000000, 0.9238795325112869605, 1.000000000000000000, 0.9238795325112869605, 1.000000000000000000, 0.9238795325112869605, 1.000000000000000000, 0.9238795325112869605, 1.000000000000000000, 0.9238795325112869605, 1.000000000000000000, 0.9238795325112869605, 1.000000000000000000, 0.9238795325112869605, 1.000000000000000000, 0.9238795325112869605, 1.000000000000000000, 0.9238795325112869605, 1.000000000000000000, 0.9238795325112869605, 1.000000000000000000, 0.9238795325112869605, 1.000000000000000000, 0.9238795325112869605, 1.000000000000000000, 0.9238795325112869605, 1.000000000000000000, 0.9238795325112869605, 1.000000000000000000, 0.9238795325112869605, 1.000000000000000000, 0.9238795325112869605, 1.000000000000000000, 0.9238795325112869605, 1.000000000000000000, 0.9238795325112869605, 1.000000000000000000, 0.9238795325112869605, 1.000000000000000000, 0.9238795325112869605, 1.000000000000000000, 0.9238795325112869605, 1.000000000000000000, 0.9238795325112869605, 1.000000000000000000, 0.9238795325112869605, 1.000000000000000000, 0.9238795325112869605, 1.000000000000000000, 0.9238795325112869605, 1.000000000000000000, 0.9238795325112869605, 1.000000000000000000, 0.9238795325112869605, 1.000000000000000000, 0.9238795325112869605, 1.000000000000000000, 0.9238795325112869605, 1.000000000000000000, 0.9238795325112869605, 1.000000000000000000, 0.9238795325112869605, 1.000000000000000000, 0.9238795325112869605, 1.000000000000000000, 0.9238795325112869605, 1.000000000000000000, 0.9238795325112869605, 1.000000000000000000, 0.9238795325112869605, 1.000000000000000000, 0.9238795325112869605, 1.000000000000000000, 0.9238795325112869605, 1.000000000000000000, 0.9238795325112869605, 1.000000000000000000, 0.9238795325112869605, 1.000000000000000000, 0.9238795325112869605, 1.000000000000000000, 0.9238795325112869605, 1.000000000000000000, 0.9238795325112869605, 1.000000000000000000, 0.9238795325112869605, 1.000000000000000000, 0.9238795325112869605, 1.000000000000000000, 0.9238795325112869605, 1.000000000000000000, 0.9238795325112869605, 1.000000000000000000, 0.9238795325112869605, 1.000000000000000000, 0.9238795325112869605, 1.000000000000000000, 0.9238795325112869605, 1.000000000000000000, 0.9238795325112869605, 1.000000000000000000, 0.9238795325112869605, 1.000000000000000000, 0.9238795325112869605, 1.000000000000000000, 0.9238795325112869605, 1.000000000000000000, 0.9238795325112869605, 1.000000000000000000, 0.9238795325112869605, 1.000000000000000000, 0.9238795325112869605, 1.000000000000000000, 0.9238795325112869605, 1.000000000000000000, 0.9238795325112869605, 1.000000000000000000, 0.9238795325112869605, 1.000000000000000000, 0.9238795325112869605, 1.000000000000000000, 0.9238795325112869605, 1.000000000000000000, 0.9238795325112869605, 1.000000000000000000, 0.9238795325112869605, 1.000000000000000000, 0.9238795325112869605, 1.000000000000000000, 0.9238795325112869605, 1.000000000000000000, 0.9238795325112869605, 1.000000000000000000, 0.9238795325112869605, 1.000000000000000000, 0.9238795325112869605, 1.000000000000000000, 0.9238795325112869605, 1.000000000000000000, 0.9238795325112869605, 1.000000000000000000, 0.9238795325112869605, 1.000000000000000000, 0.9238795325112869605, 1.000000000000000000, 0.9238795325112869605, 1.000000000000000000, 0.9238795325112869605, 1.000000000000000000, 0.9238795325112869605, 1.000000000000000000, 0.9238795325112869605, 1.000000000000000000, 0.9238795325112869605, 1.000000000000000000, 0.9238795325112869605, 1.000000000000000000, 0.9238795325112869605, 1.000000000000000000, 0.9238795325112869605, 1.000000000000000000, 0.9238795325112869605, 1.000000000000000000, 0.9238795325112869605, 1.000000000000000000, 0.9238795325112869605, 1.000000000000000000, 0.9238795325112869605, 1.000000000000000000, 0.9238795325112869605, 1.000000000000000000, 0.9238795325112869605, 1.000000000000000000, 0.9238795325112869605, 1.000000000000000000, 0.9238795325112869605, 1.000000000000000000, 0.9238795325112869605, 1.000000000000000000, 0.9238795325112869605, 1.000000000000000000, 0.9238795325112869605, 1.000000000000000000, 0.9238795325112869605, 1.000000000000000000, 0.9238795325112869605, 1.000000000000000000, 0.9238795325112869605, 1.000000000000000000, 0.9238795325112869605, 1.000000000000000000, 0.9238795325112869605, 1.000000000000000000, 0.9238795325112869605, 1.000000000000000000, 0.9238795325112869605, 1.000000000000000000, 0.9238795325112869605, 1.000000000000000000, 0.9238795325112869605, 1.000000000000000000, 0.9238795325112869605, 1.000000000000000000, 0.9238795325112869605, 1.000000000000000000, 0.9238795325112869605, 1.000000000000000000, 0.9238795325112869605, 1.000000000000000000, 0.9238795325112869605, 1.000000000000000000, 0.9238795325112869605, 1.000000000000000000, 0.9238795325112869605, 1.000000000000000000, 0.9238795325112869605, 1.000000000000000000, 0.9238795325112869605, 1.000000000000000000, 0.9238795325112869605, 1.000000000000000000, 0.9238795325112869605, 1.000000000000000000, 0.9238795325112869605, 1.000000000000000000, 0.9238795325112869605, 1.000000000000000000, 0.9238795325112869605, 1.000000000000000000, 0.9238795325112869605, 1.000000000000000000, 0.9238795325112869605, 1.000000000000000000, 0.9238795325112869605, 1.000000000000000000, 0.9238795325112869605, 1.000000000000000000, 0.9238795325112869605, 1.000000000000000000, 0.9238795325112869605, 1.000000000000000000, 0.9238795325112869605, 1.000000000000000000, 0.9238795325112869605, 1.000000000000000000, 0.9238795325112869605, 1.000000000000000000, 0.9238795325112869605, 1.000000000000000000, 0.9238795325112869605, 1.000000000000000000, 0.9238795325112869605, 1.000000000000000000, 0.9238795325112869605, 1.000000000000000000, 0.9238795325112869605, 1.000000000000000000, 0.9238795325112869605, 1.000000000000000000, 0.9238795325112869605, 1.000000000000000000, 0.9238795325112869605, 1.000000000000000000, 0.9238795325112869605, 1.000000000000000000, 0.9238795325112869605, 1.000000000000000000, 0.9238795325112869605, 1.000000000000000000, 0.9238795325112869605, 1.000000000000000000, 0.9238795325112869605, 1.000000000000000000, 0.9238795325112869605, 1.000000000000000000, 0.9238795325112869605, 1.000000000000000000, 0.9238795325112869605, 1.000000000000000000, 0.9238795325112869605, 1.000000000000000000, 0.9238795325112869605, 1.000000000000000000, 0.9238795325112869605, 1.000000000000000000, 0.9238795325112869605, 1.000000000000000000, 0.9238795325112869605, 1.000000000000000000, 0.9238795325112869605, 1.000000000000000000, 0.9238795325112869605, 1.000000000000000000, 0.9238795325112869605, 1.000000000000000000, 0.9238795325112869605, 1.000000000000000000, 0.9238795325112869605, 1.000000000000000000, 0.9238795325112869605, 1.000000000000000000, 0.9238795325112869605, 1.000000000000000000, 0.9238795325112869605, 1.000000000000000000, 0.9238795325112869605, 1.000000000000000000, 0.9238795325112869605, 1.000000000000000000, 0.9238795325112869605, 1.000000000000000000, 0.9238795325112869605, 1.000000000000000000, 0.9238795325112869605, 1.000000000000000000, 0.9238795325112869605, 1.000000000000000000, 0.9238795325112869605, 1.000000000000000000, 0.9238795325112869605, 1.000000000000000000, 0.9238795325112869605, 1.000000000000000000, 0.9238795325112869605, 1.000000000000000000, 0.9238795325112869605, 1.000000000000000000, 0.9238795325112869605, 1.000000000000000000, 0.9238795325112869605, 1.000000000000000000, 0.9238795325112869605, 1.000000000000000000, 0.9238795325112869605, 1.000000000000000000, 0.9238795325112869605, 1.000000000000000000, 0.9238795325112869605, 1.000000000000000000, 0.9238795325112869605, 1.000000000000000000, 0.9238795325112869605, 1.000000000000000000, 0.9238795325112869605, 1.000000000000000000, 0.9238795325112869605, 1.000000000000000000, 0.9238795325112869605, 1.000000000000000000, 0.9238795325112869605, 1.000000000000000000, 0.9238795325112869605, 1.000000000000000000, 0.9238795325112869605, 1.000000000000000000, 0.9238795325112869605, 1.000000000000000000, 0.9238795325112869605, 1.000000000000000000, 0.9238795325112869605, 1.000000000000000000, 0.9238795325112869605, 1.000000000000000000, 0.9238795325112869605, 1.000000000000000000, 0.9238795325112869605, 1.000000000000000000, 0.9238795325112869605, 1.000000000000000000, 0.9238795325112869605, 1.000000000000000000, 0.9238795325112869605, 1.000000000000000000, 0.9238795325112869605, 1.000000000000000000, 0.9238795325112869605, 1.000000000000000000, 0.9238795325112869605, 1.000000000000000000, 0.9238795325112869605, 1.000000000000000000, 0.9238795325112869605, 1.000000000000000000, 0.9238795325112869605, 1.000000000000000000, 0.9238795325112869605, 1.000000000000000000, 0.9238795325112869605, 1.000000000000000000, 0.9238795325112869605, 1.000000000000000000, 0.9238795325112869605, 1.000000000000000000, 0.9238795325112869605, 1.000000000000000000, 0.9238795325112869605, 1.000000000000000000, 0.9238795325112869605, 1.000000000000000000, 0.9238795325112869605, 1.000000000000000000, 0.9238795325112869605, 1.000000000000000000, 0.9238795325112869605, 1.000000000000000000, 0.9238795325112869605, 1.000000000000000000, 0.9238795325112869605, 1.000000000000000000, 0.9238795325112869605, 1.000000000000000000, 0.9238795325112869605, 1.000000000000000000, 0.9238795325112869605, 1.000000000000000000, 0.9238795325112869605, 1.000000000000000000, 0.9238795325112869605, 1.000000000000000000, 0.9238795325112869605, 1.000000000000000000, 0.9238795325112869605, 1.000000000000000000, 0.9238795325112869605, 1.000000000000000000, 0.9238795325112869605, 1.000000000000000000, 0.9238795325112869605, 1.000000000000000000, 0.9238795325112869605, 1.000000000000000000, 0.9238795325112869605, 1.000000000000000000, 0.9238795325112869605, 1.000000000000000000, 0.9238795325112869605, 1.000000000000000000, 0.9238795325112869605, 1.000000000000000000, 0.9238795325112869605, 1.000000000000000000, 0.9238795325112869605, 1.000000000000000000, 0.9238795325112869605, 1.000000000000000000, 0.9238795325112869605, 1.000000000000000000, 0.9238795325112869605, 1.000000000000000000, 0.9238795325112869605, 1.000000000000000000, 0.9238795325112869605, 1.000000000000000000, 0.9238795325112869605, 1.000000000000000000, 0.9238795325112869605, 1.000000000000000000, 0.9238795325112869605, 1.000000000000000000, 0.9238795325112869605, 1.000000000000000000, 0.9238795325112869605, 1.000000000000000000, 0.9238795325112869605, 1.000000000000000000, 0.9238795325112869605, 1.000000000000000000, 0.9238795325112869605, 1.000000000000000000, 0.9238795325112869605, 1.000000000000000000, 0.9238795325112869605, 1.000000000000000000, 0.9238795325112869605, 1.000000000000000000, 0.9238795325112869605, 1.000000000000000000, 0.9238795325112869605, 1.000000000000000000, 0.9238795325112869605, 1.000000000000000000, 0.9238795325112869605, 1.000000000000000000, 0.9238795325112869605, 1.000000000000000000, 0.9238795325112869605, 1.000000000000000000, 0.9238795325112869605, 1.000000000000000000, 0.9238795325112869605, 1.000000000000000000, 0.9238795325112869605, 1.000000000000000000, 0.9238795325112869605, 1.000000000000000000, 0.9238795325112869605, 1.000000000000000000, 0.9238795325112869605, 1.000000000000000000, 0.9238795325112869605, 1.000000000000000000, 0.9238795325112869605, 1.000000000000000000, 0.9238795325112869605, 1.000000000000000000, 0.9238795325112869605, 1.000000000000000000, 0.9238795325112869605, 1.000000000000000000, 0.9238795325112869605, 1.000000000000000000, 0.9238795325112869605, 1.000000000000000000, 0.9238795325112869605, 1.000000000000000000, 0.9238795325112869605, 1.000000000000000000, 0.9238795325112869605, 1.000000000000000000, 0.9238795325112869605, 1.000000000000000000, 0.9238795325112869605, 1.000000000000000000, 0.9238795325112869605, 1.000000000000000000, 0.9238795325112869605, 1.000000000000000000, 0.9238795325112869605, 1.000000000000000000, 0.9238795325112869605, 1.000000000000000000, 0.9238795325112869605, 1.000000000000000000, 0.9238795325112869605, 1.000000000000000000, 0.9238795325112869605, 1.000000000000000000, 0.9238795325112869605, 1.000000000000000000, 0.9238795325112869605, 1.000000000000000000, 0.9238795325112869605, 1.000000000000000000, 0.9238795325112869605, 1.000000000000000000, 0.9238795325112869605, 1.000000000000000000, 0.9238795325112869605, 1.000000000000000000, 0.9238795325112869605, 1.000000000000000000, 0.9238795325112869605, 1.000000000000000000, 0.9238795325112869605, 1.000000000000000000, 0.9238795325112869605, 1.000000000000000000, 0.9238795325112869605, 1.000000000000000000, 0.9238795325112869605, 1.000000000000000000, 0.9238795325112869605, 1.000000000000000000, 0.9238795325112869605, 1.000000000000000000, 0.9238795325112869605, 1.000000000000000000, 0.9238795325112869605, 1.000000000000000000, 0.9238795325112869605, 1.000000000000000000, 0.9238795325112869605, 1.000000000000000000, 0.9238795325112869605, 1.000000000000000000, 0.9238795325112869605, 1.000000000000000000, 0.9238795325112869605, 1.000000000000000000, 0.9238795325112869605, 1.000000000000000000, 0.9238795325112869605, 1.000000000000000000, 0.9238795325112869605, 1.000000000000000000, 0.9238795325112869605, 1.000000000000000000, 0.9238795325112869605, 1.000000000000000000, 0.9238795325112869605, 1.000000000000000000, 0.9238795325112869605, 1.000000000000000000, 0.9238795325112869605, 1.000000000000000000, 0.9238795325112869605, 1.000000000000000000, 0.9238795325112869605, 1.000000000000000000, 0.9238795325112869605, 1.000000000000000000, 0.9238795325112869605, 1.000000000000000000, 0.9238795325112869605, 1.000000000000000000, 0.9238795325112869605, 1.000000000000000000, 0.9238795325112869605, 1.000000000000000000, 0.9238795325112869605, 1.000000000000000000, 0.9238795325112869605, 1.000000000000000000, 0.9238795325112869605, 1.000000000000000000, 0.9238795325112869605, 1.000000000000000000, 0.9238795325112869605, 1.000000000000000000, 0.9238795325112869605, 1.000000000000000000, 0.9238795325112869605, 1.000000000000000000, 0.9238795325112869605, 1.000000000000000000, 0.9238795325112869605, 1.000000000000000000, 0.9238795325112869605, 1.000000000000000000, 0.9238795325112869605, 1.000000000000000000, 0.9238795325112869605, 1.000000000000000000, 0.9238795325112869605, 1.000000000000000000, 0.9238795325112869605, 1.000000000000000000, 0.9238795325112869605, 1.000000000000000000, 0.9238795325112869605, 1.000000000000000000, 0.9238795325112869605, 1.000000000000000000, 0.9238795325112869605, 1.000000000000000000, 0.9238795325112869605, 1.000000000000000000, 0.9238795325112869605, 1.000000000000000000, 0.9238795325112869605, 1.000000000000000000, 0.9238795325112869605, 1.000000000000000000, 0.9238795325112869605, 1.000000000000000000, 0.9238795325112869605, 1.000000000000000000, 0.9238795325112869605, 1.000000000000000000, 0.9238795325112869605, 1.000000000000000000, 0.9238795325112869605, 1.000000000000000000, 0.9238795325112869605, 1.000000000000000000, 0.9238795325112869605, 1.000000000000000000, 0.9238795325112869605, 1.000000000000000000, 0.9238795325112869605, 1.000000000000000000, 0.9238795325112869605, 1.000000000000000000, 0.9238795325112869605, 1.000000000000000000, 0.9238795325112869605, 1.000000000000000000, 0.9238795325112869605, 1.000000000000000000, 0.9238795325112869605, 1.000000000000000000, 0.9238795325112869605, 1.000000000000000000, 0.9238795325112869605, 1.000000000000000000, 0.9238795325112869605, 1.000000000000000000, 0.9238795325112869605, 1.000000000000000000, 0.9238795325112869605, 1.000000000000000000, 0.9238795325112869605, 1.000000000000000000, 0.9238795325112869605, 1.000000000000000000, 0.9238795325112869605, 1.000000000000000000, 0.9238795325112869605, 1.000000000000000000, 0.9238795325112869605, 1.000000000000000000, 0.9238795325112869605, 1.000000000000000000, 0.9238795325112869605, 1.000000000000000000, 0.9238795325112869605, 1.000000000000000000, 0.9238795325112869605, 1.000000000000000000, 0.9238795325112869605, 1.000000000000000000, 0.9238795325112869605, 1.000000000000000000, 0.9238795325112869605, 1.000000000000000000, 0.9238795325112869605, 1.000000000000000000, 0.9238795325112869605, 1.000000000000000000, 0.9238795325112869605, 1.000000000000000000, 0.9238795325112869605, 1.000000000000000000, 0.9238795325112869605, 1.000000000000000000, 0.9238795325112869605, 1.000000000000000000, 0.9238795325112869605, 1.000000000000000000, 0.9238795325112869605, 1.000000000000000000, 0.9238795325112869605, 1.000000000000000000) ) ) 
 REPRESENTATION_ITEM ( '' )  SURFACE ( )  ) ;
#23326 = DIRECTION ( 'NONE',  ( 0.000000000000000000, 0.000000000000000000, 1.000000000000000000 ) ) ;
#23327 = CARTESIAN_POINT ( 'NONE',  ( 1.054774247047244540, -0.07405724077823318263, 1.633858267662771313 ) ) ;
#23328 = EDGE_CURVE ( 'NONE', #39762, #21208, #4789, .T. ) ;
#23329 = CARTESIAN_POINT ( 'NONE',  ( -0.1264236179284866091, -1.742618110182456714, -0.1264236179284866091 ) ) ;
#23330 = CARTESIAN_POINT ( 'NONE',  ( -0.07405724077823318263, 0.1446850394238423654, -0.1787899950787401604 ) ) ;
#23331 = ( NAMED_UNIT ( * ) SI_UNIT ( $, .STERADIAN. ) SOLID_ANGLE_UNIT ( ) ) ;
#23332 = DIRECTION ( 'NONE',  ( 0.000000000000000000, 0.000000000000000000, -1.000000000000000000 ) ) ;
#23333 = CARTESIAN_POINT ( 'NONE',  ( -0.9500414927467377701, -0.1787899950787401604, 0.6496062991588353874 ) ) ;
#23334 = EDGE_CURVE ( 'NONE', #370, #17741, #23694, .T. ) ;
#23335 = CARTESIAN_POINT ( 'NONE',  ( -0.8759842519685039353, -0.1574803149606299191, 1.289370078632629868 ) ) ;
#23337 = CARTESIAN_POINT ( 'NONE',  ( -0.8070866141732283561, -0.0009842519685049383633, 0.8559055118110230342 ) ) ;
#23336 = CARTESIAN_POINT ( 'NONE',  ( 0.1574803149606300301, -0.7583661417322827836, 0.06523048226347956391 ) ) ;
#23338 = CARTESIAN_POINT ( 'NONE',  ( 0.1797182628040039365, -1.516776093047611962, -2.200913952912460540E-17 ) ) ;
#23339 = CARTESIAN_POINT ( 'NONE',  ( 0.000000000000000000, 0.1299212598425196763, 0.000000000000000000 ) ) ;
#23340 = CARTESIAN_POINT ( 'NONE',  ( 0.1574803149606300301, -0.4729330707586144600, 0.06523048226347956391 ) ) ;
#23341 = CARTESIAN_POINT ( 'NONE',  ( 0.000000000000000000, 0.000000000000000000, -0.1183602362204724257 ) ) ;
#23342 = CARTESIAN_POINT ( 'NONE',  ( 0.6971942568897648851, -0.07405724077823297447, 1.466535433017102763 ) ) ;
#23343 = CARTESIAN_POINT ( 'NONE',  ( 0.6971942568897648851, -0.07405724077823297447, 1.776574803095843702 ) ) ;
#23344 = AXIS2_PLACEMENT_3D ( 'NONE', #23203, #8333, #5451 ) ;
#23345 = AXIS2_PLACEMENT_3D ( 'NONE', #24251, #2418, #13681 ) ;
#23346 = DIRECTION ( 'NONE',  ( 0.000000000000000000, 1.000000000000000000, 0.000000000000000000 ) ) ;
#23347 = DIRECTION ( 'NONE',  ( -3.494233027178531125E-15, -1.000000000000000000, 0.000000000000000000 ) ) ;
#23348 = DIRECTION ( 'NONE',  ( 0.000000000000000000, -0.6156614753256639538, -0.7880107536067174623 ) ) ;
#23349 = CARTESIAN_POINT ( 'NONE',  ( -0.07405724077823318263, 0.06594488194352733645, -0.1787899950787401604 ) ) ;
#23351 = CARTESIAN_POINT ( 'NONE',  ( 0.6971942568897626646, -0.07405724077823297447, 0.5167322834108034613 ) ) ;
#23350 = ( BOUNDED_CURVE ( )  B_SPLINE_CURVE ( 2, ( #37908, #19682, #8902, #26898, #37666, #34096, #31204, #23534, #1224 ),
 .UNSPECIFIED., .F., .F. ) 
 B_SPLINE_CURVE_WITH_KNOTS ( ( 3, 2, 2, 2, 3 ),
 ( 0.6600000000000000311, 0.6624999999999999778, 0.6650000000000000355, 0.6674999999999999822, 0.6700000000000000400 ),
 .UNSPECIFIED. ) 
 CURVE ( )  GEOMETRIC_REPRESENTATION_ITEM ( )  RATIONAL_B_SPLINE_CURVE ( ( 1.000000000000000000, 0.9238795325112869605, 1.000000000000000000, 0.9238795325112869605, 1.000000000000000000, 0.9238795325112869605, 1.000000000000000000, 0.9238795325112869605, 1.000000000000000000 ) ) 
 REPRESENTATION_ITEM ( '' )  ) ;
#23352 = CARTESIAN_POINT ( 'NONE',  ( -1.033464566929133799, 0.000000000000000000, 0.7578740157480314821 ) ) ;
#23353 = ADVANCED_FACE ( 'NONE', ( #20791 ), #24400, .T. ) ;
#23354 = CARTESIAN_POINT ( 'NONE',  ( 0.7185039370078739607, 1.928577636452523993E-17, 0.8562992125984251190 ) ) ;
#23355 = PRODUCT_RELATED_PRODUCT_CATEGORY ( 'part', '', ( #33371 ) ) ;
#23356 = CARTESIAN_POINT ( 'NONE',  ( 1.033464566929134687, 0.06523048226347956391, 0.7504921258767240921 ) ) ;
#23357 = ORIENTED_EDGE ( 'NONE', *, *, #10741, .T. ) ;
#23358 = CARTESIAN_POINT ( 'NONE',  ( 2.892866454678787531E-17, -0.05708661417322834220, 0.1574803149606299191 ) ) ;
#23359 = ORIENTED_EDGE ( 'NONE', *, *, #12733, .F. ) ;
#23361 = VERTEX_POINT ( 'NONE', #30912 ) ;
#23360 = CARTESIAN_POINT ( 'NONE',  ( 0.1574803149606299191, -1.061023621939716666, -1.928577636452523993E-17 ) ) ;
#23362 = CARTESIAN_POINT ( 'NONE',  ( -0.9873396505805591694, -0.1113553986120547346, 0.6249999998924724576 ) ) ;
#23363 = DIRECTION ( 'NONE',  ( 0.000000000000000000, -1.000000000000000000, 0.000000000000000000 ) ) ;
#23364 = CARTESIAN_POINT ( 'NONE',  ( 1.054774247047244096, 0.000000000000000000, 1.675688976324189117 ) ) ;
#23365 = CARTESIAN_POINT ( 'NONE',  ( -1.033464566929134687, 0.06523048226347956391, 1.193405511811024278 ) ) ;
#23366 = CARTESIAN_POINT ( 'NONE',  ( -0.8107537697050254399, -0.1574803149606297803, 1.050688976270426567 ) ) ;
#23368 = DIRECTION ( 'NONE',  ( 0.000000000000000000, -1.000000000000000000, 0.000000000000000000 ) ) ;
#23367 = CARTESIAN_POINT ( 'NONE',  ( 0.1333875707378843478, 0.2184828823903391670, -0.3149606299212599492 ) ) ;
#23369 = CARTESIAN_POINT ( 'NONE',  ( 0.1476377952755906220, -0.4933358210236691854, -0.8766136318131759753 ) ) ;
#23370 = CARTESIAN_POINT ( 'NONE',  ( 0.7646288533564489232, -0.1113553986120547346, 1.402559055010582645 ) ) ;
#23371 = ORIENTED_EDGE ( 'NONE', *, *, #43215, .F. ) ;
#23372 = ORIENTED_EDGE ( 'NONE', *, *, #7844, .F. ) ;
#23373 = CARTESIAN_POINT ( 'NONE',  ( -0.09216094027006721534, -0.09383642490574109485, -0.2322237458740071259 ) ) ;
#23374 = ORIENTED_EDGE ( 'NONE', *, *, #40028, .T. ) ;
#23375 = CARTESIAN_POINT ( 'NONE',  ( 1.054774247047244096, 0.000000000000000000, 0.9325787401037164415 ) ) ;
#23376 = CARTESIAN_POINT ( 'NONE',  ( -0.9500414927467377701, -0.1787899950787401604, 1.510826771599780294 ) ) ;
#23377 = CARTESIAN_POINT ( 'NONE',  ( -0.1574803149606297803, 0.02411417333587350179, 0.06523048226347956391 ) ) ;
#23378 = CARTESIAN_POINT ( 'NONE',  ( -0.6971942568897637749, 2.189545951927499583E-17, 1.227854330654897685 ) ) ;
#23379 = VERTEX_POINT ( 'NONE', #13390 ) ;
#23380 = VERTEX_POINT ( 'NONE', #5475 ) ;
#23381 = DIRECTION ( 'NONE',  ( -7.047314121155773299E-15, 0.000000000000000000, 1.000000000000000000 ) ) ;
#23382 = CARTESIAN_POINT ( 'NONE',  ( -0.8759842519685039353, -0.1787899950787401882, 0.2928149605761578567 ) ) ;
#23383 = DIRECTION ( 'NONE',  ( 1.000000000000000000, 4.379520288671465147E-30, 0.000000000000000000 ) ) ;
#23384 = CARTESIAN_POINT ( 'NONE',  ( 0.1574803149606299191, 0.3883517482604913473, -0.6419475548153091848 ) ) ;
#23385 = CARTESIAN_POINT ( 'NONE',  ( -0.07405724077823318263, -0.9686279052371123965, -0.1787899950787401604 ) ) ;
#23386 = ORIENTED_EDGE ( 'NONE', *, *, #41505, .F. ) ;
#23387 = CARTESIAN_POINT ( 'NONE',  ( -0.1787899950787401604, 0.03641732288840918152, -0.07405724077823318263 ) ) ;
#23388 = AXIS2_PLACEMENT_3D ( 'NONE', #14822, #4720, #33523 ) ;
#23389 = ORIENTED_EDGE ( 'NONE', *, *, #36822, .F. ) ;
#23390 = EDGE_CURVE ( 'NONE', #37016, #47083, #31609, .T. ) ;
#23391 = LINE ( 'NONE', #26519, #13891 ) ;
#23392 = ADVANCED_FACE ( 'NONE', ( #16512 ), #27560, .T. ) ;
#23393 = CARTESIAN_POINT ( 'NONE',  ( 0.1787899950787401604, -0.5738188975840317063, -0.07405724077823318263 ) ) ;
#23394 = CARTESIAN_POINT ( 'NONE',  ( -0.9500414927467377701, 0.1787899950787401604, 0.2706692912848194243 ) ) ;
#23395 = CARTESIAN_POINT ( 'NONE',  ( -0.9412147342319837628, 0.1574803149606300301, 1.001476377952755348 ) ) ;
#23396 = FACE_OUTER_BOUND ( 'NONE', #18589, .T. ) ;
#23397 = CARTESIAN_POINT ( 'NONE',  ( -0.07444174185955065859, -1.135378455252336050, 0.1797182628040039087 ) ) ;
#23398 = CARTESIAN_POINT ( 'NONE',  ( 0.7185039370078746268, 0.06523048226347956391, 0.4207677165354331561 ) ) ;
#23399 = CARTESIAN_POINT ( 'NONE',  ( 0.8759842519685039353, 0.1787899950787401882, 0.9424212597887559051 ) ) ;
#23400 = CARTESIAN_POINT ( 'NONE',  ( 0.8759842519685039353, -0.1787899950787401882, 0.1304133857730082613 ) ) ;
#23401 = AXIS2_PLACEMENT_3D ( 'NONE', #36144, #18160, #25605 ) ;
#23402 = DIRECTION ( 'NONE',  ( 1.000000000000000000, 0.000000000000000000, -7.044195017643630340E-15 ) ) ;
#23403 = CARTESIAN_POINT ( 'NONE',  ( 0.8107537697050253289, -0.1574803149606297803, 1.611712598425196319 ) ) ;
#23405 = DIRECTION ( 'NONE',  ( 1.000000000000000000, 0.000000000000000000, 0.000000000000000000 ) ) ;
#23404 = CARTESIAN_POINT ( 'NONE',  ( 0.7127101691150015128, -0.03581842120577477528, 1.983932702903218770 ) ) ;
#23406 = DIRECTION ( 'NONE',  ( -0.000000000000000000, -0.7880107536067176843, 0.6156614753256636208 ) ) ;
#23407 = CARTESIAN_POINT ( 'NONE',  ( 0.07405724077823318263, 0.05118110241596821042, 0.1787899950787401604 ) ) ;
#23408 = CARTESIAN_POINT ( 'NONE',  ( 0.7185039370078739607, 1.928577636452523993E-17, 0.7775590551181102983 ) ) ;
#23409 = CARTESIAN_POINT ( 'NONE',  ( 1.002407869896990045, 0.1264236179284866091, 0.9325787401037164415 ) ) ;
#23410 = CARTESIAN_POINT ( 'NONE',  ( 0.7495606340400177148, 0.1264236179284866091, 1.892224409395055096 ) ) ;
#23411 = CARTESIAN_POINT ( 'NONE',  ( 0.9873396505805591694, 0.1113553986120547346, 0.3198818896562523606 ) ) ;
#23412 = ORIENTED_EDGE ( 'NONE', *, *, #19965, .F. ) ;
#23413 = DIRECTION ( 'NONE',  ( -8.673617379884034486E-16, 0.000000000000000000, -1.000000000000000000 ) ) ;
#23414 = AXIS2_PLACEMENT_3D ( 'NONE', #38166, #26467, #31003 ) ;
#23415 = VECTOR ( 'NONE', #25578, 39.37007874015748143 ) ;
#23416 = CARTESIAN_POINT ( 'NONE',  ( -0.5314960629921260393, 0.000000000000000000, 4.685039370078739829 ) ) ;
#23417 = CARTESIAN_POINT ( 'NONE',  ( -0.1574803149606297803, -1.747539369971212730, 0.06523048226347956391 ) ) ;
#23418 = CARTESIAN_POINT ( 'NONE',  ( -0.9412147342319837628, 0.1574803149606300301, 0.2042322833570398011 ) ) ;
#23419 = CARTESIAN_POINT ( 'NONE',  ( 0.7495606340400177148, -0.1264236179284866091, 1.149114173174582643 ) ) ;
#23420 = EDGE_LOOP ( 'NONE', ( #36238, #3363, #37693, #25665 ) ) ;
#23421 = CARTESIAN_POINT ( 'NONE',  ( -0.1476377952755905387, 1.117014023967196179, -3.442880580079819008 ) ) ;
#23422 = CARTESIAN_POINT ( 'NONE',  ( 0.1787899950787401604, 0.1348425197388028463, 0.07405724077823318263 ) ) ;
#23423 = CARTESIAN_POINT ( 'NONE',  ( -0.7185039370078739607, 1.928577636452523993E-17, 1.043307086506645831 ) ) ;
#23424 = DIRECTION ( 'NONE',  ( -1.000000000000000000, 0.000000000000000000, 0.000000000000000000 ) ) ;
#23425 = CARTESIAN_POINT ( 'NONE',  ( -1.002407869896990045, -0.1264236179284866091, 0.2140748030958428971 ) ) ;
#23426 = ORIENTED_EDGE ( 'NONE', *, *, #8498, .F. ) ;
#23427 = CARTESIAN_POINT ( 'NONE',  ( -0.07405724077823318263, -1.612204724355685403, 0.1787899950787401604 ) ) ;
#23428 = CARTESIAN_POINT ( 'NONE',  ( -0.6971942568897648851, -0.07405724077823297447, 1.815944881835999558 ) ) ;
#23429 = CARTESIAN_POINT ( 'NONE',  ( -0.8019270111902717657, 0.1787899950787401604, 0.5118110235682844511 ) ) ;
#23430 = CARTESIAN_POINT ( 'NONE',  ( -0.2185580477446626979, 0.1693028889594568043, -0.3031249188861500632 ) ) ;
#23431 = DIRECTION ( 'NONE',  ( -1.000000000000000000, -0.000000000000000000, 0.000000000000000000 ) ) ;
#23432 = CARTESIAN_POINT ( 'NONE',  ( -0.1787899950787401882, -0.4888050705914433469, 0.000000000000000000 ) ) ;
#23433 = CARTESIAN_POINT ( 'NONE',  ( 0.1747654535727043434, -0.08956020295265729181, 0.1168153130661813005 ) ) ;
#23434 = CARTESIAN_POINT ( 'NONE',  ( -1.033464566929133799, 0.000000000000000000, 1.889763779420031486 ) ) ;
#23435 = DIRECTION ( 'NONE',  ( 0.000000000000000000, 0.6156614753256604011, 0.7880107536067203489 ) ) ;
#23436 = DIRECTION ( 'NONE',  ( -1.000000000000000000, 0.000000000000000000, 0.000000000000000000 ) ) ;
#23437 = AXIS2_PLACEMENT_3D ( 'NONE', #7700, #44343, #8167 ) ;
#23438 = EDGE_CURVE ( 'NONE', #13132, #35281, #31142, .T. ) ;
#23439 = CARTESIAN_POINT ( 'NONE',  ( -1.054774247047244540, 0.07405724077823318263, 0.4970472440407249226 ) ) ;
#23440 = CARTESIAN_POINT ( 'NONE',  ( -0.1264236179284866091, -1.783096409174122154, 0.1264236179284866091 ) ) ;
#23441 = EDGE_CURVE ( 'NONE', #33816, #47229, #39119, .T. ) ;
#23442 = ORIENTED_EDGE ( 'NONE', *, *, #44195, .F. ) ;
#23443 = CARTESIAN_POINT ( 'NONE',  ( 0.2471920549079764384, -0.08080427097405437631, 0.07167403547456246971 ) ) ;
#23444 = ADVANCED_FACE ( 'NONE', ( #46426 ), #23469, .F. ) ;
#23445 = CARTESIAN_POINT ( 'NONE',  ( -1.002407869896990045, 0.1264236179284866091, 1.567421259788755794 ) ) ;
#23446 = VECTOR ( 'NONE', #21781, 39.37007874015748143 ) ;
#23447 = ADVANCED_FACE ( 'NONE', ( #17206 ), #11724, .T. ) ;
#23448 = CARTESIAN_POINT ( 'NONE',  ( -0.1787899950787401604, -1.464566929080096225, -0.07405724077823318263 ) ) ;
#23449 = CARTESIAN_POINT ( 'NONE',  ( -0.2559055118110236116, 0.1477471161312047254, -0.2921040715117803055 ) ) ;
#23450 = DIRECTION ( 'NONE',  ( 0.000000000000000000, -1.000000000000000000, 0.000000000000000000 ) ) ;
#23451 = CARTESIAN_POINT ( 'NONE',  ( 0.1377952755905511861, 0.1564960629921262614, -0.8070866141732283561 ) ) ;
#23452 = ORIENTED_EDGE ( 'NONE', *, *, #17173, .F. ) ;
#23453 = CARTESIAN_POINT ( 'NONE',  ( 0.7185039370078746268, -0.06523048226347956391, 0.5044291338582675976 ) ) ;
#23454 = CARTESIAN_POINT ( 'NONE',  ( 0.000000000000000000, 0.000000000000000000, -0.3149606299212598381 ) ) ;
#23455 = CARTESIAN_POINT ( 'NONE',  ( -0.9873396505805591694, 0.1113553986120547346, 1.225393700679874076 ) ) ;
#23456 = CARTESIAN_POINT ( 'NONE',  ( 1.054774247047244540, 0.07405724077823318263, 0.5019685038832442103 ) ) ;
#23457 = CARTESIAN_POINT ( 'NONE',  ( 1.054774247047244096, 0.000000000000000000, 0.1008858267178899676 ) ) ;
#23459 = CARTESIAN_POINT ( 'NONE',  ( 0.7185039370078739607, 1.928577636452523993E-17, 0.3444881889763780070 ) ) ;
#23458 = CARTESIAN_POINT ( 'NONE',  ( -0.06523048226347956391, -0.3892716535433071168, -0.1574803149606300301 ) ) ;
#23460 = FACE_OUTER_BOUND ( 'NONE', #42415, .T. ) ;
#23461 = EDGE_LOOP ( 'NONE', ( #14185, #30068, #46458, #9397 ) ) ;
#23462 = CARTESIAN_POINT ( 'NONE',  ( 0.8759842519685039353, 0.1574803149606299191, 1.584645669183810890 ) ) ;
#23463 = CARTESIAN_POINT ( 'NONE',  ( -1.054774247047244096, 0.000000000000000000, 1.090059055064346527 ) ) ;
#23464 = CARTESIAN_POINT ( 'NONE',  ( 0.8759842519685039353, -0.1574803149606299191, 1.102362204724409489 ) ) ;
#23465 = FACE_OUTER_BOUND ( 'NONE', #37187, .T. ) ;
#23466 = CARTESIAN_POINT ( 'NONE',  ( -0.6195511811023656223, 0.6102362204724407491, 0.9891732283464566011 ) ) ;
#23467 = CARTESIAN_POINT ( 'NONE',  ( 0.06523048226347956391, -0.5418307085538903722, -0.1574803149606300301 ) ) ;
#23469 = PLANE ( 'NONE',  #20124 ) ;
#23468 = CYLINDRICAL_SURFACE ( 'NONE', #10032, 0.1968503937007874405 ) ;
#23470 = CARTESIAN_POINT ( 'NONE',  ( -0.9412147342319837628, -0.1574803149606297803, 1.262303149606299746 ) ) ;
#23471 = CARTESIAN_POINT ( 'NONE',  ( -0.1656966359942823597, -0.08956191954329044413, 0.02636594708157497663 ) ) ;
#23472 = CARTESIAN_POINT ( 'NONE',  ( -0.1787899950787401604, -0.5885826771115909573, 0.07405724077823318263 ) ) ;
#23473 = ORIENTED_EDGE ( 'NONE', *, *, #27350, .F. ) ;
#23474 = CARTESIAN_POINT ( 'NONE',  ( 3.414809992080330995E-16, 0.2954942322624074524, 0.000000000000000000 ) ) ;
#23475 = CARTESIAN_POINT ( 'NONE',  ( -0.3100393700787401619, 0.000000000000000000, 0.7086614173228351632 ) ) ;
#23476 = CARTESIAN_POINT ( 'NONE',  ( 0.8759842519685039353, -0.1787899950787401882, 0.6815944881352126172 ) ) ;
#23477 = CARTESIAN_POINT ( 'NONE',  ( -0.8107537697050253289, 0.1574803149606300301, 1.124507874015748810 ) ) ;
#23478 = ORIENTED_EDGE ( 'NONE', *, *, #32167, .F. ) ;
#23479 = CARTESIAN_POINT ( 'NONE',  ( -0.09432024557781878982, 0.09445537554013626325, -0.2309772516917564245 ) ) ;
#23480 = CARTESIAN_POINT ( 'NONE',  ( 0.8107537697050254399, -0.1574803149606297803, 0.9030511811023625990 ) ) ;
#23481 = CARTESIAN_POINT ( 'NONE',  ( -0.1787899950787401882, -1.693405511757259951, 0.000000000000000000 ) ) ;
#23482 = CARTESIAN_POINT ( 'NONE',  ( 0.1787899950787401604, -0.9281496062454495100, -0.07405724077823318263 ) ) ;
#23483 = CARTESIAN_POINT ( 'NONE',  ( 2.892866454678787531E-17, -1.356299212598425230, 0.1574803149606299191 ) ) ;
#23484 = CARTESIAN_POINT ( 'NONE',  ( 0.7646288533564489232, -0.1113553986120547346, 1.166338582569637961 ) ) ;
#23485 = CARTESIAN_POINT ( 'NONE',  ( 0.1558458267876858538, 0.09164332750980257181, -0.1168596517594497897 ) ) ;
#23486 = ORIENTED_EDGE ( 'NONE', *, *, #30541, .T. ) ;
#23487 = ORIENTED_EDGE ( 'NONE', *, *, #729, .T. ) ;
#23488 = CARTESIAN_POINT ( 'NONE',  ( -1.054774247047244096, 0.000000000000000000, 1.798720472387181024 ) ) ;
#23489 = CARTESIAN_POINT ( 'NONE',  ( 1.054774247047244096, 0.000000000000000000, 1.798720472387181024 ) ) ;
#23490 = EDGE_LOOP ( 'NONE', ( #6473, #11497, #25083, #31730 ) ) ;
#23491 = CARTESIAN_POINT ( 'NONE',  ( 1.033464566929134687, -0.06523048226347956391, 1.779035433070867311 ) ) ;
#23492 = CARTESIAN_POINT ( 'NONE',  ( 1.054774247047244540, -0.07405724077823318263, 0.4183070865604097133 ) ) ;
#23493 = CARTESIAN_POINT ( 'NONE',  ( -0.8019270111902717657, 0.1787899950787401604, 1.333661417269071059 ) ) ;
#23494 = DIRECTION ( 'NONE',  ( 0.000000000000000000, 1.000000000000000000, 0.000000000000000000 ) ) ;
#23495 = CARTESIAN_POINT ( 'NONE',  ( -0.6971942568897626646, 0.07405724077823318263, 0.1230314960092287191 ) ) ;
#23496 = CARTESIAN_POINT ( 'NONE',  ( -1.033464566929133799, 1.928577636452524610E-17, 2.869337061179095023E-17 ) ) ;
#23497 = CARTESIAN_POINT ( 'NONE',  ( -1.054774247047244540, -0.07405724077823318263, 1.717519684985606476 ) ) ;
#23498 = CARTESIAN_POINT ( 'NONE',  ( -0.9500414927467378812, 0.1787899950787401604, 0.03444881884387430981 ) ) ;
#23499 = CARTESIAN_POINT ( 'NONE',  ( -0.7185039370078746268, 0.06523048226347956391, 1.680610236220472231 ) ) ;
#23500 = B_SPLINE_CURVE_WITH_KNOTS ( 'NONE', 3,
 ( #28611, #2689, #39341, #3163, #25219, #27903, #6283, #2221, #39810, #28849, #16841, #38881 ),
 .UNSPECIFIED., .F., .F.,
 ( 4, 1, 1, 1, 1, 2, 2, 4 ),
 ( 0.000000000000000000, 0.2500000000000017208, 0.3750000000000024425, 0.4375000000000028311, 0.4687500000000029976, 0.4843750000000031641, 0.5000000000000033307, 1.000000000000000000 ),
 .UNSPECIFIED. ) ;
#23501 = LINE ( 'NONE', #30471, #12135 ) ;
#23502 = CARTESIAN_POINT ( 'NONE',  ( 0.7495606340400177148, -0.1264236179284866091, 1.665846456639149764 ) ) ;
#23503 = CARTESIAN_POINT ( 'NONE',  ( 0.2009854772848184978, -0.09842519685039370636, -0.04150255699268778908 ) ) ;
#23504 = CARTESIAN_POINT ( 'NONE',  ( 1.033464566929133799, 1.928577636452524610E-17, 4.498031496062992574 ) ) ;
#23505 = CARTESIAN_POINT ( 'NONE',  ( 0.8759842519685039353, 0.1574803149606299191, 0.2854330707586145710 ) ) ;
#23506 = VECTOR ( 'NONE', #47181, 39.37007874015748143 ) ;
#23507 = ADVANCED_FACE ( 'NONE', ( #5225 ), #37700, .F. ) ;
#23508 = ORIENTED_EDGE ( 'NONE', *, *, #43324, .T. ) ;
#23509 = ( BOUNDED_CURVE ( )  B_SPLINE_CURVE ( 2, ( #26007, #571, #44417, #15228, #26254, #36787, #40817, #101, #29650 ),
 .UNSPECIFIED., .F., .T. ) 
 B_SPLINE_CURVE_WITH_KNOTS ( ( 3, 2, 2, 2, 3 ),
 ( 0.1300000000000000044, 0.1325000000000000067, 0.1350000000000000089, 0.1375000000000000111, 0.1400000000000000133 ),
 .UNSPECIFIED. ) 
 CURVE ( )  GEOMETRIC_REPRESENTATION_ITEM ( )  RATIONAL_B_SPLINE_CURVE ( ( 1.000000000000000000, 0.9238795325112869605, 1.000000000000000000, 0.9238795325112869605, 1.000000000000000000, 0.9238795325112869605, 1.000000000000000000, 0.9238795325112869605, 1.000000000000000000 ) ) 
 REPRESENTATION_ITEM ( '' )  ) ;
#23510 = ORIENTED_EDGE ( 'NONE', *, *, #13087, .T. ) ;
#23511 = EDGE_CURVE ( 'NONE', #47093, #27914, #24439, .T. ) ;
#23512 = CARTESIAN_POINT ( 'NONE',  ( 3.284318927891251994E-17, -0.9798228345919054449, 0.1787899950787401882 ) ) ;
#23513 = CARTESIAN_POINT ( 'NONE',  ( -0.07405724077823318263, -1.031496062938363822, -0.1787899950787401604 ) ) ;
#23514 = DIRECTION ( 'NONE',  ( 0.000000000000000000, 0.000000000000000000, 1.000000000000000000 ) ) ;
#23515 = CARTESIAN_POINT ( 'NONE',  ( 1.002407869896990045, -0.1264236179284866091, 1.828248031442299082 ) ) ;
#23516 = CARTESIAN_POINT ( 'NONE',  ( 0.7495606340400177148, -0.1264236179284866091, 0.4010826771115905687 ) ) ;
#23517 = CARTESIAN_POINT ( 'NONE',  ( 0.1797182628040039087, -0.4168745182444627551, 0.07444174185955046430 ) ) ;
#23518 = CARTESIAN_POINT ( 'NONE',  ( -0.7646288533564489232, 0.1113553986120547346, 0.8021653542231811373 ) ) ;
#23519 = CARTESIAN_POINT ( 'NONE',  ( -9.642888182262618425E-18, -0.03740157480314960925, -0.1574803149606299191 ) ) ;
#23520 = CARTESIAN_POINT ( 'NONE',  ( 1.054774247047244540, -0.07405724077823318263, 0.8858267715997791836 ) ) ;
#23521 = CARTESIAN_POINT ( 'NONE',  ( 0.003583035186813061154, 0.09844385435687157127, 0.1050988454125816457 ) ) ;
#23522 = CARTESIAN_POINT ( 'NONE',  ( -0.07874015748031495954, -0.5708661417322835607, 0.9783464566929284123 ) ) ;
#23523 = CARTESIAN_POINT ( 'NONE',  ( 1.054774247047244540, -0.07405724077823318263, 1.953740157426552715 ) ) ;
#23524 = CARTESIAN_POINT ( 'NONE',  ( 0.7646288533564489232, 0.1113553986120547346, 0.2214566929133858220 ) ) ;
#23525 = FACE_OUTER_BOUND ( 'NONE', #45422, .T. ) ;
#23526 = CARTESIAN_POINT ( 'NONE',  ( -0.1264236179284866091, -0.4827755904974173617, -0.1264236179284866091 ) ) ;
#23527 = CARTESIAN_POINT ( 'NONE',  ( 0.9873396505805591694, -0.1113553986120547346, 0.1230314960629921295 ) ) ;
#23528 = ADVANCED_FACE ( 'NONE', ( #34966 ), #5575, .T. ) ;
#23530 = CIRCLE ( 'NONE', #13586, 0.009842519685039378616 ) ;
#23529 = CARTESIAN_POINT ( 'NONE',  ( 0.1787899950787401882, -1.280019684985606254, -2.189545951927503898E-17 ) ) ;
#23531 = CARTESIAN_POINT ( 'NONE',  ( -0.8759842519685039353, 0.1787899950787401882, 1.764271653489543290 ) ) ;
#23532 = ORIENTED_EDGE ( 'NONE', *, *, #25281, .T. ) ;
#23533 = CARTESIAN_POINT ( 'NONE',  ( -0.6971942568897637749, 2.189545951927499583E-17, 1.306594488135212728 ) ) ;
#23534 = CARTESIAN_POINT ( 'NONE',  ( -0.7185039370078746268, 0.06523048226347956391, 1.326279527559055982 ) ) ;
#23535 = CARTESIAN_POINT ( 'NONE',  ( 0.9500414927467378812, 0.1787899950787401604, 1.451771653489543290 ) ) ;
#23536 = CARTESIAN_POINT ( 'NONE',  ( -0.8759842519685039353, 0.1787899950787401882, 1.173720472387181246 ) ) ;
#23537 = CARTESIAN_POINT ( 'NONE',  ( 0.8107537697050254399, 0.1574803149606300301, 1.547736220364914983 ) ) ;
#23538 = CARTESIAN_POINT ( 'NONE',  ( 0.06305891922640385894, -0.09842519065806150380, -0.1673058913905094147 ) ) ;
#23539 = CARTESIAN_POINT ( 'NONE',  ( -1.033464566929133799, 1.928577636452524610E-17, 2.869337061179095023E-17 ) ) ;
#23540 = CARTESIAN_POINT ( 'NONE',  ( 0.8019270111902716547, -0.1787899950787401604, 0.6053149605761580787 ) ) ;
#23541 = CARTESIAN_POINT ( 'NONE',  ( -1.054774247047244540, -0.07405724077823318263, 0.4527559054580477249 ) ) ;
#23542 = SURFACE_SIDE_STYLE ('',( #22654 ) ) ;
#23543 = CARTESIAN_POINT ( 'NONE',  ( 0.06523048226347956391, -0.09399606299212612259, 0.1574803149606297803 ) ) ;
#23544 = ORIENTED_EDGE ( 'NONE', *, *, #38476, .T. ) ;
#23545 = CARTESIAN_POINT ( 'NONE',  ( -1.033464566929133799, 0.000000000000000000, 0.2460629921259842590 ) ) ;
#23546 = CARTESIAN_POINT ( 'NONE',  ( -0.1602258124790746086, -0.09851385344451535353, -0.1931672967797941065 ) ) ;
#23547 = CARTESIAN_POINT ( 'NONE',  ( -0.2559055118110235560, -0.08435794557227528634, -0.05641901976107029787 ) ) ;
#23548 = VERTEX_POINT ( 'NONE', #33441 ) ;
#23549 = EDGE_CURVE ( 'NONE', #33555, #44909, #11149, .T. ) ;
#23550 = CARTESIAN_POINT ( 'NONE',  ( -0.7185039370078692977, 0.06523048226347515077, 1.473917322727118506 ) ) ;
#23551 = EDGE_LOOP ( 'NONE', ( #2537, #21712, #31556, #42722, #32974 ) ) ;
#23552 = CARTESIAN_POINT ( 'NONE',  ( 0.8759842519685039353, 0.000000000000000000, 4.498031496062992574 ) ) ;
#23553 = CARTESIAN_POINT ( 'NONE',  ( 0.1787899950787401604, -0.3720472440407247561, -0.07405724077823318263 ) ) ;
#23554 = CARTESIAN_POINT ( 'NONE',  ( -0.2713482210566312558, -0.1500601874062442720, 0.8011725184260182209 ) ) ;
#23555 = CARTESIAN_POINT ( 'NONE',  ( 0.6971942568897637749, 2.189545951927499583E-17, 1.341043307032850462 ) ) ;
#23556 = ADVANCED_FACE ( 'NONE', ( #25770 ), #21925, .F. ) ;
#23557 = DIRECTION ( 'NONE',  ( 0.000000000000000000, -0.7880107536067207930, 0.6156614753256598460 ) ) ;
#23558 = CIRCLE ( 'NONE', #2861, 0.09842519685039370636 ) ;
#23559 = CARTESIAN_POINT ( 'NONE',  ( -0.07405724077823318263, -0.2490157479777327099, -0.1787899950787401604 ) ) ;
#23560 = CARTESIAN_POINT ( 'NONE',  ( 0.4399002236966070845, 1.411419074098315019, -0.2911036367043311479 ) ) ;
#23561 = CARTESIAN_POINT ( 'NONE',  ( 0.9500414927467378812, -0.1787899950787401604, 1.550196850339937926 ) ) ;
#23562 = CARTESIAN_POINT ( 'NONE',  ( -1.094772975963752103E-17, -1.708169291284818980, -0.1787899950787401882 ) ) ;
#23563 = CARTESIAN_POINT ( 'NONE',  ( 0.1243106777423573922, -0.09842519685039372024, 0.1163740807232158392 ) ) ;
#23564 = CARTESIAN_POINT ( 'NONE',  ( -1.054774247047244096, 0.000000000000000000, 0.6963582676627716461 ) ) ;
#23566 = DIRECTION ( 'NONE',  ( -1.000000000000000000, 0.000000000000000000, 6.938893903907228378E-15 ) ) ;
#23565 = CARTESIAN_POINT ( 'NONE',  ( 2.892866454678787531E-17, -0.7263779527559055538, 0.1574803149606299191 ) ) ;
#23567 = CARTESIAN_POINT ( 'NONE',  ( 3.301370929368692659E-17, -1.605358770212966357, 0.1797182628040039365 ) ) ;
#23568 = DIRECTION ( 'NONE',  ( 0.000000000000000000, 1.000000000000000000, 0.000000000000000000 ) ) ;
#23569 = CARTESIAN_POINT ( 'NONE',  ( 3.284318927891251994E-17, -0.3843503936470239468, 0.1787899950787401882 ) ) ;
#23570 = CARTESIAN_POINT ( 'NONE',  ( 0.2471922904502826535, 0.07794254751779122747, -0.07737183577689113467 ) ) ;
#23571 = CARTESIAN_POINT ( 'NONE',  ( 0.8019270111902717657, -0.1787899950787401604, 1.589566929080094448 ) ) ;
#23572 = CARTESIAN_POINT ( 'NONE',  ( 0.9500414927467377701, -0.1787899950787401604, 1.825787401521040243 ) ) ;
#23573 = ORIENTED_EDGE ( 'NONE', *, *, #40182, .F. ) ;
#23574 = CARTESIAN_POINT ( 'NONE',  ( -0.5555748031496045014, 0.6449983665207589256, -0.06082000038405668829 ) ) ;
#23575 = LINE ( 'NONE', #24058, #40382 ) ;
#23576 = FACE_OUTER_BOUND ( 'NONE', #17740, .T. ) ;
#23577 = CARTESIAN_POINT ( 'NONE',  ( 0.1787899950787401604, 0.05118110241596821736, 0.07405724077823318263 ) ) ;
#23578 = CARTESIAN_POINT ( 'NONE',  ( 0.8019270111902717657, -0.1787899950787401604, 0.5216535432533228045 ) ) ;
#23579 = CARTESIAN_POINT ( 'NONE',  ( 0.7646288533564489232, -0.1113553986120547346, 0.07381889763779526936 ) ) ;
#23580 = DIRECTION ( 'NONE',  ( 0.000000000000000000, 1.000000000000000000, 0.000000000000000000 ) ) ;
#23581 = CARTESIAN_POINT ( 'NONE',  ( 1.033464566929133799, 0.000000000000000000, 0.8366141732283465249 ) ) ;
#23582 = CARTESIAN_POINT ( 'NONE',  ( -1.002407869896990045, 0.1264236179284866091, 1.365649606245448844 ) ) ;
#23583 = CARTESIAN_POINT ( 'NONE',  ( 1.033464566929134687, -0.06523048226347956391, 0.7455708660342049710 ) ) ;
#23584 = ORIENTED_EDGE ( 'NONE', *, *, #15216, .F. ) ;
#23585 = CARTESIAN_POINT ( 'NONE',  ( 1.054774247047244540, -0.07405724077823318263, 0.9694881889226144578 ) ) ;
#23586 = EDGE_LOOP ( 'NONE', ( #7098, #38392, #42845 ) ) ;
#23587 = CARTESIAN_POINT ( 'NONE',  ( -0.8107537697050253289, 0.1574803149606300301, 0.6028543306011346914 ) ) ;
#23588 = DIRECTION ( 'NONE',  ( -0.000000000000000000, 0.2126700594527834443, -0.9771240687918547607 ) ) ;
#23589 = CARTESIAN_POINT ( 'NONE',  ( 0.6971942568897648851, 0.07405724077823318263, 1.732283464513166615 ) ) ;
#23590 = CARTESIAN_POINT ( 'NONE',  ( -0.8107537697050253289, -0.1574803149606297803, 1.257381889763780736 ) ) ;
#23591 = CARTESIAN_POINT ( 'NONE',  ( 0.7185039370078746268, 0.06523048226347956391, 0.2534448817822371192 ) ) ;
#23592 = CARTESIAN_POINT ( 'NONE',  ( 0.7185039370078746268, 0.06523048226347956391, 1.956200787401576102 ) ) ;
#23593 = CARTESIAN_POINT ( 'NONE',  ( 0.8759842491179902213, 0.1574803149606299191, 1.978346456692913646 ) ) ;
#23594 = CARTESIAN_POINT ( 'NONE',  ( 0.7185039370078746268, 0.06523048226347956391, 1.473917322727117840 ) ) ;
#23595 = ORIENTED_EDGE ( 'NONE', *, *, #2499, .F. ) ;
#23596 = ORIENTED_EDGE ( 'NONE', *, *, #9928, .F. ) ;
#23597 = AXIS2_PLACEMENT_3D ( 'NONE', #8972, #37737, #34624 ) ;
#23598 = CARTESIAN_POINT ( 'NONE',  ( 0.2871444924769520068, 1.495705267341507883, -0.3569552279982047271 ) ) ;
#23599 = EDGE_CURVE ( 'NONE', #4842, #19535, #38490, .T. ) ;
#23600 = CARTESIAN_POINT ( 'NONE',  ( 0.7495606340400177148, -0.1264236179284866091, 0.9571850393163149340 ) ) ;
#23601 = CARTESIAN_POINT ( 'NONE',  ( -0.8759842519685039353, 0.1787899950787401882, 1.606791338528913426 ) ) ;
#23602 = CARTESIAN_POINT ( 'NONE',  ( 0.1574803149606300301, -0.07431102351452013866, -0.06523048226347956391 ) ) ;
#23603 = CARTESIAN_POINT ( 'NONE',  ( -0.9500414927467378812, 0.1787899950787401604, 1.412401574749386990 ) ) ;
#23604 = ( BOUNDED_CURVE ( )  B_SPLINE_CURVE ( 2, ( #41098, #8292, #19559, #10200, #9497, #5891, #2283, #34668, #42745 ),
 .UNSPECIFIED., .F., .T. ) 
 B_SPLINE_CURVE_WITH_KNOTS ( ( 3, 2, 2, 2, 3 ),
 ( 0.7800000000000000266, 0.7824999999999999734, 0.7850000000000000311, 0.7874999999999999778, 0.7900000000000000355 ),
 .UNSPECIFIED. ) 
 CURVE ( )  GEOMETRIC_REPRESENTATION_ITEM ( )  RATIONAL_B_SPLINE_CURVE ( ( 1.000000000000000000, 0.9238795325112869605, 1.000000000000000000, 0.9238795325112869605, 1.000000000000000000, 0.9238795325112869605, 1.000000000000000000, 0.9238795325112869605, 1.000000000000000000 ) ) 
 REPRESENTATION_ITEM ( '' )  ) ;
#23605 = EDGE_CURVE ( 'NONE', #26131, #31988, #40637, .T. ) ;
#23606 = DIRECTION ( 'NONE',  ( 0.000000000000000000, 0.000000000000000000, 1.000000000000000000 ) ) ;
#23607 = CYLINDRICAL_SURFACE ( 'NONE', #12689, 0.1574803149606299191 ) ;
#23608 = DIRECTION ( 'NONE',  ( 1.000000000000000000, -5.472378587457090550E-15, 4.280079833532960850E-15 ) ) ;
#23609 = CARTESIAN_POINT ( 'NONE',  ( 0.1787899950787401604, -1.096580661142624757, -0.07405724077823318263 ) ) ;
#23610 = VERTEX_POINT ( 'NONE', #26480 ) ;
#23611 = CARTESIAN_POINT ( 'NONE',  ( 3.284318927891251994E-17, 0.009350393754550925460, 0.1787899950787401882 ) ) ;
#23612 = ORIENTED_EDGE ( 'NONE', *, *, #36465, .F. ) ;
#23613 = ORIENTED_EDGE ( 'NONE', *, *, #10180, .T. ) ;
#23614 = EDGE_CURVE ( 'NONE', #23115, #7550, #14767, .T. ) ;
#23615 = CARTESIAN_POINT ( 'NONE',  ( -0.2559061271197219378, -0.05275274989394477393, -0.3118637899121943780 ) ) ;
#23616 = CARTESIAN_POINT ( 'NONE',  ( 1.033464566929134687, -0.06523048226347956391, 0.1156496061916856694 ) ) ;
#23617 = EDGE_CURVE ( 'NONE', #16359, #16139, #22905, .T. ) ;
#23618 = VECTOR ( 'NONE', #16221, 39.37007874015748143 ) ;
#23619 = CARTESIAN_POINT ( 'NONE',  ( 0.7185039370078739607, 1.928577636452523993E-17, 1.879921259842519676 ) ) ;
#23620 = CARTESIAN_POINT ( 'NONE',  ( 0.1787899950787401882, -0.6156496062454488438, -2.189545951927503898E-17 ) ) ;
#23621 = AXIS2_PLACEMENT_3D ( 'NONE', #5266, #8623, #34514 ) ;
#23622 = ( BOUNDED_CURVE ( )  B_SPLINE_CURVE ( 2, ( #33505, #30619, #617, #44472, #8298, #22690, #30163, #11924, #22927 ),
 .UNSPECIFIED., .F., .T. ) 
 B_SPLINE_CURVE_WITH_KNOTS ( ( 3, 2, 2, 2, 3 ),
 ( 0.1900000000000000022, 0.1925000000000000044, 0.1950000000000000067, 0.1975000000000000089, 0.2000000000000000111 ),
 .UNSPECIFIED. ) 
 CURVE ( )  GEOMETRIC_REPRESENTATION_ITEM ( )  RATIONAL_B_SPLINE_CURVE ( ( 1.000000000000000000, 0.9238795325112869605, 1.000000000000000000, 0.9238795325112869605, 1.000000000000000000, 0.9238795325112869605, 1.000000000000000000, 0.9238795325112879597, 1.000000000000000000 ) ) 
 REPRESENTATION_ITEM ( '' )  ) ;
#23623 = CARTESIAN_POINT ( 'NONE',  ( -0.6971942568897637749, 2.189545951927499583E-17, 0.2042322834108035723 ) ) ;
#23624 = CARTESIAN_POINT ( 'NONE',  ( -0.9412147342319837628, -0.1574803149606297803, 1.104822834645670104 ) ) ;
#23625 = CARTESIAN_POINT ( 'NONE',  ( -0.1797182628040039365, -1.142760345016116119, 0.000000000000000000 ) ) ;
#23626 = CARTESIAN_POINT ( 'NONE',  ( 1.054774247047244540, -0.07405724077823318263, 1.048228346402930944 ) ) ;
#23627 = CARTESIAN_POINT ( 'NONE',  ( 0.9500414927467377701, 0.1787899950787401604, 1.446850393647023836 ) ) ;
#23628 = CARTESIAN_POINT ( 'NONE',  ( 0.6971942568897626646, -0.07405724077823297447, 0.1230314960092287191 ) ) ;
#23629 = DIRECTION ( 'NONE',  ( 0.000000000000000000, 0.000000000000000000, 1.000000000000000000 ) ) ;
#23630 = CARTESIAN_POINT ( 'NONE',  ( 0.7185039370078746268, -0.06523048226347956391, 1.488681102362205300 ) ) ;
#23632 = FACE_OUTER_BOUND ( 'NONE', #43518, .T. ) ;
#23631 = CARTESIAN_POINT ( 'NONE',  ( 0.7830934527162080050, 0.1313591056386028688, 1.980287732290521019 ) ) ;
#23633 = LINE ( 'NONE', #26771, #29018 ) ;
#23634 = PLANE ( 'NONE',  #45964 ) ;
#23635 = CARTESIAN_POINT ( 'NONE',  ( 0.8019270111902716547, 0.1787899950787401604, 0.9793307086076531442 ) ) ;
#23636 = CARTESIAN_POINT ( 'NONE',  ( 1.002407869896990045, -0.1264236179284866091, 1.754429133804503715 ) ) ;
#23637 = CARTESIAN_POINT ( 'NONE',  ( 0.8107537697050253289, 0.1574803149606300301, 0.3666338581601894520 ) ) ;
#23638 = ORIENTED_EDGE ( 'NONE', *, *, #3076, .F. ) ;
#23639 = LINE ( 'NONE', #27743, #21479 ) ;
#23640 = CARTESIAN_POINT ( 'NONE',  ( 0.1113553986120547346, -1.646653543199559033, -0.1113553986120547346 ) ) ;
#23641 = CARTESIAN_POINT ( 'NONE',  ( -0.9412147342319837628, 0.1574803149606300301, 0.2436023620971974057 ) ) ;
#23642 = CARTESIAN_POINT ( 'NONE',  ( 0.8759842519685039353, 0.000000000000000000, 4.498031496062992574 ) ) ;
#23643 = CARTESIAN_POINT ( 'NONE',  ( 0.6971942568897637749, 2.189545951927499583E-17, 1.222933070812378009 ) ) ;
#23644 = EDGE_CURVE ( 'NONE', #8746, #8447, #14003, .T. ) ;
#23645 = ORIENTED_EDGE ( 'NONE', *, *, #30937, .F. ) ;
#23646 = CARTESIAN_POINT ( 'NONE',  ( 0.01960094289354776670, -0.05179116514259233389, 0.2741164612101792963 ) ) ;
#23647 = CARTESIAN_POINT ( 'NONE',  ( 0.1574803149606300301, -1.777066929133858109, -0.06523048226347956391 ) ) ;
#23648 = LINE ( 'NONE', #20043, #26810 ) ;
#23649 = AXIS2_PLACEMENT_3D ( 'NONE', #26181, #32441, #36492 ) ;
#23650 = CARTESIAN_POINT ( 'NONE',  ( -0.6971942568897637749, 2.189545951927499583E-17, 0.5536417322297008115 ) ) ;
#23651 = CARTESIAN_POINT ( 'NONE',  ( -0.9412147342319837628, -0.1574803149606297803, 0.2780511811023620439 ) ) ;
#23652 = CARTESIAN_POINT ( 'NONE',  ( -0.05635946233522095422, 0.07780450164205261754, 0.2528939201155192551 ) ) ;
#23653 = AXIS2_PLACEMENT_3D ( 'NONE', #18259, #14911, #29574 ) ;
#23654 = EDGE_CURVE ( 'NONE', #34498, #41232, #36948, .T. ) ;
#23655 = CARTESIAN_POINT ( 'NONE',  ( -0.1787899950787401604, -1.577755905458046115, 0.07405724077823318263 ) ) ;
#23656 = CARTESIAN_POINT ( 'NONE',  ( -1.054774247047244096, 0.000000000000000000, 1.050688976324189117 ) ) ;
#23657 = CARTESIAN_POINT ( 'NONE',  ( -1.054774247047244096, 0.000000000000000000, 1.793799212544661348 ) ) ;
#23658 = CARTESIAN_POINT ( 'NONE',  ( -0.7495606340400177148, 0.1264236179284866091, 0.9817913385289134265 ) ) ;
#23659 = VECTOR ( 'NONE', #19588, 39.37007874015748143 ) ;
#23660 = CARTESIAN_POINT ( 'NONE',  ( -0.7495606340400177148, -0.1264236179284866091, 0.7209645668753701386 ) ) ;
#23661 = VERTEX_POINT ( 'NONE', #7305 ) ;
#23662 = DIRECTION ( 'NONE',  ( -0.5735764363510518216, 0.8191520442889876907, 1.003171929053519693E-16 ) ) ;
#23663 = CARTESIAN_POINT ( 'NONE',  ( 0.2395294000716133853, -0.1968503937007874127, -0.4921259842519685179 ) ) ;
#23664 = DIRECTION ( 'NONE',  ( 0.000000000000000000, -1.000000000000000000, 0.000000000000000000 ) ) ;
#23665 = CARTESIAN_POINT ( 'NONE',  ( -0.1264236179284866091, -0.6019940469693956242, 0.1264236179284866091 ) ) ;
#23666 = CARTESIAN_POINT ( 'NONE',  ( -0.1316538794915708688, -0.08956060683158523217, -0.1194074894494051159 ) ) ;
#23667 = AXIS2_PLACEMENT_3D ( 'NONE', #14568, #7377, #44473 ) ;
#23668 = CARTESIAN_POINT ( 'NONE',  ( 0.7185039370078739607, 1.928577636452523993E-17, 1.801181102362204633 ) ) ;
#23669 = EDGE_LOOP ( 'NONE', ( #10653, #8064, #14422, #32018, #40461 ) ) ;
#23670 = CARTESIAN_POINT ( 'NONE',  ( 0.1476377952755906220, 0.7443365962042343131, -3.523993443072799270 ) ) ;
#23671 = CARTESIAN_POINT ( 'NONE',  ( -0.9500414927467378812, -0.1787899950787401604, 0.4478346456155276045 ) ) ;
#23672 = LINE ( 'NONE', #11956, #21860 ) ;
#23673 = ORIENTED_EDGE ( 'NONE', *, *, #35571, .F. ) ;
#23674 = DIRECTION ( 'NONE',  ( 0.000000000000000000, 0.000000000000000000, 1.000000000000000000 ) ) ;
#23675 = CARTESIAN_POINT ( 'NONE',  ( -0.8759842519685039353, 0.1787899950787401882, 1.532972440891118060 ) ) ;
#23676 = CARTESIAN_POINT ( 'NONE',  ( -0.1264236179284866091, -1.535925196796629866, 0.1264236179284866091 ) ) ;
#23677 = CARTESIAN_POINT ( 'NONE',  ( -0.1567662409572586624, 0.000000000000000000, -0.0004999999999998990712 ) ) ;
#23678 = AXIS2_PLACEMENT_3D ( 'NONE', #34315, #1446, #30961 ) ;
#23679 = CARTESIAN_POINT ( 'NONE',  ( 0.1270800023317771588, -0.6457131009216279249, -0.1270800023317771588 ) ) ;
#23680 = CARTESIAN_POINT ( 'NONE',  ( 1.033464566929134687, -0.06523048226347956391, 0.9522637795275589179 ) ) ;
#23681 = CARTESIAN_POINT ( 'NONE',  ( -0.8107537697050253289, -0.1574803149606297803, 1.168799212490898354 ) ) ;
#23682 = CARTESIAN_POINT ( 'NONE',  ( 0.6971942568897626646, 0.07405724077823318263, 0.07874015742655143812 ) ) ;
#23684 = CARTESIAN_POINT ( 'NONE',  ( -0.8759842519685039353, 0.1574803149606299191, 1.624015747923968522 ) ) ;
#23683 = CARTESIAN_POINT ( 'NONE',  ( 0.06523048226347956391, -0.3695866141732285781, 0.1574803149606297803 ) ) ;
#23685 = DIRECTION ( 'NONE',  ( 0.000000000000000000, 0.000000000000000000, 1.000000000000000000 ) ) ;
#23686 = ORIENTED_EDGE ( 'NONE', *, *, #2215, .F. ) ;
#23687 = DIRECTION ( 'NONE',  ( 0.000000000000000000, -1.778091562876227272E-15, 1.000000000000000000 ) ) ;
#23688 = CARTESIAN_POINT ( 'NONE',  ( -0.6971942568897637749, 2.189545951927499583E-17, 1.149114173174582643 ) ) ;
#23689 = CARTESIAN_POINT ( 'NONE',  ( 0.7185039370078746268, 0.06523048226347956391, 1.129429133858268042 ) ) ;
#23690 = DIRECTION ( 'NONE',  ( 0.000000000000000000, 0.7880107536067203489, -0.6156614753256604011 ) ) ;
#23691 = AXIS2_PLACEMENT_3D ( 'NONE', #33718, #1070, #12609 ) ;
#23692 = DIRECTION ( 'NONE',  ( 1.822029033848725028E-16, 0.000000000000000000, 1.000000000000000000 ) ) ;
#23694 = LINE ( 'NONE', #8835, #4026 ) ;
#23693 = CARTESIAN_POINT ( 'NONE',  ( -0.1377952755905510196, 0.000000000000000000, -0.1828167807439035619 ) ) ;
#23695 = LINE ( 'NONE', #34256, #11682 ) ;
#23696 = CARTESIAN_POINT ( 'NONE',  ( -0.1605366408340857254, -0.08956085509329067551, -0.06625698018490121244 ) ) ;
#23697 = CARTESIAN_POINT ( 'NONE',  ( 0.1787899950787401604, -0.5738188975840317063, 0.07405724077823318263 ) ) ;
#23698 = VECTOR ( 'NONE', #37074, 39.37007874015748854 ) ;
#23699 = CARTESIAN_POINT ( 'NONE',  ( 0.8759842519685039353, -0.1574803149606299191, 0.2755905511811023723 ) ) ;
#23700 = CARTESIAN_POINT ( 'NONE',  ( 0.6971942568897626646, -0.07405724077823297447, 0.8316929133320636325 ) ) ;
#23701 = EDGE_CURVE ( 'NONE', #41516, #16491, #14737, .T. ) ;
#23702 = ORIENTED_EDGE ( 'NONE', *, *, #2162, .F. ) ;
#23703 = CARTESIAN_POINT ( 'NONE',  ( 0.8107537697050254399, -0.1574803149606297803, 1.454232283464566677 ) ) ;
#23704 = CARTESIAN_POINT ( 'NONE',  ( 0.7185039370078739607, 1.928577636452523993E-17, 0.8956692913385826404 ) ) ;
#23705 = CARTESIAN_POINT ( 'NONE',  ( -0.07405724077823318263, -1.725393700733637958, 0.1787899950787401604 ) ) ;
#23706 = CARTESIAN_POINT ( 'NONE',  ( -0.07405724077823318263, -0.9035433070328510174, 0.1787899950787401604 ) ) ;
#23707 = CARTESIAN_POINT ( 'NONE',  ( 0.06523048226347956391, -1.353838582677164393, 0.1574803149606297803 ) ) ;
#23708 = CARTESIAN_POINT ( 'NONE',  ( 0.8759842519685039353, 0.1574803149606299191, 1.269685039262551163 ) ) ;
#23709 = EDGE_CURVE ( 'NONE', #5685, #37269, #43814, .T. ) ;
#23710 = FACE_OUTER_BOUND ( 'NONE', #47353, .T. ) ;
#23711 = ORIENTED_EDGE ( 'NONE', *, *, #44860, .T. ) ;
#23712 = VERTEX_POINT ( 'NONE', #11623 ) ;
#23713 = CARTESIAN_POINT ( 'NONE',  ( -1.054774247047244096, 0.000000000000000000, 1.877460629867496067 ) ) ;
#23714 = EDGE_CURVE ( 'NONE', #25679, #41157, #26242, .T. ) ;
#23715 = CARTESIAN_POINT ( 'NONE',  ( 1.054774247047244096, 0.000000000000000000, 1.838090551127338657 ) ) ;
#23716 = ORIENTED_EDGE ( 'NONE', *, *, #26913, .T. ) ;
#23717 = CARTESIAN_POINT ( 'NONE',  ( 0.4736248074375440931, 1.890321945096787193, -4.194630839571732217 ) ) ;
#23718 = CARTESIAN_POINT ( 'NONE',  ( 0.9500414927467378812, 0.1787899950787401604, 0.4281496062454490659 ) ) ;
#23719 = CARTESIAN_POINT ( 'NONE',  ( -1.002407869896990045, 0.1264236179284866091, 1.326279527505291433 ) ) ;
#23720 = EDGE_CURVE ( 'NONE', #42434, #3668, #4830, .T. ) ;
#23721 = DIRECTION ( 'NONE',  ( 0.000000000000000000, 0.000000000000000000, -1.000000000000000000 ) ) ;
#23722 = CARTESIAN_POINT ( 'NONE',  ( -0.7495606340400177148, 0.1264236179284866091, 0.9817913385289134265 ) ) ;
#23723 = CARTESIAN_POINT ( 'NONE',  ( -1.054774247047244096, 0.000000000000000000, 0.02706692908009476414 ) ) ;
#23724 = CARTESIAN_POINT ( 'NONE',  ( 0.2471922904502826812, -0.09842519685039370636, -0.1427165354330708902 ) ) ;
#23725 = CARTESIAN_POINT ( 'NONE',  ( -0.6971942568897648851, 0.07405724077823318263, 1.815944881835999558 ) ) ;
#23726 = CARTESIAN_POINT ( 'NONE',  ( -0.7185039370078739607, 1.928577636452523993E-17, 1.988188976270425234 ) ) ;
#23727 = CARTESIAN_POINT ( 'NONE',  ( 0.7185039370078739607, 1.928577636452523993E-17, 1.397637795168062969 ) ) ;
#23728 = CARTESIAN_POINT ( 'NONE',  ( -1.033464566929134687, -0.06523048226347956391, 1.779035433070867089 ) ) ;
#23729 = CARTESIAN_POINT ( 'NONE',  ( 0.1574803149606299746, -0.5708661417322835607, -6.991093932140394160E-17 ) ) ;
#23730 = CARTESIAN_POINT ( 'NONE',  ( 0.8019270111902716547, 0.1787899950787401604, 1.692913385773008539 ) ) ;
#23731 = CARTESIAN_POINT ( 'NONE',  ( 0.02145185034013027958, -0.09842519685039370636, -0.1903359544148515714 ) ) ;
#23732 = CARTESIAN_POINT ( 'NONE',  ( 0.8759842519685039353, 0.000000000000000000, 4.498031496062992574 ) ) ;
#23733 = CARTESIAN_POINT ( 'NONE',  ( -0.7646288533564489232, 0.1113553986120547346, 1.796259842519684957 ) ) ;
#23734 = ORIENTED_EDGE ( 'NONE', *, *, #8504, .T. ) ;
#23735 = ORIENTED_EDGE ( 'NONE', *, *, #11179, .T. ) ;
#23736 = CARTESIAN_POINT ( 'NONE',  ( -0.07405724077823318263, -1.036417322780882833, -0.1787899950787401604 ) ) ;
#23737 = CARTESIAN_POINT ( 'NONE',  ( -0.1787899950787401604, -1.179133858213953001, 0.07405724077823318263 ) ) ;
#23738 = DIRECTION ( 'NONE',  ( 7.047314121155781188E-15, 0.000000000000000000, 1.000000000000000000 ) ) ;
#23739 = CARTESIAN_POINT ( 'NONE',  ( 0.9500414927467378812, 0.1787899950787401604, 0.3838582676627718127 ) ) ;
#23740 = CARTESIAN_POINT ( 'NONE',  ( 0.07444174185955046430, -0.5251422347798958556, -0.1797182628040039087 ) ) ;
#23741 = CARTESIAN_POINT ( 'NONE',  ( -0.06523048226347956391, 0.08316929133858275147, -0.1574803149606300301 ) ) ;
#23742 = CARTESIAN_POINT ( 'NONE',  ( 0.6971942568897637749, 2.189545951927499583E-17, 0.8686023621509606496 ) ) ;
#23743 = VECTOR ( 'NONE', #33757, 39.37007874015748143 ) ;
#23744 = CARTESIAN_POINT ( 'NONE',  ( 1.033464566929133799, 0.000000000000000000, 0.6003937007874016185 ) ) ;
#23745 = CARTESIAN_POINT ( 'NONE',  ( 0.8107537697050253289, 0.1574803149606300301, 0.05167322823892971095 ) ) ;
#23746 = VECTOR ( 'NONE', #30554, 39.37007874015748143 ) ;
#23747 = ORIENTED_EDGE ( 'NONE', *, *, #11703, .F. ) ;
#23748 = CARTESIAN_POINT ( 'NONE',  ( 0.2066929133858268486, 0.7443365962042343131, -3.523993443072799270 ) ) ;
#23749 = CARTESIAN_POINT ( 'NONE',  ( -0.1787899950787401882, -0.3597440944344256208, 0.000000000000000000 ) ) ;
#23750 = CIRCLE ( 'NONE', #6120, 0.09842519685039370636 ) ;
#23751 = CARTESIAN_POINT ( 'NONE',  ( -0.1787899950787401604, -1.380905511757260173, -0.07405724077823318263 ) ) ;
#23752 = CARTESIAN_POINT ( 'NONE',  ( 0.8019270111902717657, 0.1787899950787401604, 0.3543307086076538659 ) ) ;
#23753 = ADVANCED_FACE ( 'NONE', ( #20202 ), #20861, .F. ) ;
#23754 = CARTESIAN_POINT ( 'NONE',  ( -1.054774247047244096, 0.000000000000000000, 1.872539370024976391 ) ) ;
#23755 = ORIENTED_EDGE ( 'NONE', *, *, #26876, .T. ) ;
#23756 = CARTESIAN_POINT ( 'NONE',  ( -0.6971942568897648851, -0.07405724077823297447, 1.505905511757261284 ) ) ;
#23757 = EDGE_CURVE ( 'NONE', #24486, #2197, #31489, .T. ) ;
#23758 = CARTESIAN_POINT ( 'NONE',  ( 0.7495606340400177148, 0.1264236179284866091, 1.459153543253322693 ) ) ;
#23759 = CARTESIAN_POINT ( 'NONE',  ( 0.8070866141732283561, 0.000000000000000000, 0.6580708661417323802 ) ) ;
#23760 = CARTESIAN_POINT ( 'NONE',  ( 0.7495606340400177148, -0.1264236179284866091, 0.09104330703285078152 ) ) ;
#23761 = CARTESIAN_POINT ( 'NONE',  ( -0.6971942568897648851, 0.07405724077823318263, 1.181102362150960428 ) ) ;
#23762 = EDGE_CURVE ( 'NONE', #16198, #42764, #45545, .T. ) ;
#23763 = CARTESIAN_POINT ( 'NONE',  ( 0.1598064471924473817, -0.09842432027591681287, -0.08022707942853385399 ) ) ;
#23764 = FACE_OUTER_BOUND ( 'NONE', #26108, .T. ) ;
#23765 = CARTESIAN_POINT ( 'NONE',  ( 1.002407869896990045, 0.1264236179284866091, 0.6619094487651338010 ) ) ;
#23766 = CARTESIAN_POINT ( 'NONE',  ( -0.8019270111902716547, 0.1787899950787401604, 0.5856299212060785964 ) ) ;
#23767 = FILL_AREA_STYLE_COLOUR ( '', #10065 ) ;
#23768 = CARTESIAN_POINT ( 'NONE',  ( 0.8107537697050254399, 0.1574803149606300301, 1.665846456585386548 ) ) ;
#23769 = ORIENTED_EDGE ( 'NONE', *, *, #14189, .F. ) ;
#23770 = ORIENTED_EDGE ( 'NONE', *, *, #24615, .F. ) ;
#23771 = CARTESIAN_POINT ( 'NONE',  ( -0.9873396505805591694, 0.1113553986120547346, 0.3690944881889763884 ) ) ;
#23772 = CARTESIAN_POINT ( 'NONE',  ( -0.06406129441507303623, -0.09851384877607578805, 0.2183140915305173402 ) ) ;
#23773 = VERTEX_POINT ( 'NONE', #2229 ) ;
#23774 = CARTESIAN_POINT ( 'NONE',  ( -0.6971942568897626646, 0.07405724077823318263, 0.9498031495525356416 ) ) ;
#23775 = AXIS2_PLACEMENT_3D ( 'NONE', #7243, #25934, #36712 ) ;
#23776 = CARTESIAN_POINT ( 'NONE',  ( -0.8019270111902717657, -0.1787899950787401604, 0.1279527558517483676 ) ) ;
#23777 = CARTESIAN_POINT ( 'NONE',  ( 0.1264236179284866091, -1.576403495788293530, 0.1264236179284866091 ) ) ;
#23778 = ORIENTED_EDGE ( 'NONE', *, *, #4543, .F. ) ;
#23779 = CARTESIAN_POINT ( 'NONE',  ( -0.9412147342319837628, 0.1574803149606300301, 1.385334645561763445 ) ) ;
#23780 = CARTESIAN_POINT ( 'NONE',  ( 0.1787899950787401882, -0.5713582676627716461, -2.189545951927503898E-17 ) ) ;
#23781 = CARTESIAN_POINT ( 'NONE',  ( 2.892866454678787531E-17, 0.07086614183981043702, 0.1574803149606299191 ) ) ;
#23782 = ORIENTED_EDGE ( 'NONE', *, *, #36965, .T. ) ;
#23783 = ( GEOMETRIC_REPRESENTATION_CONTEXT ( 3 ) GLOBAL_UNCERTAINTY_ASSIGNED_CONTEXT ( ( #17224 ) ) GLOBAL_UNIT_ASSIGNED_CONTEXT ( ( #18094, #6351, #7314 ) ) REPRESENTATION_CONTEXT ( 'NONE', 'WORKASPACE' ) ) ;
#23784 = EDGE_CURVE ( 'NONE', #16808, #43835, #30910, .T. ) ;
#23785 = CARTESIAN_POINT ( 'NONE',  ( 0.001477421097737172118, 0.1327706367220780892, 0.04562747989112364566 ) ) ;
#23786 = AXIS2_PLACEMENT_3D ( 'NONE', #5144, #30585, #23381 ) ;
#23787 = CARTESIAN_POINT ( 'NONE',  ( 0.5358894627757212481, -0.09842519685039370636, 1.205361022782828805E-17 ) ) ;
#23788 = CARTESIAN_POINT ( 'NONE',  ( 0.07405724077823318263, -0.8001968503399367050, -0.1787899950787401604 ) ) ;
#23789 = CARTESIAN_POINT ( 'NONE',  ( 0.9412147342319837628, -0.1574803149606297803, 0.1894685038294807999 ) ) ;
#23790 = CARTESIAN_POINT ( 'NONE',  ( 0.8019270111902717657, -0.1787899950787401604, 1.624015747977732849 ) ) ;
#23791 = VECTOR ( 'NONE', #18381, 39.37007874015748143 ) ;
#23792 = CARTESIAN_POINT ( 'NONE',  ( 0.1787899950787401882, -0.03604916507963244754, -2.189545951927503898E-17 ) ) ;
#23793 = CARTESIAN_POINT ( 'NONE',  ( -0.1787899950787401882, 0.1520669291876218521, 0.000000000000000000 ) ) ;
#23794 = CARTESIAN_POINT ( 'NONE',  ( 0.9500414927467378812, 0.1787899950787401604, 0.4232283464029293896 ) ) ;
#23795 = CARTESIAN_POINT ( 'NONE',  ( -0.6971942568897648851, 0.07405724077823318263, 0.8316929133320636325 ) ) ;
#23796 = CARTESIAN_POINT ( 'NONE',  ( -0.1113553986120547346, -0.9281496062992126150, 0.1113553986120547346 ) ) ;
#23798 = CARTESIAN_POINT ( 'NONE',  ( -0.8186592603503980436, -0.1631638552240416984, 1.987135399130128155 ) ) ;
#23797 = CARTESIAN_POINT ( 'NONE',  ( -1.100456976456230270E-17, -1.546303652102730242, -0.1797182628040039365 ) ) ;
#23799 = CARTESIAN_POINT ( 'NONE',  ( -0.06523048226347956391, -0.4827755904436537571, 0.1574803149606297803 ) ) ;
#23800 = CARTESIAN_POINT ( 'NONE',  ( 0.1787899950787401604, -0.4163385826234020093, 0.07405724077823318263 ) ) ;
#23801 = CARTESIAN_POINT ( 'NONE',  ( -0.9873396505805591694, -0.1113553986120547346, 1.254921259734991912 ) ) ;
#23802 = CARTESIAN_POINT ( 'NONE',  ( 1.002407869896990045, 0.1264236179284866091, 1.528051181048598384 ) ) ;
#23803 = CARTESIAN_POINT ( 'NONE',  ( 0.9500414927467377701, -0.1787899950787401604, 1.865157480261198097 ) ) ;
#23804 = CARTESIAN_POINT ( 'NONE',  ( 0.8759842519685039353, 0.1787899950787401882, 0.3469488188438744070 ) ) ;
#23805 = ORIENTED_EDGE ( 'NONE', *, *, #24792, .F. ) ;
#23806 = DIRECTION ( 'NONE',  ( 0.000000000000000000, 0.000000000000000000, 1.000000000000000000 ) ) ;
#23807 = FACE_OUTER_BOUND ( 'NONE', #15137, .T. ) ;
#23808 = CARTESIAN_POINT ( 'NONE',  ( 1.928577636452524610E-17, -0.09842519685039370636, -0.1574803149606299191 ) ) ;
#23809 = CARTESIAN_POINT ( 'NONE',  ( -0.07405724077823318263, 0.02657480320336980464, -0.1787899950787401604 ) ) ;
#23810 = CARTESIAN_POINT ( 'NONE',  ( 0.7495606340400177148, 0.1264236179284866091, 0.3912401574265515491 ) ) ;
#23811 = ADVANCED_FACE ( 'NONE', ( #4565 ), #32395, .F. ) ;
#23812 = CARTESIAN_POINT ( 'NONE',  ( 0.7646288533564489232, -0.1113553986120547346, 1.953740157372787500 ) ) ;
#23813 = CARTESIAN_POINT ( 'NONE',  ( -0.9873396505805591694, 0.1113553986120547346, 1.579724409341291214 ) ) ;
#23814 = CARTESIAN_POINT ( 'NONE',  ( -1.002407869896990045, 0.1264236179284866091, 1.405019684985606476 ) ) ;
#23815 = CARTESIAN_POINT ( 'NONE',  ( 0.7646288533564489232, -0.1113553986120547346, 0.7726377951680629685 ) ) ;
#23816 = VERTEX_POINT ( 'NONE', #3650 ) ;
#23817 = CARTESIAN_POINT ( 'NONE',  ( -0.7185039370078739607, 0.000000000000000000, -2.869337061179095023E-17 ) ) ;
#23818 = CARTESIAN_POINT ( 'NONE',  ( 0.9500414927467378812, -0.1787899950787401604, 1.082677165300567346 ) ) ;
#23819 = VERTEX_POINT ( 'NONE', #11560 ) ;
#23822 = ORIENTED_EDGE ( 'NONE', *, *, #13868, .T. ) ;
#23821 = CARTESIAN_POINT ( 'NONE',  ( -0.07405724077823318263, -1.312007873961984705, -0.1787899950787401604 ) ) ;
#23820 = CARTESIAN_POINT ( 'NONE',  ( 0.1113553986120547346, -1.105314960522393752, 0.1113553986120547346 ) ) ;
#23823 = CARTESIAN_POINT ( 'NONE',  ( -1.033464566929134687, 0.06523048226347956391, 0.6323818896562525271 ) ) ;
#23824 = VECTOR ( 'NONE', #43136, 39.37007874015748143 ) ;
#23825 = CARTESIAN_POINT ( 'NONE',  ( 0.9412147342319837628, 0.1574803149606300301, 0.09596456692913379882 ) ) ;
#23826 = CARTESIAN_POINT ( 'NONE',  ( -0.7185039370078746268, -0.06523048226347956391, 1.409940944881891367 ) ) ;
#23827 = EDGE_CURVE ( 'NONE', #15855, #47016, #17834, .T. ) ;
#23828 = CARTESIAN_POINT ( 'NONE',  ( -7.957671378281915615E-17, 0.1574803149606340824, -0.3937007874015748254 ) ) ;
#23830 = DIRECTION ( 'NONE',  ( 0.000000000000000000, -1.000000000000000000, 0.000000000000000000 ) ) ;
#23829 = DIRECTION ( 'NONE',  ( 1.000000000000000000, -5.464378949326940770E-15, 4.275490733183370330E-15 ) ) ;
#23831 = CARTESIAN_POINT ( 'NONE',  ( 1.054774247047244540, 0.07405724077823318263, 0.1870078739619845110 ) ) ;
#23832 = VECTOR ( 'NONE', #39744, 39.37007874015748143 ) ;
#23833 = CARTESIAN_POINT ( 'NONE',  ( 0.8107537697050253289, -0.1574803149606297803, 1.405019684931842816 ) ) ;
#23834 = ORIENTED_EDGE ( 'NONE', *, *, #22719, .T. ) ;
#23835 = ORIENTED_EDGE ( 'NONE', *, *, #259, .F. ) ;
#23836 = CARTESIAN_POINT ( 'NONE',  ( -0.1787899950787401604, 0.07578740162856664742, 0.07405724077823318263 ) ) ;
#23837 = DIRECTION ( 'NONE',  ( -1.000000000000000000, 0.000000000000000000, 2.392722035830075028E-16 ) ) ;
#23838 = CARTESIAN_POINT ( 'NONE',  ( 0.7495606340400177148, 0.1264236179284866091, 0.7111220471903307860 ) ) ;
#23839 = CARTESIAN_POINT ( 'NONE',  ( -0.9500414927467377701, 0.1787899950787401604, 1.761811023568284229 ) ) ;
#23840 = CARTESIAN_POINT ( 'NONE',  ( -0.06523048226347956391, -0.2071850392625517456, 0.1574803149606297803 ) ) ;
#23841 = VERTEX_POINT ( 'NONE', #11802 ) ;
#23842 = DIRECTION ( 'NONE',  ( -0.7986355100472960489, 0.000000000000000000, 0.6018150231520440485 ) ) ;
#23843 = DIRECTION ( 'NONE',  ( 1.151683635503274272E-16, -4.091602205503172741E-31, 1.000000000000000000 ) ) ;
#23844 = CARTESIAN_POINT ( 'NONE',  ( -0.1787899950787401604, -1.199927117835539292, -0.07405724077823318263 ) ) ;
#23845 = EDGE_LOOP ( 'NONE', ( #3761, #14652, #2395, #32393, #20974, #14286 ) ) ;
#23846 = CARTESIAN_POINT ( 'NONE',  ( 0.1787899950787401604, -0.1751968503399373434, -0.07405724077823318263 ) ) ;
#23847 = VERTEX_POINT ( 'NONE', #26421 ) ;
#23848 = VERTEX_POINT ( 'NONE', #7473 ) ;
#23849 = CARTESIAN_POINT ( 'NONE',  ( -0.2559005158470596397, -0.09846603769604915513, -0.3044373381439980930 ) ) ;
#23850 = EDGE_CURVE ( 'NONE', #11246, #11416, #41685, .T. ) ;
#23851 = CARTESIAN_POINT ( 'NONE',  ( -0.7646288533564489232, -0.1113553986120547346, 0.4183070865066456645 ) ) ;
#23852 = AXIS2_PLACEMENT_3D ( 'NONE', #45226, #31132, #41863 ) ;
#23853 = CARTESIAN_POINT ( 'NONE',  ( 0.7646288533564489232, 0.1113553986120547346, 1.875000000000000000 ) ) ;
#23854 = AXIS2_PLACEMENT_3D ( 'NONE', #2667, #38862, #16602 ) ;
#23855 = ( GEOMETRIC_REPRESENTATION_CONTEXT ( 3 ) GLOBAL_UNCERTAINTY_ASSIGNED_CONTEXT ( ( #46437 ) ) GLOBAL_UNIT_ASSIGNED_CONTEXT ( ( #34333, #1463, #34810 ) ) REPRESENTATION_CONTEXT ( 'NONE', 'WORKASPACE' ) ) ;
#23856 = CARTESIAN_POINT ( 'NONE',  ( -0.1264236179284866091, -0.6697834645131652831, 0.1264236179284866091 ) ) ;
#23857 = AXIS2_PLACEMENT_3D ( 'NONE', #25351, #35881, #7363 ) ;
#23858 = CARTESIAN_POINT ( 'NONE',  ( -0.7495606340400177148, -0.1264236179284866091, 0.3272637794737956463 ) ) ;
#23859 = CARTESIAN_POINT ( 'NONE',  ( -0.9873396505805591694, 0.1113553986120547346, 1.038385826771653475 ) ) ;
#23861 = CARTESIAN_POINT ( 'NONE',  ( -0.7162142114693390571, 0.04048521711225155223, 1.982498882657834915 ) ) ;
#23860 = CARTESIAN_POINT ( 'NONE',  ( 3.301370929368692659E-17, -1.172287904071234177, 0.1797182628040039365 ) ) ;
#23862 = CARTESIAN_POINT ( 'NONE',  ( 0.8070866141732283561, 0.000000000000000000, -0.8568897637795275246 ) ) ;
#23863 = CARTESIAN_POINT ( 'NONE',  ( 0.8759842519685039353, -0.1787899950787401882, 1.040846456639149764 ) ) ;
#23864 = CARTESIAN_POINT ( 'NONE',  ( -0.8759842519685039353, 0.000000000000000000, 0.000000000000000000 ) ) ;
#23865 = CARTESIAN_POINT ( 'NONE',  ( 1.033464566929134687, -0.06523048226347956391, 1.503444881889762774 ) ) ;
#23867 = DIRECTION ( 'NONE',  ( -3.469446951953614189E-15, -1.000000000000000000, 0.000000000000000000 ) ) ;
#23866 = CARTESIAN_POINT ( 'NONE',  ( 0.7945469227473396234, 0.1381752303017431960, 1.980025006398726806 ) ) ;
#23868 = CARTESIAN_POINT ( 'NONE',  ( 0.1527862493557218537, -0.4068158579509408290, -0.9303620633370848214 ) ) ;
#23869 = CARTESIAN_POINT ( 'NONE',  ( 0.1574803149606300301, -0.7485236219397169988, 0.06523048226347956391 ) ) ;
#23870 = CARTESIAN_POINT ( 'NONE',  ( -0.8107537697050253289, -0.1574803149606297803, 1.641240157372788611 ) ) ;
#23871 = FACE_OUTER_BOUND ( 'NONE', #9029, .T. ) ;
#23872 = EDGE_CURVE ( 'NONE', #5354, #16198, #40371, .T. ) ;
#23874 = CARTESIAN_POINT ( 'NONE',  ( 0.1645805237892204731, 0.1627998762483226503, -0.0008383936782242519276 ) ) ;
#23873 = CARTESIAN_POINT ( 'NONE',  ( 0.9500414927467377701, 0.1787899950787401604, 0.9350393700249758355 ) ) ;
#23875 = CARTESIAN_POINT ( 'NONE',  ( 0.8759842519685039353, -0.1574803149606299191, 0.3838582676090082635 ) ) ;
#23876 = ORIENTED_EDGE ( 'NONE', *, *, #21480, .F. ) ;
#23877 = CARTESIAN_POINT ( 'NONE',  ( 0.8107537697050254399, -0.1574803149606297803, 1.247539369971212508 ) ) ;
#23878 = CARTESIAN_POINT ( 'NONE',  ( 1.030962330798375515, 0.04070495257795413852, 0.03937007855506236692 ) ) ;
#23879 = CARTESIAN_POINT ( 'NONE',  ( 0.9412147342319837628, -0.1574803149606297803, 0.2386811023622048278 ) ) ;
#23880 = CARTESIAN_POINT ( 'NONE',  ( -0.1574803149606300301, -1.673720472333417808, -0.06523048226347956391 ) ) ;
#23881 = CARTESIAN_POINT ( 'NONE',  ( -0.9412147342319837628, -0.1574803149606297803, 0.1894685038294807722 ) ) ;
#23882 = CARTESIAN_POINT ( 'NONE',  ( 1.002407869896990045, -0.1264236179284866091, 1.316437007820252081 ) ) ;
#23883 = AXIS2_PLACEMENT_3D ( 'NONE', #24231, #1441, #9372 ) ;
#23884 = ADVANCED_FACE ( 'NONE', ( #37408 ), #19200, .T. ) ;
#23885 = CARTESIAN_POINT ( 'NONE',  ( 0.2698848154395015464, 4.466152701071653354E-17, 0.000000000000000000 ) ) ;
#23886 = CARTESIAN_POINT ( 'NONE',  ( 0.1264236179284866091, 0.09301181107738563936, 0.1264236179284866091 ) ) ;
#23887 = CARTESIAN_POINT ( 'NONE',  ( -0.7646288533564489232, -0.1113553986120547346, 1.008858267609007875 ) ) ;
#23888 = ( BOUNDED_CURVE ( )  B_SPLINE_CURVE ( 2, ( #21449, #2292, #24355, #20971, #38734, #17624, #35842, #38954, #36078 ),
 .UNSPECIFIED., .F., .T. ) 
 B_SPLINE_CURVE_WITH_KNOTS ( ( 3, 2, 2, 2, 3 ),
 ( 0.1199999999999999956, 0.1224999999999999978, 0.1250000000000000000, 0.1275000000000000022, 0.1300000000000000044 ),
 .UNSPECIFIED. ) 
 CURVE ( )  GEOMETRIC_REPRESENTATION_ITEM ( )  RATIONAL_B_SPLINE_CURVE ( ( 1.000000000000000000, 0.9238795325112869605, 1.000000000000000000, 0.9238795325112869605, 1.000000000000000000, 0.9238795325112869605, 1.000000000000000000, 0.9238795325112869605, 1.000000000000000000 ) ) 
 REPRESENTATION_ITEM ( '' )  ) ;
#23889 = AXIS2_PLACEMENT_3D ( 'NONE', #25932, #6995, #40513 ) ;
#23890 = CARTESIAN_POINT ( 'NONE',  ( -1.054774247047244096, 0.000000000000000000, 0.5339566928596221063 ) ) ;
#23891 = CARTESIAN_POINT ( 'NONE',  ( 0.7185039370078746268, 0.06523048226347956391, 0.2632874015748031260 ) ) ;
#23892 = FACE_OUTER_BOUND ( 'NONE', #36930, .T. ) ;
#23893 = ORIENTED_EDGE ( 'NONE', *, *, #19757, .F. ) ;
#23894 = CARTESIAN_POINT ( 'NONE',  ( 0.1377952755905511861, 0.1564960629921262614, 0.8070866141732283561 ) ) ;
#23895 = CARTESIAN_POINT ( 'NONE',  ( -0.1787899950787401604, -1.740157480261197875, -0.07405724077823318263 ) ) ;
#23896 = CARTESIAN_POINT ( 'NONE',  ( -0.7495606340400177148, 0.1264236179284866091, 0.9473425196312755814 ) ) ;
#23897 = CIRCLE ( 'NONE', #9358, 0.7972440944881888925 ) ;
#23898 = VECTOR ( 'NONE', #37011, 39.37007874015748143 ) ;
#23899 = CARTESIAN_POINT ( 'NONE',  ( -0.7495606340400177148, 0.1264236179284866091, 1.926673228292693052 ) ) ;
#23900 = CARTESIAN_POINT ( 'NONE',  ( -0.8019270111902717657, 0.1787899950787401604, 0.7480314960092282472 ) ) ;
#23901 = VERTEX_POINT ( 'NONE', #44129 ) ;
#23902 = DIRECTION ( 'NONE',  ( 0.000000000000000000, 0.000000000000000000, 1.000000000000000000 ) ) ;
#23903 = CARTESIAN_POINT ( 'NONE',  ( 0.1184675242425285574, -0.5708661417322835607, 1.224299699984021661 ) ) ;
#23904 = CARTESIAN_POINT ( 'NONE',  ( 0.1264236179284866091, -0.7496318422449862462, 0.1264236179284866091 ) ) ;
#23905 = VECTOR ( 'NONE', #11209, 39.37007874015748854 ) ;
#23906 = ORIENTED_EDGE ( 'NONE', *, *, #3583, .F. ) ;
#23907 = CARTESIAN_POINT ( 'NONE',  ( -0.1552293633745783497, -0.08956123932130295728, -0.08013377253620669605 ) ) ;
#23908 = CARTESIAN_POINT ( 'NONE',  ( 0.7185039370078746268, -0.06523048226347956391, 0.4650590551181104093 ) ) ;
#23909 = ORIENTED_EDGE ( 'NONE', *, *, #11434, .F. ) ;
#23910 = DIRECTION ( 'NONE',  ( 0.000000000000000000, 0.000000000000000000, 1.000000000000000000 ) ) ;
#23911 = DIRECTION ( 'NONE',  ( 1.822029033848725028E-16, 0.000000000000000000, 1.000000000000000000 ) ) ;
#23912 = ( BOUNDED_CURVE ( )  B_SPLINE_CURVE ( 2, ( #37124, #15335, #18669, #43837, #29987, #8124, #11038, #680, #14862 ),
 .UNSPECIFIED., .F., .T. ) 
 B_SPLINE_CURVE_WITH_KNOTS ( ( 3, 2, 2, 2, 3 ),
 ( 0.6899999999999999467, 0.6925000000000000044, 0.6949999999999999512, 0.6975000000000000089, 0.6999999999999999556 ),
 .UNSPECIFIED. ) 
 CURVE ( )  GEOMETRIC_REPRESENTATION_ITEM ( )  RATIONAL_B_SPLINE_CURVE ( ( 1.000000000000000000, 0.9238795325112899581, 1.000000000000000000, 0.9238795325112869605, 1.000000000000000000, 0.9238795325112869605, 1.000000000000000000, 0.9238795325112829637, 1.000000000000000000 ) ) 
 REPRESENTATION_ITEM ( '' )  ) ;
#23913 = CARTESIAN_POINT ( 'NONE',  ( -0.9500414927467378812, -0.1787899950787401604, 0.5265748030958428139 ) ) ;
#23914 = DIRECTION ( 'NONE',  ( 0.000000000000000000, 0.000000000000000000, 1.000000000000000000 ) ) ;
#23915 = ORIENTED_EDGE ( 'NONE', *, *, #16095, .F. ) ;
#23916 = CARTESIAN_POINT ( 'NONE',  ( -0.6971942568897637749, 2.189545951927499583E-17, 1.700295275536787498 ) ) ;
#23917 = CARTESIAN_POINT ( 'NONE',  ( -0.07405724077823318263, -1.454724409395055096, 0.1787899950787401604 ) ) ;
#23918 = CYLINDRICAL_SURFACE ( 'NONE', #1195, 0.4404574800679669777 ) ;
#23919 = CIRCLE ( 'NONE', #3240, 0.09940944881889707263 ) ;
#23920 = VERTEX_POINT ( 'NONE', #14682 ) ;
#23921 = CARTESIAN_POINT ( 'NONE',  ( -0.1797182628040039365, -0.7490595576145413492, 0.000000000000000000 ) ) ;
#23922 = CARTESIAN_POINT ( 'NONE',  ( 0.9412147342319837628, -0.1574803149606297803, 0.9473425196850396857 ) ) ;
#23923 = CARTESIAN_POINT ( 'NONE',  ( -0.8107537697050253289, 0.1574803149606300301, 1.272145669183810668 ) ) ;
#23924 = ADVANCED_FACE ( 'NONE', ( #11327 ), #25939, .T. ) ;
#23925 = CARTESIAN_POINT ( 'NONE',  ( 0.8019270111902717657, 0.1787899950787401604, 0.6299212597887560161 ) ) ;
#23927 = DIRECTION ( 'NONE',  ( 0.000000000000000000, 0.000000000000000000, 1.000000000000000000 ) ) ;
#23926 = CARTESIAN_POINT ( 'NONE',  ( -0.1574803149606300301, -0.5024606299212598381, -0.06523048226347956391 ) ) ;
#23928 = VECTOR ( 'NONE', #9136, 39.37007874015748143 ) ;
#23929 = CARTESIAN_POINT ( 'NONE',  ( 0.03901279071809810040, -0.09842519685039369248, 1.555605046820496273 ) ) ;
#23930 = VERTEX_POINT ( 'NONE', #22324 ) ;
#23931 = DIRECTION ( 'NONE',  ( 0.000000000000000000, 8.979745052115236376E-16, 1.000000000000000000 ) ) ;
#23932 = CARTESIAN_POINT ( 'NONE',  ( -0.9500414927467377701, -0.1787899950787401604, 1.122047244040725422 ) ) ;
#23933 = CARTESIAN_POINT ( 'NONE',  ( 0.8759842519685039353, -0.1574803149606299191, 1.023622047244094446 ) ) ;
#23934 = CARTESIAN_POINT ( 'NONE',  ( 0.1574803149606300301, 0.07824803160359000698, 0.06523048226347956391 ) ) ;
#23936 = DIRECTION ( 'NONE',  ( 0.000000000000000000, -1.000000000000000000, 0.000000000000000000 ) ) ;
#23935 = DIRECTION ( 'NONE',  ( 0.000000000000000000, 0.000000000000000000, -1.000000000000000000 ) ) ;
#23937 = DIRECTION ( 'NONE',  ( -1.000000000000000000, 0.000000000000000000, 0.000000000000000000 ) ) ;
#23938 = EDGE_CURVE ( 'NONE', #27624, #23076, #46891, .T. ) ;
#23939 = CARTESIAN_POINT ( 'NONE',  ( 0.4620708661417356478, 0.9842519685039370358, -0.7135826771653542844 ) ) ;
#23940 = DIRECTION ( 'NONE',  ( -1.000000000000000000, 0.000000000000000000, 0.000000000000000000 ) ) ;
#23941 = CARTESIAN_POINT ( 'NONE',  ( -0.1667349855531194136, -0.08956067304632099602, -0.04285543117372075245 ) ) ;
#23942 = CARTESIAN_POINT ( 'NONE',  ( 0.07405724077823318263, -0.6033464566391496531, -0.1787899950787401604 ) ) ;
#23943 = EDGE_LOOP ( 'NONE', ( #5482, #6552, #37032, #43318 ) ) ;
#23944 = AXIS2_PLACEMENT_3D ( 'NONE', #2670, #28339, #6741 ) ;
#23945 = CARTESIAN_POINT ( 'NONE',  ( -0.07874015748031489015, -0.5708661417322835607, 0.9783464566929127582 ) ) ;
#23946 = CARTESIAN_POINT ( 'NONE',  ( 1.054774247047244540, 0.07405724077823318263, 0.8120078739619844832 ) ) ;
#23947 = EDGE_LOOP ( 'NONE', ( #40757, #9341, #26605, #25361, #3422, #41546 ) ) ;
#23948 = ADVANCED_FACE ( 'NONE', ( #30273 ), #38361, .F. ) ;
#23949 = CARTESIAN_POINT ( 'NONE',  ( 0.7185039370078746268, -0.06523048226347956391, 1.449311023622047445 ) ) ;
#23950 = CARTESIAN_POINT ( 'NONE',  ( -0.8759842519685039353, 0.000000000000000000, 0.000000000000000000 ) ) ;
#23951 = CARTESIAN_POINT ( 'NONE',  ( -0.1264236179284866091, -1.767224409395055318, 0.1264236179284866091 ) ) ;
#23952 = CARTESIAN_POINT ( 'NONE',  ( 3.284318927891251994E-17, -1.097933070812378009, 0.1787899950787401882 ) ) ;
#23953 = CARTESIAN_POINT ( 'NONE',  ( -0.1113553986120547346, -1.400590551181102539, 0.1113553986120547346 ) ) ;
#23954 = CARTESIAN_POINT ( 'NONE',  ( 0.9873396505805591694, -0.1113553986120547346, 1.176181102254677313 ) ) ;
#23955 = PRODUCT_DEFINITION ( 'UNKNOWN', '', #5624, #3435 ) ;
#23956 = VERTEX_POINT ( 'NONE', #26660 ) ;
#23957 = ORIENTED_EDGE ( 'NONE', *, *, #5473, .T. ) ;
#23958 = CARTESIAN_POINT ( 'NONE',  ( -1.054774247047244096, 0.000000000000000000, 1.916830708607653477 ) ) ;
#23959 = CARTESIAN_POINT ( 'NONE',  ( 1.054774247047244540, -0.07405724077823318263, 1.835629921206078485 ) ) ;
#23960 = ORIENTED_EDGE ( 'NONE', *, *, #23654, .T. ) ;
#23961 = FACE_OUTER_BOUND ( 'NONE', #37989, .T. ) ;
#23962 = CARTESIAN_POINT ( 'NONE',  ( -1.002407869896990045, -0.1264236179284866091, 1.513287401521039355 ) ) ;
#23963 = DIRECTION ( 'NONE',  ( -1.000000000000000000, 0.000000000000000000, 0.000000000000000000 ) ) ;
#23964 = CARTESIAN_POINT ( 'NONE',  ( -1.002407869896990045, -0.1264236179284866091, 1.001476377898992132 ) ) ;
#23965 = CARTESIAN_POINT ( 'NONE',  ( -0.9500414927467378812, 0.1787899950787401604, 0.2312992125446618197 ) ) ;
#23966 = AXIS2_PLACEMENT_3D ( 'NONE', #31744, #31274, #21399 ) ;
#23967 = CARTESIAN_POINT ( 'NONE',  ( -0.4338976377952755703, 0.2460629921259842590, 0.000000000000000000 ) ) ;
#23968 = CARTESIAN_POINT ( 'NONE',  ( -0.6971942568897648851, 0.07405724077823318263, 1.776574803095843924 ) ) ;
#23969 = CARTESIAN_POINT ( 'NONE',  ( 0.8759842519685039353, -0.1574803149606299191, 1.407480314853102321 ) ) ;
#23970 = CARTESIAN_POINT ( 'NONE',  ( -0.7646288533564489232, -0.1113553986120547346, 1.806102362204724532 ) ) ;
#23971 = LINE ( 'NONE', #34061, #5242 ) ;
#23972 = CARTESIAN_POINT ( 'NONE',  ( -0.1787899950787401882, -0.2132145194103413355, 0.000000000000000000 ) ) ;
#23973 = CARTESIAN_POINT ( 'NONE',  ( 0.6971942568897637749, 2.189545951927499583E-17, 1.700295275536787498 ) ) ;
#23974 = CARTESIAN_POINT ( 'NONE',  ( 0.1312289434299238056, -0.09842519685039231858, -0.1483208907156891854 ) ) ;
#23975 = CARTESIAN_POINT ( 'NONE',  ( -0.7185039370078739607, 1.928577636452523993E-17, 1.486220472440944906 ) ) ;
#23976 = VECTOR ( 'NONE', #4385, 39.37007874015748143 ) ;
#23977 = ORIENTED_EDGE ( 'NONE', *, *, #27598, .F. ) ;
#23978 = CIRCLE ( 'NONE', #23944, 0.1377952755905513804 ) ;
#23979 = CARTESIAN_POINT ( 'NONE',  ( -1.054774247047244540, 0.07405724077823318263, 1.289370078686393750 ) ) ;
#23980 = VERTEX_POINT ( 'NONE', #27617 ) ;
#23981 = EDGE_CURVE ( 'NONE', #33937, #30045, #45057, .T. ) ;
#23982 = CARTESIAN_POINT ( 'NONE',  ( 0.1264236179284866091, -1.093011810969858333, 0.1264236179284866091 ) ) ;
#23983 = CARTESIAN_POINT ( 'NONE',  ( 0.1264236179284866091, -1.245570866087968520, 0.1264236179284866091 ) ) ;
#23984 = CARTESIAN_POINT ( 'NONE',  ( -0.7646288533564489232, 0.1113553986120547346, 1.284448818897637956 ) ) ;
#23985 = ( NAMED_UNIT ( * ) SI_UNIT ( $, .STERADIAN. ) SOLID_ANGLE_UNIT ( ) ) ;
#23986 = CARTESIAN_POINT ( 'NONE',  ( 1.054774247047244540, -0.07405724077823318263, 0.4133858267178901480 ) ) ;
#23987 = CARTESIAN_POINT ( 'NONE',  ( -0.07444174185955065859, -0.4267170379295021632, 0.1797182628040039087 ) ) ;
#23988 = DIRECTION ( 'NONE',  ( 0.000000000000000000, -0.7880107536067207930, 0.6156614753256598460 ) ) ;
#23989 = CARTESIAN_POINT ( 'NONE',  ( -0.9873396505805591694, 0.1113553986120547346, 0.7923228345381417848 ) ) ;
#23990 = ADVANCED_FACE ( 'NONE', ( #33859 ), #42279, .F. ) ;
#23991 = CARTESIAN_POINT ( 'NONE',  ( 0.1113553986120547346, 0.02657480314960630058, 0.1113553986120547346 ) ) ;
#23992 = VECTOR ( 'NONE', #29031, 39.37007874015748143 ) ;
#23993 = CARTESIAN_POINT ( 'NONE',  ( 1.054774247047244540, 0.07405724077823318263, 0.8907480314422986378 ) ) ;
#23995 = CARTESIAN_POINT ( 'NONE',  ( 0.1582007246420326085, -0.03721045995875271739, 0.1404371117717379547 ) ) ;
#23994 = CARTESIAN_POINT ( 'NONE',  ( 0.09016091299416212346, 0.2434398048748445675, -0.03531881253560968659 ) ) ;
#23996 = CARTESIAN_POINT ( 'NONE',  ( 0.8107537697050253289, 0.1574803149606300301, 0.09104330697908720460 ) ) ;
#23997 = CARTESIAN_POINT ( 'NONE',  ( 0.7495606340400177148, -0.1264236179284866091, 0.7209645668753701386 ) ) ;
#23998 = DIRECTION ( 'NONE',  ( 0.000000000000000000, 0.000000000000000000, 1.000000000000000000 ) ) ;
#23999 = CARTESIAN_POINT ( 'NONE',  ( -0.1264236179284866091, -0.3548228345919058890, 0.1264236179284866091 ) ) ;
#24000 = CARTESIAN_POINT ( 'NONE',  ( 2.892866454678787531E-17, 0.02165354330708661734, 0.1574803149606299191 ) ) ;
#24001 = CARTESIAN_POINT ( 'NONE',  ( 0.07405724077823318263, -1.351377952702143004, -0.1787899950787401604 ) ) ;
#24002 = CARTESIAN_POINT ( 'NONE',  ( 0.7185039370078739607, 1.928577636452523993E-17, 0.4232283464566928832 ) ) ;
#24003 = CARTESIAN_POINT ( 'NONE',  ( -1.054774247047244096, 0.000000000000000000, 1.833169291284818758 ) ) ;
#24004 = VERTEX_POINT ( 'NONE', #24000 ) ;
#24005 = CARTESIAN_POINT ( 'NONE',  ( -1.054774247047244096, 0.000000000000000000, 1.405019684985606476 ) ) ;
#24006 = DIRECTION ( 'NONE',  ( -3.494233027178502331E-15, -1.000000000000000000, -0.000000000000000000 ) ) ;
#24007 = CARTESIAN_POINT ( 'NONE',  ( -0.8019270111902717657, 0.1787899950787401604, 0.7086614172690703928 ) ) ;
#24008 = CARTESIAN_POINT ( 'NONE',  ( -1.002407869896990045, -0.1264236179284866091, 1.277066929080094448 ) ) ;
#24009 = LINE ( 'NONE', #31913, #17456 ) ;
#24010 = CARTESIAN_POINT ( 'NONE',  ( 0.7495606340400177148, -0.1264236179284866091, 0.6422244093950550958 ) ) ;
#24011 = CARTESIAN_POINT ( 'NONE',  ( -0.8019270111902716547, 0.1787899950787401604, 0.4675196849856070314 ) ) ;
#24012 = DIRECTION ( 'NONE',  ( -0.8191520442889873577, 1.003171929053519323E-16, 0.5735764363510523767 ) ) ;
#24013 = CARTESIAN_POINT ( 'NONE',  ( 2.892866454678787531E-17, -0.09645669291338582196, 0.1574803149606299191 ) ) ;
#24014 = ORIENTED_EDGE ( 'NONE', *, *, #17469, .F. ) ;
#24015 = ORIENTED_EDGE ( 'NONE', *, *, #7160, .F. ) ;
#24016 = CARTESIAN_POINT ( 'NONE',  ( -0.8759842519685039353, -0.1574803149606299191, 0.2362204724409449064 ) ) ;
#24017 = CARTESIAN_POINT ( 'NONE',  ( 0.8759842519685039353, 0.1787899950787401882, 1.257381889710015743 ) ) ;
#24018 = CARTESIAN_POINT ( 'NONE',  ( -0.1749793193338634034, -0.09851385152415884083, 0.1545203862959413366 ) ) ;
#24019 = CARTESIAN_POINT ( 'NONE',  ( -0.8107537697050254399, -0.1574803149606297803, 1.838090551073574774 ) ) ;
#24020 = ORIENTED_EDGE ( 'NONE', *, *, #33595, .F. ) ;
#24021 = CARTESIAN_POINT ( 'NONE',  ( 0.1377952755905511861, 0.000000000000000000, -0.1321438491773566926 ) ) ;
#24022 = CARTESIAN_POINT ( 'NONE',  ( -1.054774247047244540, 0.07405724077823318263, 1.013779527505291878 ) ) ;
#24023 = ( BOUNDED_CURVE ( )  B_SPLINE_CURVE ( 2, ( #45211, #1851, #31120, #45683, #44970, #16025, #27052, #12183, #26808 ),
 .UNSPECIFIED., .F., .T. ) 
 B_SPLINE_CURVE_WITH_KNOTS ( ( 3, 2, 2, 2, 3 ),
 ( 0.1900000000000000022, 0.1925000000000000044, 0.1950000000000000067, 0.1975000000000000089, 0.2000000000000000111 ),
 .UNSPECIFIED. ) 
 CURVE ( )  GEOMETRIC_REPRESENTATION_ITEM ( )  RATIONAL_B_SPLINE_CURVE ( ( 1.000000000000000000, 0.9238795325112869605, 1.000000000000000000, 0.9238795325112869605, 1.000000000000000000, 0.9238795325112869605, 1.000000000000000000, 0.9238795325112869605, 1.000000000000000000 ) ) 
 REPRESENTATION_ITEM ( '' )  ) ;
#24024 = CARTESIAN_POINT ( 'NONE',  ( 0.1787899950787401604, -1.613312944607189880, 0.07405724077823318263 ) ) ;
#24025 = ORIENTED_EDGE ( 'NONE', *, *, #45544, .T. ) ;
#24026 = DIRECTION ( 'NONE',  ( 0.000000000000000000, 0.000000000000000000, 1.000000000000000000 ) ) ;
#24027 = CARTESIAN_POINT ( 'NONE',  ( 0.1787899950787401882, -0.6500984251430865779, -2.189545951927503898E-17 ) ) ;
#24028 = CARTESIAN_POINT ( 'NONE',  ( -0.3052312982475723357, -0.05465342266228453288, 1.034226492048918145 ) ) ;
#24029 = EDGE_LOOP ( 'NONE', ( #15906, #46045, #44645, #12588 ) ) ;
#24030 = CARTESIAN_POINT ( 'NONE',  ( 0.8019270111902717657, -0.1787899950787401604, 1.466535433017102763 ) ) ;
#24031 = VECTOR ( 'NONE', #15087, 39.37007874015748143 ) ;
#24032 = EDGE_CURVE ( 'NONE', #17766, #28233, #34792, .T. ) ;
#24033 = CARTESIAN_POINT ( 'NONE',  ( -0.09005431032995797613, 0.2435012976196485601, -0.3128573757126095756 ) ) ;
#24034 = CARTESIAN_POINT ( 'NONE',  ( -0.07405724077823318263, -0.3671259841982050798, -0.1787899950787401604 ) ) ;
#24035 = EDGE_CURVE ( 'NONE', #15682, #13443, #953, .T. ) ;
#24036 = CARTESIAN_POINT ( 'NONE',  ( -0.1264236179284866091, -0.7436023621509606496, 0.1264236179284866091 ) ) ;
#24037 = CARTESIAN_POINT ( 'NONE',  ( 1.033464566929133799, 0.000000000000000000, 1.860236220472440971 ) ) ;
#24038 = CARTESIAN_POINT ( 'NONE',  ( 0.6195511811023612925, 0.6102362204724401940, 1.186023622047243986 ) ) ;
#24039 = CARTESIAN_POINT ( 'NONE',  ( 1.054774247047244540, 0.07405724077823318263, 1.560039370024977057 ) ) ;
#24040 = EDGE_CURVE ( 'NONE', #740, #3655, #34088, .T. ) ;
#24041 = CARTESIAN_POINT ( 'NONE',  ( 0.07405724077823318263, 0.08944296090461954785, -0.1787899950787401604 ) ) ;
#24042 = CARTESIAN_POINT ( 'NONE',  ( -0.1264236179284866091, 0.1176181102899840625, 0.1264236179284866091 ) ) ;
#24043 = CARTESIAN_POINT ( 'NONE',  ( -0.6971942568897643300, 0.000000000000000000, 1.995570866087968520 ) ) ;
#24044 = EDGE_CURVE ( 'NONE', #18563, #12246, #27142, .T. ) ;
#24045 = CARTESIAN_POINT ( 'NONE',  ( 0.8759842519685039353, -0.1787899950787401882, 0.4453740156942677664 ) ) ;
#24046 = DIMENSIONAL_EXPONENTS ( 1.000000000000000000, 0.000000000000000000, 0.000000000000000000, 0.000000000000000000, 0.000000000000000000, 0.000000000000000000, 0.000000000000000000 ) ;
#24047 = CARTESIAN_POINT ( 'NONE',  ( -0.6971942568897637749, 2.189545951927499583E-17, 0.8341535432533228045 ) ) ;
#24049 = LINE ( 'NONE', #46060, #44606 ) ;
#24048 = CARTESIAN_POINT ( 'NONE',  ( -0.06523048226347956391, -0.9010826771653551726, -0.1574803149606300301 ) ) ;
#24050 = CARTESIAN_POINT ( 'NONE',  ( 0.07444174185955046430, -1.548764282023991301, -0.1797182628040039087 ) ) ;
#24051 = CARTESIAN_POINT ( 'NONE',  ( 2.892866454678787531E-17, -0.4409448817822370081, 0.1574803149606299191 ) ) ;
#24052 = CARTESIAN_POINT ( 'NONE',  ( -0.8107537697050254399, 0.1574803149606300301, 1.035925196742866650 ) ) ;
#24053 = CARTESIAN_POINT ( 'NONE',  ( 1.054774247047244540, 0.07405724077823318263, 1.486220472387181690 ) ) ;
#24054 = CARTESIAN_POINT ( 'NONE',  ( 0.1574803149606299191, 0.000000000000000000, -0.3149606299212598381 ) ) ;
#24055 = CARTESIAN_POINT ( 'NONE',  ( 0.6971942568897626646, -0.07405724077823297447, 0.3198818897100159098 ) ) ;
#24057 = ORIENTED_EDGE ( 'NONE', *, *, #18300, .F. ) ;
#24056 = CARTESIAN_POINT ( 'NONE',  ( 0.2519685039370078705, 4.616380251121755931E-17, 0.000000000000000000 ) ) ;
#24058 = CARTESIAN_POINT ( 'NONE',  ( 0.1733357866104492107, 0.3740157480314960647, 1.025733466389925352 ) ) ;
#24059 = CARTESIAN_POINT ( 'NONE',  ( 0.2055371055873737307, -0.1768241869785752152, -0.3061783854716485509 ) ) ;
#24060 = CARTESIAN_POINT ( 'NONE',  ( 0.07405724077823318263, -0.01771653537930735489, -0.1787899950787401604 ) ) ;
#24061 = CARTESIAN_POINT ( 'NONE',  ( 0.6971942568897637749, 2.189545951927499583E-17, 0.4355314960092284138 ) ) ;
#24062 = CARTESIAN_POINT ( 'NONE',  ( -0.07405724077823318263, -0.8986220471903317852, 0.1787899950787401604 ) ) ;
#24063 = CARTESIAN_POINT ( 'NONE',  ( 0.8759842491179902213, 0.1574803149606299191, 1.978346456692913646 ) ) ;
#24064 = CARTESIAN_POINT ( 'NONE',  ( -0.6971942568897648851, 0.07405724077823318263, 1.377952755851748146 ) ) ;
#24065 = CARTESIAN_POINT ( 'NONE',  ( 0.7646288533564489232, 0.1113553986120547346, 0.7627952754830236159 ) ) ;
#24066 = EDGE_LOOP ( 'NONE', ( #21408, #28828, #42254, #40700, #27533 ) ) ;
#24067 = DIRECTION ( 'NONE',  ( 0.000000000000000000, -0.9699617890481188054, -0.2432573283306645462 ) ) ;
#24068 = CARTESIAN_POINT ( 'NONE',  ( 0.8019270111902717657, -0.1787899950787401604, 0.9990157479777320715 ) ) ;
#24069 = ORIENTED_EDGE ( 'NONE', *, *, #4187, .F. ) ;
#24071 = CARTESIAN_POINT ( 'NONE',  ( 0.1264236179284866091, -1.319389763725763665, -0.1264236179284866091 ) ) ;
#24070 = CARTESIAN_POINT ( 'NONE',  ( -0.1574803149606299191, -1.080708661309795371, 0.000000000000000000 ) ) ;
#24072 = CARTESIAN_POINT ( 'NONE',  ( -1.033464566929134687, -0.06523048226347956391, 0.5093503935932609528 ) ) ;
#24073 = CARTESIAN_POINT ( 'NONE',  ( 0.4934383202099732468, 4.616380251121755931E-17, 0.000000000000000000 ) ) ;
#24074 = CARTESIAN_POINT ( 'NONE',  ( 0.9500414927467378812, 0.1787899950787401604, 1.683070866087970074 ) ) ;
#24075 = CARTESIAN_POINT ( 'NONE',  ( -0.8759842519685039353, 0.1574803149606299191, 1.437007874015747921 ) ) ;
#24076 = CARTESIAN_POINT ( 'NONE',  ( 0.8759842519685039353, -0.1574803149606299191, 1.801181102254677091 ) ) ;
#24078 = CARTESIAN_POINT ( 'NONE',  ( -2.458663194297838277E-15, -0.2954942322624074524, -0.1122047244094488277 ) ) ;
#24077 = CARTESIAN_POINT ( 'NONE',  ( -0.8759842519685039353, 0.1574803149606299191, 0.7283464566929134243 ) ) ;
#24079 = CARTESIAN_POINT ( 'NONE',  ( 0.6971942568897637749, 2.189545951927499583E-17, 0.1254921259304885850 ) ) ;
#24080 = CARTESIAN_POINT ( 'NONE',  ( -0.6971942568897637749, 2.189545951927499583E-17, 0.1205708660879689087 ) ) ;
#24081 = CARTESIAN_POINT ( 'NONE',  ( 1.033464566929133799, 0.000000000000000000, 1.417322834538141674 ) ) ;
#24082 = EDGE_LOOP ( 'NONE', ( #30690, #26509, #13748, #47356, #34429, #25572, #24393, #35162 ) ) ;
#24083 = EDGE_LOOP ( 'NONE', ( #30172, #2254, #29704, #35641 ) ) ;
#24084 = CARTESIAN_POINT ( 'NONE',  ( 0.1515708385138894443, 0.1286422661082891605, 0.1012763973430838016 ) ) ;
#24085 = VECTOR ( 'NONE', #28530, 39.37007874015748854 ) ;
#24086 = CARTESIAN_POINT ( 'NONE',  ( -0.6971942568897637749, 2.189545951927499583E-17, 1.734744094434425232 ) ) ;
#24087 = CARTESIAN_POINT ( 'NONE',  ( -0.1377952755905509363, 1.687505431895957030E-17, -0.1436967020037460685 ) ) ;
#24088 = PLANE ( 'NONE',  #22608 ) ;
#24089 = CARTESIAN_POINT ( 'NONE',  ( 1.614954907737318939E-16, 0.1574803149606340824, 0.3937007874015748254 ) ) ;
#24090 = CARTESIAN_POINT ( 'NONE',  ( -0.1264236179284866091, -1.123647590276482200, -0.1264236179284866091 ) ) ;
#24091 = VERTEX_POINT ( 'NONE', #8413 ) ;
#24092 = CARTESIAN_POINT ( 'NONE',  ( -0.1787899950787401604, -0.08169291333206318839, -0.07405724077823318263 ) ) ;
#24093 = ORIENTED_EDGE ( 'NONE', *, *, #15546, .T. ) ;
#24094 = ORIENTED_EDGE ( 'NONE', *, *, #34878, .F. ) ;
#24095 = CARTESIAN_POINT ( 'NONE',  ( -0.2559049524053137459, -0.08043145352417861715, -0.3078373565276721902 ) ) ;
#24096 = CARTESIAN_POINT ( 'NONE',  ( -1.033464566929133799, 0.000000000000000000, 0.4330708660342047489 ) ) ;
#24097 = ADVANCED_FACE ( 'NONE', ( #30963 ), #978, .T. ) ;
#24098 = CARTESIAN_POINT ( 'NONE',  ( 0.9412147342319837628, -0.1574803149606297803, 1.852854330708662012 ) ) ;
#24099 = VECTOR ( 'NONE', #29536, 39.37007874015748143 ) ;
#24100 = AXIS2_PLACEMENT_3D ( 'NONE', #41086, #19309, #26295 ) ;
#24101 = AXIS2_PLACEMENT_3D ( 'NONE', #3586, #6459, #25412 ) ;
#24102 = CARTESIAN_POINT ( 'NONE',  ( 3.284318927891251994E-17, -0.6254921259304881964, 0.1787899950787401882 ) ) ;
#24103 = ADVANCED_FACE ( 'NONE', ( #27383 ), #15635, .F. ) ;
#24104 = CARTESIAN_POINT ( 'NONE',  ( -1.002407869896990045, 0.1264236179284866091, 0.3863188975840318173 ) ) ;
#24105 = CARTESIAN_POINT ( 'NONE',  ( -0.8107537697050253289, -0.1574803149606297803, 0.9817913385826764205 ) ) ;
#24106 = CARTESIAN_POINT ( 'NONE',  ( 0.1797182628040039087, -1.125535935567297807, 0.07444174185955046430 ) ) ;
#24107 = CYLINDRICAL_SURFACE ( 'NONE', #20249, 0.1377952755905511306 ) ;
#24108 = CARTESIAN_POINT ( 'NONE',  ( 0.8759842519685039353, -0.1787899950787401882, 1.119586614119464585 ) ) ;
#24109 = CARTESIAN_POINT ( 'NONE',  ( 0.6971942568897637749, 2.189545951927499583E-17, 1.419783464513165505 ) ) ;
#24110 = CARTESIAN_POINT ( 'NONE',  ( 0.6971942568897626646, -0.07405724077823297447, 0.1624015747493861017 ) ) ;
#24111 = CARTESIAN_POINT ( 'NONE',  ( 0.1184675242425285574, 0.3740157480314960647, 1.224299699984021661 ) ) ;
#24112 = CARTESIAN_POINT ( 'NONE',  ( 0.7185039370078739607, 1.928577636452523993E-17, 1.604330708661417360 ) ) ;
#24114 = CARTESIAN_POINT ( 'NONE',  ( 0.1574803149606300023, 0.7443365962042343131, -3.523993443072799270 ) ) ;
#24113 = CARTESIAN_POINT ( 'NONE',  ( 0.7185039370078746268, -0.06523048226347956391, 1.409940944881891367 ) ) ;
#24115 = CARTESIAN_POINT ( 'NONE',  ( -0.1026092249587055166, 0.1299212598425196763, 0.1321676130798911386 ) ) ;
#24116 = CARTESIAN_POINT ( 'NONE',  ( -1.033464566929133799, 1.928577636452524610E-17, 2.869337061179095023E-17 ) ) ;
#24117 = CARTESIAN_POINT ( 'NONE',  ( -1.094772975963752103E-17, 0.1077755906049446960, -0.1787899950787401882 ) ) ;
#24118 = CARTESIAN_POINT ( 'NONE',  ( 0.1476377952755906220, 2.117069812090769609, -1.766975050165344951 ) ) ;
#24119 = CARTESIAN_POINT ( 'NONE',  ( 1.002407869896990045, -0.1264236179284866091, 0.9227362204186770889 ) ) ;
#24120 = CARTESIAN_POINT ( 'NONE',  ( 0.8019270111902716547, 0.1787899950787401604, 1.968503936954110412 ) ) ;
#24121 = CARTESIAN_POINT ( 'NONE',  ( 0.9412147342319837628, -0.1574803149606297803, 0.3863188975302684902 ) ) ;
#24122 = ORIENTED_EDGE ( 'NONE', *, *, #37129, .F. ) ;
#24123 = CARTESIAN_POINT ( 'NONE',  ( 1.054774247047244096, 0.000000000000000000, 1.995570866087968520 ) ) ;
#24124 = CARTESIAN_POINT ( 'NONE',  ( 0.06523048226347956391, -1.722933070758614349, -0.1574803149606300301 ) ) ;
#24125 = ORIENTED_EDGE ( 'NONE', *, *, #29501, .F. ) ;
#24126 = CARTESIAN_POINT ( 'NONE',  ( -0.8759842519685039353, 0.1574803149606299191, 0.3248031494987720369 ) ) ;
#24127 = DIRECTION ( 'NONE',  ( 0.000000000000000000, 0.000000000000000000, 1.000000000000000000 ) ) ;
#24128 = CARTESIAN_POINT ( 'NONE',  ( 0.8759842519685039353, -0.1787899950787401882, 1.350885826717889815 ) ) ;
#24129 = CIRCLE ( 'NONE', #9592, 0.1787899950787401049 ) ;
#24131 = CARTESIAN_POINT ( 'NONE',  ( 1.033464566929134687, -0.06523048226347956391, 0.07627952745152805081 ) ) ;
#24130 = CARTESIAN_POINT ( 'NONE',  ( -0.5314960629921260393, 0.000000000000000000, 4.842519685039370358 ) ) ;
#24132 = CARTESIAN_POINT ( 'NONE',  ( -0.1787899950787401882, 0.1569881890301415284, 0.000000000000000000 ) ) ;
#24133 = EDGE_CURVE ( 'NONE', #30017, #26580, #9379, .T. ) ;
#24134 = CARTESIAN_POINT ( 'NONE',  ( 0.1574803149606300023, 0.5323553679591566112, -0.7566348232351033376 ) ) ;
#24135 = CARTESIAN_POINT ( 'NONE',  ( -0.9500414927467378812, 0.1787899950787401604, 0.5413385826234012876 ) ) ;
#24136 = CIRCLE ( 'NONE', #30278, 0.4724409448818896462 ) ;
#24137 = CARTESIAN_POINT ( 'NONE',  ( -0.2066929133858267931, -0.2714884749021747590, -1.284167712019358198 ) ) ;
#24138 = CARTESIAN_POINT ( 'NONE',  ( -0.08837071341806060354, 0.09266989036297286486, 0.2344122156857451345 ) ) ;
#24139 = EDGE_LOOP ( 'NONE', ( #9338, #31343 ) ) ;
#24140 = CARTESIAN_POINT ( 'NONE',  ( -1.054774247047244540, 0.07405724077823318263, 1.402559055064346749 ) ) ;
#24141 = CARTESIAN_POINT ( 'NONE',  ( -0.1787899950787401604, -1.695866141678520567, 0.07405724077823318263 ) ) ;
#24142 = CARTESIAN_POINT ( 'NONE',  ( -0.7495606340400177148, -0.1264236179284866091, 0.9965551180564724554 ) ) ;
#24143 = AXIS2_PLACEMENT_3D ( 'NONE', #11964, #37574, #4734 ) ;
#24144 = CARTESIAN_POINT ( 'NONE',  ( -0.7495606340400177148, 0.1264236179284866091, 1.966043307032850462 ) ) ;
#24145 = ORIENTED_EDGE ( 'NONE', *, *, #23236, .F. ) ;
#24146 = CARTESIAN_POINT ( 'NONE',  ( -0.7495606340400177148, 0.1264236179284866091, 0.6717519684501732646 ) ) ;
#24147 = CARTESIAN_POINT ( 'NONE',  ( -0.1476377952755905387, 1.117014023967196179, -3.442880580079819008 ) ) ;
#24148 = CARTESIAN_POINT ( 'NONE',  ( 0.1533123297493048931, 0.1250557930784849670, -0.05373872839130795082 ) ) ;
#24149 = CARTESIAN_POINT ( 'NONE',  ( -0.8070866141732283561, -0.3937007874015746034, 0.6590551181102368705 ) ) ;
#24150 = VERTEX_POINT ( 'NONE', #41449 ) ;
#24151 = CARTESIAN_POINT ( 'NONE',  ( -0.06782836439666850570, -0.08956100471190649170, -0.1695658838066383955 ) ) ;
#24152 = LINE ( 'NONE', #31814, #44747 ) ;
#24153 = EDGE_LOOP ( 'NONE', ( #44097, #43619, #30292, #45556 ) ) ;
#24154 = FACE_OUTER_BOUND ( 'NONE', #4331, .T. ) ;
#24155 = CARTESIAN_POINT ( 'NONE',  ( -0.8019270111902717657, 0.1787899950787401604, 0.6249999999462366729 ) ) ;
#24156 = DIRECTION ( 'NONE',  ( -5.411399086424348811E-15, -1.000000000000000000, 0.000000000000000000 ) ) ;
#24157 = EDGE_CURVE ( 'NONE', #39441, #34250, #45274, .T. ) ;
#24158 = ORIENTED_EDGE ( 'NONE', *, *, #24044, .T. ) ;
#24159 = CARTESIAN_POINT ( 'NONE',  ( -1.054774247047244540, 0.07405724077823318263, 1.722440944828126153 ) ) ;
#24160 = EDGE_CURVE ( 'NONE', #20228, #35982, #8896, .T. ) ;
#24161 = CARTESIAN_POINT ( 'NONE',  ( -0.8759842519685039353, -0.1574803149606299191, 0.1870078739082208508 ) ) ;
#24162 = DIRECTION ( 'NONE',  ( 0.000000000000000000, 0.000000000000000000, 1.000000000000000000 ) ) ;
#24164 = CARTESIAN_POINT ( 'NONE',  ( 0.1797182628040039087, -0.7662839670633605493, -0.07444174185955065859 ) ) ;
#24163 = VECTOR ( 'NONE', #10955, 39.37007874015748143 ) ;
#24165 = CARTESIAN_POINT ( 'NONE',  ( -0.8759842519685039353, 0.1574803149606299191, 0.9645669291338583307 ) ) ;
#24166 = CARTESIAN_POINT ( 'NONE',  ( -1.033464566929134687, -0.06523048226347956391, 1.257381889656253193 ) ) ;
#24168 = LINE ( 'NONE', #7516, #8640 ) ;
#24167 = CARTESIAN_POINT ( 'NONE',  ( 0.1574803149606300301, -0.4040354330708660902, 0.06523048226347956391 ) ) ;
#24169 = AXIS2_PLACEMENT_3D ( 'NONE', #24497, #34581, #16144 ) ;
#24170 = AXIS2_PLACEMENT_3D ( 'NONE', #4968, #29721, #44496 ) ;
#24171 = FACE_OUTER_BOUND ( 'NONE', #11184, .T. ) ;
#24172 = CARTESIAN_POINT ( 'NONE',  ( 0.2759478392031499694, 0.000000000000000000, -1.945618984458255724E-15 ) ) ;
#24173 = CARTESIAN_POINT ( 'NONE',  ( 0.7185039370078739607, 1.928577636452523993E-17, 1.092519685039370136 ) ) ;
#24175 = FACE_OUTER_BOUND ( 'NONE', #14369, .T. ) ;
#24174 = FACE_OUTER_BOUND ( 'NONE', #8149, .T. ) ;
#24176 = DIRECTION ( 'NONE',  ( 0.000000000000000000, 0.000000000000000000, -1.000000000000000000 ) ) ;
#24177 = ( BOUNDED_CURVE ( )  B_SPLINE_CURVE ( 2, ( #46321, #20916, #31962, #35555, #46547, #13730, #25231, #39819, #7008 ),
 .UNSPECIFIED., .F., .T. ) 
 B_SPLINE_CURVE_WITH_KNOTS ( ( 3, 2, 2, 2, 3 ),
 ( 0.7500000000000000000, 0.7524999999999999467, 0.7550000000000000044, 0.7574999999999999512, 0.7600000000000000089 ),
 .UNSPECIFIED. ) 
 CURVE ( )  GEOMETRIC_REPRESENTATION_ITEM ( )  RATIONAL_B_SPLINE_CURVE ( ( 1.000000000000000000, 0.9238795325112899581, 1.000000000000000000, 0.9238795325112869605, 1.000000000000000000, 0.9238795325112869605, 1.000000000000000000, 0.9238795325112869605, 1.000000000000000000 ) ) 
 REPRESENTATION_ITEM ( '' )  ) ;
#24179 = CARTESIAN_POINT ( 'NONE',  ( 0.000000000000000000, -0.09842519685039370636, 0.000000000000000000 ) ) ;
#24178 = CARTESIAN_POINT ( 'NONE',  ( 0.1574803149606299746, 0.000000000000000000, 0.000000000000000000 ) ) ;
#24180 = DIRECTION ( 'NONE',  ( -0.5735764363510409414, -0.6455006197386570221, 0.5043203561029929727 ) ) ;
#24181 = CARTESIAN_POINT ( 'NONE',  ( 0.1787899950787401882, -0.4926181101824567143, -2.189545951927503898E-17 ) ) ;
#24182 = ORIENTED_EDGE ( 'NONE', *, *, #34682, .F. ) ;
#24183 = CARTESIAN_POINT ( 'NONE',  ( -0.7185039370078746268, -0.06523048226347956391, 1.055610236220473341 ) ) ;
#24184 = DIRECTION ( 'NONE',  ( -1.000000000000000000, 0.000000000000000000, 0.000000000000000000 ) ) ;
#24185 = CARTESIAN_POINT ( 'NONE',  ( 1.002407869896990045, 0.1264236179284866091, 0.8538385826234016207 ) ) ;
#24186 = DIRECTION ( 'NONE',  ( 0.000000000000000000, 1.000000000000000000, 0.000000000000000000 ) ) ;
#24187 = CARTESIAN_POINT ( 'NONE',  ( -0.8759842519685039353, 0.1574803149606299191, 0.5314960629921260393 ) ) ;
#24188 = CARTESIAN_POINT ( 'NONE',  ( 0.1797182628040039087, 0.1343065841177418784, 0.07444174185955046430 ) ) ;
#24189 = CARTESIAN_POINT ( 'NONE',  ( 0.1787899950787401604, -1.129921259788756682, 0.07405724077823318263 ) ) ;
#24190 = CARTESIAN_POINT ( 'NONE',  ( 0.1574803149606299191, -1.346456692913385877, -1.928577636452523993E-17 ) ) ;
#24191 = CARTESIAN_POINT ( 'NONE',  ( -0.8107537697050254399, 0.1574803149606300301, 1.400098425196850904 ) ) ;
#24192 = VERTEX_POINT ( 'NONE', #16107 ) ;
#24193 = CARTESIAN_POINT ( 'NONE',  ( -0.6971942568897637749, 2.189545951927499583E-17, 1.975885826717889815 ) ) ;
#24194 = CARTESIAN_POINT ( 'NONE',  ( 1.002407869896990045, 0.1264236179284866091, 1.882381889710015743 ) ) ;
#24195 = ORIENTED_EDGE ( 'NONE', *, *, #13686, .T. ) ;
#24196 = DIRECTION ( 'NONE',  ( -1.000000000000000000, 0.000000000000000000, 0.000000000000000000 ) ) ;
#24197 = CARTESIAN_POINT ( 'NONE',  ( -0.8019270111902717657, -0.1787899950787401604, 1.505905511757261284 ) ) ;
#24198 = AXIS2_PLACEMENT_3D ( 'NONE', #163, #3298, #24879 ) ;
#24199 = FACE_OUTER_BOUND ( 'NONE', #41603, .T. ) ;
#24200 = CARTESIAN_POINT ( 'NONE',  ( -0.6971942568897626646, -0.07405724077823297447, 0.2460629920722207375 ) ) ;
#24201 = ( BOUNDED_CURVE ( )  B_SPLINE_CURVE ( 2, ( #24646, #28029, #32329, #10026, #24187, #28500, #20801, #42370, #2120 ),
 .UNSPECIFIED., .F., .F. ) 
 B_SPLINE_CURVE_WITH_KNOTS ( ( 3, 2, 2, 2, 3 ),
 ( 0.2600000000000000089, 0.2625000000000000111, 0.2650000000000000133, 0.2675000000000000155, 0.2700000000000000178 ),
 .UNSPECIFIED. ) 
 CURVE ( )  GEOMETRIC_REPRESENTATION_ITEM ( )  RATIONAL_B_SPLINE_CURVE ( ( 1.000000000000000000, 0.9238795325112869605, 1.000000000000000000, 0.9238795325112869605, 1.000000000000000000, 0.9238795325112869605, 1.000000000000000000, 0.9238795325112869605, 1.000000000000000000 ) ) 
 REPRESENTATION_ITEM ( '' )  ) ;
#24202 = CARTESIAN_POINT ( 'NONE',  ( -0.9873396505805591694, 0.1113553986120547346, 0.5659448818897637734 ) ) ;
#24203 = CARTESIAN_POINT ( 'NONE',  ( -0.8759842519685039353, 0.1787899950787401882, 1.926673228292693052 ) ) ;
#24204 = CARTESIAN_POINT ( 'NONE',  ( 0.05554372828378647403, -0.07731288306167657942, -0.2533648624690311157 ) ) ;
#24205 = CARTESIAN_POINT ( 'NONE',  ( -0.8107537697050253289, -0.1574803149606297803, 1.808562992125984703 ) ) ;
#24206 = DIRECTION ( 'NONE',  ( -0.000000000000000000, 1.000000000000000000, -0.000000000000000000 ) ) ;
#24207 = CARTESIAN_POINT ( 'NONE',  ( 0.1787899950787401604, -0.2353601887016795458, 0.07405724077823318263 ) ) ;
#24208 = EDGE_CURVE ( 'NONE', #36995, #42269, #30732, .T. ) ;
#24209 = CARTESIAN_POINT ( 'NONE',  ( 0.9500414927467377701, -0.1787899950787401604, 1.712598425143087466 ) ) ;
#24210 = CARTESIAN_POINT ( 'NONE',  ( 0.06844676939238621138, -0.09842519685039370636, 0.2099670925079330785 ) ) ;
#24211 = CARTESIAN_POINT ( 'NONE',  ( -0.1113553986120547346, 0.006889763779527558960, -0.1113553986120547346 ) ) ;
#24212 = FACE_OUTER_BOUND ( 'NONE', #2984, .T. ) ;
#24213 = VECTOR ( 'NONE', #34357, 39.37007874015748143 ) ;
#24214 = EDGE_CURVE ( 'NONE', #5872, #36671, #35494, .T. ) ;
#24215 = EDGE_CURVE ( 'NONE', #36523, #34498, #46933, .T. ) ;
#24216 = ORIENTED_EDGE ( 'NONE', *, *, #26324, .F. ) ;
#24217 = ADVANCED_FACE ( 'NONE', ( #40233 ), #12515, .T. ) ;
#24218 = CARTESIAN_POINT ( 'NONE',  ( -0.1264236179284866091, -0.9945866141194644738, -0.1264236179284866091 ) ) ;
#24219 = CARTESIAN_POINT ( 'NONE',  ( 0.1787899950787401882, -1.280019684985606254, -2.189545951927503898E-17 ) ) ;
#24220 = ADVANCED_FACE ( 'NONE', ( #44705 ), #6086, .F. ) ;
#24221 = CARTESIAN_POINT ( 'NONE',  ( -0.8107537697050254399, -0.1574803149606297803, 1.365649606191686294 ) ) ;
#24222 = SHAPE_REPRESENTATION_RELATIONSHIP ( 'NONE' , 'NONE' ,  #19102, #44979 ) ;
#24223 = CARTESIAN_POINT ( 'NONE',  ( -1.100456976456230270E-17, -0.4833115261184787181, -0.1797182628040039365 ) ) ;
#24224 = LINE ( 'NONE', #17947, #20894 ) ;
#24225 = CARTESIAN_POINT ( 'NONE',  ( -1.033464566929134687, 0.06523048226347956391, 0.7898622046168821687 ) ) ;
#24226 = CARTESIAN_POINT ( 'NONE',  ( -0.9412147342319837628, 0.1574803149606300301, 0.7258858267716535861 ) ) ;
#24227 = CARTESIAN_POINT ( 'NONE',  ( -0.06523048226347956391, -0.05954724409448820810, 0.1574803149606297803 ) ) ;
#24228 = AXIS2_PLACEMENT_3D ( 'NONE', #33935, #11169, #15716 ) ;
#24229 = CARTESIAN_POINT ( 'NONE',  ( 1.054774247047244540, 0.07405724077823318263, 0.8513779527021426707 ) ) ;
#24231 = CARTESIAN_POINT ( 'NONE',  ( 0.8759842519685039353, 0.000000000000000000, 2.007874015640504162 ) ) ;
#24230 = CARTESIAN_POINT ( 'NONE',  ( 0.1647197266561027384, 0.2003932537366638067, -0.03489849683095651994 ) ) ;
#24232 = CARTESIAN_POINT ( 'NONE',  ( 0.7185039370078746268, 0.06523048226347956391, 0.05659448808144944970 ) ) ;
#24233 = CARTESIAN_POINT ( 'NONE',  ( 0.8107537697050253289, 0.1574803149606300301, 0.1796259842519684069 ) ) ;
#24234 = CARTESIAN_POINT ( 'NONE',  ( 1.033464566929134687, 0.06523048226347956391, 0.7111220471365682361 ) ) ;
#24235 = CARTESIAN_POINT ( 'NONE',  ( 0.1787899950787401882, -0.5762795275052914334, -2.189545951927503898E-17 ) ) ;
#24236 = CARTESIAN_POINT ( 'NONE',  ( -1.094772975963752103E-17, -1.348917322780881944, -0.1787899950787401882 ) ) ;
#24237 = CARTESIAN_POINT ( 'NONE',  ( -0.8759842519685039353, 0.1787899950787401882, 1.961122047190330786 ) ) ;
#24238 = EDGE_LOOP ( 'NONE', ( #9761, #36887, #12653, #40782 ) ) ;
#24239 = CARTESIAN_POINT ( 'NONE',  ( -0.7495606340400177148, 0.1264236179284866091, 1.459153543253322693 ) ) ;
#24240 = CARTESIAN_POINT ( 'NONE',  ( 0.7495606340400177148, -0.1264236179284866091, 1.429625984198204858 ) ) ;
#24241 = EDGE_CURVE ( 'NONE', #10554, #47128, #44032, .T. ) ;
#24242 = CARTESIAN_POINT ( 'NONE',  ( 0.000000000000000000, 0.000000000000000000, -0.04012007874015743186 ) ) ;
#24243 = CARTESIAN_POINT ( 'NONE',  ( -0.8759842519685039353, 0.1787899950787401882, 0.6274606298674959559 ) ) ;
#24244 = EDGE_CURVE ( 'NONE', #1067, #42873, #27834, .T. ) ;
#24245 = CARTESIAN_POINT ( 'NONE',  ( 0.4811709046783464450, 4.466152701071653354E-17, 0.000000000000000000 ) ) ;
#24246 = CARTESIAN_POINT ( 'NONE',  ( 1.002407869896990045, -0.1264236179284866091, 0.6914370078202519698 ) ) ;
#24247 = CARTESIAN_POINT ( 'NONE',  ( -0.8759842519685039353, -0.1787899950787401882, 0.6028543306548976854 ) ) ;
#24248 = LINE ( 'NONE', #42189, #32297 ) ;
#24249 = PLANE ( 'NONE',  #42064 ) ;
#24250 = VERTEX_POINT ( 'NONE', #47409 ) ;
#24251 = CARTESIAN_POINT ( 'NONE',  ( 0.1574803149606300023, -0.9875035750853327077, -1.463737590216208861 ) ) ;
#24252 = CARTESIAN_POINT ( 'NONE',  ( -0.8107537697050253289, 0.1574803149606300301, 0.2583661417322835052 ) ) ;
#24253 = EDGE_CURVE ( 'NONE', #11416, #28921, #10242, .T. ) ;
#24254 = CARTESIAN_POINT ( 'NONE',  ( 0.8759842519685039353, -0.1787899950787401882, 1.237696850339937038 ) ) ;
#24255 = CARTESIAN_POINT ( 'NONE',  ( 0.1778978046402051039, -0.09851384678937105677, 0.1186814646440462612 ) ) ;
#24256 = EDGE_LOOP ( 'NONE', ( #29832, #6914, #14310, #29426, #39536 ) ) ;
#24257 = B_SPLINE_CURVE_WITH_KNOTS ( 'NONE', 3,
 ( #43202, #9935, #21409, #25016, #20702, #38697, #28395, #2488, #46337, #35343, #35576, #17826, #5869, #17114, #16878, #24778, #17584, #44106, #24542 ),
 .UNSPECIFIED., .F., .F.,
 ( 4, 1, 1, 1, 2, 2, 1, 1, 1, 1, 2, 2, 4 ),
 ( 0.000000000000000000, 0.1250000000000016376, 0.1875000000000024425, 0.2187500000000027756, 0.2343750000000029976, 0.2500000000000031641, 0.3750000000000044409, 0.4375000000000049960, 0.4687500000000053846, 0.4843750000000054956, 0.4921875000000056066, 0.5000000000000056621, 1.000000000000000000 ),
 .UNSPECIFIED. ) ;
#24258 = PLANE ( 'NONE',  #34818 ) ;
#24259 = CARTESIAN_POINT ( 'NONE',  ( -0.8019270111902717657, 0.1787899950787401604, 0.9055118109698585549 ) ) ;
#24260 = CARTESIAN_POINT ( 'NONE',  ( -0.1787899950787401882, -1.551797196575694926, 0.000000000000000000 ) ) ;
#24261 = EDGE_LOOP ( 'NONE', ( #150, #46970, #688, #37729 ) ) ;
#24262 = CARTESIAN_POINT ( 'NONE',  ( 1.033464566929134687, 0.06523048226347956391, 0.9965551181102363376 ) ) ;
#24263 = CARTESIAN_POINT ( 'NONE',  ( 0.1264236179284866091, -0.6058070865604094912, -0.1264236179284866091 ) ) ;
#24264 = DIRECTION ( 'NONE',  ( -1.000000000000000000, 0.000000000000000000, 0.000000000000000000 ) ) ;
#24265 = VERTEX_POINT ( 'NONE', #14582 ) ;
#24266 = DIRECTION ( 'NONE',  ( 0.5735764363510447161, -0.8191520442889925757, 1.003171929053525486E-16 ) ) ;
#24267 = CARTESIAN_POINT ( 'NONE',  ( 0.1787899950787401882, -0.3400590550643468601, -2.189545951927503898E-17 ) ) ;
#24268 = CARTESIAN_POINT ( 'NONE',  ( -0.07405724077823318263, -0.7017716534895438452, 0.1787899950787401604 ) ) ;
#24269 = EDGE_CURVE ( 'NONE', #3655, #110, #1464, .T. ) ;
#24270 = FACE_OUTER_BOUND ( 'NONE', #13309, .T. ) ;
#24271 = CARTESIAN_POINT ( 'NONE',  ( 0.1602931993194444682, -0.1591122789105269553, 0.000000000000000000 ) ) ;
#24272 = CARTESIAN_POINT ( 'NONE',  ( 3.284318927891251994E-17, 0.03284847271564315246, 0.1787899950787401882 ) ) ;
#24273 = CARTESIAN_POINT ( 'NONE',  ( -0.1787899950787401604, 0.03641732288840918152, 0.07405724077823318263 ) ) ;
#24274 = APPLICATION_PROTOCOL_DEFINITION ( 'draft international standard', 'automotive_design', 1998, #8584 ) ;
#24275 = DIRECTION ( 'NONE',  ( 1.822029033848725028E-16, 0.000000000000000000, 1.000000000000000000 ) ) ;
#24276 = CARTESIAN_POINT ( 'NONE',  ( 0.8019270111902717657, -0.1787899950787401604, 0.5216535432533228045 ) ) ;
#24277 = CIRCLE ( 'NONE', #25824, 0.2952755905511810774 ) ;
#24278 = CARTESIAN_POINT ( 'NONE',  ( -0.9500414927467377701, -0.1787899950787401604, 0.8858267715997791836 ) ) ;
#24280 = CARTESIAN_POINT ( 'NONE',  ( 0.8759842519685039353, 0.000000000000000000, 4.498031496062992574 ) ) ;
#24279 = CARTESIAN_POINT ( 'NONE',  ( 0.1574803149606300301, -0.8715551181102356715, -0.06523048226347956391 ) ) ;
#24282 = CARTESIAN_POINT ( 'NONE',  ( -0.8493115269941948764, -0.1716529789732494093, 1.987718322235668911 ) ) ;
#24281 = CARTESIAN_POINT ( 'NONE',  ( -0.1797182628040039087, -1.499551683598794982, -0.07444174185955065859 ) ) ;
#24283 = CARTESIAN_POINT ( 'NONE',  ( -1.094772975963752103E-17, -0.4040354330171023745, -0.1787899950787401882 ) ) ;
#24284 = CARTESIAN_POINT ( 'NONE',  ( 1.054774247047244096, 0.000000000000000000, 1.483759842465921075 ) ) ;
#24286 = CARTESIAN_POINT ( 'NONE',  ( 0.1643927470070918051, 0.1622860936273138877, 1.482178915982735805E-13 ) ) ;
#24285 = CARTESIAN_POINT ( 'NONE',  ( 1.054774247047244096, 0.000000000000000000, 1.951279527505291433 ) ) ;
#24287 = CARTESIAN_POINT ( 'NONE',  ( 0.6971942568897637749, 2.189545951927499583E-17, 0.4355314960092284138 ) ) ;
#24288 = ORIENTED_EDGE ( 'NONE', *, *, #162, .T. ) ;
#24289 = CARTESIAN_POINT ( 'NONE',  ( -0.2137641352136847028, -0.06208088008912424766, -0.1620118252825171745 ) ) ;
#24290 = CARTESIAN_POINT ( 'NONE',  ( 1.033464566929133799, 1.928577636452524610E-17, 4.498031496062992574 ) ) ;
#24291 = CYLINDRICAL_SURFACE ( 'NONE', #16030, 0.1377952755905512694 ) ;
#24292 = CARTESIAN_POINT ( 'NONE',  ( 0.1264236179284866091, -0.1087598424659214497, 0.1264236179284866091 ) ) ;
#24293 = CARTESIAN_POINT ( 'NONE',  ( 0.8019270111902717657, 0.1787899950787401604, 0.4281496062454490659 ) ) ;
#24294 = CARTESIAN_POINT ( 'NONE',  ( -0.1787899950787401604, -0.9429133857730090940, 0.07405724077823318263 ) ) ;
#24295 = CARTESIAN_POINT ( 'NONE',  ( 0.8759842519685039353, 0.000000000000000000, 4.498031496062992574 ) ) ;
#24296 = CARTESIAN_POINT ( 'NONE',  ( 0.1627249056762484491, 0.5419983459879520460, -0.7609487005970335671 ) ) ;
#24297 = CARTESIAN_POINT ( 'NONE',  ( -1.054774247047244096, 0.000000000000000000, 1.439468503883244210 ) ) ;
#24298 = ORIENTED_EDGE ( 'NONE', *, *, #46241, .T. ) ;
#24299 = DIRECTION ( 'NONE',  ( 0.000000000000000000, -0.9699617890481200266, -0.2432573283306594947 ) ) ;
#24300 = CARTESIAN_POINT ( 'NONE',  ( -0.9412147342319837628, -0.1574803149606297803, 0.5831692912310553201 ) ) ;
#24301 = VERTEX_POINT ( 'NONE', #40426 ) ;
#24302 = CARTESIAN_POINT ( 'NONE',  ( -0.7185039370078746268, 0.06523048226347956391, 1.326279527559055982 ) ) ;
#24303 = CARTESIAN_POINT ( 'NONE',  ( -1.002407869896990045, 0.1264236179284866091, 0.8538385826234016207 ) ) ;
#24304 = EDGE_CURVE ( 'NONE', #18202, #32512, #37588, .T. ) ;
#24305 = DIRECTION ( 'NONE',  ( 1.000000000000000000, -3.368395098984144529E-15, 0.000000000000000000 ) ) ;
#24306 = DIRECTION ( 'NONE',  ( 0.000000000000000000, 1.000000000000000000, 0.000000000000000000 ) ) ;
#24307 = CARTESIAN_POINT ( 'NONE',  ( 1.054774247047244540, 0.07405724077823318263, 0.2263779527021417270 ) ) ;
#24308 = CARTESIAN_POINT ( 'NONE',  ( 0.8759842519685039353, 0.1574803149606299191, 1.466535432963338437 ) ) ;
#24309 = ORIENTED_EDGE ( 'NONE', *, *, #18239, .F. ) ;
#24310 = ADVANCED_FACE ( 'NONE', ( #40891 ), #8084, .T. ) ;
#24311 = CARTESIAN_POINT ( 'NONE',  ( -0.1476377952755905387, 0.5419727308409664213, -0.7545416139885205986 ) ) ;
#24312 = ADVANCED_FACE ( 'NONE', ( #415 ), #13261, .F. ) ;
#24313 = CARTESIAN_POINT ( 'NONE',  ( -0.6971942568897637749, 2.189545951927499583E-17, 1.695374015694267822 ) ) ;
#24314 = EDGE_LOOP ( 'NONE', ( #21415, #9981, #9986, #8388, #39177 ) ) ;
#24315 = ADVANCED_FACE ( 'NONE', ( #11459 ), #30152, .F. ) ;
#24316 = VECTOR ( 'NONE', #31788, 39.37007874015748143 ) ;
#24317 = LINE ( 'NONE', #38915, #46719 ) ;
#24318 = CARTESIAN_POINT ( 'NONE',  ( 0.05249343832021334533, 0.4668427075568369333, -0.7022306805398672580 ) ) ;
#24319 = CARTESIAN_POINT ( 'NONE',  ( -0.1787899950787401882, -1.079356251693805113, 0.000000000000000000 ) ) ;
#24320 = ORIENTED_EDGE ( 'NONE', *, *, #42657, .T. ) ;
#24321 = CARTESIAN_POINT ( 'NONE',  ( 0.1264236179284866091, -0.1432086613635592531, 0.1264236179284866091 ) ) ;
#24322 = ORIENTED_EDGE ( 'NONE', *, *, #13752, .F. ) ;
#24323 = ORIENTED_EDGE ( 'NONE', *, *, #46629, .F. ) ;
#24324 = CARTESIAN_POINT ( 'NONE',  ( -0.2559054651920882328, -0.06820678008027236672, -0.3098418326308006177 ) ) ;
#24325 = CARTESIAN_POINT ( 'NONE',  ( -0.7646288533564489232, 0.1113553986120547346, 0.9202755904436535905 ) ) ;
#24326 = PRODUCT ( 'Pivot Pin', 'Pivot Pin', '', ( #22611 ) ) ;
#24327 = CARTESIAN_POINT ( 'NONE',  ( 0.7646288533564489232, 0.1113553986120547346, 1.835629921259842590 ) ) ;
#24328 = CARTESIAN_POINT ( 'NONE',  ( -0.07444174185955065859, -0.1265201875358013817, -0.1797182628040039087 ) ) ;
#24329 = CARTESIAN_POINT ( 'NONE',  ( 0.1787899950787401604, -0.7706692912848194243, -0.07405724077823318263 ) ) ;
#24330 = CARTESIAN_POINT ( 'NONE',  ( -0.7495606340400177148, 0.1264236179284866091, 0.3961614172690708924 ) ) ;
#24331 = CARTESIAN_POINT ( 'NONE',  ( -0.8759842519685039353, 0.1574803149606299191, 1.043307086614173151 ) ) ;
#24332 = AXIS2_PLACEMENT_3D ( 'NONE', #8001, #30332, #41270 ) ;
#24333 = CARTESIAN_POINT ( 'NONE',  ( -0.1270800023317771588, -1.187051683598793428, -0.1270800023317771588 ) ) ;
#24334 = CARTESIAN_POINT ( 'NONE',  ( -0.1126596235262965900, 0.2304501682926980155, -0.02834147079956141763 ) ) ;
#24335 = CARTESIAN_POINT ( 'NONE',  ( 0.7495606340400177148, -0.1264236179284866091, 1.154035433017102319 ) ) ;
#24336 = CARTESIAN_POINT ( 'NONE',  ( 0.8759842519685039353, 0.1787899950787401882, 1.528051181048598384 ) ) ;
#24337 = CARTESIAN_POINT ( 'NONE',  ( 0.000000000000000000, 0.000000000000000000, 0.000000000000000000 ) ) ;
#24338 = CARTESIAN_POINT ( 'NONE',  ( 1.033464566929134687, -0.06523048226347956391, 1.660925196850393526 ) ) ;
#24340 = CARTESIAN_POINT ( 'NONE',  ( 1.033464566929134687, 0.06523048226347956391, 1.705216535433070613 ) ) ;
#24339 = CARTESIAN_POINT ( 'NONE',  ( 0.1574803149606299746, 0.4666052258408023845, -0.7025346432751043979 ) ) ;
#24341 = CARTESIAN_POINT ( 'NONE',  ( 0.7185039370078739607, 1.928577636452523993E-17, 1.437007873908220601 ) ) ;
#24342 = DIRECTION ( 'NONE',  ( 0.000000000000000000, 0.000000000000000000, -1.000000000000000000 ) ) ;
#24343 = AXIS2_PLACEMENT_3D ( 'NONE', #35791, #13292, #27921 ) ;
#24344 = CARTESIAN_POINT ( 'NONE',  ( -0.07405724077823318263, 0.006889763833291078637, 0.1787899950787401604 ) ) ;
#24345 = PLANE ( 'NONE',  #36030 ) ;
#24346 = CARTESIAN_POINT ( 'NONE',  ( 0.6971942568897648851, 0.07405724077823318263, 1.181102362150960428 ) ) ;
#24347 = CARTESIAN_POINT ( 'NONE',  ( 1.002407869896990045, -0.1264236179284866091, 1.990649606245448844 ) ) ;
#24348 = CARTESIAN_POINT ( 'NONE',  ( 0.9873396505805591694, -0.1113553986120547346, 0.2706692912310554866 ) ) ;
#24349 = EDGE_LOOP ( 'NONE', ( #42929, #127, #31924, #24644 ) ) ;
#24350 = LINE ( 'NONE', #20508, #29950 ) ;
#24351 = CARTESIAN_POINT ( 'NONE',  ( -0.8107537697050253289, 0.1574803149606300301, 0.2091535431995598104 ) ) ;
#24352 = ORIENTED_EDGE ( 'NONE', *, *, #33471, .T. ) ;
#24353 = CARTESIAN_POINT ( 'NONE',  ( 0.8759842519685039353, 0.1787899950787401882, 1.370570866087968520 ) ) ;
#24355 = CARTESIAN_POINT ( 'NONE',  ( -0.9873396505805591694, 0.1113553986120547346, 0.2805118109160948947 ) ) ;
#24354 = CARTESIAN_POINT ( 'NONE',  ( 0.05836929678887253087, -0.07899262986804667097, 0.2517335218907257310 ) ) ;
#24356 = DIMENSIONAL_EXPONENTS ( 1.000000000000000000, 0.000000000000000000, 0.000000000000000000, 0.000000000000000000, 0.000000000000000000, 0.000000000000000000, 0.000000000000000000 ) ;
#24357 = CARTESIAN_POINT ( 'NONE',  ( -0.06523048226347956391, -1.767224409448819866, -0.1574803149606300301 ) ) ;
#24358 = CARTESIAN_POINT ( 'NONE',  ( -1.033464566929134687, -0.06523048226347956391, 1.021161417215306955 ) ) ;
#24359 = ADVANCED_FACE ( 'NONE', ( #37313 ), #34713, .T. ) ;
#24360 = VERTEX_POINT ( 'NONE', #11945 ) ;
#24361 = CARTESIAN_POINT ( 'NONE',  ( -0.9873396505805591694, 0.1113553986120547346, 0.2017716534357799352 ) ) ;
#24362 = FACE_OUTER_BOUND ( 'NONE', #11827, .T. ) ;
#24363 = ORIENTED_EDGE ( 'NONE', *, *, #35719, .T. ) ;
#24364 = CARTESIAN_POINT ( 'NONE',  ( 0.1787899950787401604, -1.636811023568283341, -0.07405724077823318263 ) ) ;
#24365 = CARTESIAN_POINT ( 'NONE',  ( -0.6971942568897637749, 2.189545951927499583E-17, 0.9522637794737952577 ) ) ;
#24366 = CARTESIAN_POINT ( 'NONE',  ( -1.033464566929134687, 0.06523048226347956391, 0.01230314960629920289 ) ) ;
#24367 = EDGE_CURVE ( 'NONE', #23901, #14042, #21670, .T. ) ;
#24368 = CARTESIAN_POINT ( 'NONE',  ( -0.9500414927467378812, 0.1787899950787401604, 0.6249999999462356737 ) ) ;
#24369 = CONICAL_SURFACE ( 'NONE', #8278, 0.1377952755905511861, 1.047197551196598297 ) ;
#24370 = CARTESIAN_POINT ( 'NONE',  ( 0.1574028386749138364, 0.1230214933236144365, -0.03225005981621940909 ) ) ;
#24371 = CARTESIAN_POINT ( 'NONE',  ( 0.8759842519685039353, 0.000000000000000000, 4.498031496062992574 ) ) ;
#24372 = ORIENTED_EDGE ( 'NONE', *, *, #41849, .T. ) ;
#24373 = CARTESIAN_POINT ( 'NONE',  ( -0.1104063604032177182, -0.08956089369968209257, -0.1415710564723076936 ) ) ;
#24374 = CARTESIAN_POINT ( 'NONE',  ( 0.2471922904502826812, -0.09842519685039370636, 0.1427165354330708902 ) ) ;
#24375 = ORIENTED_EDGE ( 'NONE', *, *, #26702, .T. ) ;
#24376 = DIRECTION ( 'NONE',  ( 1.000000000000000000, 0.000000000000000000, 0.000000000000000000 ) ) ;
#24377 = CIRCLE ( 'NONE', #9088, 0.3912448816427701037 ) ;
#24378 = CARTESIAN_POINT ( 'NONE',  ( -1.054774247047244540, 0.07405724077823318263, 0.6938976377415123631 ) ) ;
#24379 = VERTEX_POINT ( 'NONE', #44962 ) ;
#24380 = CARTESIAN_POINT ( 'NONE',  ( -0.8759842519685039353, 0.1787899950787401882, 1.729822834591905556 ) ) ;
#24381 = EDGE_CURVE ( 'NONE', #28928, #26635, #12173, .T. ) ;
#24382 = DIRECTION ( 'NONE',  ( 1.000000000000000000, 0.000000000000000000, 0.000000000000000000 ) ) ;
#24383 = CARTESIAN_POINT ( 'NONE',  ( 0.7185039370078739607, 1.928577636452523993E-17, 0.3444881889763780070 ) ) ;
#24384 = ADVANCED_BREP_SHAPE_REPRESENTATION ( 'Threaded Bushing', ( #36588, #20860 ), #22411 ) ;
#24385 = VERTEX_POINT ( 'NONE', #19587 ) ;
#24386 = CARTESIAN_POINT ( 'NONE',  ( 1.033464566929133799, 0.000000000000000000, 0.6003937007874016185 ) ) ;
#24387 = CARTESIAN_POINT ( 'NONE',  ( -0.1270800023317771588, -0.6752406599767460937, -0.1270800023317771588 ) ) ;
#24388 = CARTESIAN_POINT ( 'NONE',  ( 0.2471922904502827090, 0.07885719401822738339, 0.07558487950069545103 ) ) ;
#24389 = CARTESIAN_POINT ( 'NONE',  ( -0.8759842519685039353, 0.1574803149606299191, 1.387795275483023616 ) ) ;
#24391 = DIRECTION ( 'NONE',  ( 0.000000000000000000, 0.000000000000000000, 1.000000000000000000 ) ) ;
#24390 = CARTESIAN_POINT ( 'NONE',  ( -9.642888182262618425E-18, -0.3917322834645669549, -0.1574803149606299191 ) ) ;
#24392 = DIRECTION ( 'NONE',  ( 0.000000000000000000, 0.000000000000000000, -1.000000000000000000 ) ) ;
#24393 = ORIENTED_EDGE ( 'NONE', *, *, #40983, .F. ) ;
#24394 = FACE_OUTER_BOUND ( 'NONE', #6595, .T. ) ;
#24395 = CARTESIAN_POINT ( 'NONE',  ( 0.9873396505805591694, 0.1113553986120547346, 1.195866141732283561 ) ) ;
#24397 = DIRECTION ( 'NONE',  ( 0.000000000000000000, 0.000000000000000000, -1.000000000000000000 ) ) ;
#24396 = DIRECTION ( 'NONE',  ( -1.000000000000000000, 0.000000000000000000, 0.000000000000000000 ) ) ;
#24398 = CARTESIAN_POINT ( 'NONE',  ( 0.7185039370078739607, 1.928577636452523993E-17, 1.958661417322834719 ) ) ;
#24400 = CYLINDRICAL_SURFACE ( 'NONE', #28563, 0.04921259842519680461 ) ;
#24399 = DIRECTION ( 'NONE',  ( -0.000000000000000000, -0.000000000000000000, -1.000000000000000000 ) ) ;
#24401 = AXIS2_PLACEMENT_3D ( 'NONE', #14496, #26240, #40338 ) ;
#24402 = CARTESIAN_POINT ( 'NONE',  ( -1.033464566929133799, 1.928577636452524610E-17, 2.869337061179095023E-17 ) ) ;
#24403 = CARTESIAN_POINT ( 'NONE',  ( -0.1235961452251413406, 0.09842519685039370636, 0.2140748031496062798 ) ) ;
#24404 = VERTEX_POINT ( 'NONE', #44729 ) ;
#24405 = AXIS2_PLACEMENT_3D ( 'NONE', #1870, #2566, #37650 ) ;
#24406 = CARTESIAN_POINT ( 'NONE',  ( 0.0003553830333942854065, 0.1126092284109782571, -0.08054791328661504990 ) ) ;
#24407 = CARTESIAN_POINT ( 'NONE',  ( 0.9500414927467378812, 0.1787899950787401604, 0.8169291338045038264 ) ) ;
#24408 = FACE_OUTER_BOUND ( 'NONE', #36340, .T. ) ;
#24409 = DIRECTION ( 'NONE',  ( 0.000000000000000000, 1.000000000000000000, 0.000000000000000000 ) ) ;
#24410 = CARTESIAN_POINT ( 'NONE',  ( 0.1797182628040039087, 0.02111760773978908073, -0.07444174185955065859 ) ) ;
#24411 = CARTESIAN_POINT ( 'NONE',  ( 0.07405724077823318263, -1.041338582623402287, -0.1787899950787401604 ) ) ;
#24413 = AXIS2_PLACEMENT_3D ( 'NONE', #33475, #18359, #25801 ) ;
#24412 = CARTESIAN_POINT ( 'NONE',  ( 0.1113553986120547346, -1.341535433070866201, -0.1113553986120547346 ) ) ;
#24414 = CARTESIAN_POINT ( 'NONE',  ( 0.1596650774283297214, 0.1494101348903360271, -0.02216197906078976390 ) ) ;
#24415 = EDGE_CURVE ( 'NONE', #39582, #30632, #41356, .T. ) ;
#24416 = CARTESIAN_POINT ( 'NONE',  ( -0.8019270111902717657, -0.1787899950787401604, 1.904527559001354398 ) ) ;
#24417 = ORIENTED_EDGE ( 'NONE', *, *, #38250, .F. ) ;
#24418 = CARTESIAN_POINT ( 'NONE',  ( -0.8107537697050254399, -0.1574803149606297803, 0.8144685038294804391 ) ) ;
#24419 = ORIENTED_EDGE ( 'NONE', *, *, #17008, .T. ) ;
#24420 = CARTESIAN_POINT ( 'NONE',  ( 0.7185039370078746268, -0.06523048226347956391, 0.5437992125984247860 ) ) ;
#24421 = CARTESIAN_POINT ( 'NONE',  ( -1.002407869896990045, 0.1264236179284866091, 1.562499999946236118 ) ) ;
#24422 = DIRECTION ( 'NONE',  ( 1.822029033848725028E-16, 0.000000000000000000, 1.000000000000000000 ) ) ;
#24423 = EDGE_CURVE ( 'NONE', #35869, #32338, #14034, .T. ) ;
#24424 = CARTESIAN_POINT ( 'NONE',  ( -1.002407869896990045, -0.1264236179284866091, 0.2977362204186775885 ) ) ;
#24425 = CARTESIAN_POINT ( 'NONE',  ( -0.2471922904502826535, 0.08140987345728177560, 0.07064030526712006264 ) ) ;
#24426 = CARTESIAN_POINT ( 'NONE',  ( -1.054774247047244540, 0.07405724077823318263, 1.958661417269071947 ) ) ;
#24427 = CARTESIAN_POINT ( 'NONE',  ( -0.1528720448724869563, 0.09445537554013619386, 0.1971723546074427569 ) ) ;
#24428 = CARTESIAN_POINT ( 'NONE',  ( -0.7646288533564489232, -0.1113553986120547346, 1.924212598425196985 ) ) ;
#24429 = CARTESIAN_POINT ( 'NONE',  ( -0.4240551181102362177, -2.591110818884263559E-17, 0.000000000000000000 ) ) ;
#24430 = CARTESIAN_POINT ( 'NONE',  ( 0.07405724077823318263, -0.2402814485441996661, 0.1787899950787401604 ) ) ;
#24431 = CARTESIAN_POINT ( 'NONE',  ( 0.1605230700181201065, -0.09842519685039370636, 0.1447514863646086891 ) ) ;
#24432 = LINE ( 'NONE', #28053, #39425 ) ;
#24433 = CARTESIAN_POINT ( 'NONE',  ( -1.033464566929135131, 1.928577636452536319E-17, 0.03937007874015843040 ) ) ;
#24434 = ORIENTED_EDGE ( 'NONE', *, *, #20509, .F. ) ;
#24435 = CARTESIAN_POINT ( 'NONE',  ( -0.9500414927467377701, -0.1787899950787401604, 1.200787401521039355 ) ) ;
#24436 = VERTEX_POINT ( 'NONE', #37806 ) ;
#24437 = CARTESIAN_POINT ( 'NONE',  ( 3.284318927891251994E-17, -1.097933070812378009, 0.1787899950787401882 ) ) ;
#24438 = CARTESIAN_POINT ( 'NONE',  ( 0.07405724077823318263, -1.287401574749386768, 0.1787899950787401604 ) ) ;
#24439 = ( BOUNDED_CURVE ( )  B_SPLINE_CURVE ( 2, ( #45471, #16281, #34736, #1875, #45710, #12927, #42109, #9318, #20327 ),
 .UNSPECIFIED., .F., .T. ) 
 B_SPLINE_CURVE_WITH_KNOTS ( ( 3, 2, 2, 2, 3 ),
 ( 0.9699999999999999734, 0.9725000000000000311, 0.9749999999999999778, 0.9775000000000000355, 0.9799999999999999822 ),
 .UNSPECIFIED. ) 
 CURVE ( )  GEOMETRIC_REPRESENTATION_ITEM ( )  RATIONAL_B_SPLINE_CURVE ( ( 1.000000000000000000, 0.9238795325112939549, 1.000000000000000000, 0.9238795325112869605, 1.000000000000000000, 0.9238795325112869605, 1.000000000000000000, 0.9238795325112869605, 1.000000000000000000 ) ) 
 REPRESENTATION_ITEM ( '' )  ) ;
#24440 = DIRECTION ( 'NONE',  ( -1.000000000000000000, 0.000000000000000000, 0.000000000000000000 ) ) ;
#24441 = LENGTH_MEASURE_WITH_UNIT ( LENGTH_MEASURE( 0.02539999999999999897 ), #42624 ) ;
#24442 = CARTESIAN_POINT ( 'NONE',  ( 0.07444174185955046430, -0.4857721560397386673, -0.1797182628040039087 ) ) ;
#24443 = DIRECTION ( 'NONE',  ( 0.000000000000000000, 1.000000000000000000, 0.000000000000000000 ) ) ;
#24444 = CARTESIAN_POINT ( 'NONE',  ( -0.7646288533564489232, -0.1113553986120547346, 0.8513779526483780113 ) ) ;
#24445 = CARTESIAN_POINT ( 'NONE',  ( -0.9412147342319837628, -0.1574803149606297803, 0.6717519685039377020 ) ) ;
#24446 = AXIS2_PLACEMENT_3D ( 'NONE', #23642, #34919, #15999 ) ;
#24447 = CARTESIAN_POINT ( 'NONE',  ( -0.06523048226347956391, -0.02017716535433068670, 0.1574803149606297803 ) ) ;
#24448 = CARTESIAN_POINT ( 'NONE',  ( 0.6971942568897637749, 2.189545951927499583E-17, 0.9473425196312755814 ) ) ;
#24449 = CARTESIAN_POINT ( 'NONE',  ( -1.033464566929133799, 0.000000000000000000, 1.072834645669291431 ) ) ;
#24451 = CARTESIAN_POINT ( 'NONE',  ( 0.4151545546392377273, 4.766607801171850497E-17, 0.000000000000000000 ) ) ;
#24450 = CARTESIAN_POINT ( 'NONE',  ( 0.1706040688522296178, 0.1969959271857260608, -0.03730110279444987659 ) ) ;
#24452 = CARTESIAN_POINT ( 'NONE',  ( 0.7185039370078739607, 1.928577636452523993E-17, 1.082677165246803241 ) ) ;
#24453 = CARTESIAN_POINT ( 'NONE',  ( 0.9412147342319837628, -0.1574803149606297803, 0.1894685038294807722 ) ) ;
#24454 = CARTESIAN_POINT ( 'NONE',  ( 0.7185039370078746268, -0.06523048226347956391, 0.1894685039370080093 ) ) ;
#24455 = CARTESIAN_POINT ( 'NONE',  ( 0.000000000000000000, 0.09842519685039370636, 0.000000000000000000 ) ) ;
#24456 = CARTESIAN_POINT ( 'NONE',  ( 0.7185039370078739607, 1.928577636452523993E-17, 0.3740157479239689664 ) ) ;
#24457 = CARTESIAN_POINT ( 'NONE',  ( -1.094772975963752103E-17, -0.6058070865604094912, -0.1787899950787401882 ) ) ;
#24458 = CARTESIAN_POINT ( 'NONE',  ( -0.1264236179284866091, -1.383366141678519678, -0.1264236179284866091 ) ) ;
#24459 = ( BOUNDED_CURVE ( )  B_SPLINE_CURVE ( 2, ( #23198, #37814, #45209, #12431, #15299, #29952, #26337, #9292, #9531 ),
 .UNSPECIFIED., .F., .F. ) 
 B_SPLINE_CURVE_WITH_KNOTS ( ( 3, 2, 2, 2, 3 ),
 ( 0.5699999999999999512, 0.5725000000000000089, 0.5749999999999999556, 0.5775000000000000133, 0.5799999999999999600 ),
 .UNSPECIFIED. ) 
 CURVE ( )  GEOMETRIC_REPRESENTATION_ITEM ( )  RATIONAL_B_SPLINE_CURVE ( ( 1.000000000000000000, 0.9238795325112899581, 1.000000000000000000, 0.9238795325112869605, 1.000000000000000000, 0.9238795325112869605, 1.000000000000000000, 0.9238795325112869605, 1.000000000000000000 ) ) 
 REPRESENTATION_ITEM ( '' )  ) ;
#24460 = ADVANCED_FACE ( 'NONE', ( #19344 ), #36985, .T. ) ;
#24461 = AXIS2_PLACEMENT_3D ( 'NONE', #43364, #11753, #7653 ) ;
#24462 = CARTESIAN_POINT ( 'NONE',  ( -1.054774247047244540, 0.07405724077823318263, 1.874999999946236784 ) ) ;
#24463 = ORIENTED_EDGE ( 'NONE', *, *, #25166, .F. ) ;
#24464 = CARTESIAN_POINT ( 'NONE',  ( -0.7495606340400177148, 0.1264236179284866091, 1.419783464513165505 ) ) ;
#24465 = CARTESIAN_POINT ( 'NONE',  ( 1.054774247047244540, -0.07405724077823318263, 1.481299212544662680 ) ) ;
#24466 = ORIENTED_EDGE ( 'NONE', *, *, #33481, .T. ) ;
#24467 = DIRECTION ( 'NONE',  ( -3.469446951953613794E-15, -1.000000000000000000, 0.000000000000000000 ) ) ;
#24468 = CARTESIAN_POINT ( 'NONE',  ( 0.1113553986120547346, -1.262795275483023394, 0.1113553986120547346 ) ) ;
#24469 = CARTESIAN_POINT ( 'NONE',  ( -1.054774247047244540, -0.07405724077823318263, 0.6938976377415123631 ) ) ;
#24470 = CARTESIAN_POINT ( 'NONE',  ( 1.002407869896990045, 0.1264236179284866091, 0.1894685038832444879 ) ) ;
#24471 = CARTESIAN_POINT ( 'NONE',  ( 0.1346784485371297357, -0.09842520765884796297, -0.1175907832281543053 ) ) ;
#24472 = FILL_AREA_STYLE ('',( #28087 ) ) ;
#24473 = CARTESIAN_POINT ( 'NONE',  ( 0.6971942568897648851, 0.07405724077823318263, 0.5561023621509617598 ) ) ;
#24474 = CARTESIAN_POINT ( 'NONE',  ( -1.054774247047244540, -0.07405724077823318263, 0.6102362204186774219 ) ) ;
#24475 = EDGE_CURVE ( 'NONE', #5435, #1272, #7930, .T. ) ;
#24476 = AXIS2_PLACEMENT_3D ( 'NONE', #38912, #20697, #5619 ) ;
#24477 = ADVANCED_FACE ( 'NONE', ( #29407 ), #44881, .T. ) ;
#24478 = B_SPLINE_CURVE_WITH_KNOTS ( 'NONE', 3,
 ( #3685, #14717, #39855, #29390, #14482, #11133, #22362, #17595, #25755, #47059, #36303, #28654, #43214, #25024, #6800, #3206, #17836, #29141, #32479, #14253, #3454, #10902, #1254 ),
 .UNSPECIFIED., .F., .F.,
 ( 4, 2, 2, 1, 1, 1, 2, 2, 2, 1, 1, 2, 2, 4 ),
 ( 0.000000000000000000, 0.2499999999999978906, 0.3749999999999967248, 0.4374999999999960032, 0.4687499999999957812, 0.4843749999999957812, 0.4921874999999958367, 0.4999999999999958922, 0.6249999999999973355, 0.6874999999999981126, 0.7187499999999983347, 0.7343749999999984457, 0.7499999999999985567, 1.000000000000000000 ),
 .UNSPECIFIED. ) ;
#24479 = CARTESIAN_POINT ( 'NONE',  ( 0.000000000000000000, 0.000000000000000000, -0.1183602362204724257 ) ) ;
#24480 = ORIENTED_EDGE ( 'NONE', *, *, #23714, .T. ) ;
#24481 = CARTESIAN_POINT ( 'NONE',  ( -0.6971942568897648851, -0.07405724077823297447, 1.387795275536786610 ) ) ;
#24482 = CARTESIAN_POINT ( 'NONE',  ( -1.033464566929133799, 0.000000000000000000, 0.4035433070866141780 ) ) ;
#24483 = AXIS2_PLACEMENT_3D ( 'NONE', #25790, #14758, #18109 ) ;
#24484 = CARTESIAN_POINT ( 'NONE',  ( -0.2364785587839823289, -0.09851385148207500442, -0.06085331962129881395 ) ) ;
#24485 = ( REPRESENTATION_RELATIONSHIP ('NONE','NONE', #9609, #4677 ) REPRESENTATION_RELATIONSHIP_WITH_TRANSFORMATION ( #34356 )SHAPE_REPRESENTATION_RELATIONSHIP( ) ) ;
#24486 = VERTEX_POINT ( 'NONE', #33210 ) ;
#24487 = CARTESIAN_POINT ( 'NONE',  ( 0.07405724077823318263, -1.618234204449711111, 0.1787899950787401604 ) ) ;
#24488 = ORIENTED_EDGE ( 'NONE', *, *, #12026, .F. ) ;
#24489 = CARTESIAN_POINT ( 'NONE',  ( 0.1787899950787401604, -0.6082677164816695514, -0.07405724077823318263 ) ) ;
#24490 = CARTESIAN_POINT ( 'NONE',  ( 0.9412147342319837628, -0.1574803149606297803, 1.616633858267715773 ) ) ;
#24491 = CARTESIAN_POINT ( 'NONE',  ( 0.8759842519685039353, -0.1574803149606299191, 0.3937007874015748254 ) ) ;
#24492 = EDGE_LOOP ( 'NONE', ( #38690, #19282, #6689, #4242, #15007, #29558 ) ) ;
#24493 = CARTESIAN_POINT ( 'NONE',  ( 0.8759842519685039353, 0.1787899950787401882, 1.409940944828126153 ) ) ;
#24494 = FACE_OUTER_BOUND ( 'NONE', #33587, .T. ) ;
#24495 = CARTESIAN_POINT ( 'NONE',  ( 0.07405724077823318263, -0.2933070865604095467, -0.1787899950787401604 ) ) ;
#24496 = CARTESIAN_POINT ( 'NONE',  ( -0.1787899950787401604, -0.7854330708123791194, 0.07405724077823318263 ) ) ;
#24497 = CARTESIAN_POINT ( 'NONE',  ( -0.8759842519685039353, 0.000000000000000000, 0.000000000000000000 ) ) ;
#24498 = DIRECTION ( 'NONE',  ( 0.000000000000000000, 0.000000000000000000, 1.000000000000000000 ) ) ;
#24499 = CARTESIAN_POINT ( 'NONE',  ( 1.054774247047244540, -0.07405724077823318263, 1.673228346402929834 ) ) ;
#24500 = CARTESIAN_POINT ( 'NONE',  ( 0.7495606340400177148, 0.1264236179284866091, 0.3124999999462365619 ) ) ;
#24501 = CARTESIAN_POINT ( 'NONE',  ( 0.07405724077823318263, -0.02866727531585293309, -0.1787899950787401604 ) ) ;
#24502 = PRODUCT_CONTEXT ( 'NONE', #29442, 'mechanical' ) ;
#24503 = CARTESIAN_POINT ( 'NONE',  ( 0.8759842519685039353, 0.000000000000000000, 4.498031496062992574 ) ) ;
#24504 = CARTESIAN_POINT ( 'NONE',  ( 0.6971942568897626646, 0.07405724077823318263, 0.4724409448281262636 ) ) ;
#24505 = CARTESIAN_POINT ( 'NONE',  ( -0.8759842519685039353, -0.1787899950787401882, 0.7652559054580472253 ) ) ;
#24507 = DIRECTION ( 'NONE',  ( 1.000000000000000000, 0.000000000000000000, 0.000000000000000000 ) ) ;
#24506 = CARTESIAN_POINT ( 'NONE',  ( -9.642888182262618425E-18, -0.8248031496062991907, -0.1574803149606299191 ) ) ;
#24509 = CARTESIAN_POINT ( 'NONE',  ( -0.8262250934091986965, -0.1657888017163012262, 1.987284192870486521 ) ) ;
#24508 = CARTESIAN_POINT ( 'NONE',  ( -0.1797182628040039365, -1.693941447378320753, 0.000000000000000000 ) ) ;
#24510 = CARTESIAN_POINT ( 'NONE',  ( 0.8019270111902717657, 0.1787899950787401604, 1.692913385773008539 ) ) ;
#24512 = CARTESIAN_POINT ( 'NONE',  ( -0.8107537697050254399, -0.1574803149606297803, 1.808562992125984481 ) ) ;
#24511 = CARTESIAN_POINT ( 'NONE',  ( 0.2471922904502826812, 0.03219022224904102836, -0.1427165354330708902 ) ) ;
#24513 = CARTESIAN_POINT ( 'NONE',  ( 1.002407869896990045, 0.1264236179284866091, 0.4207677164816693294 ) ) ;
#24514 = EDGE_CURVE ( 'NONE', #4886, #20673, #29388, .T. ) ;
#24515 = ORIENTED_EDGE ( 'NONE', *, *, #33323, .T. ) ;
#24516 = CYLINDRICAL_SURFACE ( 'NONE', #13713, 0.1574803149606299191 ) ;
#24517 = CARTESIAN_POINT ( 'NONE',  ( 0.1787899950787401882, -0.1825787401037169411, -2.189545951927503898E-17 ) ) ;
#24518 = CARTESIAN_POINT ( 'NONE',  ( 1.002407869896990045, -0.1264236179284866091, 0.6077755904974173617 ) ) ;
#24519 = CARTESIAN_POINT ( 'NONE',  ( -0.1787899950787401604, -0.9822834645131651721, 0.07405724077823318263 ) ) ;
#24520 = CARTESIAN_POINT ( 'NONE',  ( 0.7895178597430446699, -0.1388632226133483527, 0.03936991021426686221 ) ) ;
#24521 = CARTESIAN_POINT ( 'NONE',  ( -0.7185039370078746268, -0.06523048226347956391, 0.9276574802074332160 ) ) ;
#24522 = CARTESIAN_POINT ( 'NONE',  ( -1.002407869896990045, -0.1264236179284866091, 1.513287401521039355 ) ) ;
#24523 = ORIENTED_EDGE ( 'NONE', *, *, #6270, .F. ) ;
#24524 = CARTESIAN_POINT ( 'NONE',  ( -0.2644880271752205192, -0.1617936740470128087, -0.9200531219794864102 ) ) ;
#24525 = CARTESIAN_POINT ( 'NONE',  ( 1.054774247047244096, 0.000000000000000000, 1.011318897584031484 ) ) ;
#24526 = VERTEX_POINT ( 'NONE', #14736 ) ;
#24527 = DIRECTION ( 'NONE',  ( 1.000000000000000000, -0.000000000000000000, -0.000000000000000000 ) ) ;
#24528 = CARTESIAN_POINT ( 'NONE',  ( 0.7495606340400177148, -0.1264236179284866091, 1.857775590497417362 ) ) ;
#24529 = CARTESIAN_POINT ( 'NONE',  ( -0.9873396505805591694, -0.1113553986120547346, 1.343503937007874072 ) ) ;
#24530 = CARTESIAN_POINT ( 'NONE',  ( -0.9500414927467378812, -0.1787899950787401604, 0.9202755904974182499 ) ) ;
#24531 = PLANE ( 'NONE',  #28183 ) ;
#24532 = CARTESIAN_POINT ( 'NONE',  ( 0.2519685039370078705, 4.616380251121755931E-17, 0.000000000000000000 ) ) ;
#24533 = CARTESIAN_POINT ( 'NONE',  ( 0.8759842519685039353, 0.1787899950787401882, 0.1156496062454492185 ) ) ;
#24534 = EDGE_CURVE ( 'NONE', #24379, #37983, #14372, .T. ) ;
#24535 = PRODUCT_DEFINITION_CONTEXT ( 'detailed design', #3971, 'design' ) ;
#24536 = CARTESIAN_POINT ( 'NONE',  ( 0.9873396505805591694, 0.1113553986120547346, 1.619094488081448846 ) ) ;
#24537 = ORIENTED_EDGE ( 'NONE', *, *, #15774, .F. ) ;
#24538 = CARTESIAN_POINT ( 'NONE',  ( 0.2362204724409448509, 0.000000000000000000, -1.186023622047243986 ) ) ;
#24539 = CARTESIAN_POINT ( 'NONE',  ( -0.7495606340400177148, 0.1264236179284866091, 1.651082677111590513 ) ) ;
#24540 = VECTOR ( 'NONE', #37846, 39.37007874015748143 ) ;
#24541 = ORIENTED_EDGE ( 'NONE', *, *, #2905, .T. ) ;
#24542 = CARTESIAN_POINT ( 'NONE',  ( -0.2471922904502826812, 0.03219022224904098672, -0.1427165354330708902 ) ) ;
#24543 = CARTESIAN_POINT ( 'NONE',  ( -0.7185039370078739607, 1.928577636452523993E-17, 0.7775590551181102983 ) ) ;
#24544 = CARTESIAN_POINT ( 'NONE',  ( 0.07405724077823318263, -1.145793259567821520, 0.1787899950787401604 ) ) ;
#24545 = VERTEX_POINT ( 'NONE', #11148 ) ;
#24546 = CARTESIAN_POINT ( 'NONE',  ( -0.1787899950787401604, -0.04232283459190578495, -0.07405724077823318263 ) ) ;
#24547 = EDGE_LOOP ( 'NONE', ( #22182, #7000, #42084, #1517 ) ) ;
#24548 = DIRECTION ( 'NONE',  ( 0.000000000000000000, 0.9771240687918540946, 0.2126700594527874133 ) ) ;
#24549 = CARTESIAN_POINT ( 'NONE',  ( 1.033464566929134687, 0.06523048226347956391, 1.862696850393700254 ) ) ;
#24550 = CARTESIAN_POINT ( 'NONE',  ( 0.07444174185955046430, -0.2495516835987934279, -0.1797182628040039087 ) ) ;
#24551 = CARTESIAN_POINT ( 'NONE',  ( 0.1787899950787401604, -0.8100393700249772788, -0.07405724077823318263 ) ) ;
#24552 = EDGE_CURVE ( 'NONE', #19233, #25854, #29396, .T. ) ;
#24553 = EDGE_CURVE ( 'NONE', #25965, #30060, #7304, .T. ) ;
#24554 = AXIS2_PLACEMENT_3D ( 'NONE', #20557, #9317, #27077 ) ;
#24555 = CARTESIAN_POINT ( 'NONE',  ( -1.054774247047244540, -0.07405724077823318263, 0.3001968503399373711 ) ) ;
#24556 = DIRECTION ( 'NONE',  ( 0.000000000000000000, 0.000000000000000000, 1.000000000000000000 ) ) ;
#24557 = CARTESIAN_POINT ( 'NONE',  ( -0.1797182628040039087, -1.337150108795643888, 0.07444174185955065859 ) ) ;
#24558 = CARTESIAN_POINT ( 'NONE',  ( -0.05770278849818247929, 0.2621795117899895500, -0.05428606100831778053 ) ) ;
#24559 = CARTESIAN_POINT ( 'NONE',  ( 0.6971942568897637749, 2.189545951927499583E-17, 1.109744094434425232 ) ) ;
#24560 = CARTESIAN_POINT ( 'NONE',  ( 1.002407869896990045, 0.1264236179284866091, 1.523129921206078707 ) ) ;
#24561 = CARTESIAN_POINT ( 'NONE',  ( 0.9500414927467377701, -0.1787899950787401604, 0.1722440944344254543 ) ) ;
#24562 = EDGE_CURVE ( 'NONE', #33555, #1767, #8237, .T. ) ;
#24563 = VECTOR ( 'NONE', #2986, 39.37007874015748143 ) ;
#24564 = CARTESIAN_POINT ( 'NONE',  ( -0.7185039370078739607, 1.928577636452523993E-17, 1.919291338582677309 ) ) ;
#24565 = CARTESIAN_POINT ( 'NONE',  ( 1.033464566929134687, -0.06523048226347956391, 1.700295275590550936 ) ) ;
#24567 = CARTESIAN_POINT ( 'NONE',  ( 1.033464566929133799, 0.000000000000000000, 0.3937007872940480047 ) ) ;
#24566 = FACE_OUTER_BOUND ( 'NONE', #44136, .T. ) ;
#24568 = CARTESIAN_POINT ( 'NONE',  ( 0.1636096867514420516, -0.08042879899057427118, -0.1393067463704355524 ) ) ;
#24569 = FACE_OUTER_BOUND ( 'NONE', #25299, .T. ) ;
#24570 = CARTESIAN_POINT ( 'NONE',  ( -0.8107537697050253289, 0.1574803149606300301, 1.783956692805858779 ) ) ;
#24571 = CARTESIAN_POINT ( 'NONE',  ( 0.6971942568897637749, 2.189545951927499583E-17, 0.1599409448281264023 ) ) ;
#24572 = ( BOUNDED_CURVE ( )  B_SPLINE_CURVE ( 2, ( #23581, #8477, #23112, #8718, #1762, #9195, #27447, #37725, #23354 ),
 .UNSPECIFIED., .F., .T. ) 
 B_SPLINE_CURVE_WITH_KNOTS ( ( 3, 2, 2, 2, 3 ),
 ( 0.4199999999999999845, 0.4224999999999999867, 0.4249999999999999889, 0.4274999999999999911, 0.4299999999999999933 ),
 .UNSPECIFIED. ) 
 CURVE ( )  GEOMETRIC_REPRESENTATION_ITEM ( )  RATIONAL_B_SPLINE_CURVE ( ( 1.000000000000000000, 0.9238795325112869605, 1.000000000000000000, 0.9238795325112869605, 1.000000000000000000, 0.9238795325112869605, 1.000000000000000000, 0.9238795325112869605, 1.000000000000000000 ) ) 
 REPRESENTATION_ITEM ( '' )  ) ;
#24573 = CARTESIAN_POINT ( 'NONE',  ( -0.3980944881889762477, 0.1574803149606354702, -0.7480314960629921295 ) ) ;
#24575 = CARTESIAN_POINT ( 'NONE',  ( -1.033464566929134687, 0.06523048226347956391, 1.813484251860976171 ) ) ;
#24574 = CARTESIAN_POINT ( 'NONE',  ( 0.9500414927467377701, -0.1787899950787401604, 1.117125984198203970 ) ) ;
#24576 = CARTESIAN_POINT ( 'NONE',  ( 1.033464566929133799, 0.000000000000000000, 0.6692913384751496553 ) ) ;
#24577 = CARTESIAN_POINT ( 'NONE',  ( 0.9873396505805591694, 0.1113553986120547346, 0.4379921258767252024 ) ) ;
#24578 = ORIENTED_EDGE ( 'NONE', *, *, #8998, .T. ) ;
#24579 = VECTOR ( 'NONE', #39004, 39.37007874015748143 ) ;
#24580 = LENGTH_MEASURE_WITH_UNIT ( LENGTH_MEASURE( 0.02539999999999999897 ), #28679 ) ;
#24581 = CARTESIAN_POINT ( 'NONE',  ( 1.027827790200348312, 0.05458466606556203887, 0.03937234633583642368 ) ) ;
#24582 = CARTESIAN_POINT ( 'NONE',  ( -0.7185039370078746268, -0.06523048226347956391, 0.4552165353255435698 ) ) ;
#24583 = ORIENTED_EDGE ( 'NONE', *, *, #35619, .T. ) ;
#24584 = CARTESIAN_POINT ( 'NONE',  ( 0.7495606340400177148, 0.1264236179284866091, 1.336122047190330786 ) ) ;
#24586 = CARTESIAN_POINT ( 'NONE',  ( 1.229559056033039366E-16, 0.000000000000000000, 0.3937007874015748254 ) ) ;
#24585 = CARTESIAN_POINT ( 'NONE',  ( -0.7185039370078739607, 1.928577636452523993E-17, 0.1082677165354330728 ) ) ;
#24587 = CARTESIAN_POINT ( 'NONE',  ( 0.1787899950787401882, 0.01919291343959027632, -2.189545951927503898E-17 ) ) ;
#24588 = CARTESIAN_POINT ( 'NONE',  ( 0.9873396505805591694, 0.1113553986120547346, 0.4379921258767252024 ) ) ;
#24589 = ORIENTED_EDGE ( 'NONE', *, *, #18454, .F. ) ;
#24590 = CARTESIAN_POINT ( 'NONE',  ( 0.7646288533564489232, -0.1113553986120547346, 0.5068897637795275468 ) ) ;
#24591 = CARTESIAN_POINT ( 'NONE',  ( 0.9500414927467378812, 0.1787899950787401604, 0.4675196849856070869 ) ) ;
#24592 = ORIENTED_EDGE ( 'NONE', *, *, #11122, .F. ) ;
#24593 = CARTESIAN_POINT ( 'NONE',  ( 0.1264236179284866091, -1.644192913332062966, 0.1264236179284866091 ) ) ;
#24594 = CARTESIAN_POINT ( 'NONE',  ( -1.002407869896990045, -0.1264236179284866091, 0.9276574802611967652 ) ) ;
#24595 = CARTESIAN_POINT ( 'NONE',  ( -1.033464566929134687, -0.06523048226347956391, 0.04675196850393704279 ) ) ;
#24596 = ORIENTED_EDGE ( 'NONE', *, *, #14353, .F. ) ;
#24597 = CARTESIAN_POINT ( 'NONE',  ( -0.8019270111902716547, 0.1787899950787401604, 1.136811023568283119 ) ) ;
#24598 = CARTESIAN_POINT ( 'NONE',  ( -0.6971942568897637749, 2.189545951927499583E-17, 0.6766732282926929409 ) ) ;
#24599 = AXIS2_PLACEMENT_3D ( 'NONE', #33144, #14438, #3160 ) ;
#24600 = CARTESIAN_POINT ( 'NONE',  ( 0.006399490001471973451, 0.05645636337047107295, -0.1377922246562235109 ) ) ;
#24601 = CARTESIAN_POINT ( 'NONE',  ( -0.07405724077823318263, -0.6930373540560104129, -0.1787899950787401604 ) ) ;
#24602 = ORIENTED_EDGE ( 'NONE', *, *, #26648, .T. ) ;
#24603 = CARTESIAN_POINT ( 'NONE',  ( 0.1081428761283521750, -0.08956233663024114333, 0.09372579465688228584 ) ) ;
#24604 = FACE_OUTER_BOUND ( 'NONE', #9830, .T. ) ;
#24605 = ORIENTED_EDGE ( 'NONE', *, *, #20502, .F. ) ;
#24606 = CARTESIAN_POINT ( 'NONE',  ( -0.7646288533564489232, -0.1113553986120547346, 1.727362204724409489 ) ) ;
#24607 = AXIS2_PLACEMENT_3D ( 'NONE', #43758, #11420, #25332 ) ;
#24608 = AXIS2_PLACEMENT_3D ( 'NONE', #7438, #40482, #235 ) ;
#24610 = DIRECTION ( 'NONE',  ( 1.822029033848725028E-16, 0.000000000000000000, 1.000000000000000000 ) ) ;
#24609 = AXIS2_PLACEMENT_3D ( 'NONE', #32727, #47072, #10673 ) ;
#24611 = CARTESIAN_POINT ( 'NONE',  ( -0.8759842519685039353, -0.1787899950787401882, 0.6028543306548976854 ) ) ;
#24612 = FACE_OUTER_BOUND ( 'NONE', #22936, .T. ) ;
#24613 = ORIENTED_EDGE ( 'NONE', *, *, #23644, .F. ) ;
#24614 = CARTESIAN_POINT ( 'NONE',  ( -0.8759842519685039353, 0.1787899950787401882, 1.690452755851748146 ) ) ;
#24615 = EDGE_CURVE ( 'NONE', #2057, #43422, #5625, .T. ) ;
#24616 = DIRECTION ( 'NONE',  ( -0.000000000000000000, 1.000000000000000000, -0.000000000000000000 ) ) ;
#24617 = ADVANCED_FACE ( 'NONE', ( #25993 ), #19262, .F. ) ;
#24618 = DIRECTION ( 'NONE',  ( 0.000000000000000000, 0.000000000000000000, 1.000000000000000000 ) ) ;
#24619 = ORIENTED_EDGE ( 'NONE', *, *, #37677, .F. ) ;
#24620 = CARTESIAN_POINT ( 'NONE',  ( 0.2471922904502826812, 0.09336655125506181097, 0.03811874944176495139 ) ) ;
#24621 = CARTESIAN_POINT ( 'NONE',  ( -1.033464566929133799, 0.000000000000000000, 1.377952755797984263 ) ) ;
#24622 = ADVANCED_FACE ( 'NONE', ( #37238 ), #34254, .T. ) ;
#24623 = CARTESIAN_POINT ( 'NONE',  ( 0.1113553986120547346, -0.5935039370078740717, -0.1113553986120547346 ) ) ;
#24624 = FACE_OUTER_BOUND ( 'NONE', #39883, .T. ) ;
#24625 = ADVANCED_FACE ( 'NONE', ( #9603 ), #1786, .T. ) ;
#24626 = CARTESIAN_POINT ( 'NONE',  ( -0.2559055118110235560, 0.04947374976879801572, -0.03739270108708937779 ) ) ;
#24627 = AXIS2_PLACEMENT_3D ( 'NONE', #42099, #37580, #19126 ) ;
#24628 = CARTESIAN_POINT ( 'NONE',  ( 0.7646288533564489232, -0.1113553986120547346, 1.215551181102362266 ) ) ;
#24630 = ( NAMED_UNIT ( * ) PLANE_ANGLE_UNIT ( ) SI_UNIT ( $, .RADIAN. ) ) ;
#24629 = CARTESIAN_POINT ( 'NONE',  ( -0.9412147342319837628, 0.1574803149606300301, 1.267224409341291436 ) ) ;
#24631 = CARTESIAN_POINT ( 'NONE',  ( 0.4736248074375590811, 1.209494567139730359, -1.479906699140348447 ) ) ;
#24632 = CIRCLE ( 'NONE', #122, 0.3937007874015748254 ) ;
#24634 = CARTESIAN_POINT ( 'NONE',  ( 1.033464566929134687, -0.06523048226347956391, 0.2731299211523157133 ) ) ;
#24633 = CARTESIAN_POINT ( 'NONE',  ( 0.8759842519685039353, 0.1787899950787401882, 0.6619094487651338010 ) ) ;
#24635 = CARTESIAN_POINT ( 'NONE',  ( -0.2066929133858267931, 0.5419727308409657551, -0.7545416139885203766 ) ) ;
#24636 = CARTESIAN_POINT ( 'NONE',  ( -0.3551574803149606385, 0.1574803149606299191, 1.928577636452523993E-17 ) ) ;
#24637 = ORIENTED_EDGE ( 'NONE', *, *, #46658, .F. ) ;
#24638 = CARTESIAN_POINT ( 'NONE',  ( -0.7646288533564489232, -0.1113553986120547346, 1.058070866141732402 ) ) ;
#24639 = CARTESIAN_POINT ( 'NONE',  ( 0.8759842519685039353, -0.1574803149606299191, 1.732283464566929165 ) ) ;
#24640 = VECTOR ( 'NONE', #18765, 39.37007874015748143 ) ;
#24642 = CARTESIAN_POINT ( 'NONE',  ( 0.1573498687646868455, 0.02697554138032596735, -0.1404067023994485797 ) ) ;
#24641 = VECTOR ( 'NONE', #36548, 39.37007874015748143 ) ;
#24643 = CARTESIAN_POINT ( 'NONE',  ( 0.6971942568897626646, -0.07405724077823297447, 0.7923228345919055560 ) ) ;
#24644 = ORIENTED_EDGE ( 'NONE', *, *, #46577, .F. ) ;
#24645 = CYLINDRICAL_SURFACE ( 'NONE', #11166, 0.1574803149606299191 ) ;
#24646 = CARTESIAN_POINT ( 'NONE',  ( -1.033464566929133799, 0.000000000000000000, 0.5216535433070865757 ) ) ;
#24647 = CARTESIAN_POINT ( 'NONE',  ( -1.100456976456230270E-17, 0.1072396549838836588, -0.1797182628040039365 ) ) ;
#24648 = CARTESIAN_POINT ( 'NONE',  ( -0.1264236179284866091, -0.9945866141194644738, -0.1264236179284866091 ) ) ;
#24649 = CARTESIAN_POINT ( 'NONE',  ( -9.642888182262618425E-18, -1.494094488188976388, -0.1574803149606299191 ) ) ;
#24650 = B_SPLINE_CURVE_WITH_KNOTS ( 'NONE', 3,
 ( #9563, #28024, #46428, #20795, #39237, #31385 ),
 .UNSPECIFIED., .F., .F.,
 ( 4, 2, 4 ),
 ( 0.000000000000000000, 0.5000000000000000000, 1.000000000000000000 ),
 .UNSPECIFIED. ) ;
#24651 = CARTESIAN_POINT ( 'NONE',  ( 0.9412147342319837628, 0.1574803149606300301, 1.267224409341291436 ) ) ;
#24652 = CARTESIAN_POINT ( 'NONE',  ( 0.1574803149606300023, -0.4812165006432428394, -0.8611016091043821596 ) ) ;
#24653 = CARTESIAN_POINT ( 'NONE',  ( -1.002407869896990045, -0.1264236179284866091, 1.911909448765133801 ) ) ;
#24654 = ORIENTED_EDGE ( 'NONE', *, *, #21706, .T. ) ;
#24655 = LINE ( 'NONE', #16989, #34407 ) ;
#24656 = ORIENTED_EDGE ( 'NONE', *, *, #33754, .F. ) ;
#24657 = CARTESIAN_POINT ( 'NONE',  ( -1.054774247047244540, 0.07405724077823318263, 1.958661417269071947 ) ) ;
#24658 = CARTESIAN_POINT ( 'NONE',  ( -1.054774247047244540, -0.07405724077823318263, 1.555118110182455382 ) ) ;
#24659 = CARTESIAN_POINT ( 'NONE',  ( 0.8759842519685039353, 0.1787899950787401882, 0.8636811023084409733 ) ) ;
#24660 = CARTESIAN_POINT ( 'NONE',  ( -0.7495606340400177148, -0.1264236179284866091, 1.031003936954110189 ) ) ;
#24661 = CARTESIAN_POINT ( 'NONE',  ( -0.9500414927467378812, -0.1787899950787401604, 0.1771653542769452139 ) ) ;
#24662 = CARTESIAN_POINT ( 'NONE',  ( -0.7646288533564489232, -0.1113553986120547346, 1.796259842412157415 ) ) ;
#24663 = CARTESIAN_POINT ( 'NONE',  ( -0.6971942568897648851, 0.07405724077823318263, 1.855314960576157635 ) ) ;
#24664 = CARTESIAN_POINT ( 'NONE',  ( -0.9412147342319837628, 0.1574803149606300301, 1.828248031496063630 ) ) ;
#24665 = CARTESIAN_POINT ( 'NONE',  ( 0.2559054646112969289, 0.04956735787872018628, -0.03742695103908252191 ) ) ;
#24666 = CARTESIAN_POINT ( 'NONE',  ( 0.4736248074375574713, 1.975221432870720495, -0.9622519263226653186 ) ) ;
#24667 = AXIS2_PLACEMENT_3D ( 'NONE', #10614, #43885, #29342 ) ;
#24668 = DIMENSIONAL_EXPONENTS ( 1.000000000000000000, 0.000000000000000000, 0.000000000000000000, 0.000000000000000000, 0.000000000000000000, 0.000000000000000000, 0.000000000000000000 ) ;
#24669 = CARTESIAN_POINT ( 'NONE',  ( -1.054774247047244540, 0.07405724077823318263, 0.1033464566391498751 ) ) ;
#24670 = ORIENTED_EDGE ( 'NONE', *, *, #483, .T. ) ;
#24671 = CARTESIAN_POINT ( 'NONE',  ( -1.054774247047244096, 0.000000000000000000, 1.247539370024976391 ) ) ;
#24672 = ORIENTED_EDGE ( 'NONE', *, *, #40190, .T. ) ;
#24673 = AXIS2_PLACEMENT_3D ( 'NONE', #26928, #12066, #8446 ) ;
#24674 = AXIS2_PLACEMENT_3D ( 'NONE', #4101, #3645, #26 ) ;
#24675 = CARTESIAN_POINT ( 'NONE',  ( -0.1264236179284866091, -1.112696850339937038, -0.1264236179284866091 ) ) ;
#24676 = CARTESIAN_POINT ( 'NONE',  ( -0.07405724077823318263, -1.174212598371433769, 0.1787899950787401604 ) ) ;
#24677 = EDGE_CURVE ( 'NONE', #23265, #18385, #44617, .T. ) ;
#24678 = CARTESIAN_POINT ( 'NONE',  ( -0.9873396505805591694, 0.1113553986120547346, 1.540354330601133803 ) ) ;
#24679 = CARTESIAN_POINT ( 'NONE',  ( 0.1797182628040039087, -0.5694335733625731644, -0.07444174185955065859 ) ) ;
#24680 = CARTESIAN_POINT ( 'NONE',  ( -0.8759842519685039353, -0.1574803149606299191, 0.2362204724409449064 ) ) ;
#24681 = CARTESIAN_POINT ( 'NONE',  ( -0.9873396505805591694, 0.1113553986120547346, 0.8021653543307086798 ) ) ;
#24682 = CARTESIAN_POINT ( 'NONE',  ( 0.1574803149606300301, -0.2071850393700788440, 0.06523048226347956391 ) ) ;
#24683 = CARTESIAN_POINT ( 'NONE',  ( 0.7185039370078746268, -0.06523048226347956391, 1.872539369971213841 ) ) ;
#24684 = EDGE_CURVE ( 'NONE', #36924, #43976, #974, .T. ) ;
#24685 = CARTESIAN_POINT ( 'NONE',  ( 1.033464566929134687, -0.06523048226347956391, 0.7947834645669291653 ) ) ;
#24686 = CARTESIAN_POINT ( 'NONE',  ( -0.1113553986120547346, -0.07185039370078739884, -0.1113553986120547346 ) ) ;
#24688 = CARTESIAN_POINT ( 'NONE',  ( 0.1592537043533306107, -0.1452344447278721418, -0.02937400284930944891 ) ) ;
#24687 = DIRECTION ( 'NONE',  ( 0.000000000000000000, 1.000000000000000000, 0.000000000000000000 ) ) ;
#24689 = CARTESIAN_POINT ( 'NONE',  ( 0.9412147342319837628, -0.1574803149606297803, 0.1500984250893234451 ) ) ;
#24690 = CARTESIAN_POINT ( 'NONE',  ( -0.8759842519685039353, 0.1574803149606299191, 1.584645669183810890 ) ) ;
#24691 = CARTESIAN_POINT ( 'NONE',  ( -0.8759842519685039353, -0.1574803149606299191, 1.181102362204724310 ) ) ;
#24692 = CARTESIAN_POINT ( 'NONE',  ( 0.1787899950787401604, -0.5787401574265509385, 0.07405724077823318263 ) ) ;
#24693 = CARTESIAN_POINT ( 'NONE',  ( 0.06523048226347956391, -1.024114173228346525, -0.1574803149606300301 ) ) ;
#24694 = VECTOR ( 'NONE', #17571, 39.37007874015748143 ) ;
#24695 = CARTESIAN_POINT ( 'NONE',  ( -0.6971942568897637749, 2.189545951927499583E-17, 1.931594488135212728 ) ) ;
#24696 = ORIENTED_EDGE ( 'NONE', *, *, #37545, .T. ) ;
#24697 = CARTESIAN_POINT ( 'NONE',  ( -0.6971942568897648851, -0.07405724077823297447, 1.466535433017102763 ) ) ;
#24698 = CARTESIAN_POINT ( 'NONE',  ( 0.8019270111902717657, 0.1787899950787401604, 1.535433070812378675 ) ) ;
#24699 = DIRECTION ( 'NONE',  ( 0.000000000000000000, -1.000000000000000000, 0.000000000000000000 ) ) ;
#24700 = CARTESIAN_POINT ( 'NONE',  ( -0.8759842519685039353, 0.1787899950787401882, 0.5880905511273386566 ) ) ;
#24701 = CARTESIAN_POINT ( 'NONE',  ( 0.1519290731529907845, -0.09842257466124233745, -0.09437017930498711737 ) ) ;
#24702 = CARTESIAN_POINT ( 'NONE',  ( 1.033464566929133799, 0.000000000000000000, 0.9153543307086614567 ) ) ;
#24703 = CARTESIAN_POINT ( 'NONE',  ( 1.054774247047244540, 0.07405724077823318263, 0.7775590550643457499 ) ) ;
#24704 = CARTESIAN_POINT ( 'NONE',  ( -0.9500414927467377701, 0.1787899950787401604, 0.6200787401037166635 ) ) ;
#24705 = EDGE_CURVE ( 'NONE', #37245, #35268, #17251, .T. ) ;
#24706 = CARTESIAN_POINT ( 'NONE',  ( -0.1377952755905511584, 0.1564960629921283985, 0.7066929133858274037 ) ) ;
#24707 = ORIENTED_EDGE ( 'NONE', *, *, #18298, .T. ) ;
#24708 = CARTESIAN_POINT ( 'NONE',  ( 0.1574803149606300301, -0.1924212597349927445, -0.06523048226347956391 ) ) ;
#24709 = CARTESIAN_POINT ( 'NONE',  ( -0.6971942568897648851, 0.07405724077823318263, 1.461614173174583753 ) ) ;
#24710 = ORIENTED_EDGE ( 'NONE', *, *, #25397, .T. ) ;
#24711 = CARTESIAN_POINT ( 'NONE',  ( -0.8759842519685039353, -0.1574803149606299191, 1.496062992125984259 ) ) ;
#24712 = AXIS2_PLACEMENT_3D ( 'NONE', #38776, #10501, #5935 ) ;
#24713 = CARTESIAN_POINT ( 'NONE',  ( -0.7185039370078746268, -0.06523048226347956391, 0.4256889763779528324 ) ) ;
#24714 = CARTESIAN_POINT ( 'NONE',  ( 0.6971942568897648851, 0.07405724077823318263, 1.304133858213953667 ) ) ;
#24715 = CARTESIAN_POINT ( 'NONE',  ( -0.1598647906827895537, -0.09851385182058956802, 0.1688384727535816865 ) ) ;
#24716 = VERTEX_POINT ( 'NONE', #28288 ) ;
#24717 = LINE ( 'NONE', #2659, #27918 ) ;
#24718 = CARTESIAN_POINT ( 'NONE',  ( -0.1787899950787401882, -1.669907432796167601, 0.000000000000000000 ) ) ;
#24719 = ORIENTED_EDGE ( 'NONE', *, *, #12733, .T. ) ;
#24720 = CARTESIAN_POINT ( 'NONE',  ( -0.07405724077823318263, -0.5590551180564723444, -0.1787899950787401604 ) ) ;
#24721 = FACE_OUTER_BOUND ( 'NONE', #19129, .T. ) ;
#24722 = ORIENTED_EDGE ( 'NONE', *, *, #16679, .F. ) ;
#24723 = CARTESIAN_POINT ( 'NONE',  ( 0.6971942568897648851, -0.07405724077823297447, 1.422244094434426120 ) ) ;
#24724 = EDGE_CURVE ( 'NONE', #46256, #32405, #5983, .T. ) ;
#24725 = CARTESIAN_POINT ( 'NONE',  ( -1.033464566929134687, -0.06523048226347956391, 1.149114173228346969 ) ) ;
#24726 = CARTESIAN_POINT ( 'NONE',  ( -0.1264236179284866091, -0.7534448818360000022, -0.1264236179284866091 ) ) ;
#24727 = EDGE_CURVE ( 'NONE', #18058, #5079, #39043, .T. ) ;
#24728 = DIRECTION ( 'NONE',  ( 1.000000000000000000, -0.000000000000000000, -0.000000000000000000 ) ) ;
#24729 = DIRECTION ( 'NONE',  ( 0.000000000000000000, 0.000000000000000000, -1.000000000000000000 ) ) ;
#24730 = DIRECTION ( 'NONE',  ( 0.000000000000000000, 0.000000000000000000, -1.000000000000000000 ) ) ;
#24731 = AXIS2_PLACEMENT_3D ( 'NONE', #4012, #15067, #33291 ) ;
#24732 = CARTESIAN_POINT ( 'NONE',  ( 0.1787899950787401604, -0.03850979500089227181, 0.07405724077823318263 ) ) ;
#24733 = CARTESIAN_POINT ( 'NONE',  ( 3.284318927891251994E-17, 0.004429133912031243958, 0.1787899950787401882 ) ) ;
#24734 = CARTESIAN_POINT ( 'NONE',  ( 0.1574803149606299191, 0.000000000000000000, -0.1183602362204724257 ) ) ;
#24735 = CARTESIAN_POINT ( 'NONE',  ( -0.7646288533564489232, -0.1113553986120547346, 1.481299212490897466 ) ) ;
#24736 = CARTESIAN_POINT ( 'NONE',  ( 0.6971942568897626646, -0.07405724077823297447, 0.5954724408911187261 ) ) ;
#24737 = ( BOUNDED_CURVE ( )  B_SPLINE_CURVE ( 2, ( #13249, #37932, #45557, #23779, #9408, #4843, #5320, #27878, #19707 ),
 .UNSPECIFIED., .F., .T. ) 
 B_SPLINE_CURVE_WITH_KNOTS ( ( 3, 2, 2, 2, 3 ),
 ( 0.6800000000000000488, 0.6824999999999999956, 0.6850000000000000533, 0.6875000000000000000, 0.6899999999999999467 ),
 .UNSPECIFIED. ) 
 CURVE ( )  GEOMETRIC_REPRESENTATION_ITEM ( )  RATIONAL_B_SPLINE_CURVE ( ( 1.000000000000000000, 0.9238795325112869605, 1.000000000000000000, 0.9238795325112869605, 1.000000000000000000, 0.9238795325112869605, 1.000000000000000000, 0.9238795325112799661, 1.000000000000000000 ) ) 
 REPRESENTATION_ITEM ( '' )  ) ;
#24738 = CARTESIAN_POINT ( 'NONE',  ( -0.8759842519685039353, 0.1787899950787401882, 0.9424212597887559051 ) ) ;
#24740 = CARTESIAN_POINT ( 'NONE',  ( 0.5839895013123354017, 4.616380251121755931E-17, 0.000000000000000000 ) ) ;
#24739 = CARTESIAN_POINT ( 'NONE',  ( -0.06523048226347956391, -0.8863188976377954775, 0.1574803149606297803 ) ) ;
#24741 = CARTESIAN_POINT ( 'NONE',  ( 0.1797182628040039365, -1.752996565488557090, -2.200913952912460540E-17 ) ) ;
#24742 = CARTESIAN_POINT ( 'NONE',  ( 0.06523048226347956391, -0.5024606298137324067, -0.1574803149606300301 ) ) ;
#24743 = CARTESIAN_POINT ( 'NONE',  ( -0.7185039370078766252, -0.06523048226348168721, 1.242618110128693276 ) ) ;
#24744 = CARTESIAN_POINT ( 'NONE',  ( 0.8019270111902717657, -0.1787899950787401604, 1.628937007820252303 ) ) ;
#24746 = LINE ( 'NONE', #42926, #37670 ) ;
#24745 = CARTESIAN_POINT ( 'NONE',  ( 0.8759842519685039353, -0.1787899950787401882, 1.980807086560409491 ) ) ;
#24747 = CARTESIAN_POINT ( 'NONE',  ( 0.8019270111902716547, -0.1787899950787401604, 0.5216535432533228045 ) ) ;
#24748 = ORIENTED_EDGE ( 'NONE', *, *, #3903, .T. ) ;
#24749 = CARTESIAN_POINT ( 'NONE',  ( -0.2020936974011077469, -0.07057211410350064384, -0.1687521643629676660 ) ) ;
#24750 = CARTESIAN_POINT ( 'NONE',  ( 0.9412147342319837628, 0.1574803149606300301, 0.01722440944881892255 ) ) ;
#24751 = CARTESIAN_POINT ( 'NONE',  ( 0.1387951811623661658, -0.2153607970560919849, -0.3149606299212599492 ) ) ;
#24752 = CARTESIAN_POINT ( 'NONE',  ( -0.1787899950787401882, -0.08415354325332302654, 0.000000000000000000 ) ) ;
#24753 = CARTESIAN_POINT ( 'NONE',  ( 0.7495606340400177148, 0.1264236179284866091, 0.5880905511273386566 ) ) ;
#24754 = CARTESIAN_POINT ( 'NONE',  ( 0.1264236179284866091, -0.9601377952218268508, -0.1264236179284866091 ) ) ;
#24755 = CARTESIAN_POINT ( 'NONE',  ( 1.002407869896990045, -0.1264236179284866091, 0.1402559054580474474 ) ) ;
#24756 = FACE_OUTER_BOUND ( 'NONE', #19689, .T. ) ;
#24757 = CARTESIAN_POINT ( 'NONE',  ( 0.8019270111902716547, 0.1787899950787401604, 0.5462598424659214080 ) ) ;
#24758 = CARTESIAN_POINT ( 'NONE',  ( 0.8759842519685039353, 0.1574803149606299191, 1.151574803042078710 ) ) ;
#24759 = ORIENTED_EDGE ( 'NONE', *, *, #12746, .F. ) ;
#24760 = CARTESIAN_POINT ( 'NONE',  ( 0.9873396505805591694, -0.1113553986120547346, 0.4379921259842519676 ) ) ;
#24761 = CARTESIAN_POINT ( 'NONE',  ( 0.8759842519685039353, -0.1787899950787401882, 1.119586614119464585 ) ) ;
#24762 = CARTESIAN_POINT ( 'NONE',  ( 0.1113553986120547346, -1.134842519577511810, -0.1113553986120547346 ) ) ;
#24763 = CARTESIAN_POINT ( 'NONE',  ( -1.033464566929133799, 0.000000000000000000, 0.6692913384751496553 ) ) ;
#24764 = CARTESIAN_POINT ( 'NONE',  ( 0.7185039370078746268, -0.06523048226347956391, 1.488681102362205300 ) ) ;
#24765 = CARTESIAN_POINT ( 'NONE',  ( 0.8759842519685039353, 0.1787899950787401882, 1.764271653489543290 ) ) ;
#24766 = CARTESIAN_POINT ( 'NONE',  ( -0.8107537697050253289, 0.1574803149606300301, 1.400098425196850904 ) ) ;
#24767 = CARTESIAN_POINT ( 'NONE',  ( -0.7495606340400177148, -0.1264236179284866091, 0.8735236219934803259 ) ) ;
#24768 = FACE_OUTER_BOUND ( 'NONE', #29676, .T. ) ;
#24769 = CARTESIAN_POINT ( 'NONE',  ( -0.8759842519685039353, -0.1574803149606299191, 0.03937007874015843040 ) ) ;
#24770 = CARTESIAN_POINT ( 'NONE',  ( 1.054774247047244540, 0.07405724077823318263, 0.3051181101824569919 ) ) ;
#24771 = CARTESIAN_POINT ( 'NONE',  ( 0.8107537697050253289, 0.1574803149606300301, 1.508366141624757129 ) ) ;
#24772 = ORIENTED_EDGE ( 'NONE', *, *, #24475, .T. ) ;
#24773 = CARTESIAN_POINT ( 'NONE',  ( -0.07405724077823318263, 0.02657480320336980464, -0.1787899950787401604 ) ) ;
#24774 = CARTESIAN_POINT ( 'NONE',  ( 0.2011713568916692896, -0.1793478952077613708, -0.05654496252297557674 ) ) ;
#24775 = CARTESIAN_POINT ( 'NONE',  ( 0.6971942568897626646, -0.07405724077823297447, 0.8366141731745828647 ) ) ;
#24776 = CARTESIAN_POINT ( 'NONE',  ( -0.7495606340400177148, -0.1264236179284866091, 1.700295275536787498 ) ) ;
#24777 = ORIENTED_EDGE ( 'NONE', *, *, #4362, .T. ) ;
#24778 = CARTESIAN_POINT ( 'NONE',  ( -0.2471922904502826812, 0.07821434602335945729, -0.07684457919973873563 ) ) ;
#24779 = DIRECTION ( 'NONE',  ( -0.000000000000000000, 1.000000000000000000, -0.000000000000000000 ) ) ;
#24780 = CARTESIAN_POINT ( 'NONE',  ( -0.1787899950787401882, -1.276206645394592609, 0.000000000000000000 ) ) ;
#24781 = ORIENTED_EDGE ( 'NONE', *, *, #37423, .F. ) ;
#24782 = CARTESIAN_POINT ( 'NONE',  ( 0.1787899950787401604, -0.06200787396198446239, 0.07405724077823318263 ) ) ;
#24783 = EDGE_CURVE ( 'NONE', #2328, #18450, #28596, .T. ) ;
#24784 = ORIENTED_EDGE ( 'NONE', *, *, #31995, .F. ) ;
#24785 = CARTESIAN_POINT ( 'NONE',  ( 0.001477421097679590357, -0.1327706367218486061, -0.04562747989148444039 ) ) ;
#24786 = CARTESIAN_POINT ( 'NONE',  ( -0.8107537697050254399, -0.1574803149606297803, 1.454232283464566677 ) ) ;
#24787 = EDGE_CURVE ( 'NONE', #27285, #1651, #15595, .T. ) ;
#24788 = CARTESIAN_POINT ( 'NONE',  ( 0.7495606340400177148, 0.1264236179284866091, 0.03690944876513417572 ) ) ;
#24789 = B_SPLINE_CURVE_WITH_KNOTS ( 'NONE', 3,
 ( #8842, #22746, #37352, #23238, #23479, #4505, #38080, #37599, #19141, #35209, #34974, #46199, #5483, #31619, #13398, #45718, #28028, #38788, #42587 ),
 .UNSPECIFIED., .F., .F.,
 ( 4, 1, 1, 1, 2, 2, 1, 1, 1, 1, 2, 2, 4 ),
 ( 0.000000000000000000, 0.1250000000000026645, 0.1875000000000038858, 0.2187500000000046074, 0.2343750000000049682, 0.2500000000000053291, 0.3750000000000067168, 0.4375000000000074385, 0.4687500000000076605, 0.4843750000000076605, 0.4921875000000074940, 0.5000000000000073275, 1.000000000000000000 ),
 .UNSPECIFIED. ) ;
#24790 = CARTESIAN_POINT ( 'NONE',  ( -0.1787899950787401604, -1.459645669237573884, 0.07405724077823318263 ) ) ;
#24791 = CARTESIAN_POINT ( 'NONE',  ( 0.07405724077823318263, -0.7657480314423001921, -0.1787899950787401604 ) ) ;
#24792 = EDGE_CURVE ( 'NONE', #41784, #46518, #37748, .T. ) ;
#24793 = CARTESIAN_POINT ( 'NONE',  ( -0.8759842519685039353, -0.1787899950787401882, 0.3715551180564728440 ) ) ;
#24794 = PRODUCT_DEFINITION ( 'UNKNOWN', '', #14795, #43194 ) ;
#24796 = CARTESIAN_POINT ( 'NONE',  ( -0.7226907848552633906, 0.05979789147634147206, 1.982109394411383230 ) ) ;
#24795 = CARTESIAN_POINT ( 'NONE',  ( -0.07444174185955065859, -1.253488691472810279, 0.1797182628040039087 ) ) ;
#24797 = CARTESIAN_POINT ( 'NONE',  ( -0.1993772601175057280, 0.1803837174632751672, -0.05517042925146035948 ) ) ;
#24798 = CARTESIAN_POINT ( 'NONE',  ( 0.7495606340400177148, 0.1264236179284866091, 1.183562992072220599 ) ) ;
#24799 = CARTESIAN_POINT ( 'NONE',  ( 0.6971942568897648851, -0.07405724077823297447, 1.540354330654897685 ) ) ;
#24801 = CARTESIAN_POINT ( 'NONE',  ( 0.9873396505805591694, -0.1113553986120547346, 1.530511810916094451 ) ) ;
#24800 = CARTESIAN_POINT ( 'NONE',  ( 0.1527643571647078757, -0.02877566944792483983, 0.1377952755905511861 ) ) ;
#24802 = DIRECTION ( 'NONE',  ( -1.000000000000000000, 0.000000000000000000, 0.000000000000000000 ) ) ;
#24803 = CARTESIAN_POINT ( 'NONE',  ( -0.8107537697050253289, 0.1574803149606300301, 1.665846456585386548 ) ) ;
#24804 = CARTESIAN_POINT ( 'NONE',  ( 0.8759842519685039353, 0.1787899950787401882, 0.2288385826234019815 ) ) ;
#24805 = CARTESIAN_POINT ( 'NONE',  ( 0.7012303660228902391, 0.004218421126415324365, 0.03936661617635339033 ) ) ;
#24807 = CARTESIAN_POINT ( 'NONE',  ( -0.9412147342319837628, 0.1574803149606300301, 1.946358267716537638 ) ) ;
#24806 = CARTESIAN_POINT ( 'NONE',  ( 0.6971942568897648851, -0.07405724077823297447, 1.107283464513165727 ) ) ;
#24808 = CARTESIAN_POINT ( 'NONE',  ( 0.8019270111902716547, -0.1787899950787401604, 1.904527559001354398 ) ) ;
#24809 = CARTESIAN_POINT ( 'NONE',  ( 0.7185039370078739607, 1.928577636452523993E-17, 0.5708661416247566844 ) ) ;
#24810 = ORIENTED_EDGE ( 'NONE', *, *, #44670, .F. ) ;
#24811 = FILL_AREA_STYLE ('',( #32740 ) ) ;
#24812 = CARTESIAN_POINT ( 'NONE',  ( 0.9403060794343187645, 0.1577454412895565594, 0.03936873803210047540 ) ) ;
#24813 = CARTESIAN_POINT ( 'NONE',  ( -0.7185039370078746268, 0.06523048226347956391, 0.3321850392625518844 ) ) ;
#24814 = ORIENTED_EDGE ( 'NONE', *, *, #24783, .T. ) ;
#24815 = CARTESIAN_POINT ( 'NONE',  ( 0.7495606340400177148, 0.1264236179284866091, 1.414862204670645829 ) ) ;
#24817 = CARTESIAN_POINT ( 'NONE',  ( -0.9412147342319837628, -0.1574803149606297803, 0.2288385825696384601 ) ) ;
#24816 = CARTESIAN_POINT ( 'NONE',  ( -0.8107537697050254399, 0.1574803149606300301, 1.636318897637794922 ) ) ;
#24818 = CARTESIAN_POINT ( 'NONE',  ( -0.1264236179284866091, 0.04379921265218866822, 0.1264236179284866091 ) ) ;
#24819 = ORIENTED_EDGE ( 'NONE', *, *, #40395, .T. ) ;
#24820 = CARTESIAN_POINT ( 'NONE',  ( 0.9412147342319837628, 0.1574803149606300301, 0.4404527557979849850 ) ) ;
#24821 = ORIENTED_EDGE ( 'NONE', *, *, #47127, .T. ) ;
#24822 = CYLINDRICAL_SURFACE ( 'NONE', #41266, 0.1574803149606299191 ) ;
#24823 = ( LENGTH_UNIT ( ) NAMED_UNIT ( * ) SI_UNIT ( $, .METRE. ) ) ;
#24824 = EDGE_LOOP ( 'NONE', ( #11292, #37537 ) ) ;
#24825 = CARTESIAN_POINT ( 'NONE',  ( 1.002407869896990045, 0.1264236179284866091, 0.6225393700249762796 ) ) ;
#24826 = ORIENTED_EDGE ( 'NONE', *, *, #47238, .T. ) ;
#24827 = CARTESIAN_POINT ( 'NONE',  ( -1.054774247047244096, 0.000000000000000000, 1.321358267662771757 ) ) ;
#24829 = CARTESIAN_POINT ( 'NONE',  ( -1.094772975963752103E-17, -1.629429133804503937, -0.1787899950787401882 ) ) ;
#24828 = CARTESIAN_POINT ( 'NONE',  ( -0.1574803149606299191, -0.4114173227271181177, 0.000000000000000000 ) ) ;
#24830 = CARTESIAN_POINT ( 'NONE',  ( -1.002407869896990045, -0.1264236179284866091, 1.203248031442299304 ) ) ;
#24831 = CARTESIAN_POINT ( 'NONE',  ( -0.8759842519685039353, 0.1787899950787401882, 1.961122047190330786 ) ) ;
#24832 = ORIENTED_EDGE ( 'NONE', *, *, #19906, .F. ) ;
#24833 = EDGE_CURVE ( 'NONE', #14468, #30794, #42626, .T. ) ;
#24834 = CARTESIAN_POINT ( 'NONE',  ( -1.054774247047244540, 0.07405724077823318263, 1.048228346402928723 ) ) ;
#24835 = CARTESIAN_POINT ( 'NONE',  ( -0.8759842519685039353, -0.1787899950787401882, 0.8439960629383622681 ) ) ;
#24836 = PLANE ( 'NONE',  #15763 ) ;
#24837 = VECTOR ( 'NONE', #45629, 39.37007874015748143 ) ;
#24838 = CARTESIAN_POINT ( 'NONE',  ( 0.004759645784635634091, 0.04840028875945810022, -0.1377938811595105506 ) ) ;
#24839 = CARTESIAN_POINT ( 'NONE',  ( 0.07405724077823318263, -0.7373286926386874995, -0.1787899950787401604 ) ) ;
#24840 = VERTEX_POINT ( 'NONE', #43345 ) ;
#24841 = CARTESIAN_POINT ( 'NONE',  ( -0.1574803149606297803, -0.01525590540428398145, 0.06523048226347956391 ) ) ;
#24842 = DIRECTION ( 'NONE',  ( 1.000000000000000000, 0.000000000000000000, 0.000000000000000000 ) ) ;
#24843 = EDGE_CURVE ( 'NONE', #18796, #6378, #14796, .T. ) ;
#24844 = VECTOR ( 'NONE', #26763, 39.37007874015748143 ) ;
#24845 = ORIENTED_EDGE ( 'NONE', *, *, #27252, .F. ) ;
#24846 = FACE_OUTER_BOUND ( 'NONE', #30023, .T. ) ;
#24847 = CARTESIAN_POINT ( 'NONE',  ( -0.7495606340400177148, 0.1264236179284866091, 0.7062007873478109987 ) ) ;
#24848 = CARTESIAN_POINT ( 'NONE',  ( 0.9412147342319837628, 0.1574803149606300301, 1.345964566821607589 ) ) ;
#24849 = ORIENTED_EDGE ( 'NONE', *, *, #22493, .F. ) ;
#24850 = CARTESIAN_POINT ( 'NONE',  ( -0.6971942568897637749, 2.189545951927499583E-17, 1.660925196796630088 ) ) ;
#24851 = CARTESIAN_POINT ( 'NONE',  ( -0.9412147342319837628, -0.1574803149606297803, 1.134350393593259732 ) ) ;
#24852 = ( BOUNDED_CURVE ( )  B_SPLINE_CURVE ( 2, ( #4538, #706, #16083, #23017, #23505, #38108, #15364, #19174, #30014 ),
 .UNSPECIFIED., .F., .T. ) 
 B_SPLINE_CURVE_WITH_KNOTS ( ( 3, 2, 2, 2, 3 ),
 ( 0.1199999999999999956, 0.1224999999999999978, 0.1250000000000000000, 0.1275000000000000022, 0.1300000000000000044 ),
 .UNSPECIFIED. ) 
 CURVE ( )  GEOMETRIC_REPRESENTATION_ITEM ( )  RATIONAL_B_SPLINE_CURVE ( ( 1.000000000000000000, 0.9238795325112869605, 1.000000000000000000, 0.9238795325112869605, 1.000000000000000000, 0.9238795325112869605, 1.000000000000000000, 0.9238795325112869605, 1.000000000000000000 ) ) 
 REPRESENTATION_ITEM ( '' )  ) ;
#24853 = CARTESIAN_POINT ( 'NONE',  ( -1.033464566929133799, 0.000000000000000000, 0.1181102361129454797 ) ) ;
#24854 = CARTESIAN_POINT ( 'NONE',  ( -0.1377952755905511861, 0.1564960629921283985, -0.8070866141732283561 ) ) ;
#24855 = VERTEX_POINT ( 'NONE', #6924 ) ;
#24856 = CARTESIAN_POINT ( 'NONE',  ( -1.100456976456230270E-17, -0.8376422347798956336, -0.1797182628040039365 ) ) ;
#24857 = CARTESIAN_POINT ( 'NONE',  ( 0.000000000000000000, 0.4666052258408023845, -0.7025346432751043979 ) ) ;
#24858 = CARTESIAN_POINT ( 'NONE',  ( 0.9500414927467378812, -0.1787899950787401604, 0.6889763778989935750 ) ) ;
#24859 = CARTESIAN_POINT ( 'NONE',  ( 0.1574803149606300301, -0.5615157480314956207, 0.06523048226347956391 ) ) ;
#24860 = CARTESIAN_POINT ( 'NONE',  ( -0.1406027654606837041, 0.1242474013968406649, -0.08019598169044524216 ) ) ;
#24861 = CYLINDRICAL_SURFACE ( 'NONE', #23857, 0.1574803149606299191 ) ;
#24862 = CARTESIAN_POINT ( 'NONE',  ( 1.033464566929134687, 0.06523048226347956391, 1.272145669291338432 ) ) ;
#24864 = CARTESIAN_POINT ( 'NONE',  ( -0.7185039370078739607, 1.928577636452523993E-17, 0.2559055117034968463 ) ) ;
#24863 = CARTESIAN_POINT ( 'NONE',  ( 0.7516165683754897353, -0.1160273600567148788, 1.985629433047727543 ) ) ;
#24865 = CARTESIAN_POINT ( 'NONE',  ( 0.2871444924769515628, 0.9382165298418956301, -1.070508272602716637 ) ) ;
#24866 = CARTESIAN_POINT ( 'NONE',  ( -9.642888182262618425E-18, -0.6181102361129449108, -0.1574803149606299191 ) ) ;
#24867 = CARTESIAN_POINT ( 'NONE',  ( 1.054774247047244096, 0.000000000000000000, 0.6520669290800944484 ) ) ;
#24868 = DIRECTION ( 'NONE',  ( 0.000000000000000000, 0.000000000000000000, -1.000000000000000000 ) ) ;
#24870 = AXIS2_PLACEMENT_3D ( 'NONE', #22294, #29778, #17993 ) ;
#24869 = CARTESIAN_POINT ( 'NONE',  ( 0.1787899950787401604, -0.6476377952218281830, -0.07405724077823318263 ) ) ;
#24871 = LINE ( 'NONE', #13846, #23087 ) ;
#24872 = VERTEX_POINT ( 'NONE', #17019 ) ;
#24873 = CARTESIAN_POINT ( 'NONE',  ( 0.5314960629921260393, 0.000000000000000000, 4.842519685039370358 ) ) ;
#24874 = B_SPLINE_CURVE_WITH_KNOTS ( 'NONE', 3,
 ( #9234, #27939, #9713, #30837, #23849, #31530, #42507, #24095, #5876, #46112, #24324, #45872, #23615, #38922, #30594, #38226, #12376, #38463, #16664 ),
 .UNSPECIFIED., .F., .F.,
 ( 4, 2, 2, 1, 2, 2, 2, 2, 2, 4 ),
 ( 0.000000000000000000, 0.2499999999999995559, 0.3749999999999995559, 0.4374999999999996669, 0.4687499999999996669, 0.4999999999999996669, 0.6249999999999996669, 0.6874999999999997780, 0.7499999999999998890, 1.000000000000000000 ),
 .UNSPECIFIED. ) ;
#24875 = VECTOR ( 'NONE', #25329, 39.37007874015748143 ) ;
#24876 = AXIS2_PLACEMENT_3D ( 'NONE', #20307, #45937, #6151 ) ;
#24877 = DIRECTION ( 'NONE',  ( 0.000000000000000000, 0.000000000000000000, 1.000000000000000000 ) ) ;
#24878 = CARTESIAN_POINT ( 'NONE',  ( 0.8759842519685039353, 0.1787899950787401882, 0.9768700786863937502 ) ) ;
#24879 = DIRECTION ( 'NONE',  ( -1.000000000000000000, 0.000000000000000000, 0.000000000000000000 ) ) ;
#24880 = CARTESIAN_POINT ( 'NONE',  ( 0.7646288533564489232, -0.1113553986120547346, 0.6938976376877481478 ) ) ;
#24881 = CARTESIAN_POINT ( 'NONE',  ( -0.1797182628040039087, 0.1146215447476630483, -0.07444174185955065859 ) ) ;
#24882 = CARTESIAN_POINT ( 'NONE',  ( 0.1787899950787401604, -1.046259842465921297, -0.07405724077823318263 ) ) ;
#24883 = CARTESIAN_POINT ( 'NONE',  ( -9.642888182262618425E-18, -1.533464566929133799, -0.1574803149606299191 ) ) ;
#24884 = ( BOUNDED_CURVE ( )  B_SPLINE_CURVE ( 2, ( #21264, #46660, #21499, #13843, #43780, #32793, #36134, #24634, #39232 ),
 .UNSPECIFIED., .F., .T. ) 
 B_SPLINE_CURVE_WITH_KNOTS ( ( 3, 2, 2, 2, 3 ),
 ( 0.1100000000000000006, 0.1125000000000000028, 0.1150000000000000050, 0.1174999999999999933, 0.1199999999999999956 ),
 .UNSPECIFIED. ) 
 CURVE ( )  GEOMETRIC_REPRESENTATION_ITEM ( )  RATIONAL_B_SPLINE_CURVE ( ( 1.000000000000000000, 0.9238795325112869605, 1.000000000000000000, 0.9238795325112869605, 1.000000000000000000, 0.9238795325112869605, 1.000000000000000000, 0.9238795325112869605, 1.000000000000000000 ) ) 
 REPRESENTATION_ITEM ( '' )  ) ;
#24885 = CARTESIAN_POINT ( 'NONE',  ( -0.8070866141732283561, 0.000000000000000000, 0.6590551181102368705 ) ) ;
#24886 = CARTESIAN_POINT ( 'NONE',  ( -0.6971942568897637749, 2.189545951927499583E-17, 0.1205708660879689087 ) ) ;
#24887 = ORIENTED_EDGE ( 'NONE', *, *, #22493, .T. ) ;
#24888 = ORIENTED_EDGE ( 'NONE', *, *, #31189, .F. ) ;
#24889 = CARTESIAN_POINT ( 'NONE',  ( 0.6971942568897648851, -0.07405724077823297447, 1.978346456639149320 ) ) ;
#24890 = VERTEX_POINT ( 'NONE', #6685 ) ;
#24891 = CARTESIAN_POINT ( 'NONE',  ( -0.6971942568897648851, 0.07405724077823318263, 1.894685039316315489 ) ) ;
#24892 = CARTESIAN_POINT ( 'NONE',  ( 1.002407869896990045, -0.1264236179284866091, 0.8489173227808819444 ) ) ;
#24893 = EDGE_CURVE ( 'NONE', #12346, #13468, #33985, .T. ) ;
#24894 = CARTESIAN_POINT ( 'NONE',  ( -1.054774247047244540, 0.07405724077823318263, 1.087598425143086578 ) ) ;
#24895 = CARTESIAN_POINT ( 'NONE',  ( -1.002407869896990045, 0.1264236179284866091, 0.2288385826234019815 ) ) ;
#24896 = EDGE_CURVE ( 'NONE', #43422, #30077, #24224, .T. ) ;
#24897 = CARTESIAN_POINT ( 'NONE',  ( -0.2471922904502826535, 0.07794254751779101931, 0.07737183577689189795 ) ) ;
#24898 = CARTESIAN_POINT ( 'NONE',  ( -0.8019270111902717657, 0.1787899950787401604, 1.889763779473794258 ) ) ;
#24899 = CARTESIAN_POINT ( 'NONE',  ( -1.002407869896990045, -0.1264236179284866091, 0.1402559054580474474 ) ) ;
#24900 = CARTESIAN_POINT ( 'NONE',  ( 0.7646288533564489232, 0.1113553986120547346, 0.3001968503937008093 ) ) ;
#24901 = CARTESIAN_POINT ( 'NONE',  ( -0.9412147342319837628, 0.1574803149606300301, 1.906988188976377563 ) ) ;
#24902 = CARTESIAN_POINT ( 'NONE',  ( -0.8759842519685039353, -0.1574803149606299191, 1.889763779527559251 ) ) ;
#24903 = CARTESIAN_POINT ( 'NONE',  ( -0.1561257034333340399, -0.09842519685039370636, 0.06437166193198956554 ) ) ;
#24904 = CARTESIAN_POINT ( 'NONE',  ( 0.7185039370078739607, 1.928577636452523993E-17, 1.751968503829480106 ) ) ;
#24905 = CARTESIAN_POINT ( 'NONE',  ( -0.9873396505805591694, 0.1113553986120547346, 0.04429133847515007855 ) ) ;
#24906 = EDGE_CURVE ( 'NONE', #2197, #39408, #31656, .T. ) ;
#24907 = CIRCLE ( 'NONE', #4209, 0.2460629921259842590 ) ;
#24908 = EDGE_CURVE ( 'NONE', #829, #43186, #32605, .T. ) ;
#24909 = CARTESIAN_POINT ( 'NONE',  ( -1.054774247047244540, -0.07405724077823318263, 0.1771653542769450751 ) ) ;
#24910 = VECTOR ( 'NONE', #38042, 39.37007874015748854 ) ;
#24911 = ORIENTED_EDGE ( 'NONE', *, *, #40650, .F. ) ;
#24912 = AXIS2_PLACEMENT_3D ( 'NONE', #23732, #20590, #9354 ) ;
#24913 = CARTESIAN_POINT ( 'NONE',  ( -0.9500414927467377701, -0.1787899950787401604, 1.240157480261197875 ) ) ;
#24914 = ORIENTED_EDGE ( 'NONE', *, *, #5639, .T. ) ;
#24915 = AXIS2_PLACEMENT_3D ( 'NONE', #45341, #31231, #6029 ) ;
#24916 = CARTESIAN_POINT ( 'NONE',  ( -0.1787899950787401604, -1.184055118056472455, 0.07405724077823318263 ) ) ;
#24917 = CARTESIAN_POINT ( 'NONE',  ( -0.1787899950787401604, -1.459645669237573884, -0.07405724077823318263 ) ) ;
#24918 = CARTESIAN_POINT ( 'NONE',  ( -1.033464566929133799, 0.000000000000000000, 1.535433070758614127 ) ) ;
#24919 = CARTESIAN_POINT ( 'NONE',  ( 0.1377952755905511861, 0.1574803149606299191, -0.7066929133858274037 ) ) ;
#24920 = CARTESIAN_POINT ( 'NONE',  ( -0.8107537697050253289, -0.1574803149606297803, 0.9325787400499522262 ) ) ;
#24921 = CARTESIAN_POINT ( 'NONE',  ( -1.033464566929133799, 0.000000000000000000, 0.7578740157480314821 ) ) ;
#24922 = CARTESIAN_POINT ( 'NONE',  ( 0.1574803149606300301, -0.1235236220472441943, -0.06523048226347956391 ) ) ;
#24923 = CARTESIAN_POINT ( 'NONE',  ( 0.9412147342319837628, 0.1574803149606300301, 1.818405511703498068 ) ) ;
#24924 = CARTESIAN_POINT ( 'NONE',  ( -0.1476377952755905387, 0.05639690512153997665, -0.1570009270184610506 ) ) ;
#24925 = CARTESIAN_POINT ( 'NONE',  ( 0.9412147342319837628, 0.1574803149606300301, 0.7258858267716535861 ) ) ;
#24926 = DIRECTION ( 'NONE',  ( 3.469446951953620894E-15, 1.000000000000000000, 0.000000000000000000 ) ) ;
#24927 = CARTESIAN_POINT ( 'NONE',  ( -0.7185039370078739607, 1.928577636452523993E-17, 1.092519685039370136 ) ) ;
#24929 = CARTESIAN_POINT ( 'NONE',  ( 0.1619907858920943411, -0.1553500912767243614, -0.01195870310697006757 ) ) ;
#24928 = CARTESIAN_POINT ( 'NONE',  ( 0.1377952755905511861, -1.365923996832131609E-16, -0.7066929133858274037 ) ) ;
#24930 = CARTESIAN_POINT ( 'NONE',  ( 1.033464566929134687, 0.06523048226347956391, 0.2386811022546777294 ) ) ;
#24931 = ORIENTED_EDGE ( 'NONE', *, *, #35715, .F. ) ;
#24933 = CARTESIAN_POINT ( 'NONE',  ( -0.1264236179284866091, -0.04478346451316559534, -0.1264236179284866091 ) ) ;
#24932 = AXIS2_PLACEMENT_3D ( 'NONE', #11218, #43544, #47396 ) ;
#24934 = CARTESIAN_POINT ( 'NONE',  ( -1.033464566929133799, 0.000000000000000000, 0.6299212597349921339 ) ) ;
#24935 = CARTESIAN_POINT ( 'NONE',  ( 0.06523048226347956391, -1.462106299105069951, 0.1574803149606297803 ) ) ;
#24936 = CARTESIAN_POINT ( 'NONE',  ( 0.1787899950787401604, -0.5344488188438744070, -0.07405724077823318263 ) ) ;
#24937 = CARTESIAN_POINT ( 'NONE',  ( -0.1574803149606300301, -1.093011811023621993, -0.06523048226347956391 ) ) ;
#24938 = CARTESIAN_POINT ( 'NONE',  ( 0.7185039370078739607, 1.928577636452523993E-17, 0.9645669290263307882 ) ) ;
#24939 = CARTESIAN_POINT ( 'NONE',  ( 0.1574803149606299191, 0.4003652867858621955, 0.7276473417831970103 ) ) ;
#24940 = CARTESIAN_POINT ( 'NONE',  ( -0.8019270111902717657, -0.1787899950787401604, 0.4429133857730075952 ) ) ;
#24941 = EDGE_LOOP ( 'NONE', ( #20060, #43411, #10396, #31603 ) ) ;
#24942 = CARTESIAN_POINT ( 'NONE',  ( -0.7495606340400177148, -0.1264236179284866091, 1.587106299158834721 ) ) ;
#24943 = CARTESIAN_POINT ( 'NONE',  ( 0.7495606340400177148, -0.1264236179284866091, 1.508366141678519678 ) ) ;
#24944 = AXIS2_PLACEMENT_3D ( 'NONE', #43288, #32054, #6391 ) ;
#24946 = CARTESIAN_POINT ( 'NONE',  ( -1.033464566929133799, 0.000000000000000000, 0.4822834645669291653 ) ) ;
#24945 = VECTOR ( 'NONE', #28402, 39.37007874015748143 ) ;
#24947 = CARTESIAN_POINT ( 'NONE',  ( -0.9500414927467378812, 0.1787899950787401604, 0.6643700786863929730 ) ) ;
#24948 = FACE_OUTER_BOUND ( 'NONE', #12013, .T. ) ;
#24949 = CARTESIAN_POINT ( 'NONE',  ( -0.8019270111902716547, -0.1787899950787401604, 0.7185039369541108556 ) ) ;
#24950 = CARTESIAN_POINT ( 'NONE',  ( 0.6195511811023624027, 0.9842519685039370358, -0.8759842519685050455 ) ) ;
#24951 = ADVANCED_FACE ( 'NONE', ( #13651 ), #20603, .F. ) ;
#24952 = CARTESIAN_POINT ( 'NONE',  ( 0.1574803149606299191, -0.2342519683964098265, -1.928577636452523993E-17 ) ) ;
#24953 = CARTESIAN_POINT ( 'NONE',  ( -0.6971942568897648851, 0.07405724077823318263, 1.382874015694268044 ) ) ;
#24954 = ORIENTED_EDGE ( 'NONE', *, *, #28058, .T. ) ;
#24955 = CARTESIAN_POINT ( 'NONE',  ( -0.9412147342319837628, 0.1574803149606300301, 0.4502952755905510474 ) ) ;
#24956 = CARTESIAN_POINT ( 'NONE',  ( 1.054774247047244540, 0.07405724077823318263, 1.368110236166710125 ) ) ;
#24957 = CARTESIAN_POINT ( 'NONE',  ( -0.1699452736636291317, -0.09851383556842245592, 0.02540171885215976658 ) ) ;
#24958 = CARTESIAN_POINT ( 'NONE',  ( -1.033464566929133799, 0.000000000000000000, 1.584645669291338654 ) ) ;
#24959 = ORIENTED_EDGE ( 'NONE', *, *, #37372, .T. ) ;
#24960 = ADVANCED_FACE ( 'NONE', ( #43578 ), #14067, .T. ) ;
#24961 = CARTESIAN_POINT ( 'NONE',  ( -0.07405724077823318263, -1.756029480040262269, -0.1787899950787401604 ) ) ;
#24962 = ORIENTED_EDGE ( 'NONE', *, *, #15700, .F. ) ;
#24963 = CARTESIAN_POINT ( 'NONE',  ( -0.8759842519685039353, 0.000000000000000000, 0.000000000000000000 ) ) ;
#24964 = ORIENTED_EDGE ( 'NONE', *, *, #34067, .T. ) ;
#24965 = CIRCLE ( 'NONE', #23437, 0.1003937007874010356 ) ;
#24966 = DIRECTION ( 'NONE',  ( -1.000000000000000000, 0.000000000000000000, 0.000000000000000000 ) ) ;
#24967 = CARTESIAN_POINT ( 'NONE',  ( -0.1787899950787401882, -0.3203740156942680994, 0.000000000000000000 ) ) ;
#24968 = CARTESIAN_POINT ( 'NONE',  ( -0.1264236179284866091, -0.8617125983714329918, 0.1264236179284866091 ) ) ;
#24969 = DIRECTION ( 'NONE',  ( 0.000000000000000000, 0.000000000000000000, -1.000000000000000000 ) ) ;
#24970 = CARTESIAN_POINT ( 'NONE',  ( 0.1636096891710253631, -0.1608575822371333675, 1.015068312943880306E-08 ) ) ;
#24971 = CARTESIAN_POINT ( 'NONE',  ( 1.054774247047244096, 0.000000000000000000, 0.2583661416785200671 ) ) ;
#24972 = CARTESIAN_POINT ( 'NONE',  ( 0.07405724077823318263, -0.1074074327961678510, -0.1787899950787401604 ) ) ;
#24973 = CARTESIAN_POINT ( 'NONE',  ( -1.094772975963752103E-17, -0.2859251967966303098, -0.1787899950787401882 ) ) ;
#24974 = CARTESIAN_POINT ( 'NONE',  ( 0.1264236179284866091, 0.04872047249470835839, 0.1264236179284866091 ) ) ;
#24975 = CARTESIAN_POINT ( 'NONE',  ( 0.3547871005709968273, 0.09842519685039370636, 0.000000000000000000 ) ) ;
#24976 = CARTESIAN_POINT ( 'NONE',  ( 0.1574803149606299746, 0.08719492171395765157, -0.5641677032617172793 ) ) ;
#24977 = CARTESIAN_POINT ( 'NONE',  ( 1.002407869896990045, 0.1264236179284866091, 0.5782480314422993040 ) ) ;
#24978 = CARTESIAN_POINT ( 'NONE',  ( -0.8759842519685039353, 0.1787899950787401882, 0.9030511810485984947 ) ) ;
#24980 = LINE ( 'NONE', #17783, #7820 ) ;
#24979 = CARTESIAN_POINT ( 'NONE',  ( -0.9999090329106934405, 0.1097224490248799866, 0.03937007874015842346 ) ) ;
#24981 = CARTESIAN_POINT ( 'NONE',  ( -0.1270800023317771588, -1.807130423756275972, 0.1270800023317771588 ) ) ;
#24982 = LINE ( 'NONE', #43407, #38410 ) ;
#24983 = CARTESIAN_POINT ( 'NONE',  ( 1.002407869896990045, -0.1264236179284866091, 1.596948818843874074 ) ) ;
#24985 = CARTESIAN_POINT ( 'NONE',  ( 0.1636882031745872657, 0.1609730488751321964, 5.008074394060701725E-08 ) ) ;
#24984 = CARTESIAN_POINT ( 'NONE',  ( -1.033464566929133799, 0.000000000000000000, 1.190944881889763884 ) ) ;
#24986 = EDGE_LOOP ( 'NONE', ( #13527, #11590, #31045, #5538, #25195, #29748 ) ) ;
#24988 = VERTEX_POINT ( 'NONE', #2617 ) ;
#24987 = CARTESIAN_POINT ( 'NONE',  ( -0.2278981769381095701, -0.05062618494087340465, -0.1538518510337364420 ) ) ;
#24989 = CARTESIAN_POINT ( 'NONE',  ( 1.033464566929133799, 0.000000000000000000, 0.7874015746956221085 ) ) ;
#24991 = CARTESIAN_POINT ( 'NONE',  ( -0.07405724077823318263, -0.1948818897100161873, 0.1787899950787401604 ) ) ;
#24990 = CARTESIAN_POINT ( 'NONE',  ( 0.06523048226347956391, -0.9109251967428659835, 0.1574803149606297803 ) ) ;
#24992 = CARTESIAN_POINT ( 'NONE',  ( 0.6971942568897637749, 2.189545951927499583E-17, 0.6323818897100157432 ) ) ;
#24993 = CARTESIAN_POINT ( 'NONE',  ( 0.1787899950787401604, -1.124999999946237228, 0.07405724077823318263 ) ) ;
#24994 = CARTESIAN_POINT ( 'NONE',  ( 0.6971942568897626646, 0.07405724077823318263, 0.08366141726907129483 ) ) ;
#24995 = CARTESIAN_POINT ( 'NONE',  ( -0.8759842519685039353, -0.1574803149606299191, 0.9350393699712126194 ) ) ;
#24996 = CARTESIAN_POINT ( 'NONE',  ( -0.6971942568897637749, 2.189545951927499583E-17, 1.537893700733637736 ) ) ;
#24997 = ORIENTED_EDGE ( 'NONE', *, *, #38625, .F. ) ;
#24998 = CARTESIAN_POINT ( 'NONE',  ( 0.9412147342319837628, -0.1574803149606297803, 0.1599409448818898405 ) ) ;
#24999 = CARTESIAN_POINT ( 'NONE',  ( 0.7495606340400177148, -0.1264236179284866091, 1.154035433017102319 ) ) ;
#25000 = CARTESIAN_POINT ( 'NONE',  ( -0.1113553986120547346, -1.124999999892472458, -0.1113553986120547346 ) ) ;
#25001 = CARTESIAN_POINT ( 'NONE',  ( -0.9873396505805591694, -0.1113553986120547346, 0.7037401573727875004 ) ) ;
#25002 = CARTESIAN_POINT ( 'NONE',  ( 0.7185039370078739607, 1.928577636452523993E-17, 1.397637795168062969 ) ) ;
#25003 = CARTESIAN_POINT ( 'NONE',  ( -0.8759842519685039353, 0.1787899950787401882, 0.9768700786863937502 ) ) ;
#25004 = DIRECTION ( 'NONE',  ( -1.000000000000000000, 0.000000000000000000, 0.000000000000000000 ) ) ;
#25005 = CARTESIAN_POINT ( 'NONE',  ( -0.7831748123774774362, -0.1359591512319747730, 0.03937007874015843734 ) ) ;
#25006 = CARTESIAN_POINT ( 'NONE',  ( 1.002407869896990045, -0.1264236179284866091, 0.2977362204186775885 ) ) ;
#25007 = CARTESIAN_POINT ( 'NONE',  ( -0.8019270111902716547, -0.1787899950787401604, 0.1673228345919057503 ) ) ;
#25008 = CARTESIAN_POINT ( 'NONE',  ( -0.8019270111902717657, -0.1787899950787401604, 0.6397637794737947026 ) ) ;
#25009 = CARTESIAN_POINT ( 'NONE',  ( 0.7185039370078739607, 1.928577636452523993E-17, 1.633858267609007875 ) ) ;
#25010 = ORIENTED_EDGE ( 'NONE', *, *, #36320, .F. ) ;
#25011 = ADVANCED_FACE ( 'NONE', ( #4484, #44054 ), #14602, .F. ) ;
#25012 = CARTESIAN_POINT ( 'NONE',  ( -0.1787899950787401604, -0.002952755851748290004, 0.07405724077823318263 ) ) ;
#25013 = CARTESIAN_POINT ( 'NONE',  ( 0.7495606340400177148, 0.1264236179284866091, 0.7504921259304880854 ) ) ;
#25014 = CARTESIAN_POINT ( 'NONE',  ( -0.7495606340400177148, -0.1264236179284866091, 1.779035433017102319 ) ) ;
#25015 = EDGE_CURVE ( 'NONE', #31651, #35175, #29508, .T. ) ;
#25016 = CARTESIAN_POINT ( 'NONE',  ( -0.2471922904502826257, 0.09572725253288318081, -0.02812286105090850558 ) ) ;
#25017 = CARTESIAN_POINT ( 'NONE',  ( 0.7646288533564489232, 0.1113553986120547346, 1.323818897637795367 ) ) ;
#25018 = CARTESIAN_POINT ( 'NONE',  ( 0.07405724077823318263, -1.288509795000891689, -0.1787899950787401604 ) ) ;
#25019 = ORIENTED_EDGE ( 'NONE', *, *, #3669, .T. ) ;
#25020 = CARTESIAN_POINT ( 'NONE',  ( -0.1787899950787401604, -0.2785433070328505734, -0.07405724077823318263 ) ) ;
#25021 = ORIENTED_EDGE ( 'NONE', *, *, #2007, .T. ) ;
#25022 = CARTESIAN_POINT ( 'NONE',  ( 1.054774247047244540, -0.07405724077823318263, 1.082677165300567346 ) ) ;
#25023 = CYLINDRICAL_SURFACE ( 'NONE', #6567, 0.5905511811023621549 ) ;
#25024 = CARTESIAN_POINT ( 'NONE',  ( -0.2471911249971451008, -0.08424752482805999976, 0.06442904123723289245 ) ) ;
#25025 = AXIS2_PLACEMENT_3D ( 'NONE', #11984, #27088, #30683 ) ;
#25026 = ( BOUNDED_CURVE ( )  B_SPLINE_CURVE ( 2, ( #34339, #1471, #40369, #27407, #12293, #14769, #5078, #43979, #26916 ),
 .UNSPECIFIED., .F., .F. ) 
 B_SPLINE_CURVE_WITH_KNOTS ( ( 3, 2, 2, 2, 3 ),
 ( 0.9899999999999999911, 0.9925000000000000488, 0.9949999999999999956, 0.9975000000000000533, 1.000000000000000000 ),
 .UNSPECIFIED. ) 
 CURVE ( )  GEOMETRIC_REPRESENTATION_ITEM ( )  RATIONAL_B_SPLINE_CURVE ( ( 1.000000000000000000, 0.9238795325112869605, 1.000000000000000000, 0.9238795325112869605, 1.000000000000000000, 0.9238795325112869605, 1.000000000000000000, 0.9238795325112869605, 1.000000000000000000 ) ) 
 REPRESENTATION_ITEM ( '' )  ) ;
#25027 = CARTESIAN_POINT ( 'NONE',  ( 0.8759842519685039353, -0.1787899950787401882, 0.05167322829269314910 ) ) ;
#25028 = CARTESIAN_POINT ( 'NONE',  ( -0.1264236179284866091, -1.654035433017102319, 0.1264236179284866091 ) ) ;
#25029 = EDGE_CURVE ( 'NONE', #15018, #22876, #7172, .T. ) ;
#25030 = CARTESIAN_POINT ( 'NONE',  ( -1.054774247047244540, -0.07405724077823318263, 0.4970472440407249226 ) ) ;
#25031 = CARTESIAN_POINT ( 'NONE',  ( 0.1555687797274982465, -0.1458529223346496095, 0.02296587926509184932 ) ) ;
#25032 = CARTESIAN_POINT ( 'NONE',  ( 1.002407869896990045, -0.1264236179284866091, 1.242618110182456714 ) ) ;
#25033 = CARTESIAN_POINT ( 'NONE',  ( 0.8019270111902716547, -0.1787899950787401604, 1.466535433017102763 ) ) ;
#25034 = CARTESIAN_POINT ( 'NONE',  ( -0.9412147342319837628, 0.1574803149606300301, 0.5979330707586145710 ) ) ;
#25035 = CARTESIAN_POINT ( 'NONE',  ( 0.7185039370078746268, 0.06523048226347956391, 1.680610236220472231 ) ) ;
#25036 = LINE ( 'NONE', #7302, #37312 ) ;
#25037 = CARTESIAN_POINT ( 'NONE',  ( 1.033464566929134687, 0.06523048226347956391, 0.6717519683964101596 ) ) ;
#25038 = CARTESIAN_POINT ( 'NONE',  ( -0.8107537697050253289, -0.1574803149606297803, 1.798720472333418918 ) ) ;
#25039 = CARTESIAN_POINT ( 'NONE',  ( 0.8759842519685039353, 0.1787899950787401882, 0.1500984251430870220 ) ) ;
#25041 = CARTESIAN_POINT ( 'NONE',  ( -0.3980944881889768028, 5.463695987328542214E-16, -0.7480314960629921295 ) ) ;
#25040 = CARTESIAN_POINT ( 'NONE',  ( 1.054774247047244540, 0.07405724077823318263, 1.126968503883244654 ) ) ;
#25042 = CARTESIAN_POINT ( 'NONE',  ( -1.033464566929134687, -0.06523048226347956391, 1.926673228238929170 ) ) ;
#25043 = CARTESIAN_POINT ( 'NONE',  ( -0.6971942568897648851, 0.07405724077823318263, 1.141732283410804349 ) ) ;
#25044 = CARTESIAN_POINT ( 'NONE',  ( 0.9412147342319837628, -0.1574803149606297803, 0.4256889762704256230 ) ) ;
#25045 = ORIENTED_EDGE ( 'NONE', *, *, #41432, .F. ) ;
#25046 = EDGE_CURVE ( 'NONE', #19692, #47237, #4253, .T. ) ;
#25047 = CARTESIAN_POINT ( 'NONE',  ( -1.033464566929133799, 0.000000000000000000, 1.112204724409448842 ) ) ;
#25048 = CARTESIAN_POINT ( 'NONE',  ( 0.8692927555521646754, 0.1747984728378554065, 0.03936921762936072822 ) ) ;
#25049 = CARTESIAN_POINT ( 'NONE',  ( 0.8759842519685039353, 0.1574803149606299191, 0.2952755905511810774 ) ) ;
#25050 = CARTESIAN_POINT ( 'NONE',  ( -0.7185039370078739607, 1.928577636452523993E-17, 0.4133858266641267654 ) ) ;
#25051 = EDGE_LOOP ( 'NONE', ( #3782, #7877, #2847, #13464 ) ) ;
#25052 = CARTESIAN_POINT ( 'NONE',  ( 0.8759842519685039353, 0.1787899950787401882, 1.528051181048598384 ) ) ;
#25054 = CARTESIAN_POINT ( 'NONE',  ( 0.3980944881889770803, 0.1864803149606326926, -0.7480314960629921295 ) ) ;
#25053 = CARTESIAN_POINT ( 'NONE',  ( -0.9873396505805591694, -0.1113553986120547346, 1.776574803149606252 ) ) ;
#25055 = CARTESIAN_POINT ( 'NONE',  ( 0.1264236179284866091, 0.02411417328210995956, -0.1264236179284866091 ) ) ;
#25056 = ORIENTED_EDGE ( 'NONE', *, *, #2146, .F. ) ;
#25057 = AXIS2_PLACEMENT_3D ( 'NONE', #31390, #32078, #45959 ) ;
#25058 = CARTESIAN_POINT ( 'NONE',  ( 0.8107537697050254399, 0.1574803149606300301, 0.4453740156405042727 ) ) ;
#25059 = ADVANCED_FACE ( 'NONE', ( #22729 ), #25402, .T. ) ;
#25060 = ORIENTED_EDGE ( 'NONE', *, *, #27158, .F. ) ;
#25061 = CARTESIAN_POINT ( 'NONE',  ( 1.033464566929133799, 1.928577636452524610E-17, 4.498031496062992574 ) ) ;
#25062 = CARTESIAN_POINT ( 'NONE',  ( 0.6971942568897626646, -0.07405724077823297447, 0.5216535432533228045 ) ) ;
#25063 = ORIENTED_EDGE ( 'NONE', *, *, #21097, .T. ) ;
#25064 = CARTESIAN_POINT ( 'NONE',  ( -0.1113553986120547346, 0.09547244105240886014, -0.1113553986120547346 ) ) ;
#25065 = CARTESIAN_POINT ( 'NONE',  ( -0.6971942568897648851, -0.07405724077823297447, 1.112204724355684959 ) ) ;
#25066 = CARTESIAN_POINT ( 'NONE',  ( -1.033464566929134687, 0.06523048226347956391, 0.09104330708661413640 ) ) ;
#25067 = ORIENTED_EDGE ( 'NONE', *, *, #43327, .T. ) ;
#25068 = CARTESIAN_POINT ( 'NONE',  ( -0.8759842519685039353, -0.1787899950787401882, 1.154035433017102319 ) ) ;
#25069 = EDGE_CURVE ( 'NONE', #31518, #5360, #44513, .T. ) ;
#25070 = CARTESIAN_POINT ( 'NONE',  ( -0.8759842519685039353, 0.1787899950787401882, 0.8243110235682834519 ) ) ;
#25071 = CARTESIAN_POINT ( 'NONE',  ( -0.9500414927467378812, 0.1787899950787401604, 0.1525590550643468046 ) ) ;
#25072 = CARTESIAN_POINT ( 'NONE',  ( 0.3161444924769527542, 1.025704337919492115, -1.138861239548320858 ) ) ;
#25073 = DIRECTION ( 'NONE',  ( 0.000000000000000000, 1.000000000000000000, 0.000000000000000000 ) ) ;
#25074 = CARTESIAN_POINT ( 'NONE',  ( -0.1787899950787401604, -0.8013050705914438465, 0.07405724077823318263 ) ) ;
#25075 = EDGE_LOOP ( 'NONE', ( #10895, #43105, #11023, #13641 ) ) ;
#25076 = CARTESIAN_POINT ( 'NONE',  ( -0.1589669047091706866, -0.08956155894763247194, 0.04881376169791724201 ) ) ;
#25077 = CARTESIAN_POINT ( 'NONE',  ( 0.6141732283464567121, 0.000000000000000000, 0.000000000000000000 ) ) ;
#25078 = ORIENTED_EDGE ( 'NONE', *, *, #18066, .F. ) ;
#25079 = LINE ( 'NONE', #36105, #17994 ) ;
#25080 = CARTESIAN_POINT ( 'NONE',  ( -0.2362204724409469048, 2.422684756221293634E-15, 1.186023622047244208 ) ) ;
#25081 = CARTESIAN_POINT ( 'NONE',  ( -0.6971942568897637749, 2.189545951927499583E-17, 0.5930118109698583329 ) ) ;
#25082 = CARTESIAN_POINT ( 'NONE',  ( 0.000000000000000000, 0.000000000000000000, 0.000000000000000000 ) ) ;
#25083 = ORIENTED_EDGE ( 'NONE', *, *, #36431, .T. ) ;
#25084 = CARTESIAN_POINT ( 'NONE',  ( -1.054774247047244540, 0.07405724077823318263, 1.801181102308441861 ) ) ;
#25085 = VERTEX_POINT ( 'NONE', #29734 ) ;
#25086 = CARTESIAN_POINT ( 'NONE',  ( -0.7185039370078746268, -0.06523048226347956391, 1.124507873908221267 ) ) ;
#25087 = CARTESIAN_POINT ( 'NONE',  ( -0.9500414927467377701, -0.1787899950787401604, 0.05905511805647267048 ) ) ;
#25088 = CARTESIAN_POINT ( 'NONE',  ( 1.033464566929133799, 0.000000000000000000, 0.6791338582677166613 ) ) ;
#25089 = CARTESIAN_POINT ( 'NONE',  ( 0.1270800023317771588, -0.8130359355672972521, 0.1270800023317771588 ) ) ;
#25090 = FACE_OUTER_BOUND ( 'NONE', #17998, .T. ) ;
#25091 = CARTESIAN_POINT ( 'NONE',  ( -0.8759842519685039353, -0.1574803149606299191, 1.446850393593259732 ) ) ;
#25092 = CARTESIAN_POINT ( 'NONE',  ( 1.054774247047244540, -0.07405724077823318263, 0.7332677164816707727 ) ) ;
#25093 = CARTESIAN_POINT ( 'NONE',  ( -0.1574803149606297803, -0.5762795275590550936, 0.06523048226347956391 ) ) ;
#25094 = CARTESIAN_POINT ( 'NONE',  ( -0.1456127326761254559, 0.1283478695987083085, 0.08092402698540318573 ) ) ;
#25095 = EDGE_CURVE ( 'NONE', #28102, #13381, #11253, .T. ) ;
#25096 = LINE ( 'NONE', #28971, #38388 ) ;
#25097 = CARTESIAN_POINT ( 'NONE',  ( 0.8107537697050253289, 0.1574803149606300301, 1.321358267716534751 ) ) ;
#25099 = FACE_OUTER_BOUND ( 'NONE', #17377, .T. ) ;
#25098 = CARTESIAN_POINT ( 'NONE',  ( 0.8230356807856350487, -0.1645567810599724290, 1.987220178087543143 ) ) ;
#25100 = CARTESIAN_POINT ( 'NONE',  ( 0.2395294000716133853, -0.1968503937007874127, 0.4921259842519685179 ) ) ;
#25101 = CARTESIAN_POINT ( 'NONE',  ( -0.1574803149606300301, -0.6107283463491653963, -0.06523048226347956391 ) ) ;
#25103 = DIRECTION ( 'NONE',  ( -0.5735764363510518216, -0.8191520442889876907, 0.000000000000000000 ) ) ;
#25102 = CARTESIAN_POINT ( 'NONE',  ( 0.9500414927467377701, 0.1787899950787401604, 0.6200787401037166635 ) ) ;
#25104 = CARTESIAN_POINT ( 'NONE',  ( -0.1264236179284866091, -0.6747047243556849594, -0.1264236179284866091 ) ) ;
#25105 = FACE_OUTER_BOUND ( 'NONE', #43929, .T. ) ;
#25106 = ORIENTED_EDGE ( 'NONE', *, *, #10694, .T. ) ;
#25107 = EDGE_CURVE ( 'NONE', #33534, #5993, #25637, .T. ) ;
#25108 = CYLINDRICAL_SURFACE ( 'NONE', #45934, 0.1574803149606299191 ) ;
#25109 = DIRECTION ( 'NONE',  ( 1.000000000000000000, 0.000000000000000000, 0.000000000000000000 ) ) ;
#25110 = CARTESIAN_POINT ( 'NONE',  ( 0.6971942568897637749, 2.189545951927499583E-17, 0.9473425196312755814 ) ) ;
#25111 = DIRECTION ( 'NONE',  ( -1.000000000000000000, -0.000000000000000000, -0.000000000000000000 ) ) ;
#25112 = CARTESIAN_POINT ( 'NONE',  ( -0.07444174185955065859, 0.04572390695238758712, 0.1797182628040039087 ) ) ;
#25113 = CARTESIAN_POINT ( 'NONE',  ( -0.1787899950787401882, -1.186515747977732183, 0.000000000000000000 ) ) ;
#25114 = CARTESIAN_POINT ( 'NONE',  ( -0.1574803149606300301, -1.565452755905512028, -0.06523048226347956391 ) ) ;
#25115 = DIRECTION ( 'NONE',  ( -0.6018150231520356108, -6.927058840138832622E-16, 0.7986355100473022661 ) ) ;
#25116 = VECTOR ( 'NONE', #1632, 39.37007874015748143 ) ;
#25117 = CARTESIAN_POINT ( 'NONE',  ( -1.002407869896990045, 0.1264236179284866091, 0.06643700782025216411 ) ) ;
#25118 = EDGE_LOOP ( 'NONE', ( #221, #36743, #10702, #35329 ) ) ;
#25119 = CARTESIAN_POINT ( 'NONE',  ( 0.9500414927467378812, -0.1787899950787401604, 1.988188976324187562 ) ) ;
#25120 = EDGE_LOOP ( 'NONE', ( #9593, #43569, #31733, #3135 ) ) ;
#25121 = CARTESIAN_POINT ( 'NONE',  ( -0.8759842519685039353, -0.1787899950787401882, 1.906988188922614125 ) ) ;
#25122 = CARTESIAN_POINT ( 'NONE',  ( -0.6971942568897637749, 2.189545951927499583E-17, 1.616633858213952779 ) ) ;
#25123 = CARTESIAN_POINT ( 'NONE',  ( 1.054774247047244540, 0.07405724077823318263, 0.8956692912848198684 ) ) ;
#25124 = AXIS2_PLACEMENT_3D ( 'NONE', #45973, #20580, #13412 ) ;
#25125 = CARTESIAN_POINT ( 'NONE',  ( -1.002407869896990045, -0.1264236179284866091, 0.4158464566391496531 ) ) ;
#25126 = CARTESIAN_POINT ( 'NONE',  ( -0.9873396505805591694, -0.1113553986120547346, 1.806102362097196767 ) ) ;
#25127 = CARTESIAN_POINT ( 'NONE',  ( -0.9500414927467378812, 0.1787899950787401604, 1.884842519631275026 ) ) ;
#25128 = CARTESIAN_POINT ( 'NONE',  ( 1.033464566929133799, 0.000000000000000000, 0.2854330708661417804 ) ) ;
#25129 = CARTESIAN_POINT ( 'NONE',  ( -0.8107537697050253289, 0.1574803149606300301, 1.911909448818899238 ) ) ;
#25130 = CARTESIAN_POINT ( 'NONE',  ( -0.9412147342319837628, -0.1574803149606297803, 1.892224409448819866 ) ) ;
#25131 = CARTESIAN_POINT ( 'NONE',  ( 3.284318927891251994E-17, -0.4002223934260890070, 0.1787899950787401882 ) ) ;
#25132 = CARTESIAN_POINT ( 'NONE',  ( -0.1735869313432972239, -0.09842519685039370636, -0.005721762985481354535 ) ) ;
#25133 = DIRECTION ( 'NONE',  ( 0.000000000000000000, 0.000000000000000000, 1.000000000000000000 ) ) ;
#25134 = CARTESIAN_POINT ( 'NONE',  ( -1.054774247047244540, -0.07405724077823318263, 0.09842519679663024046 ) ) ;
#25135 = ( BOUNDED_CURVE ( )  B_SPLINE_CURVE ( 2, ( #29345, #7702, #10617, #22316, #39807, #21622, #36255, #40043, #3407 ),
 .UNSPECIFIED., .F., .F. ) 
 B_SPLINE_CURVE_WITH_KNOTS ( ( 3, 2, 2, 2, 3 ),
 ( 0.8499999999999999778, 0.8525000000000000355, 0.8549999999999999822, 0.8575000000000000400, 0.8599999999999999867 ),
 .UNSPECIFIED. ) 
 CURVE ( )  GEOMETRIC_REPRESENTATION_ITEM ( )  RATIONAL_B_SPLINE_CURVE ( ( 1.000000000000000000, 0.9238795325112869605, 1.000000000000000000, 0.9238795325112869605, 1.000000000000000000, 0.9238795325112869605, 1.000000000000000000, 0.9238795325112869605, 1.000000000000000000 ) ) 
 REPRESENTATION_ITEM ( '' )  ) ;
#25136 = EDGE_LOOP ( 'NONE', ( #27573, #28332, #9633, #45277 ) ) ;
#25137 = ORIENTED_EDGE ( 'NONE', *, *, #5759, .F. ) ;
#25138 = CARTESIAN_POINT ( 'NONE',  ( -0.8019270111902716547, -0.1787899950787401604, 1.392716535379308285 ) ) ;
#25139 = ORIENTED_EDGE ( 'NONE', *, *, #16149, .T. ) ;
#25140 = CARTESIAN_POINT ( 'NONE',  ( -0.07405724077823318263, -1.115157480261196987, -0.1787899950787401604 ) ) ;
#25141 = CARTESIAN_POINT ( 'NONE',  ( -0.1787899950787401882, -1.339074803095842592, 0.000000000000000000 ) ) ;
#25142 = VECTOR ( 'NONE', #43235, 39.37007874015748143 ) ;
#25143 = CARTESIAN_POINT ( 'NONE',  ( -0.7185039370078739607, 1.928577636452523993E-17, 1.555118110128692832 ) ) ;
#25144 = LENGTH_MEASURE_WITH_UNIT ( LENGTH_MEASURE( 0.02539999999999999897 ), #6207 ) ;
#25145 = CARTESIAN_POINT ( 'NONE',  ( 0.7185039370078746268, -0.06523048226347956391, 0.3863188976377951445 ) ) ;
#25146 = CARTESIAN_POINT ( 'NONE',  ( -0.1270800023317771588, -0.5866579828113921424, 0.1270800023317771588 ) ) ;
#25147 = CARTESIAN_POINT ( 'NONE',  ( -0.7646288533564489232, 0.1113553986120547346, 0.8809055117034961802 ) ) ;
#25148 = CARTESIAN_POINT ( 'NONE',  ( -0.9412147342319837628, -0.1574803149606297803, 0.8292322834645677876 ) ) ;
#25149 = CIRCLE ( 'NONE', #4455, 0.4724409448818900348 ) ;
#25150 = CARTESIAN_POINT ( 'NONE',  ( 0.6971942568897626646, -0.07405724077823297447, 0.4035433070328508509 ) ) ;
#25151 = CARTESIAN_POINT ( 'NONE',  ( -0.06523048226347956391, -0.1382874015748031260, 0.1574803149606297803 ) ) ;
#25152 = CARTESIAN_POINT ( 'NONE',  ( 0.8107537697050253289, 0.1574803149606300301, 1.862696850286174710 ) ) ;
#25153 = ORIENTED_EDGE ( 'NONE', *, *, #15546, .F. ) ;
#25154 = EDGE_CURVE ( 'NONE', #30513, #23380, #22247, .T. ) ;
#25155 = CARTESIAN_POINT ( 'NONE',  ( 0.8759842519685039353, -0.1574803149606299191, 0.8661417322834645827 ) ) ;
#25156 = CARTESIAN_POINT ( 'NONE',  ( 0.2395294000716133853, -0.1968503937007874127, 1.181102362204724310 ) ) ;
#25157 = CARTESIAN_POINT ( 'NONE',  ( -0.5314960629921259283, 1.928577636452524610E-17, 5.000000000000000000 ) ) ;
#25158 = ( BOUNDED_CURVE ( )  B_SPLINE_CURVE ( 2, ( #721, #15861, #15381, #18946, #15624, #30030, #44339, #11547, #8403 ),
 .UNSPECIFIED., .F., .F. ) 
 B_SPLINE_CURVE_WITH_KNOTS ( ( 3, 2, 2, 2, 3 ),
 ( 0.5200000000000000178, 0.5224999999999999645, 0.5250000000000000222, 0.5274999999999999689, 0.5300000000000000266 ),
 .UNSPECIFIED. ) 
 CURVE ( )  GEOMETRIC_REPRESENTATION_ITEM ( )  RATIONAL_B_SPLINE_CURVE ( ( 1.000000000000000000, 0.9238795325112869605, 1.000000000000000000, 0.9238795325112869605, 1.000000000000000000, 0.9238795325112869605, 1.000000000000000000, 0.9238795325112869605, 1.000000000000000000 ) ) 
 REPRESENTATION_ITEM ( '' )  ) ;
#25159 = EDGE_CURVE ( 'NONE', #21151, #16941, #34755, .T. ) ;
#25161 = CARTESIAN_POINT ( 'NONE',  ( 0.9412147342319837628, 0.1574803149606300301, 1.513287401574803681 ) ) ;
#25160 = LINE ( 'NONE', #43111, #23992 ) ;
#25162 = CARTESIAN_POINT ( 'NONE',  ( 0.9873396505805591694, -0.1113553986120547346, 0.1919291337507405548 ) ) ;
#25163 = ADVANCED_FACE ( 'NONE', ( #37104 ), #7405, .T. ) ;
#25164 = ORIENTED_EDGE ( 'NONE', *, *, #5852, .T. ) ;
#25165 = CARTESIAN_POINT ( 'NONE',  ( 0.1264236179284866091, -0.06446850388324429360, 0.1264236179284866091 ) ) ;
#25166 = EDGE_CURVE ( 'NONE', #2480, #18061, #19399, .T. ) ;
#25167 = VERTEX_POINT ( 'NONE', #40909 ) ;
#25168 = CARTESIAN_POINT ( 'NONE',  ( 0.8759842519685039353, 0.1574803149606299191, 1.899606299105070839 ) ) ;
#25169 = CARTESIAN_POINT ( 'NONE',  ( -0.06523048226347956391, -1.521161417215307177, -0.1574803149606300301 ) ) ;
#25170 = CARTESIAN_POINT ( 'NONE',  ( -0.1264236179284866091, -0.6008858267178898149, -0.1264236179284866091 ) ) ;
#25171 = CARTESIAN_POINT ( 'NONE',  ( -9.642888182262618425E-18, -1.061023622047244208, -0.1574803149606299191 ) ) ;
#25172 = CARTESIAN_POINT ( 'NONE',  ( 0.7646288533564489232, 0.1113553986120547346, 0.9202755904436535905 ) ) ;
#25173 = CARTESIAN_POINT ( 'NONE',  ( 0.2759478392031582961, -0.5708661417322835607, 1.214596435718460654 ) ) ;
#25174 = CARTESIAN_POINT ( 'NONE',  ( -1.002407869896990045, -0.1264236179284866091, 0.4502952755367874427 ) ) ;
#25175 = ORIENTED_EDGE ( 'NONE', *, *, #1287, .T. ) ;
#25176 = ORIENTED_EDGE ( 'NONE', *, *, #6307, .F. ) ;
#25177 = CARTESIAN_POINT ( 'NONE',  ( -0.8019270111902717657, 0.1787899950787401604, 1.614173228292692386 ) ) ;
#25178 = VERTEX_POINT ( 'NONE', #18197 ) ;
#25179 = CARTESIAN_POINT ( 'NONE',  ( 0.8019270111902717657, 0.1787899950787401604, 1.614173228292692386 ) ) ;
#25180 = ORIENTED_EDGE ( 'NONE', *, *, #4876, .F. ) ;
#25181 = CARTESIAN_POINT ( 'NONE',  ( -0.9500414927467378812, 0.1787899950787401604, 0.7824803149068669805 ) ) ;
#25182 = CARTESIAN_POINT ( 'NONE',  ( -0.8019270111902717657, 0.1787899950787401604, 1.294291338528912982 ) ) ;
#25183 = CARTESIAN_POINT ( 'NONE',  ( -0.8759842519685039353, 0.1787899950787401882, 0.6225393700249762796 ) ) ;
#25184 = DIRECTION ( 'NONE',  ( -1.000000000000000000, 1.776356839400250070E-15, 0.000000000000000000 ) ) ;
#25185 = AXIS2_PLACEMENT_3D ( 'NONE', #17554, #32192, #42471 ) ;
#25186 = DIRECTION ( 'NONE',  ( 1.000000000000000000, 0.000000000000000000, -1.822029033848725275E-16 ) ) ;
#25187 = CARTESIAN_POINT ( 'NONE',  ( -0.1113553986120547346, -0.2096456691838114172, 0.1113553986120547346 ) ) ;
#25188 = CARTESIAN_POINT ( 'NONE',  ( -1.002407869896990045, 0.1264236179284866091, 1.449311023568283341 ) ) ;
#25189 = ORIENTED_EDGE ( 'NONE', *, *, #32550, .T. ) ;
#25190 = CARTESIAN_POINT ( 'NONE',  ( -0.7185039370078739607, 1.928577636452523993E-17, 1.840551181102362266 ) ) ;
#25191 = CARTESIAN_POINT ( 'NONE',  ( -0.8107537697050253289, 0.1574803149606300301, 0.4158464566929134243 ) ) ;
#25192 = CARTESIAN_POINT ( 'NONE',  ( 0.8759842519685039353, 0.1787899950787401882, 1.414862204670645829 ) ) ;
#25193 = CARTESIAN_POINT ( 'NONE',  ( 0.1430555697033809026, -0.09851384659136652733, -0.1381766785746311177 ) ) ;
#25194 = DIRECTION ( 'NONE',  ( 1.144917494144692682E-16, -3.972230510298674823E-31, 1.000000000000000000 ) ) ;
#25195 = ORIENTED_EDGE ( 'NONE', *, *, #36108, .F. ) ;
#25196 = AXIS2_PLACEMENT_3D ( 'NONE', #8204, #12546, #5317 ) ;
#25197 = CARTESIAN_POINT ( 'NONE',  ( 3.284318927891251994E-17, -1.660064913111128249, 0.1787899950787401882 ) ) ;
#25198 = VERTEX_POINT ( 'NONE', #19123 ) ;
#25199 = CIRCLE ( 'NONE', #31341, 0.08090551181102362266 ) ;
#25200 = CARTESIAN_POINT ( 'NONE',  ( 0.7646288533564489232, 0.1113553986120547346, 0.4970472440944882497 ) ) ;
#25201 = ORIENTED_EDGE ( 'NONE', *, *, #2376, .T. ) ;
#25202 = CARTESIAN_POINT ( 'NONE',  ( -0.07405724077823318263, -0.4064960629383624346, -0.1787899950787401604 ) ) ;
#25203 = CARTESIAN_POINT ( 'NONE',  ( -0.07405724077823318263, -0.8592519684501739308, 0.1787899950787401604 ) ) ;
#25204 = DIRECTION ( 'NONE',  ( 1.000000000000000000, 0.000000000000000000, -1.822029033848725275E-16 ) ) ;
#25205 = DIRECTION ( 'NONE',  ( 0.000000000000000000, 0.000000000000000000, 1.000000000000000000 ) ) ;
#25206 = CARTESIAN_POINT ( 'NONE',  ( 1.002407869896990045, 0.1264236179284866091, 0.3420275590013546751 ) ) ;
#25207 = CARTESIAN_POINT ( 'NONE',  ( 0.07405724077823318263, -0.1861475902764828938, -0.1787899950787401604 ) ) ;
#25208 = CARTESIAN_POINT ( 'NONE',  ( 0.2471921892202938176, -0.09660984127287172707, -0.02628542481976669717 ) ) ;
#25209 = CARTESIAN_POINT ( 'NONE',  ( 0.6971942568897637749, 2.189545951927499583E-17, 0.6717519684501732646 ) ) ;
#25210 = EDGE_CURVE ( 'NONE', #17273, #42395, #33787, .T. ) ;
#25211 = CARTESIAN_POINT ( 'NONE',  ( -0.7495606340400177148, 0.1264236179284866091, 0.9473425196312755814 ) ) ;
#25212 = CIRCLE ( 'NONE', #7619, 0.2204724409448818867 ) ;
#25214 = CARTESIAN_POINT ( 'NONE',  ( -0.7185039370078739607, 0.000000000000000000, -2.869337061179095023E-17 ) ) ;
#25213 = ( NAMED_UNIT ( * ) SI_UNIT ( $, .STERADIAN. ) SOLID_ANGLE_UNIT ( ) ) ;
#25215 = CARTESIAN_POINT ( 'NONE',  ( 0.1797182628040039087, -1.750535935567296475, -0.07444174185955065859 ) ) ;
#25216 = CARTESIAN_POINT ( 'NONE',  ( 0.7185039370078739607, 1.928577636452523993E-17, 0.9645669290263307882 ) ) ;
#25217 = CARTESIAN_POINT ( 'NONE',  ( 0.9500414927467378812, -0.1787899950787401604, 1.712598425143087688 ) ) ;
#25219 = CARTESIAN_POINT ( 'NONE',  ( 0.2559055118110235560, 0.06384451362999800372, -0.3104478705636015134 ) ) ;
#25218 = CARTESIAN_POINT ( 'NONE',  ( -0.1550311931537672050, -0.09383642490574117812, 0.1959255884475979703 ) ) ;
#25220 = CARTESIAN_POINT ( 'NONE',  ( 1.054774247047244540, -0.07405724077823318263, 0.4921259841982049132 ) ) ;
#25221 = EDGE_CURVE ( 'NONE', #22114, #44500, #33070, .T. ) ;
#25222 = VERTEX_POINT ( 'NONE', #36879 ) ;
#25223 = ADVANCED_FACE ( 'NONE', ( #4033 ), #33543, .T. ) ;
#25224 = DIRECTION ( 'NONE',  ( -1.000000000000000000, 0.000000000000000000, 0.000000000000000000 ) ) ;
#25225 = DIRECTION ( 'NONE',  ( 0.000000000000000000, -1.000000000000000000, 0.000000000000000000 ) ) ;
#25226 = CARTESIAN_POINT ( 'NONE',  ( 0.07405724077823318263, -0.1505905511273389341, 0.1787899950787401604 ) ) ;
#25227 = AXIS2_PLACEMENT_3D ( 'NONE', #13622, #39249, #43074 ) ;
#25228 = CARTESIAN_POINT ( 'NONE',  ( 0.6971942568897626646, 0.07405724077823318263, 0.5511811023084406402 ) ) ;
#25229 = CARTESIAN_POINT ( 'NONE',  ( 0.1787899950787401604, -1.046259842465921297, 0.07405724077823318263 ) ) ;
#25230 = CARTESIAN_POINT ( 'NONE',  ( 0.8759842519685039353, 0.1787899950787401882, 0.1550196849856066983 ) ) ;
#25231 = CARTESIAN_POINT ( 'NONE',  ( -0.9873396505805591694, -0.1113553986120547346, 1.530511810916094451 ) ) ;
#25232 = CARTESIAN_POINT ( 'NONE',  ( -0.7495606340400177148, 0.1264236179284866091, 1.611712598371433103 ) ) ;
#25233 = ORIENTED_EDGE ( 'NONE', *, *, #35611, .T. ) ;
#25234 = CARTESIAN_POINT ( 'NONE',  ( -1.054774247047244096, 0.000000000000000000, 1.129429133804503937 ) ) ;
#25236 = AXIS2_PLACEMENT_3D ( 'NONE', #1586, #5905, #1830 ) ;
#25235 = CARTESIAN_POINT ( 'NONE',  ( -0.2610212580023196227, -0.1673090378115812127, -0.8873684129880539118 ) ) ;
#25237 = CARTESIAN_POINT ( 'NONE',  ( 0.6971942568897637749, 2.189545951927499583E-17, 1.227854330654897685 ) ) ;
#25238 = ORIENTED_EDGE ( 'NONE', *, *, #10564, .T. ) ;
#25239 = CARTESIAN_POINT ( 'NONE',  ( -0.8759842519685039353, 0.1574803149606299191, 0.7185039369003465293 ) ) ;
#25240 = CARTESIAN_POINT ( 'NONE',  ( 0.7185039370078746268, 0.06523048226347977208, 0.1058070866141732902 ) ) ;
#25241 = CARTESIAN_POINT ( 'NONE',  ( 0.8759842519685039353, 0.1787899950787401882, 1.843011810969858333 ) ) ;
#25242 = CARTESIAN_POINT ( 'NONE',  ( -0.7646288533564489232, 0.1113553986120547346, 0.6151574803149606474 ) ) ;
#25243 = CARTESIAN_POINT ( 'NONE',  ( -0.9500414927467378812, -0.1787899950787401604, 0.8809055117572599514 ) ) ;
#25244 = CARTESIAN_POINT ( 'NONE',  ( 0.1377952755905511861, 0.1564960629921262614, -0.7066929133858274037 ) ) ;
#25245 = CARTESIAN_POINT ( 'NONE',  ( 0.8759842519685039353, 0.1787899950787401882, 0.3124999999462365619 ) ) ;
#25246 = CARTESIAN_POINT ( 'NONE',  ( -0.8759842519685039353, 0.1787899950787401882, 0.1894685038832444879 ) ) ;
#25247 = CARTESIAN_POINT ( 'NONE',  ( -1.054774247047244096, 0.000000000000000000, 0.7701771653005669016 ) ) ;
#25248 = CARTESIAN_POINT ( 'NONE',  ( 1.033464566929134687, -0.06523048226347956391, 1.532972440837355066 ) ) ;
#25249 = EDGE_LOOP ( 'NONE', ( #26691, #13453, #30709, #39895 ) ) ;
#25250 = CARTESIAN_POINT ( 'NONE',  ( 0.1787899950787401604, 0.05118110241596821042, 0.07405724077823318263 ) ) ;
#25251 = VERTEX_POINT ( 'NONE', #658 ) ;
#25252 = CARTESIAN_POINT ( 'NONE',  ( 1.002407869896990045, -0.1264236179284866091, 0.8489173227808819444 ) ) ;
#25253 = CARTESIAN_POINT ( 'NONE',  ( 0.9500414927467377701, 0.1787899950787401604, 1.058070866087969186 ) ) ;
#25254 = CARTESIAN_POINT ( 'NONE',  ( -0.6971942568897648851, 0.07405724077823318263, 1.929133858213952557 ) ) ;
#25255 = EDGE_CURVE ( 'NONE', #30476, #44500, #435, .T. ) ;
#25256 = CARTESIAN_POINT ( 'NONE',  ( 1.054774247047244096, 0.000000000000000000, 1.872539370024976391 ) ) ;
#25257 = ORIENTED_EDGE ( 'NONE', *, *, #20179, .F. ) ;
#25258 = VECTOR ( 'NONE', #17921, 39.37007874015748143 ) ;
#25259 = CARTESIAN_POINT ( 'NONE',  ( -1.033464566929133799, 1.928577636452524610E-17, 2.869337061179095023E-17 ) ) ;
#25260 = CARTESIAN_POINT ( 'NONE',  ( -0.1787899950787401882, -1.315576724134750242, 0.000000000000000000 ) ) ;
#25261 = ORIENTED_EDGE ( 'NONE', *, *, #46847, .F. ) ;
#25262 = CARTESIAN_POINT ( 'NONE',  ( 0.1787899950787401882, -0.2957677164816697180, -2.189545951927503898E-17 ) ) ;
#25263 = ORIENTED_EDGE ( 'NONE', *, *, #17211, .T. ) ;
#25264 = CARTESIAN_POINT ( 'NONE',  ( 0.9500414927467378812, -0.1787899950787401604, 1.077755905458048113 ) ) ;
#25265 = DIRECTION ( 'NONE',  ( -3.469446951953614189E-15, -1.000000000000000000, 0.000000000000000000 ) ) ;
#25266 = AXIS2_PLACEMENT_3D ( 'NONE', #24147, #19586, #27043 ) ;
#25267 = DIRECTION ( 'NONE',  ( 1.000000000000000000, 0.000000000000000000, -0.000000000000000000 ) ) ;
#25268 = CARTESIAN_POINT ( 'NONE',  ( 0.8019270111902717657, -0.1787899950787401604, 0.08858267711159097113 ) ) ;
#25269 = CIRCLE ( 'NONE', #1547, 0.08090551181102362266 ) ;
#25270 = CARTESIAN_POINT ( 'NONE',  ( 3.284318927891251994E-17, -1.570374015694267600, 0.1787899950787401882 ) ) ;
#25271 = CARTESIAN_POINT ( 'NONE',  ( 0.1264236179284866091, -0.7386811023084409733, 0.1264236179284866091 ) ) ;
#25272 = EDGE_CURVE ( 'NONE', #16941, #26427, #26101, .T. ) ;
#25273 = CARTESIAN_POINT ( 'NONE',  ( -1.054774247047244096, 0.000000000000000000, 0.4601377952218267953 ) ) ;
#25274 = CARTESIAN_POINT ( 'NONE',  ( 0.06841996760812382727, 0.1299212598425196763, 0.1651804176431311000 ) ) ;
#25276 = CARTESIAN_POINT ( 'NONE',  ( -0.7196516388670834985, -0.06167255061999755983, 1.984442901297172490 ) ) ;
#25275 = CARTESIAN_POINT ( 'NONE',  ( -0.1797182628040039087, -1.263331211157848966, -0.07444174185955065859 ) ) ;
#25277 = CYLINDRICAL_SURFACE ( 'NONE', #47033, 0.1968503937007874127 ) ;
#25278 = CARTESIAN_POINT ( 'NONE',  ( 0.8019270111902717657, 0.1787899950787401604, 1.259842519631276359 ) ) ;
#25279 = CARTESIAN_POINT ( 'NONE',  ( 0.8019270111902716547, -0.1787899950787401604, 1.624015747977732849 ) ) ;
#25280 = DIRECTION ( 'NONE',  ( 8.659560562353279948E-17, 0.7071067811866824648, -0.7071067811864125696 ) ) ;
#25281 = EDGE_CURVE ( 'NONE', #42416, #18452, #34721, .T. ) ;
#25282 = CARTESIAN_POINT ( 'NONE',  ( 1.033464566929134687, 0.06523048226347956391, 0.01230314960629920289 ) ) ;
#25283 = CARTESIAN_POINT ( 'NONE',  ( 0.1595445804228954878, 0.05486576152185763944, 0.1404716313526493954 ) ) ;
#25284 = CARTESIAN_POINT ( 'NONE',  ( 0.7185039370078739607, 1.928577636452523993E-17, 0.8070866140657008136 ) ) ;
#25285 = CARTESIAN_POINT ( 'NONE',  ( -1.033464566929134687, 0.06523048226347956391, 1.656003936900346085 ) ) ;
#25286 = CARTESIAN_POINT ( 'NONE',  ( -0.1787899950787401882, 0.03887795280966901967, 0.000000000000000000 ) ) ;
#25287 = CARTESIAN_POINT ( 'NONE',  ( 0.8019270111902717657, -0.1787899950787401604, 0.1673228345919057225 ) ) ;
#25288 = CARTESIAN_POINT ( 'NONE',  ( 0.7026501795067128242, -0.01243134911390358054, 0.03936888280061108525 ) ) ;
#25290 = CARTESIAN_POINT ( 'NONE',  ( -1.060626887254335780E-16, -0.0009842519685041700977, -0.4921259842519680738 ) ) ;
#25289 = CARTESIAN_POINT ( 'NONE',  ( 1.002407869896990045, -0.1264236179284866091, 1.158956692859621995 ) ) ;
#25291 = AXIS2_PLACEMENT_3D ( 'NONE', #19684, #34327, #23296 ) ;
#25292 = CARTESIAN_POINT ( 'NONE',  ( 0.7646288533564489232, -0.1113553986120547346, 1.215551181102362266 ) ) ;
#25293 = CARTESIAN_POINT ( 'NONE',  ( 0.9412147342319837628, -0.1574803149606297803, 0.5044291337507409434 ) ) ;
#25294 = VERTEX_POINT ( 'NONE', #1618 ) ;
#25295 = CARTESIAN_POINT ( 'NONE',  ( -0.7646288533564489232, 0.1113553986120547346, 1.126968503937007871 ) ) ;
#25296 = CARTESIAN_POINT ( 'NONE',  ( 0.9427463997941362139, 0.1565286221232543296, 0.03936821677798599262 ) ) ;
#25297 = CARTESIAN_POINT ( 'NONE',  ( -0.8759842519685039353, 0.1574803149606299191, 0.3641732282389295583 ) ) ;
#25298 = AXIS2_PLACEMENT_3D ( 'NONE', #1993, #12570, #12807 ) ;
#25299 = EDGE_LOOP ( 'NONE', ( #42641, #16600, #46081, #27082 ) ) ;
#25300 = CARTESIAN_POINT ( 'NONE',  ( 1.002407869896990045, 0.1264236179284866091, 1.444389763725763665 ) ) ;
#25302 = DIRECTION ( 'NONE',  ( 3.469446951953615767E-15, 1.000000000000000000, 0.000000000000000000 ) ) ;
#25301 = CARTESIAN_POINT ( 'NONE',  ( -0.7646288533564489232, 0.1113553986120547346, 1.638779527559055316 ) ) ;
#25303 = CARTESIAN_POINT ( 'NONE',  ( -1.054774247047244540, 0.07405724077823318263, 0.06397637789899228433 ) ) ;
#25305 = AXIS2_PLACEMENT_3D ( 'NONE', #12344, #20687, #38898 ) ;
#25304 = CARTESIAN_POINT ( 'NONE',  ( 0.1787899950787401604, 0.02165354336085011100, -0.07405724077823318263 ) ) ;
#25306 = ORIENTED_EDGE ( 'NONE', *, *, #30192, .T. ) ;
#25307 = CARTESIAN_POINT ( 'NONE',  ( 1.033464566929134909, 0.06523048226347841205, 0.4355314959554649201 ) ) ;
#25308 = ORIENTED_EDGE ( 'NONE', *, *, #22403, .T. ) ;
#25309 = DIRECTION ( 'NONE',  ( -0.000000000000000000, 1.000000000000000000, -0.000000000000000000 ) ) ;
#25310 = CARTESIAN_POINT ( 'NONE',  ( 0.1632645169460268941, -0.09126532511078781773, -0.1911722030488886837 ) ) ;
#25311 = CARTESIAN_POINT ( 'NONE',  ( 0.7495606340400177148, 0.1264236179284866091, 0.5536417322297008115 ) ) ;
#25312 = ORIENTED_EDGE ( 'NONE', *, *, #23109, .F. ) ;
#25313 = CARTESIAN_POINT ( 'NONE',  ( -1.002407869896990045, 0.1264236179284866091, 1.483759842465921075 ) ) ;
#25314 = CARTESIAN_POINT ( 'NONE',  ( -0.1264236179284866091, -1.772145669237574994, 0.1264236179284866091 ) ) ;
#25315 = CARTESIAN_POINT ( 'NONE',  ( -0.7495606340400177148, 0.1264236179284866091, 1.183562992072220599 ) ) ;
#25316 = CARTESIAN_POINT ( 'NONE',  ( -0.9873396505805591694, -0.1113553986120547346, 0.08366141732283464971 ) ) ;
#25317 = ORIENTED_EDGE ( 'NONE', *, *, #41756, .T. ) ;
#25318 = CARTESIAN_POINT ( 'NONE',  ( -0.6971942568897648851, 0.07405724077823318263, 1.141732283410804349 ) ) ;
#25319 = ADVANCED_FACE ( 'NONE', ( #12442 ), #27103, .T. ) ;
#25320 = CARTESIAN_POINT ( 'NONE',  ( -0.7495606340400177148, -0.1264236179284866091, 0.1697834645131657827 ) ) ;
#25321 = CARTESIAN_POINT ( 'NONE',  ( 0.01230737760510397689, 0.07955613945526338049, 0.1377952755905511861 ) ) ;
#25322 = CARTESIAN_POINT ( 'NONE',  ( 0.8759842519685039353, -0.1574803149606299191, 1.643700787294047228 ) ) ;
#25323 = CARTESIAN_POINT ( 'NONE',  ( -0.07405724077823318263, -0.8751239682292385469, 0.1787899950787401604 ) ) ;
#25324 = ORIENTED_EDGE ( 'NONE', *, *, #33414, .F. ) ;
#25325 = CARTESIAN_POINT ( 'NONE',  ( -0.1574803149606300301, -0.02017716524680367163, -0.06523048226347956391 ) ) ;
#25326 = CARTESIAN_POINT ( 'NONE',  ( -0.9412147342319837628, -0.1574803149606297803, 0.8587598424121577478 ) ) ;
#25327 = ORIENTED_EDGE ( 'NONE', *, *, #31858, .F. ) ;
#25328 = ORIENTED_EDGE ( 'NONE', *, *, #11074, .T. ) ;
#25329 = DIRECTION ( 'NONE',  ( 0.000000000000000000, 0.000000000000000000, -1.000000000000000000 ) ) ;
#25330 = CARTESIAN_POINT ( 'NONE',  ( 0.08946752424252854552, 0.3740157480314960647, 1.224299699984021661 ) ) ;
#25331 = CARTESIAN_POINT ( 'NONE',  ( -0.8019270111902717657, -0.1787899950787401604, 0.7185039369541108556 ) ) ;
#25332 = DIRECTION ( 'NONE',  ( 0.000000000000000000, 0.000000000000000000, 1.000000000000000000 ) ) ;
#25334 = ORIENTED_EDGE ( 'NONE', *, *, #43038, .T. ) ;
#25333 = CIRCLE ( 'NONE', #43677, 0.1673228346456689108 ) ;
#25335 = CARTESIAN_POINT ( 'NONE',  ( -1.002407869896990045, 0.1264236179284866091, 1.764271653489543290 ) ) ;
#25336 = CIRCLE ( 'NONE', #17690, 0.1968503937007874405 ) ;
#25337 = EDGE_CURVE ( 'NONE', #14813, #33650, #45694, .T. ) ;
#25338 = ADVANCED_FACE ( 'NONE', ( #44749 ), #27307, .F. ) ;
#25339 = AXIS2_PLACEMENT_3D ( 'NONE', #37341, #33319, #4492 ) ;
#25340 = CARTESIAN_POINT ( 'NONE',  ( -0.3980944881889745268, 0.6449983665207583705, -0.06082000038405668829 ) ) ;
#25341 = ADVANCED_FACE ( 'NONE', ( #5212 ), #45220, .T. ) ;
#25342 = CARTESIAN_POINT ( 'NONE',  ( -0.6971942568897626646, -0.07405724077823297447, 0.1279527558517483676 ) ) ;
#25343 = CARTESIAN_POINT ( 'NONE',  ( -0.1270800023317771588, -0.8327209749373759573, -0.1270800023317771588 ) ) ;
#25344 = DIRECTION ( 'NONE',  ( 1.000000000000000000, 0.000000000000000000, 0.000000000000000000 ) ) ;
#25345 = CARTESIAN_POINT ( 'NONE',  ( -0.9412147342319837628, 0.1574803149606300301, 1.345964566821607589 ) ) ;
#25346 = VECTOR ( 'NONE', #46664, 39.37007874015748143 ) ;
#25347 = CARTESIAN_POINT ( 'NONE',  ( 0.7495606340400177148, 0.1264236179284866091, 0.7111220471903307860 ) ) ;
#25348 = CARTESIAN_POINT ( 'NONE',  ( -0.1574803149606299191, -0.5393700787401575214, 0.000000000000000000 ) ) ;
#25349 = CARTESIAN_POINT ( 'NONE',  ( 0.1574803149606299746, 0.7443365962042343131, -3.523993443072799270 ) ) ;
#25350 = ORIENTED_EDGE ( 'NONE', *, *, #6158, .F. ) ;
#25351 = CARTESIAN_POINT ( 'NONE',  ( -0.8759842519685039353, 0.000000000000000000, 0.000000000000000000 ) ) ;
#25352 = ADVANCED_FACE ( 'NONE', ( #31128 ), #20075, .F. ) ;
#25353 = CARTESIAN_POINT ( 'NONE',  ( 1.033464566929134687, -0.06523048226347956391, 1.306594488188977055 ) ) ;
#25355 = DIRECTION ( 'NONE',  ( 1.000000000000000000, -0.000000000000000000, -0.000000000000000000 ) ) ;
#25354 = CARTESIAN_POINT ( 'NONE',  ( 0.7801632783431100560, -0.1419831758506162611, 1.986316665493995215 ) ) ;
#25356 = DIRECTION ( 'NONE',  ( 1.000000000000000000, -4.710082747697002339E-15, 4.710082747697002339E-15 ) ) ;
#25357 = CARTESIAN_POINT ( 'NONE',  ( 0.1574803149606300301, -0.6254921258767247583, -0.06523048226347956391 ) ) ;
#25359 = DIRECTION ( 'NONE',  ( 0.000000000000000000, 0.000000000000000000, -1.000000000000000000 ) ) ;
#25358 = CARTESIAN_POINT ( 'NONE',  ( 0.6971942568897637749, 2.189545951927499583E-17, 0.6323818897100157432 ) ) ;
#25360 = CARTESIAN_POINT ( 'NONE',  ( -1.033464566929134687, -0.06523048226347956391, 0.3912401573727880555 ) ) ;
#25361 = ORIENTED_EDGE ( 'NONE', *, *, #16679, .T. ) ;
#25362 = CARTESIAN_POINT ( 'NONE',  ( 0.1636082376784445125, 0.08043339677773757301, 0.1393150588506956167 ) ) ;
#25363 = CARTESIAN_POINT ( 'NONE',  ( 0.1578913225048159952, 0.03378178545796894222, -0.1404269458896922063 ) ) ;
#25364 = CARTESIAN_POINT ( 'NONE',  ( 0.9500414927467378812, 0.1787899950787401604, 1.013779527505291878 ) ) ;
#25365 = PLANE ( 'NONE',  #23401 ) ;
#25366 = CARTESIAN_POINT ( 'NONE',  ( -0.1787899950787401604, -1.184055118056472455, 0.07405724077823318263 ) ) ;
#25367 = CARTESIAN_POINT ( 'NONE',  ( -0.1113553986120547346, -1.597440944881889813, 0.1113553986120547346 ) ) ;
#25368 = CYLINDRICAL_SURFACE ( 'NONE', #22189, 0.09842519685039370636 ) ;
#25369 = AXIS2_PLACEMENT_3D ( 'NONE', #25349, #14324, #39462 ) ;
#25370 = CARTESIAN_POINT ( 'NONE',  ( -0.6971942568897626646, -0.07405724077823297447, 0.1624015747493861295 ) ) ;
#25371 = ORIENTED_EDGE ( 'NONE', *, *, #18600, .F. ) ;
#25372 = DIRECTION ( 'NONE',  ( 0.000000000000000000, 1.000000000000000000, 0.000000000000000000 ) ) ;
#25373 = VERTEX_POINT ( 'NONE', #19363 ) ;
#25374 = CARTESIAN_POINT ( 'NONE',  ( 0.1574803149606300301, -0.3154527557979848185, 0.06523048226347956391 ) ) ;
#25375 = CARTESIAN_POINT ( 'NONE',  ( -0.8019270111902716547, 0.1787899950787401604, 1.929133858213952557 ) ) ;
#25376 = AXIS2_PLACEMENT_3D ( 'NONE', #1552, #41548, #22668 ) ;
#25377 = AXIS2_PLACEMENT_3D ( 'NONE', #14044, #14290, #21455 ) ;
#25378 = CARTESIAN_POINT ( 'NONE',  ( -1.054774247047244096, 0.000000000000000000, 1.715059055064346527 ) ) ;
#25379 = CARTESIAN_POINT ( 'NONE',  ( -0.7495606340400177148, 0.1264236179284866091, 1.060531496009228247 ) ) ;
#25380 = VECTOR ( 'NONE', #39227, 39.37007874015748143 ) ;
#25381 = CARTESIAN_POINT ( 'NONE',  ( -1.054774247047244096, 0.000000000000000000, 0.4207677164816693294 ) ) ;
#25382 = EDGE_CURVE ( 'NONE', #9638, #46176, #14859, .T. ) ;
#25383 = DIRECTION ( 'NONE',  ( -1.000000000000000000, 0.000000000000000000, 0.000000000000000000 ) ) ;
#25384 = CARTESIAN_POINT ( 'NONE',  ( 0.8759842519685039353, 0.1574803149606299191, 0.4035433069790866356 ) ) ;
#25385 = DIRECTION ( 'NONE',  ( 0.000000000000000000, 0.000000000000000000, 1.000000000000000000 ) ) ;
#25386 = CARTESIAN_POINT ( 'NONE',  ( -0.07405724077823318263, -0.3780767241347506857, -0.1787899950787401604 ) ) ;
#25387 = CARTESIAN_POINT ( 'NONE',  ( 0.0003584782005013444962, -0.09842519685039370636, 0.1560556493606787276 ) ) ;
#25388 = CARTESIAN_POINT ( 'NONE',  ( -0.8759842519685039353, 0.000000000000000000, 0.000000000000000000 ) ) ;
#25389 = CARTESIAN_POINT ( 'NONE',  ( -0.7495606340400177148, -0.1264236179284866091, 0.1648622046706460786 ) ) ;
#25390 = EDGE_LOOP ( 'NONE', ( #17406, #25855, #23977, #44857 ) ) ;
#25391 = ORIENTED_EDGE ( 'NONE', *, *, #39318, .T. ) ;
#25392 = EDGE_CURVE ( 'NONE', #3114, #42764, #37828, .T. ) ;
#25393 = CARTESIAN_POINT ( 'NONE',  ( -0.9500414927467377701, -0.1787899950787401604, 1.318897637741511364 ) ) ;
#25394 = ORIENTED_EDGE ( 'NONE', *, *, #42957, .F. ) ;
#25395 = CARTESIAN_POINT ( 'NONE',  ( 0.1787899950787401604, -1.243110236166709459, -0.07405724077823318263 ) ) ;
#25396 = CARTESIAN_POINT ( 'NONE',  ( -0.1787899950787401882, -1.417814960576157635, 0.000000000000000000 ) ) ;
#25397 = EDGE_CURVE ( 'NONE', #44147, #21725, #40849, .T. ) ;
#25398 = DIRECTION ( 'NONE',  ( 0.000000000000000000, 3.469446951953614583E-15, 1.000000000000000000 ) ) ;
#25399 = DIRECTION ( 'NONE',  ( 7.000000000000000150E-15, 2.999999999999999839E-15, 1.000000000000000000 ) ) ;
#25400 = CARTESIAN_POINT ( 'NONE',  ( 0.7185039370078739607, 1.928577636452523993E-17, 0.3838582677165354173 ) ) ;
#25401 = CARTESIAN_POINT ( 'NONE',  ( 3.301370929368692659E-17, -0.6211068017090294324, 0.1797182628040039365 ) ) ;
#25402 = CYLINDRICAL_SURFACE ( 'NONE', #4847, 0.1574803149606299191 ) ;
#25403 = CARTESIAN_POINT ( 'NONE',  ( -0.7185039370078746268, 0.06523048226347956391, 1.001476377845228027 ) ) ;
#25404 = B_SPLINE_CURVE_WITH_KNOTS ( 'NONE', 3,
 ( #1096, #5169, #23160, #23868, #26536, #37778 ),
 .UNSPECIFIED., .F., .F.,
 ( 4, 2, 4 ),
 ( -7.834150686268513193E-06, 0.0001896218827938178436, 0.0003870779162739032618 ),
 .UNSPECIFIED. ) ;
#25405 = CARTESIAN_POINT ( 'NONE',  ( -0.06523048226347956391, -0.07431102362204727863, -0.1574803149606300301 ) ) ;
#25406 = CIRCLE ( 'NONE', #11616, 0.3100393700787401619 ) ;
#25407 = AXIS2_PLACEMENT_3D ( 'NONE', #44885, #25773, #339 ) ;
#25408 = CARTESIAN_POINT ( 'NONE',  ( 0.7185039370078746268, -0.06523048226347956391, 1.754429133750741387 ) ) ;
#25409 = EDGE_LOOP ( 'NONE', ( #44296, #47132, #2702, #21317 ) ) ;
#25410 = CARTESIAN_POINT ( 'NONE',  ( 0.1574803149606299191, 0.4003652867858621955, 0.7276473417831970103 ) ) ;
#25411 = CARTESIAN_POINT ( 'NONE',  ( 0.7646288533564489232, -0.1113553986120547346, 0.7431102362204724532 ) ) ;
#25412 = DIRECTION ( 'NONE',  ( 0.000000000000000000, 0.000000000000000000, 1.000000000000000000 ) ) ;
#25413 = B_SPLINE_CURVE_WITH_KNOTS ( 'NONE', 3,
 ( #21470, #10721, #43754, #22421, #36102, #47115, #15024, #18123, #3261, #40378, #36579, #29898 ),
 .UNSPECIFIED., .F., .F.,
 ( 4, 2, 2, 2, 2, 4 ),
 ( 0.000000000000000000, 0.2500000000000016098, 0.3750000000000012212, 0.5000000000000008882, 0.7500000000000004441, 1.000000000000000000 ),
 .UNSPECIFIED. ) ;
#25414 = PRODUCT_RELATED_PRODUCT_CATEGORY ( 'part', '', ( #20092 ) ) ;
#25416 = CARTESIAN_POINT ( 'NONE',  ( 0.7185039370078739607, 1.928577636452523993E-17, 1.525590551181102317 ) ) ;
#25415 = CARTESIAN_POINT ( 'NONE',  ( -0.5555748031496053896, 0.3833307086614213266, 0.7480314960629921295 ) ) ;
#25417 = CARTESIAN_POINT ( 'NONE',  ( 0.7646288533564489232, -0.1113553986120547346, 0.2214566928058590567 ) ) ;
#25418 = ORIENTED_EDGE ( 'NONE', *, *, #26869, .F. ) ;
#25419 = CARTESIAN_POINT ( 'NONE',  ( 0.9412147342319837628, 0.1574803149606300301, 1.897145669183811778 ) ) ;
#25420 = CARTESIAN_POINT ( 'NONE',  ( -0.7646288533564489232, -0.1113553986120547346, 0.7726377951680629685 ) ) ;
#25421 = CARTESIAN_POINT ( 'NONE',  ( 0.1574803149606300301, -1.535925196742866650, 0.06523048226347956391 ) ) ;
#25422 = CARTESIAN_POINT ( 'NONE',  ( -0.1264236179284866091, -0.6697834645131652831, 0.1264236179284866091 ) ) ;
#25423 = CARTESIAN_POINT ( 'NONE',  ( -0.7185039370078739607, 1.928577636452523993E-17, 0.09842519674286673292 ) ) ;
#25424 = CARTESIAN_POINT ( 'NONE',  ( -0.1574803149606299191, -1.129921259842519676, 0.000000000000000000 ) ) ;
#25425 = CARTESIAN_POINT ( 'NONE',  ( 1.033464566929134687, -0.06523048226347956391, 0.9030511809948348345 ) ) ;
#25426 = DIRECTION ( 'NONE',  ( -0.000000000000000000, 0.7880107536067174623, -0.6156614753256640649 ) ) ;
#25427 = CARTESIAN_POINT ( 'NONE',  ( -0.7495606340400177148, -0.1264236179284866091, 0.4404527558517480901 ) ) ;
#25428 = ORIENTED_EDGE ( 'NONE', *, *, #12423, .T. ) ;
#25429 = ORIENTED_EDGE ( 'NONE', *, *, #44807, .T. ) ;
#25430 = CARTESIAN_POINT ( 'NONE',  ( -0.6971942568897648851, 0.07405724077823318263, 1.540354330654897685 ) ) ;
#25431 = CARTESIAN_POINT ( 'NONE',  ( 0.8019270111902717657, -0.1787899950787401604, 1.510826771599780294 ) ) ;
#25432 = ORIENTED_EDGE ( 'NONE', *, *, #42032, .F. ) ;
#25433 = CARTESIAN_POINT ( 'NONE',  ( -1.002407869896990045, -0.1264236179284866091, 0.7308070865604093802 ) ) ;
#25434 = CARTESIAN_POINT ( 'NONE',  ( 0.7495606340400177148, -0.1264236179284866091, 0.1697834645131657827 ) ) ;
#25435 = CARTESIAN_POINT ( 'NONE',  ( -0.8019270111902716547, -0.1787899950787401604, 0.6397637794737947026 ) ) ;
#25436 = STYLED_ITEM ( 'NONE', ( #46958 ), #36893 ) ;
#25437 = CARTESIAN_POINT ( 'NONE',  ( 0.001477421097695146273, -0.1058998750575174536, 0.09216900433216509980 ) ) ;
#25438 = ( BOUNDED_CURVE ( )  B_SPLINE_CURVE ( 2, ( #28346, #10126, #24735, #662, #21129, #44057, #22250, #4256, #39332 ),
 .UNSPECIFIED., .F., .T. ) 
 B_SPLINE_CURVE_WITH_KNOTS ( ( 3, 2, 2, 2, 3 ),
 ( 0.7299999999999999822, 0.7325000000000000400, 0.7349999999999999867, 0.7375000000000000444, 0.7399999999999999911 ),
 .UNSPECIFIED. ) 
 CURVE ( )  GEOMETRIC_REPRESENTATION_ITEM ( )  RATIONAL_B_SPLINE_CURVE ( ( 1.000000000000000000, 0.9238795325112939549, 1.000000000000000000, 0.9238795325112869605, 1.000000000000000000, 0.9238795325112869605, 1.000000000000000000, 0.9238795325112869605, 1.000000000000000000 ) ) 
 REPRESENTATION_ITEM ( '' )  ) ;
#25439 = VECTOR ( 'NONE', #36892, 39.37007874015748143 ) ;
#25440 = CARTESIAN_POINT ( 'NONE',  ( 0.7185039370078739607, 1.928577636452523993E-17, 0.6496062991050708391 ) ) ;
#25441 = CARTESIAN_POINT ( 'NONE',  ( 2.892866454678787531E-17, -0.2834645668216070891, 0.1574803149606299191 ) ) ;
#25442 = CARTESIAN_POINT ( 'NONE',  ( -0.7646288533564489232, 0.1113553986120547346, 1.825787401467275473 ) ) ;
#25443 = VERTEX_POINT ( 'NONE', #34468 ) ;
#25444 = CARTESIAN_POINT ( 'NONE',  ( 0.7185039370078739607, 1.928577636452523993E-17, 1.643700787401574992 ) ) ;
#25445 = CARTESIAN_POINT ( 'NONE',  ( 0.8019270111902716547, -0.1787899950787401604, 1.432086614119464141 ) ) ;
#25446 = CARTESIAN_POINT ( 'NONE',  ( -0.1736230502038370316, -0.09851383841496653970, -0.005720786448288354628 ) ) ;
#25447 = DIRECTION ( 'NONE',  ( -0.000000000000000000, 0.7880107536067207930, -0.6156614753256598460 ) ) ;
#25448 = VERTEX_POINT ( 'NONE', #16268 ) ;
#25449 = CIRCLE ( 'NONE', #28527, 0.3937007874015747699 ) ;
#25450 = EDGE_CURVE ( 'NONE', #14813, #3281, #11016, .T. ) ;
#25451 = CARTESIAN_POINT ( 'NONE',  ( -0.07405724077823318263, -1.701895621772544942, 0.1787899950787401604 ) ) ;
#25452 = ORIENTED_EDGE ( 'NONE', *, *, #38813, .F. ) ;
#25453 = ADVANCED_FACE ( 'NONE', ( #38290 ), #20312, .T. ) ;
#25454 = ORIENTED_EDGE ( 'NONE', *, *, #22498, .T. ) ;
#25455 = CARTESIAN_POINT ( 'NONE',  ( 0.3980944881889810216, 1.332209862199691841, -0.06082000038405670217 ) ) ;
#25456 = ( BOUNDED_CURVE ( )  B_SPLINE_CURVE ( 2, ( #37487, #19744, #40583, #19270, #37018, #33926, #4171, #8723, #23358 ),
 .UNSPECIFIED., .F., .F. ) 
 B_SPLINE_CURVE_WITH_KNOTS ( ( 3, 2, 2, 2, 3 ),
 ( 0.1049999999999999961, 0.1074999999999999983, 0.1100000000000000006, 0.1125000000000000028, 0.1150000000000000050 ),
 .UNSPECIFIED. ) 
 CURVE ( )  GEOMETRIC_REPRESENTATION_ITEM ( )  RATIONAL_B_SPLINE_CURVE ( ( 1.000000000000000000, 0.9238795325112869605, 1.000000000000000000, 0.9238795325112869605, 1.000000000000000000, 0.9238795325112869605, 1.000000000000000000, 0.9238795325112869605, 1.000000000000000000 ) ) 
 REPRESENTATION_ITEM ( '' )  ) ;
#25457 = CARTESIAN_POINT ( 'NONE',  ( 0.07405724077823318263, -0.3720472440407247561, -0.1787899950787401604 ) ) ;
#25458 = CARTESIAN_POINT ( 'NONE',  ( -0.07405724077823318263, -0.8986220471903317852, 0.1787899950787401604 ) ) ;
#25459 = CARTESIAN_POINT ( 'NONE',  ( 0.7185039370078739607, 1.928577636452523993E-17, 1.840551181102362266 ) ) ;
#25460 = ( LENGTH_UNIT ( ) NAMED_UNIT ( * ) SI_UNIT ( $, .METRE. ) ) ;
#25461 = CARTESIAN_POINT ( 'NONE',  ( 0.6971942568897648851, -0.07405724077823297447, 1.737204724355685848 ) ) ;
#25462 = CARTESIAN_POINT ( 'NONE',  ( 0.1797182628040039365, -0.2175634946224157540, -2.200913952912460540E-17 ) ) ;
#25463 = CARTESIAN_POINT ( 'NONE',  ( -0.07405724077823318263, -0.08772239342608903478, 0.1787899950787401604 ) ) ;
#25464 = CARTESIAN_POINT ( 'NONE',  ( 3.284318927891251994E-17, -0.2662401574265516047, 0.1787899950787401882 ) ) ;
#25465 = CARTESIAN_POINT ( 'NONE',  ( 0.1264236179284866091, -0.05954724404072461036, -0.1264236179284866091 ) ) ;
#25466 = CARTESIAN_POINT ( 'NONE',  ( 1.033464566929133799, 1.928577636452524610E-17, 4.498031496062992574 ) ) ;
#25467 = CARTESIAN_POINT ( 'NONE',  ( 1.054774247047244540, -0.07405724077823318263, 0.6102362204186774219 ) ) ;
#25468 = CIRCLE ( 'NONE', #20853, 0.08090551181102362266 ) ;
#25470 = CARTESIAN_POINT ( 'NONE',  ( 0.000000000000000000, -1.360801781844024705E-15, 0.9783464566929289674 ) ) ;
#25469 = CARTESIAN_POINT ( 'NONE',  ( -0.9160508336777043459, 0.1674337118376148514, 0.03937007874015843040 ) ) ;
#25471 = CARTESIAN_POINT ( 'NONE',  ( 0.1797182628040039087, -1.671795778086982098, -0.07444174185955065859 ) ) ;
#25472 = CARTESIAN_POINT ( 'NONE',  ( 3.284318927891251994E-17, -0.4237204723871811352, 0.1787899950787401882 ) ) ;
#25473 = CARTESIAN_POINT ( 'NONE',  ( -1.033464566929133799, 0.000000000000000000, 1.299212598317669221 ) ) ;
#25474 = CARTESIAN_POINT ( 'NONE',  ( 1.054774247047244096, 0.000000000000000000, 1.601870078686393750 ) ) ;
#25476 = CARTESIAN_POINT ( 'NONE',  ( 0.7185039370078766252, -0.06523048226348168721, 1.872539369971213619 ) ) ;
#25475 = DIRECTION ( 'NONE',  ( 1.000000000000000000, -3.469446951953614189E-15, 0.000000000000000000 ) ) ;
#25477 = CARTESIAN_POINT ( 'NONE',  ( 1.002407869896990045, -0.1264236179284866091, 0.4896653542769449086 ) ) ;
#25478 = EDGE_LOOP ( 'NONE', ( #20993, #43020, #11755, #5105, #22588 ) ) ;
#25479 = CIRCLE ( 'NONE', #1736, 0.09842519685039370636 ) ;
#25480 = ORIENTED_EDGE ( 'NONE', *, *, #17197, .T. ) ;
#25481 = CARTESIAN_POINT ( 'NONE',  ( 0.7185039370078746268, -0.06523048226347956391, 0.03198818897637801389 ) ) ;
#25482 = DIRECTION ( 'NONE',  ( 0.000000000000000000, 0.9771240687918540946, 0.2126700594527874133 ) ) ;
#25483 = DIRECTION ( 'NONE',  ( 0.000000000000000000, -1.000000000000000000, 0.000000000000000000 ) ) ;
#25484 = CARTESIAN_POINT ( 'NONE',  ( -0.1787899950787401604, -0.2047244093950554844, -0.07405724077823318263 ) ) ;
#25486 = DIRECTION ( 'NONE',  ( -1.000000000000000000, 0.000000000000000000, 0.000000000000000000 ) ) ;
#25485 = CARTESIAN_POINT ( 'NONE',  ( -0.9500414927467378812, 0.1787899950787401604, 0.4281496062454490659 ) ) ;
#25487 = CARTESIAN_POINT ( 'NONE',  ( -0.1264236179284866091, -1.107775590497417362, -0.1264236179284866091 ) ) ;
#25488 = CARTESIAN_POINT ( 'NONE',  ( 0.7495606340400177148, 0.1264236179284866091, 0.04183070860765386589 ) ) ;
#25489 = DIRECTION ( 'NONE',  ( 0.000000000000000000, 0.000000000000000000, -1.000000000000000000 ) ) ;
#25490 = CARTESIAN_POINT ( 'NONE',  ( -0.8759842519685039353, 0.1787899950787401882, 1.606791338528913426 ) ) ;
#25491 = ORIENTED_EDGE ( 'NONE', *, *, #28993, .T. ) ;
#25492 = CIRCLE ( 'NONE', #5587, 0.09842519685039310962 ) ;
#25493 = CARTESIAN_POINT ( 'NONE',  ( -0.8759842519685039353, 0.1787899950787401882, 1.099901574749385880 ) ) ;
#25494 = CARTESIAN_POINT ( 'NONE',  ( -0.3042596054108610559, -0.05980719604265496286, -0.7196201501354283492 ) ) ;
#25495 = CARTESIAN_POINT ( 'NONE',  ( 1.054774247047244540, 0.07405724077823318263, 1.131889763725763665 ) ) ;
#25496 = B_SPLINE_CURVE_WITH_KNOTS ( 'NONE', 3,
 ( #9107, #41661, #9585, #34764, #16543, #31170, #31406, #13190, #35232, #24204, #27826, #5966, #20585, #21050, #14117, #42835, #33055, #35912, #10531, #7152, #29257, #32094, #21775 ),
 .UNSPECIFIED., .F., .F.,
 ( 4, 2, 2, 1, 1, 1, 2, 2, 2, 1, 1, 2, 2, 4 ),
 ( 0.000000000000000000, 0.2500000000000006106, 0.3750000000000008327, 0.4375000000000010547, 0.4687500000000012212, 0.4843750000000014433, 0.4921875000000014988, 0.5000000000000014433, 0.6250000000000012212, 0.6875000000000011102, 0.7187500000000009992, 0.7343750000000007772, 0.7500000000000005551, 1.000000000000000000 ),
 .UNSPECIFIED. ) ;
#25497 = CARTESIAN_POINT ( 'NONE',  ( 0.6971942568897648851, -0.07405724077823297447, 1.776574803095843924 ) ) ;
#25498 = CARTESIAN_POINT ( 'NONE',  ( -0.8759842519685039353, -0.1574803149606299191, 0.6299212598425196763 ) ) ;
#25499 = CARTESIAN_POINT ( 'NONE',  ( -0.6971942568897637749, 2.189545951927499583E-17, 1.104822834591905556 ) ) ;
#25500 = FACE_OUTER_BOUND ( 'NONE', #27222, .T. ) ;
#25501 = CARTESIAN_POINT ( 'NONE',  ( -0.07097307671285064956, -0.2545179073170276141, -0.04495255068434172996 ) ) ;
#25502 = CARTESIAN_POINT ( 'NONE',  ( 1.054774247047244540, 0.07405724077823318263, 0.3444881889226146243 ) ) ;
#25503 = CARTESIAN_POINT ( 'NONE',  ( -1.002407869896990045, -0.1264236179284866091, 0.2534448818360003908 ) ) ;
#25504 = CARTESIAN_POINT ( 'NONE',  ( -0.6971942568897637749, 2.189545951927499583E-17, 0.7504921259304880854 ) ) ;
#25505 = CARTESIAN_POINT ( 'NONE',  ( 1.033464566929134687, -0.06523048226347956391, 1.651082677057826853 ) ) ;
#25506 = EDGE_LOOP ( 'NONE', ( #15181, #34824, #46871, #32390 ) ) ;
#25507 = CARTESIAN_POINT ( 'NONE',  ( -0.1264236179284866091, -0.03986220467064590517, 0.1264236179284866091 ) ) ;
#25508 = ORIENTED_EDGE ( 'NONE', *, *, #45760, .F. ) ;
#25509 = CARTESIAN_POINT ( 'NONE',  ( 0.7495606340400177148, 0.1264236179284866091, 0.8686023621509606496 ) ) ;
#25510 = CARTESIAN_POINT ( 'NONE',  ( 0.8759842519685039353, 0.1787899950787401882, 1.060531496009228247 ) ) ;
#25511 = CARTESIAN_POINT ( 'NONE',  ( -1.054774247047244540, 0.07405724077823318263, 1.835629921206078485 ) ) ;
#25512 = EDGE_CURVE ( 'NONE', #16719, #752, #5699, .T. ) ;
#25513 = CARTESIAN_POINT ( 'NONE',  ( 0.6971942568897648851, -0.07405724077823297447, 1.934055118056471567 ) ) ;
#25514 = EDGE_CURVE ( 'NONE', #4077, #3165, #23273, .T. ) ;
#25515 = STYLED_ITEM ( 'NONE', ( #4152 ), #36032 ) ;
#25516 = CARTESIAN_POINT ( 'NONE',  ( 0.5358894627757212481, 0.09842519685039370636, 0.000000000000000000 ) ) ;
#25517 = CARTESIAN_POINT ( 'NONE',  ( 0.07405724077823318263, -1.224533417048137451, 0.1787899950787401604 ) ) ;
#25518 = ORIENTED_EDGE ( 'NONE', *, *, #11475, .F. ) ;
#25519 = CARTESIAN_POINT ( 'NONE',  ( -0.1787899950787401604, -0.3129921259304885850, 0.07405724077823318263 ) ) ;
#25520 = ADVANCED_FACE ( 'NONE', ( #12193 ), #26819, .F. ) ;
#25521 = DIRECTION ( 'NONE',  ( -1.000000000000000000, 0.000000000000000000, 0.000000000000000000 ) ) ;
#25522 = ORIENTED_EDGE ( 'NONE', *, *, #25029, .F. ) ;
#25523 = CARTESIAN_POINT ( 'NONE',  ( 0.9500414927467378812, -0.1787899950787401604, 1.235236220418678199 ) ) ;
#25524 = PRODUCT_DEFINITION_FORMATION_WITH_SPECIFIED_SOURCE ( 'ANY', '', #26085, .NOT_KNOWN. ) ;
#25525 = VECTOR ( 'NONE', #4384, 39.37007874015748854 ) ;
#25526 = EDGE_CURVE ( 'NONE', #24855, #39709, #3029, .T. ) ;
#25527 = CARTESIAN_POINT ( 'NONE',  ( 0.1574803149606299191, 0.9876813667277579700, 0.7893767492247204531 ) ) ;
#25528 = CARTESIAN_POINT ( 'NONE',  ( 0.2204724409448818867, -0.07955613945526318620, 0.1377952755905511861 ) ) ;
#25529 = VECTOR ( 'NONE', #9219, 39.37007874015748143 ) ;
#25530 = CARTESIAN_POINT ( 'NONE',  ( 1.033464566929133799, 0.000000000000000000, 1.938976377952756014 ) ) ;
#25531 = CARTESIAN_POINT ( 'NONE',  ( 0.1787899950787401882, -1.678641732229700922, -2.189545951927503898E-17 ) ) ;
#25532 = CARTESIAN_POINT ( 'NONE',  ( -0.1264236179284866091, -1.649114173174582643, 0.1264236179284866091 ) ) ;
#25533 = CARTESIAN_POINT ( 'NONE',  ( -0.8759842519685039353, 0.1787899950787401882, 0.5487204723871811352 ) ) ;
#25534 = CARTESIAN_POINT ( 'NONE',  ( -0.1545411696117860445, -0.09842519685039370636, -0.08990488994085453489 ) ) ;
#25535 = CARTESIAN_POINT ( 'NONE',  ( 0.1555687797274980522, -0.09281549603114055969, 0.1148293963254594513 ) ) ;
#25536 = CARTESIAN_POINT ( 'NONE',  ( 0.8019270111902717657, -0.1787899950787401604, 1.195866141678520345 ) ) ;
#25537 = CARTESIAN_POINT ( 'NONE',  ( 1.054774247047244540, -0.07405724077823318263, 1.673228346402929834 ) ) ;
#25538 = CARTESIAN_POINT ( 'NONE',  ( -0.9412147342319837628, 0.1574803149606300301, 1.906988188976377563 ) ) ;
#25539 = CARTESIAN_POINT ( 'NONE',  ( 1.928577636452524610E-17, -0.09842519685039370636, -0.1574803149606299191 ) ) ;
#25540 = CARTESIAN_POINT ( 'NONE',  ( 0.2204724409448818867, -0.1591122789105269553, 0.000000000000000000 ) ) ;
#25541 = CARTESIAN_POINT ( 'NONE',  ( -0.7185039370078746268, -0.06523048226347956391, 1.016240157480315487 ) ) ;
#25542 = CARTESIAN_POINT ( 'NONE',  ( -0.7646288533564489232, -0.1113553986120547346, 1.678149606191684962 ) ) ;
#25543 = CARTESIAN_POINT ( 'NONE',  ( 0.6971942568897626646, -0.07405724077823297447, 0.1230314960092287191 ) ) ;
#25544 = CARTESIAN_POINT ( 'NONE',  ( 0.7130838980242285574, -0.05254116306688896842, 0.03937007909647829984 ) ) ;
#25545 = CARTESIAN_POINT ( 'NONE',  ( -0.7185039370078714072, 0.06523048226347728795, 1.828248031388537198 ) ) ;
#25546 = CARTESIAN_POINT ( 'NONE',  ( 1.033464566929133799, 0.000000000000000000, 1.230314960629921295 ) ) ;
#25547 = CARTESIAN_POINT ( 'NONE',  ( 0.8107537697050253289, 0.1574803149606300301, 0.5634842518609766149 ) ) ;
#25548 = VERTEX_POINT ( 'NONE', #39456 ) ;
#25549 = CARTESIAN_POINT ( 'NONE',  ( 0.8565624266329610048, 0.1746252292145809570, 0.03937093662838074548 ) ) ;
#25550 = CARTESIAN_POINT ( 'NONE',  ( -0.8759842519685039353, -0.1574803149606299191, 0.3838582676090082635 ) ) ;
#25551 = CARTESIAN_POINT ( 'NONE',  ( 0.003086919931961261236, 0.03878710687431414367, 0.1377952978224512848 ) ) ;
#25552 = CARTESIAN_POINT ( 'NONE',  ( 0.7495606340400177148, -0.1264236179284866091, 1.424704724355685181 ) ) ;
#25553 = CARTESIAN_POINT ( 'NONE',  ( -0.9412147342319837628, 0.1574803149606300301, 1.158956692913385655 ) ) ;
#25554 = CARTESIAN_POINT ( 'NONE',  ( 0.9412147342319837628, 0.1574803149606300301, 1.670767716535433545 ) ) ;
#25555 = CARTESIAN_POINT ( 'NONE',  ( 0.1787899950787401604, -0.1358267715997797664, -0.07405724077823318263 ) ) ;
#25556 = ORIENTED_EDGE ( 'NONE', *, *, #8935, .F. ) ;
#25557 = CARTESIAN_POINT ( 'NONE',  ( 1.033464566929134687, 0.06523048226347956391, 0.7209645669291341319 ) ) ;
#25558 = CARTESIAN_POINT ( 'NONE',  ( -1.033464566929133799, 1.928577636452524610E-17, 2.869337061179095023E-17 ) ) ;
#25559 = FACE_OUTER_BOUND ( 'NONE', #7638, .T. ) ;
#25560 = CARTESIAN_POINT ( 'NONE',  ( 0.4330708661417322913, 0.1574803149606299191, -0.9891732283464564901 ) ) ;
#25561 = CARTESIAN_POINT ( 'NONE',  ( 0.8759842519685039353, -0.1787899950787401882, 0.6471456692375747721 ) ) ;
#25562 = VERTEX_POINT ( 'NONE', #45942 ) ;
#25563 = CARTESIAN_POINT ( 'NONE',  ( -0.7495606340400177148, 0.1264236179284866091, 1.454232283410803017 ) ) ;
#25564 = CARTESIAN_POINT ( 'NONE',  ( -0.1574803149606299191, 0.1003937008949285503, 0.000000000000000000 ) ) ;
#25565 = CARTESIAN_POINT ( 'NONE',  ( -0.9500414927467378812, -0.1787899950787401604, 1.161417322780881278 ) ) ;
#25566 = CARTESIAN_POINT ( 'NONE',  ( -1.054774247047244096, 0.000000000000000000, 1.124507873961984261 ) ) ;
#25567 = ADVANCED_FACE ( 'NONE', ( #5928 ), #2557, .T. ) ;
#25568 = CARTESIAN_POINT ( 'NONE',  ( -0.1711365707896517763, 0.1966896243421524526, -0.3121915932859947174 ) ) ;
#25569 = CARTESIAN_POINT ( 'NONE',  ( -1.002407869896990045, -0.1264236179284866091, 0.2189960629383626012 ) ) ;
#25570 = CARTESIAN_POINT ( 'NONE',  ( 0.9873396505805591694, 0.1113553986120547346, 0.7923228345381417848 ) ) ;
#25571 = CARTESIAN_POINT ( 'NONE',  ( -0.07405724077823318263, -0.8357538894890804704, 0.1787899950787401604 ) ) ;
#25572 = ORIENTED_EDGE ( 'NONE', *, *, #40135, .F. ) ;
#25573 = CARTESIAN_POINT ( 'NONE',  ( -1.033464566929134687, 0.06523048226347956391, 0.05167322834645669133 ) ) ;
#25574 = FACE_OUTER_BOUND ( 'NONE', #30475, .T. ) ;
#25575 = ORIENTED_EDGE ( 'NONE', *, *, #141, .F. ) ;
#25576 = ORIENTED_EDGE ( 'NONE', *, *, #39112, .F. ) ;
#25577 = EDGE_CURVE ( 'NONE', #35449, #815, #38845, .T. ) ;
#25578 = DIRECTION ( 'NONE',  ( -1.000000000000000000, 0.000000000000000000, 0.000000000000000000 ) ) ;
#25579 = CARTESIAN_POINT ( 'NONE',  ( -0.6971942568897626646, 0.07405724077823318263, 0.7874015747493863238 ) ) ;
#25580 = ( BOUNDED_CURVE ( )  B_SPLINE_CURVE ( 2, ( #5922, #35868, #6142, #24848, #2089, #17653, #27779, #9294, #20769 ),
 .UNSPECIFIED., .F., .T. ) 
 B_SPLINE_CURVE_WITH_KNOTS ( ( 3, 2, 2, 2, 3 ),
 ( 0.6600000000000000311, 0.6624999999999999778, 0.6650000000000000355, 0.6674999999999999822, 0.6700000000000000400 ),
 .UNSPECIFIED. ) 
 CURVE ( )  GEOMETRIC_REPRESENTATION_ITEM ( )  RATIONAL_B_SPLINE_CURVE ( ( 1.000000000000000000, 0.9238795325112869605, 1.000000000000000000, 0.9238795325112869605, 1.000000000000000000, 0.9238795325112869605, 1.000000000000000000, 0.9238795325112829637, 1.000000000000000000 ) ) 
 REPRESENTATION_ITEM ( '' )  ) ;
#25581 = DIRECTION ( 'NONE',  ( -0.000000000000000000, 1.000000000000000000, -0.000000000000000000 ) ) ;
#25582 = ORIENTED_EDGE ( 'NONE', *, *, #36437, .F. ) ;
#25583 = CARTESIAN_POINT ( 'NONE',  ( -0.7495606340400177148, 0.1264236179284866091, 1.774114173174582643 ) ) ;
#25584 = CARTESIAN_POINT ( 'NONE',  ( 0.9873396505805591694, -0.1113553986120547346, 0.7135826771653542844 ) ) ;
#25585 = CARTESIAN_POINT ( 'NONE',  ( -0.07444174185955065859, -0.8351816048586360175, -0.1797182628040039087 ) ) ;
#25586 = DIRECTION ( 'NONE',  ( 0.000000000000000000, 0.000000000000000000, -1.000000000000000000 ) ) ;
#25587 = CARTESIAN_POINT ( 'NONE',  ( -1.033464566929133799, 0.000000000000000000, 1.574803149498771537 ) ) ;
#25588 = VECTOR ( 'NONE', #3340, 39.37007874015748143 ) ;
#25589 = CARTESIAN_POINT ( 'NONE',  ( 1.054774247047244096, 0.000000000000000000, 0.7357283464029290565 ) ) ;
#25590 = DIRECTION ( 'NONE',  ( 0.000000000000000000, 0.9771240687918510970, 0.2126700594528006527 ) ) ;
#25591 = CARTESIAN_POINT ( 'NONE',  ( -0.2559055118110235005, 0.1248284115715151549, -0.08765918451895586549 ) ) ;
#25592 = CARTESIAN_POINT ( 'NONE',  ( 0.7185039370078739607, 1.928577636452523993E-17, 1.368110236220472675 ) ) ;
#25594 = CARTESIAN_POINT ( 'NONE',  ( 0.1574803149606300301, 0.1176181103437476255, 0.06523048226347956391 ) ) ;
#25593 = CARTESIAN_POINT ( 'NONE',  ( 0.8559655446573316562, -0.1727717671435132496, 1.987845004397921445 ) ) ;
#25595 = CARTESIAN_POINT ( 'NONE',  ( 0.9873396505805591694, -0.1113553986120547346, 1.491141732175936818 ) ) ;
#25596 = EDGE_CURVE ( 'NONE', #46651, #46167, #9703, .T. ) ;
#25597 = ORIENTED_EDGE ( 'NONE', *, *, #5235, .F. ) ;
#25599 = CARTESIAN_POINT ( 'NONE',  ( 0.1574803149606299746, -5.122214988120488358E-16, -8.878505979408856939E-16 ) ) ;
#25598 = CARTESIAN_POINT ( 'NONE',  ( 0.7495606340400177148, 0.1264236179284866091, 0.7455708660879684091 ) ) ;
#25600 = CARTESIAN_POINT ( 'NONE',  ( -0.1264236179284866091, -0.7042322834108031282, 0.1264236179284866091 ) ) ;
#25601 = CARTESIAN_POINT ( 'NONE',  ( -1.033464566929133799, 0.000000000000000000, 0.3937007872940476716 ) ) ;
#25602 = CARTESIAN_POINT ( 'NONE',  ( 0.1624141299553157614, 0.07987677361383865859, 0.1383529584519434252 ) ) ;
#25603 = CARTESIAN_POINT ( 'NONE',  ( -0.2471922904502826812, 0.03219022224904106305, 0.1427165354330708902 ) ) ;
#25604 = CARTESIAN_POINT ( 'NONE',  ( 0.7495606340400177148, -0.1264236179284866091, 0.9916338582139527791 ) ) ;
#25605 = DIRECTION ( 'NONE',  ( 0.000000000000000000, 0.000000000000000000, 1.000000000000000000 ) ) ;
#25606 = CARTESIAN_POINT ( 'NONE',  ( 0.06523048226347956391, -1.535925196850394636, -0.1574803149606300301 ) ) ;
#25607 = LINE ( 'NONE', #13857, #20651 ) ;
#25608 = EDGE_LOOP ( 'NONE', ( #41835, #15245, #46916, #67 ) ) ;
#25609 = CARTESIAN_POINT ( 'NONE',  ( -1.054774247047244540, 0.07405724077823318263, 0.02460629915883492599 ) ) ;
#25610 = ORIENTED_EDGE ( 'NONE', *, *, #42114, .T. ) ;
#25611 = CARTESIAN_POINT ( 'NONE',  ( -0.8107537697050254399, 0.1574803149606300301, 0.6126968503937006982 ) ) ;
#25612 = ORIENTED_EDGE ( 'NONE', *, *, #34278, .F. ) ;
#25613 = CONICAL_SURFACE ( 'NONE', #16439, 0.2471922904502826812, 0.5235987755982992597 ) ;
#25614 = CARTESIAN_POINT ( 'NONE',  ( -0.7185039370078739607, 1.928577636452523993E-17, 1.840551181102362266 ) ) ;
#25615 = CARTESIAN_POINT ( 'NONE',  ( -0.6971942568897648851, 0.07405724077823318263, 1.653543307032850462 ) ) ;
#25616 = CARTESIAN_POINT ( 'NONE',  ( -0.6971942568897648851, -0.07405724077823297447, 1.107283464513165949 ) ) ;
#25617 = EDGE_CURVE ( 'NONE', #14162, #3991, #11033, .T. ) ;
#25618 = CARTESIAN_POINT ( 'NONE',  ( -1.033464566929134687, -0.06523048226347956391, 0.1648622047244094890 ) ) ;
#25619 = CARTESIAN_POINT ( 'NONE',  ( 0.9500414927467378812, 0.1787899950787401604, 0.06889763774151215492 ) ) ;
#25620 = CLOSED_SHELL ( 'NONE', ( #4357, #23447, #22893, #36329, #46196, #45395, #22223, #45736, #11065, #21000, #10302, #15170, #189, #14615, #18852, #44607, #15271, #23392, #28832, #13476, #32400, #5114, #24960, #11368, #33300, #45485, #45270, #33583, #14350, #42028, #24460, #4977, #36235, #39693, #30029, #30143, #19585, #3468, #29914, #21791, #19847, #40249, #9814, #28936, #3338, #24103, #25338, #28157, #1670, #21967, #3247, #27243, #40023, #24217, #10052, #21761, #11347, #41354, #6915, #45642, #1564, #12136, #36044, #36639, #22124, #31252, #4594, #15727, #1674, #40020, #13750, #27586, #3783, #38826, #31078, #45572, #8547, #15384, #37165, #42361, #10854, #18935, #39787, #31417, #12312, #37097, #31681, #10297, #17651, #47235, #32664, #26212, #42173, #16362, #38298, #25879, #15065, #32304, #34946, #44838, #13532 ) ) ;
#25621 = CARTESIAN_POINT ( 'NONE',  ( -0.1673228346456692994, 0.06415291647593684976, -0.1630605872086742514 ) ) ;
#25622 = CARTESIAN_POINT ( 'NONE',  ( -0.1787899950787401604, -0.3682342044497113887, 0.07405724077823318263 ) ) ;
#25623 = CARTESIAN_POINT ( 'NONE',  ( -0.1604209458837513869, -0.09842519685039370636, 0.05490810003033267522 ) ) ;
#25624 = DIRECTION ( 'NONE',  ( 0.000000000000000000, 0.000000000000000000, -1.000000000000000000 ) ) ;
#25625 = CARTESIAN_POINT ( 'NONE',  ( 0.1574803149606299191, 0.3740157480314960647, 0.9783464566929134243 ) ) ;
#25626 = ADVANCED_FACE ( 'NONE', ( #6396, #25090 ), #9777, .F. ) ;
#25627 = CARTESIAN_POINT ( 'NONE',  ( -0.7495606340400177148, -0.1264236179284866091, 0.3223425196312759144 ) ) ;
#25628 = ORIENTED_EDGE ( 'NONE', *, *, #33855, .T. ) ;
#25629 = CARTESIAN_POINT ( 'NONE',  ( 0.2471908670705635913, -0.09572725253288331959, 0.02814577918614308283 ) ) ;
#25630 = VERTEX_POINT ( 'NONE', #43044 ) ;
#25631 = CARTESIAN_POINT ( 'NONE',  ( -0.9500414927467377701, 0.1787899950787401604, 1.412401574749386990 ) ) ;
#25632 = ORIENTED_EDGE ( 'NONE', *, *, #1730, .F. ) ;
#25633 = CARTESIAN_POINT ( 'NONE',  ( 0.1264236179284866091, -1.250492125930488196, 0.1264236179284866091 ) ) ;
#25634 = CARTESIAN_POINT ( 'NONE',  ( -0.1264236179284866091, -1.412893700733637958, 0.1264236179284866091 ) ) ;
#25635 = ( NAMED_UNIT ( * ) SI_UNIT ( $, .STERADIAN. ) SOLID_ANGLE_UNIT ( ) ) ;
#25636 = CARTESIAN_POINT ( 'NONE',  ( 0.9412147342319837628, 0.1574803149606300301, 0.3715551181102361711 ) ) ;
#25637 = LINE ( 'NONE', #11730, #15623 ) ;
#25638 = CARTESIAN_POINT ( 'NONE',  ( -0.7646288533564489232, 0.1113553986120547346, 0.9202755904436535905 ) ) ;
#25639 = CARTESIAN_POINT ( 'NONE',  ( 0.9500414927467378812, -0.1787899950787401604, 0.4133858267178901480 ) ) ;
#25640 = CARTESIAN_POINT ( 'NONE',  ( -0.1574803149606299191, -0.1850393700787401619, 0.000000000000000000 ) ) ;
#25641 = STYLED_ITEM ( 'NONE', ( #8813 ), #5043 ) ;
#25642 = CARTESIAN_POINT ( 'NONE',  ( 0.7185039370078739607, 1.928577636452523993E-17, 1.830708661309795149 ) ) ;
#25643 = CARTESIAN_POINT ( 'NONE',  ( -0.1787899950787401882, -0.2022637794737956740, 0.000000000000000000 ) ) ;
#25644 = FACE_OUTER_BOUND ( 'NONE', #39760, .T. ) ;
#25645 = CARTESIAN_POINT ( 'NONE',  ( 0.8759842519685039353, 0.1574803149606299191, 1.003937007874015741 ) ) ;
#25646 = DIRECTION ( 'NONE',  ( 1.000000000000000000, -3.469446951953625627E-15, -0.000000000000000000 ) ) ;
#25648 = CARTESIAN_POINT ( 'NONE',  ( -0.6195511811023656223, 0.9842519685039370358, -1.186023622047243986 ) ) ;
#25647 = CARTESIAN_POINT ( 'NONE',  ( 0.7185039370078739607, 1.928577636452523993E-17, 1.013779527559055094 ) ) ;
#25649 = CARTESIAN_POINT ( 'NONE',  ( 0.5358894627757212481, 4.766607801171850497E-17, 0.000000000000000000 ) ) ;
#25650 = ORIENTED_EDGE ( 'NONE', *, *, #47402, .T. ) ;
#25651 = ORIENTED_EDGE ( 'NONE', *, *, #45584, .F. ) ;
#25652 = CARTESIAN_POINT ( 'NONE',  ( 0.8759842519685039353, 0.000000000000000000, 4.498031496062992574 ) ) ;
#25653 = CARTESIAN_POINT ( 'NONE',  ( 0.2821522309711287368, 4.616380251121755931E-17, 0.000000000000000000 ) ) ;
#25654 = CARTESIAN_POINT ( 'NONE',  ( 0.1787899950787401882, -1.594980314906866203, -2.189545951927503898E-17 ) ) ;
#25655 = CARTESIAN_POINT ( 'NONE',  ( -0.06523048226347956391, -1.560531495955465253, -0.1574803149606300301 ) ) ;
#25657 = CARTESIAN_POINT ( 'NONE',  ( 0.1787899950787401882, -0.6943897637257637756, -2.189545951927503898E-17 ) ) ;
#25656 = CARTESIAN_POINT ( 'NONE',  ( -0.06523048226347956391, -1.009350393593261064, -0.1574803149606300301 ) ) ;
#25658 = CARTESIAN_POINT ( 'NONE',  ( 0.3849708276051176936, 4.766607801171850497E-17, 0.000000000000000000 ) ) ;
#25659 = CARTESIAN_POINT ( 'NONE',  ( -0.1574803149606299191, -1.051181102362204856, 0.000000000000000000 ) ) ;
#25660 = CARTESIAN_POINT ( 'NONE',  ( 0.8759842519685039353, -0.1574803149606299191, 0.9744094487113701408 ) ) ;
#25661 = CARTESIAN_POINT ( 'NONE',  ( 0.3425196850393700809, 0.08090551181102362266, 0.000000000000000000 ) ) ;
#25662 = ORIENTED_EDGE ( 'NONE', *, *, #38469, .F. ) ;
#25663 = EDGE_LOOP ( 'NONE', ( #39370, #42027, #19371, #8418 ) ) ;
#25664 = CARTESIAN_POINT ( 'NONE',  ( -0.8759842519685039353, 0.1787899950787401882, 1.572342519631275692 ) ) ;
#25665 = ORIENTED_EDGE ( 'NONE', *, *, #41740, .T. ) ;
#25666 = EDGE_CURVE ( 'NONE', #31512, #15464, #25722, .T. ) ;
#25667 = CARTESIAN_POINT ( 'NONE',  ( 0.6971942568897637749, 2.189545951927499583E-17, 1.739665354276945131 ) ) ;
#25668 = ADVANCED_FACE ( 'NONE', ( #46646, #10251 ), #8049, .T. ) ;
#25669 = CARTESIAN_POINT ( 'NONE',  ( -0.06523048226347956391, -1.324311023514519459, -0.1574803149606300301 ) ) ;
#25670 = CARTESIAN_POINT ( 'NONE',  ( -0.8759842519685039353, -0.1787899950787401882, 0.8046259841982047467 ) ) ;
#25671 = CARTESIAN_POINT ( 'NONE',  ( 1.054774247047244540, -0.07405724077823318263, 0.2608267715997796832 ) ) ;
#25672 = DIRECTION ( 'NONE',  ( 1.822029033848725028E-16, 0.000000000000000000, 1.000000000000000000 ) ) ;
#25673 = CARTESIAN_POINT ( 'NONE',  ( -0.8759842519685039353, -0.1787899950787401882, 0.7603346456155274380 ) ) ;
#25674 = FACE_OUTER_BOUND ( 'NONE', #8022, .T. ) ;
#25675 = ADVANCED_FACE ( 'NONE', ( #36595 ), #47376, .F. ) ;
#25676 = CARTESIAN_POINT ( 'NONE',  ( -0.7185039370078746268, -0.06523048226347956391, 0.8587598425196851792 ) ) ;
#25677 = CARTESIAN_POINT ( 'NONE',  ( -1.002407869896990045, -0.1264236179284866091, 1.557578740103716441 ) ) ;
#25678 = CARTESIAN_POINT ( 'NONE',  ( -0.9412147342319837628, 0.1574803149606300301, 1.818405511703498068 ) ) ;
#25679 = VERTEX_POINT ( 'NONE', #15263 ) ;
#25680 = CIRCLE ( 'NONE', #4983, 0.009842519685039376881 ) ;
#25681 = AXIS2_PLACEMENT_3D ( 'NONE', #39965, #3074, #29262 ) ;
#25682 = CARTESIAN_POINT ( 'NONE',  ( -0.7646288533564489232, 0.1113553986120547346, 1.638779527559055316 ) ) ;
#25683 = DIRECTION ( 'NONE',  ( 0.000000000000000000, 0.000000000000000000, -1.000000000000000000 ) ) ;
#25684 = CARTESIAN_POINT ( 'NONE',  ( 1.054774247047244540, 0.07405724077823318263, 1.525590551127339989 ) ) ;
#25685 = CARTESIAN_POINT ( 'NONE',  ( -0.1585677771909188849, -0.09851383642568464771, -0.08159708949282913626 ) ) ;
#25686 = CARTESIAN_POINT ( 'NONE',  ( -1.033464566929133799, 0.000000000000000000, 0.3543307085538902057 ) ) ;
#25687 = AXIS2_PLACEMENT_3D ( 'NONE', #21123, #18248, #29329 ) ;
#25688 = VECTOR ( 'NONE', #16589, 39.37007874015748143 ) ;
#25689 = ORIENTED_EDGE ( 'NONE', *, *, #31097, .T. ) ;
#25690 = ADVANCED_FACE ( 'NONE', ( #139 ), #44000, .T. ) ;
#25691 = EDGE_LOOP ( 'NONE', ( #16529, #27816, #1050, #45866 ) ) ;
#25692 = CARTESIAN_POINT ( 'NONE',  ( 0.000000000000000000, 0.000000000000000000, 0.000000000000000000 ) ) ;
#25693 = DIRECTION ( 'NONE',  ( 3.469446951953620894E-15, 1.000000000000000000, 0.000000000000000000 ) ) ;
#25694 = CARTESIAN_POINT ( 'NONE',  ( 0.1787899950787401604, -0.3769685038832444324, -0.07405724077823318263 ) ) ;
#25695 = CARTESIAN_POINT ( 'NONE',  ( 3.284318927891251994E-17, -0.8961614172690708369, 0.1787899950787401882 ) ) ;
#25696 = CARTESIAN_POINT ( 'NONE',  ( 0.8759842519685039353, 0.1574803149606299191, 1.043307086614173151 ) ) ;
#25697 = FACE_OUTER_BOUND ( 'NONE', #13525, .T. ) ;
#25698 = CARTESIAN_POINT ( 'NONE',  ( 0.7495606340400177148, -0.1264236179284866091, 1.779035433017102319 ) ) ;
#25699 = CARTESIAN_POINT ( 'NONE',  ( 0.07444174185955065859, -0.1462052269058802256, 0.1797182628040039087 ) ) ;
#25700 = CARTESIAN_POINT ( 'NONE',  ( 0.1264236179284866091, -0.1590806611426246187, 0.1264236179284866091 ) ) ;
#25701 = CARTESIAN_POINT ( 'NONE',  ( -0.1264236179284866091, -0.3203740156942680994, -0.1264236179284866091 ) ) ;
#25702 = CARTESIAN_POINT ( 'NONE',  ( -0.07405724077823318263, -0.1161417322297011862, 0.1787899950787401604 ) ) ;
#25703 = AXIS2_PLACEMENT_3D ( 'NONE', #16921, #17155, #31563 ) ;
#25704 = CARTESIAN_POINT ( 'NONE',  ( 1.054774247047244096, 0.000000000000000000, 0.6914370078202519698 ) ) ;
#25706 = CYLINDRICAL_SURFACE ( 'NONE', #30824, 0.3937007874015748254 ) ;
#25705 = CARTESIAN_POINT ( 'NONE',  ( -1.023926211165723021, 0.06782980145170247610, 0.03937007874015843040 ) ) ;
#25707 = PLANE ( 'NONE',  #43322 ) ;
#25708 = CARTESIAN_POINT ( 'NONE',  ( 0.9412147342319837628, 0.1574803149606300301, 0.9522637794200313754 ) ) ;
#25709 = CARTESIAN_POINT ( 'NONE',  ( 1.002407869896990045, 0.1264236179284866091, 1.843011810969858333 ) ) ;
#25711 = CARTESIAN_POINT ( 'NONE',  ( 1.033464566929133799, 0.000000000000000000, 1.889763779420031486 ) ) ;
#25710 = CARTESIAN_POINT ( 'NONE',  ( -0.1895013542075498492, -0.07859528327916792678, 0.1760244123200213340 ) ) ;
#25712 = AXIS2_PLACEMENT_3D ( 'NONE', #6861, #39214, #545 ) ;
#25713 = CIRCLE ( 'NONE', #37911, 0.1003937007874010356 ) ;
#25715 = ORIENTED_EDGE ( 'NONE', *, *, #14363, .F. ) ;
#25714 = EDGE_CURVE ( 'NONE', #21602, #19657, #19352, .T. ) ;
#25716 = CARTESIAN_POINT ( 'NONE',  ( 0.1554371429169691954, -0.1056204263327882586, 0.09265060645564116015 ) ) ;
#25717 = CARTESIAN_POINT ( 'NONE',  ( -0.1264236179284866091, -0.3252952755367877757, -0.1264236179284866091 ) ) ;
#25719 = DIRECTION ( 'NONE',  ( -1.000000000000000000, 0.000000000000000000, 0.000000000000000000 ) ) ;
#25718 = CARTESIAN_POINT ( 'NONE',  ( -0.6971942568897626646, 0.07405724077823318263, 0.4773622046706456068 ) ) ;
#25720 = CARTESIAN_POINT ( 'NONE',  ( -0.1264236179284866091, -1.137303149552535420, 0.1264236179284866091 ) ) ;
#25721 = CARTESIAN_POINT ( 'NONE',  ( 0.9500414927467378812, 0.1787899950787401604, 0.1131889763241892138 ) ) ;
#25722 = ( BOUNDED_CURVE ( )  B_SPLINE_CURVE ( 2, ( #16957, #39680, #31597, #6867, #35654, #20778, #2792, #46178, #13375 ),
 .UNSPECIFIED., .F., .T. ) 
 B_SPLINE_CURVE_WITH_KNOTS ( ( 3, 2, 2, 2, 3 ),
 ( 0.2999999999999999889, 0.3024999999999999911, 0.3049999999999999933, 0.3074999999999999956, 0.3099999999999999978 ),
 .UNSPECIFIED. ) 
 CURVE ( )  GEOMETRIC_REPRESENTATION_ITEM ( )  RATIONAL_B_SPLINE_CURVE ( ( 1.000000000000000000, 0.9238795325112869605, 1.000000000000000000, 0.9238795325112869605, 1.000000000000000000, 0.9238795325112869605, 1.000000000000000000, 0.9238795325112869605, 1.000000000000000000 ) ) 
 REPRESENTATION_ITEM ( '' )  ) ;
#25723 = FACE_OUTER_BOUND ( 'NONE', #45370, .T. ) ;
#25724 = VERTEX_POINT ( 'NONE', #10968 ) ;
#25725 = CARTESIAN_POINT ( 'NONE',  ( -1.054774247047244540, -0.07405724077823318263, 1.205708661363558365 ) ) ;
#25726 = CARTESIAN_POINT ( 'NONE',  ( 0.7185039370078746268, -0.06523048226347956391, 1.016240157480315487 ) ) ;
#25727 = ADVANCED_FACE ( 'NONE', ( #14792 ), #28662, .T. ) ;
#25728 = CARTESIAN_POINT ( 'NONE',  ( 0.7495606340400177148, -0.1264236179284866091, 1.193405511757259951 ) ) ;
#25729 = CARTESIAN_POINT ( 'NONE',  ( -0.8759842519685039353, -0.1574803149606299191, 0.5511811023622047445 ) ) ;
#25730 = CARTESIAN_POINT ( 'NONE',  ( -0.7495606340400177148, -0.1264236179284866091, 1.109744094434425232 ) ) ;
#25731 = CARTESIAN_POINT ( 'NONE',  ( 0.1564139474900879123, 0.1149079234230807184, -0.08174552760864516043 ) ) ;
#25732 = CARTESIAN_POINT ( 'NONE',  ( -0.1939037905414077168, -0.1835438265964373927, -0.05114647357133220162 ) ) ;
#25733 = CARTESIAN_POINT ( 'NONE',  ( 0.8019270111902716547, 0.1787899950787401604, 0.2755905511273391006 ) ) ;
#25734 = CARTESIAN_POINT ( 'NONE',  ( -1.054774247047244540, 0.07405724077823318263, 0.2214566928596221063 ) ) ;
#25735 = CARTESIAN_POINT ( 'NONE',  ( -1.002407869896990045, 0.1264236179284866091, 0.7750984251430865779 ) ) ;
#25736 = CARTESIAN_POINT ( 'NONE',  ( 1.033464566929134687, 0.06523048226347956391, 1.695374015640504828 ) ) ;
#25737 = ORIENTED_EDGE ( 'NONE', *, *, #575, .T. ) ;
#25738 = CARTESIAN_POINT ( 'NONE',  ( -0.1264236179284866091, -0.0004921259304884456750, 0.1264236179284866091 ) ) ;
#25739 = CARTESIAN_POINT ( 'NONE',  ( 1.002407869896990045, -0.1264236179284866091, 0.8095472440407244230 ) ) ;
#25740 = CARTESIAN_POINT ( 'NONE',  ( 1.002407869896990045, 0.1264236179284866091, 1.016240157426551161 ) ) ;
#25741 = CARTESIAN_POINT ( 'NONE',  ( -0.8759842519685039353, 0.1787899950787401882, 1.882381889710015743 ) ) ;
#25742 = ORIENTED_EDGE ( 'NONE', *, *, #13747, .T. ) ;
#25743 = VECTOR ( 'NONE', #964, 39.37007874015748143 ) ;
#25744 = CARTESIAN_POINT ( 'NONE',  ( 0.8759842519685039353, -0.1787899950787401882, 1.980807086560409491 ) ) ;
#25745 = ( BOUNDED_CURVE ( )  B_SPLINE_CURVE ( 2, ( #35904, #14106, #41118, #21765, #40419, #36849, #29937, #629, #29708 ),
 .UNSPECIFIED., .F., .F. ) 
 B_SPLINE_CURVE_WITH_KNOTS ( ( 3, 2, 2, 2, 3 ),
 ( 0.03500000000000000333, 0.03749999999999999861, 0.04000000000000000083, 0.04250000000000000305, 0.04499999999999999833 ),
 .UNSPECIFIED. ) 
 CURVE ( )  GEOMETRIC_REPRESENTATION_ITEM ( )  RATIONAL_B_SPLINE_CURVE ( ( 1.000000000000000000, 0.9238795325112869605, 1.000000000000000000, 0.9238795325112869605, 1.000000000000000000, 0.9238795325112869605, 1.000000000000000000, 0.9238795325112869605, 1.000000000000000000 ) ) 
 REPRESENTATION_ITEM ( '' )  ) ;
#25746 = EDGE_CURVE ( 'NONE', #1914, #43027, #3007, .T. ) ;
#25747 = CARTESIAN_POINT ( 'NONE',  ( 1.033464566929133799, 0.000000000000000000, 1.309055118110236338 ) ) ;
#25748 = CARTESIAN_POINT ( 'NONE',  ( 0.1787899950787401604, -1.298352314685932152, 0.07405724077823318263 ) ) ;
#25749 = CARTESIAN_POINT ( 'NONE',  ( 0.1787899950787401604, -0.2588582676627719792, 0.07405724077823318263 ) ) ;
#25750 = CARTESIAN_POINT ( 'NONE',  ( -0.2066929133858267931, -0.2274162997038020051, -0.9219983537151217323 ) ) ;
#25751 = AXIS2_PLACEMENT_3D ( 'NONE', #25388, #180, #33060 ) ;
#25752 = ORIENTED_EDGE ( 'NONE', *, *, #38696, .T. ) ;
#25753 = CARTESIAN_POINT ( 'NONE',  ( 1.002407869896990045, 0.1264236179284866091, 1.247539370024976391 ) ) ;
#25754 = CARTESIAN_POINT ( 'NONE',  ( -0.9873396505805591694, 0.1113553986120547346, 0.8316929132782993062 ) ) ;
#25755 = CARTESIAN_POINT ( 'NONE',  ( -0.2471922279628200048, -0.07692167320558097876, 0.07932652958038384494 ) ) ;
#25756 = CARTESIAN_POINT ( 'NONE',  ( 0.8019270111902717657, -0.1787899950787401604, 0.04921259837143338034 ) ) ;
#25757 = CARTESIAN_POINT ( 'NONE',  ( -0.07405724077823318263, -1.646653543253324026, 0.1787899950787401604 ) ) ;
#25758 = B_SPLINE_CURVE_WITH_KNOTS ( 'NONE', 3,
 ( #9979, #12652, #2298, #9028, #5188, #19810, #38499, #16241, #27758, #23652, #5671, #31330, #45908, #13124, #42321, #9513, #24138, #36567, #10941, #29430 ),
 .UNSPECIFIED., .F., .F.,
 ( 4, 1, 1, 1, 1, 1, 2, 2, 1, 1, 1, 2, 2, 4 ),
 ( 0.000000000000000000, 0.2499999999999955591, 0.3749999999999933387, 0.4374999999999921174, 0.4687499999999915068, 0.4843749999999912847, 0.4921874999999911737, 0.4999999999999910072, 0.6249999999999926725, 0.6874999999999935607, 0.7187499999999942268, 0.7343749999999943379, 0.7499999999999945599, 1.000000000000000000 ),
 .UNSPECIFIED. ) ;
#25759 = CARTESIAN_POINT ( 'NONE',  ( -1.054774247047244096, 0.000000000000000000, 0.4995078739619842612 ) ) ;
#25760 = CARTESIAN_POINT ( 'NONE',  ( 0.8759842519685039353, -0.1574803149606299191, 0.3051181101286932762 ) ) ;
#25761 = CARTESIAN_POINT ( 'NONE',  ( -0.1270800023317771588, -1.462642234779895745, -0.1270800023317771588 ) ) ;
#25762 = CARTESIAN_POINT ( 'NONE',  ( 0.7495606340400177148, 0.1264236179284866091, 1.262303149552535420 ) ) ;
#25763 = CARTESIAN_POINT ( 'NONE',  ( 0.9500414927467377701, -0.1787899950787401604, 1.628937007820252303 ) ) ;
#25765 = ADVANCED_FACE ( 'NONE', ( #7358 ), #34784, .F. ) ;
#25764 = CARTESIAN_POINT ( 'NONE',  ( 0.9412147342319837628, 0.1574803149606300301, 0.1353346456692914035 ) ) ;
#25766 = DIRECTION ( 'NONE',  ( 0.000000000000000000, 0.2126700594527834998, -0.9771240687918549828 ) ) ;
#25767 = CARTESIAN_POINT ( 'NONE',  ( -0.8107537697050254399, 0.1574803149606300301, 1.006397637795276800 ) ) ;
#25768 = DIRECTION ( 'NONE',  ( -0.000000000000000000, 1.000000000000000000, -0.000000000000000000 ) ) ;
#25769 = DIRECTION ( 'NONE',  ( -1.000000000000000000, 0.000000000000000000, 0.000000000000000000 ) ) ;
#25770 = FACE_OUTER_BOUND ( 'NONE', #43366, .T. ) ;
#25771 = CARTESIAN_POINT ( 'NONE',  ( 0.6971942568897637749, 2.189545951927499583E-17, 0.3174212597887562382 ) ) ;
#25772 = EDGE_CURVE ( 'NONE', #2262, #3336, #7580, .T. ) ;
#25773 = DIRECTION ( 'NONE',  ( 1.000000000000000000, 0.000000000000000000, 0.000000000000000000 ) ) ;
#25774 = DIRECTION ( 'NONE',  ( 0.5735764363510447161, -0.8191520442889925757, 1.003171929053525486E-16 ) ) ;
#25775 = CARTESIAN_POINT ( 'NONE',  ( 0.9873396505805591694, 0.1113553986120547346, 0.6348425195775118102 ) ) ;
#25776 = ORIENTED_EDGE ( 'NONE', *, *, #29559, .T. ) ;
#25777 = PRESENTATION_STYLE_ASSIGNMENT (( #22390 ) ) ;
#25778 = EDGE_CURVE ( 'NONE', #5864, #42441, #3980, .T. ) ;
#25779 = CARTESIAN_POINT ( 'NONE',  ( 0.9141235117445012381, 0.1680089951793457825, 0.03937079690018885358 ) ) ;
#25780 = DIRECTION ( 'NONE',  ( 0.000000000000000000, 0.000000000000000000, -1.000000000000000000 ) ) ;
#25781 = CARTESIAN_POINT ( 'NONE',  ( 0.8019270111902717657, 0.1787899950787401604, 1.373031496009229135 ) ) ;
#25782 = CARTESIAN_POINT ( 'NONE',  ( -0.7646288533564489232, 0.1113553986120547346, 1.166338582677165281 ) ) ;
#25783 = EDGE_CURVE ( 'NONE', #28038, #1697, #44227, .T. ) ;
#25785 = CARTESIAN_POINT ( 'NONE',  ( 1.033464566929133799, 0.000000000000000000, 1.899606299212598604 ) ) ;
#25784 = CARTESIAN_POINT ( 'NONE',  ( -0.8759842519685039353, 0.1574803149606299191, 1.830708661417322913 ) ) ;
#25786 = DIRECTION ( 'NONE',  ( 1.000000000000000000, 0.000000000000000000, 0.000000000000000000 ) ) ;
#25787 = CARTESIAN_POINT ( 'NONE',  ( 0.07405724077823318263, -0.1062992125446616531, 0.1787899950787401604 ) ) ;
#25788 = ORIENTED_EDGE ( 'NONE', *, *, #42449, .T. ) ;
#25789 = CARTESIAN_POINT ( 'NONE',  ( 0.7185039370078714072, 0.06523048226347728795, 1.552657480207434659 ) ) ;
#25790 = CARTESIAN_POINT ( 'NONE',  ( 0.1574803149606300023, 0.000000000000000000, 0.000000000000000000 ) ) ;
#25791 = CARTESIAN_POINT ( 'NONE',  ( -0.07564704710143098365, -0.08785038237282348506, 0.2417569064347979690 ) ) ;
#25792 = CARTESIAN_POINT ( 'NONE',  ( 0.8759842519685039353, -0.1787899950787401882, 0.5290354330171024300 ) ) ;
#25793 = ORIENTED_EDGE ( 'NONE', *, *, #30410, .T. ) ;
#25794 = CARTESIAN_POINT ( 'NONE',  ( 0.07405724077823318263, -1.804133858213953889, 0.1787899950787401604 ) ) ;
#25795 = CARTESIAN_POINT ( 'NONE',  ( -0.7495606340400177148, -0.1264236179284866091, 1.193405511757259951 ) ) ;
#25796 = ORIENTED_EDGE ( 'NONE', *, *, #11840, .T. ) ;
#25797 = CARTESIAN_POINT ( 'NONE',  ( 0.1126279540338993995, 0.3740157480314960647, 1.206847064312612128 ) ) ;
#25798 = CARTESIAN_POINT ( 'NONE',  ( -0.8019270111902717657, -0.1787899950787401604, 0.8021653542769460188 ) ) ;
#25799 = CARTESIAN_POINT ( 'NONE',  ( -0.9500414927467378812, 0.1787899950787401604, 0.1919291338045042428 ) ) ;
#25800 = CARTESIAN_POINT ( 'NONE',  ( 1.033464566929134687, -0.06523048226347956391, 0.6766732283464570452 ) ) ;
#25801 = DIRECTION ( 'NONE',  ( 0.000000000000000000, 0.000000000000000000, -1.000000000000000000 ) ) ;
#25802 = CARTESIAN_POINT ( 'NONE',  ( -0.1264236179284866091, -0.8382145194103405306, 0.1264236179284866091 ) ) ;
#25803 = ORIENTED_EDGE ( 'NONE', *, *, #16570, .T. ) ;
#25804 = CARTESIAN_POINT ( 'NONE',  ( 0.1264236179284866091, 0.1422244095025824717, -0.1264236179284866091 ) ) ;
#25805 = ORIENTED_EDGE ( 'NONE', *, *, #19690, .T. ) ;
#25806 = ORIENTED_EDGE ( 'NONE', *, *, #20298, .T. ) ;
#25807 = CARTESIAN_POINT ( 'NONE',  ( 0.003436456682582578626, -0.04094436872149315176, 0.1377952874252535709 ) ) ;
#25808 = CARTESIAN_POINT ( 'NONE',  ( -0.8019270111902717657, 0.1787899950787401604, 0.7824803149068669805 ) ) ;
#25809 = DIRECTION ( 'NONE',  ( 0.000000000000000000, 0.000000000000000000, 1.000000000000000000 ) ) ;
#25810 = VERTEX_POINT ( 'NONE', #11673 ) ;
#25811 = CARTESIAN_POINT ( 'NONE',  ( -0.7495606340400177148, -0.1264236179284866091, 1.783956692859621995 ) ) ;
#25812 = CARTESIAN_POINT ( 'NONE',  ( -0.1264236179284866091, -0.5221456692375747721, -0.1264236179284866091 ) ) ;
#25813 = ORIENTED_EDGE ( 'NONE', *, *, #41040, .F. ) ;
#25814 = CARTESIAN_POINT ( 'NONE',  ( -1.100456976456230270E-17, -0.9557524710003681978, -0.1797182628040039365 ) ) ;
#25815 = CARTESIAN_POINT ( 'NONE',  ( -0.7646288533564489232, 0.1113553986120547346, 0.4084645668216063119 ) ) ;
#25816 = CARTESIAN_POINT ( 'NONE',  ( -0.7646288533564489232, 0.1113553986120547346, 1.589566929026330566 ) ) ;
#25817 = CARTESIAN_POINT ( 'NONE',  ( 0.9500414927467378812, 0.1787899950787401604, 0.7037401574265510495 ) ) ;
#25818 = CARTESIAN_POINT ( 'NONE',  ( 0.000000000000000000, 0.000000000000000000, 0.000000000000000000 ) ) ;
#25819 = CARTESIAN_POINT ( 'NONE',  ( 1.033464566929134687, 0.06523048226347956391, 1.390255905511810441 ) ) ;
#25820 = CYLINDRICAL_SURFACE ( 'NONE', #18700, 0.04921259842519678379 ) ;
#25822 = CARTESIAN_POINT ( 'NONE',  ( 0.7185039370078739607, 0.000000000000000000, 4.498031496062992574 ) ) ;
#25821 = CARTESIAN_POINT ( 'NONE',  ( 0.8505431175464920335, -0.1718778923049482099, 1.987741662751643767 ) ) ;
#25823 = DIRECTION ( 'NONE',  ( 1.000000000000000000, 0.000000000000000000, -7.083454193571960199E-15 ) ) ;
#25824 = AXIS2_PLACEMENT_3D ( 'NONE', #34975, #28745, #43309 ) ;
#25825 = EDGE_CURVE ( 'NONE', #27278, #40074, #26297, .T. ) ;
#25826 = CARTESIAN_POINT ( 'NONE',  ( 1.054774247047244540, -0.07405724077823318263, 0.8858267715997791836 ) ) ;
#25827 = CARTESIAN_POINT ( 'NONE',  ( -1.094772975963752103E-17, -0.8371062991588346103, -0.1787899950787401882 ) ) ;
#25828 = CARTESIAN_POINT ( 'NONE',  ( -0.7185039370078746268, 0.06523048226347956391, 1.168799212598425896 ) ) ;
#25829 = PLANE ( 'NONE',  #26757 ) ;
#25830 = CARTESIAN_POINT ( 'NONE',  ( 1.002407869896990045, 0.1264236179284866091, 1.011318897584031484 ) ) ;
#25831 = EDGE_CURVE ( 'NONE', #19535, #39641, #43948, .T. ) ;
#25832 = LINE ( 'NONE', #10269, #4239 ) ;
#25833 = CARTESIAN_POINT ( 'NONE',  ( 0.1574803149606299191, -1.622047244094488194, -1.928577636452523993E-17 ) ) ;
#25834 = CARTESIAN_POINT ( 'NONE',  ( -0.7185039370078739607, 1.928577636452523993E-17, 0.5019685039370078705 ) ) ;
#25835 = ORIENTED_EDGE ( 'NONE', *, *, #40661, .T. ) ;
#25836 = CARTESIAN_POINT ( 'NONE',  ( 0.1498753904841986506, -0.1193342091828952928, -0.06889763779527559306 ) ) ;
#25837 = CARTESIAN_POINT ( 'NONE',  ( -0.6971942568897637749, 2.189545951927499583E-17, 0.1599409448281264023 ) ) ;
#25838 = CARTESIAN_POINT ( 'NONE',  ( 0.9412147342319837628, 0.1574803149606300301, 1.749507874015747699 ) ) ;
#25839 = CARTESIAN_POINT ( 'NONE',  ( 0.1787899950787401604, -1.444881889710016631, 0.07405724077823318263 ) ) ;
#25840 = CARTESIAN_POINT ( 'NONE',  ( -0.8759842519685039353, 0.1787899950787401882, 1.685531496009228469 ) ) ;
#25841 = CARTESIAN_POINT ( 'NONE',  ( -1.054774247047244540, -0.07405724077823318263, 0.8464566928596233275 ) ) ;
#25842 = CARTESIAN_POINT ( 'NONE',  ( -0.6971942568897626646, -0.07405724077823297447, 0.3248031495525359746 ) ) ;
#25843 = CARTESIAN_POINT ( 'NONE',  ( 0.3123359580052492146, 0.08090551181102362266, 0.000000000000000000 ) ) ;
#25844 = CARTESIAN_POINT ( 'NONE',  ( 0.1588891437629025849, 0.04395497937033298469, 0.1404564352527446769 ) ) ;
#25845 = CARTESIAN_POINT ( 'NONE',  ( 0.8070866141732283561, -0.0009842519685049383633, 0.6590551181102368705 ) ) ;
#25846 = CARTESIAN_POINT ( 'NONE',  ( -1.033464566929134687, -0.06523048226347956391, 1.975885826771653475 ) ) ;
#25847 = CARTESIAN_POINT ( 'NONE',  ( -0.2610236670165029249, 0.1673052798952545106, -0.8646194990212731080 ) ) ;
#25848 = CARTESIAN_POINT ( 'NONE',  ( 0.1264236179284866091, -0.3854586138985299226, -0.1264236179284866091 ) ) ;
#25849 = CARTESIAN_POINT ( 'NONE',  ( -0.2080960361476567044, -0.08955968088635905822, -0.1267239370720273928 ) ) ;
#25850 = FACE_OUTER_BOUND ( 'NONE', #1252, .T. ) ;
#25851 = DIRECTION ( 'NONE',  ( 1.000000000000000000, 0.000000000000000000, 0.000000000000000000 ) ) ;
#25852 = CIRCLE ( 'NONE', #8213, 0.1624015748031507056 ) ;
#25853 = CARTESIAN_POINT ( 'NONE',  ( -0.7495606340400177148, -0.1264236179284866091, 0.2829724408911185041 ) ) ;
#25854 = VERTEX_POINT ( 'NONE', #16214 ) ;
#25855 = ORIENTED_EDGE ( 'NONE', *, *, #46636, .F. ) ;
#25856 = CARTESIAN_POINT ( 'NONE',  ( -1.002407869896990045, -0.1264236179284866091, 1.321358267662771757 ) ) ;
#25857 = ORIENTED_EDGE ( 'NONE', *, *, #7616, .T. ) ;
#25858 = CARTESIAN_POINT ( 'NONE',  ( 0.1787899950787401604, -1.405511810969858999, 0.07405724077823318263 ) ) ;
#25859 = CARTESIAN_POINT ( 'NONE',  ( 0.07405724077823318263, -1.444881889710016631, 0.1787899950787401604 ) ) ;
#25860 = CARTESIAN_POINT ( 'NONE',  ( 0.5113546317124669782, 0.09842519685039370636, 1.205361022782828805E-17 ) ) ;
#25861 = DIRECTION ( 'NONE',  ( 0.000000000000000000, 0.000000000000000000, 1.000000000000000000 ) ) ;
#25862 = CARTESIAN_POINT ( 'NONE',  ( 0.9412147342319837628, 0.1574803149606300301, 0.4109251968503938590 ) ) ;
#25863 = CARTESIAN_POINT ( 'NONE',  ( -0.8759842519685039353, 0.000000000000000000, 0.000000000000000000 ) ) ;
#25864 = CARTESIAN_POINT ( 'NONE',  ( -0.9873396505805591694, -0.1113553986120547346, 1.136811023514519681 ) ) ;
#25865 = CARTESIAN_POINT ( 'NONE',  ( 0.6971942568897626646, 0.07405724077823318263, 0.3986220471903312301 ) ) ;
#25866 = CARTESIAN_POINT ( 'NONE',  ( -0.9873396505805591694, -0.1113553986120547346, 1.697834645669291209 ) ) ;
#25867 = CARTESIAN_POINT ( 'NONE',  ( -0.06523048226347956391, -0.3499015748031495399, -0.1574803149606300301 ) ) ;
#25868 = DIRECTION ( 'NONE',  ( 0.000000000000000000, 0.000000000000000000, 1.000000000000000000 ) ) ;
#25869 = ORIENTED_EDGE ( 'NONE', *, *, #10584, .T. ) ;
#25870 = CARTESIAN_POINT ( 'NONE',  ( -0.8070866141732283561, -0.0009842519685049383633, -0.8559055118110230342 ) ) ;
#25871 = CARTESIAN_POINT ( 'NONE',  ( 0.7185039370078746268, 0.06523048226347956391, 0.9719488188976380671 ) ) ;
#25872 = CARTESIAN_POINT ( 'NONE',  ( -0.1377952755905511861, 0.1574803149606320007, 0.8070866141732283561 ) ) ;
#25873 = CARTESIAN_POINT ( 'NONE',  ( 2.892866454678787531E-17, -0.5196850392625512738, 0.1574803149606299191 ) ) ;
#25874 = ADVANCED_FACE ( 'NONE', ( #12388 ), #23154, .T. ) ;
#25875 = VECTOR ( 'NONE', #7410, 39.37007874015748143 ) ;
#25876 = CARTESIAN_POINT ( 'NONE',  ( -0.7646288533564489232, -0.1113553986120547346, 0.4675196850393700809 ) ) ;
#25877 = DIRECTION ( 'NONE',  ( 1.000000000000000000, -5.472378587457090550E-15, 4.275490733183370330E-15 ) ) ;
#25878 = CARTESIAN_POINT ( 'NONE',  ( -0.3094175599200249538, 0.02245875686878769095, 1.042162571470887977 ) ) ;
#25879 = ADVANCED_FACE ( 'NONE', ( #16445 ), #34819, .T. ) ;
#25880 = CARTESIAN_POINT ( 'NONE',  ( -0.7185039370078739607, 1.928577636452523993E-17, 0.6102362203649134287 ) ) ;
#25881 = CARTESIAN_POINT ( 'NONE',  ( -0.9412147342319837628, -0.1574803149606297803, 0.9867125984251977622 ) ) ;
#25882 = CARTESIAN_POINT ( 'NONE',  ( -0.1264236179284866091, -1.609744094434425232, 0.1264236179284866091 ) ) ;
#25883 = CARTESIAN_POINT ( 'NONE',  ( 0.1574803149606300301, -1.575295275483024948, 0.06523048226347956391 ) ) ;
#25884 = CARTESIAN_POINT ( 'NONE',  ( -0.1787899950787401882, -0.7534448818360000022, 0.000000000000000000 ) ) ;
#25886 = VECTOR ( 'NONE', #14458, 39.37007874015748143 ) ;
#25885 = CARTESIAN_POINT ( 'NONE',  ( 0.1574803149606300301, -1.265255905511811774, -0.06523048226347956391 ) ) ;
#25887 = CARTESIAN_POINT ( 'NONE',  ( 0.9873396505805591694, -0.1113553986120547346, 0.9399606298137322957 ) ) ;
#25888 = DIRECTION ( 'NONE',  ( -1.000000000000000000, 0.000000000000000000, 7.047314121155780399E-15 ) ) ;
#25889 = EDGE_LOOP ( 'NONE', ( #525, #12371, #14319, #5231 ) ) ;
#25890 = EDGE_LOOP ( 'NONE', ( #25582, #43075, #17897, #36868 ) ) ;
#25891 = ORIENTED_EDGE ( 'NONE', *, *, #45438, .F. ) ;
#25892 = CARTESIAN_POINT ( 'NONE',  ( -1.002407869896990045, 0.1264236179284866091, 1.567421259788755794 ) ) ;
#25893 = CARTESIAN_POINT ( 'NONE',  ( 1.054774247047244540, 0.07405724077823318263, 1.761811023568284007 ) ) ;
#25894 = CARTESIAN_POINT ( 'NONE',  ( -1.054774247047244540, -0.07405724077823318263, 0.8120078739619844832 ) ) ;
#25895 = FACE_OUTER_BOUND ( 'NONE', #9306, .T. ) ;
#25896 = CARTESIAN_POINT ( 'NONE',  ( 1.002407869896990045, 0.1264236179284866091, 0.3469488188438744070 ) ) ;
#25897 = CARTESIAN_POINT ( 'NONE',  ( 0.5966535433070866423, 1.205361022782828805E-17, -0.09842519685039370636 ) ) ;
#25898 = CARTESIAN_POINT ( 'NONE',  ( -1.054774247047244096, 0.000000000000000000, 1.281988188922614125 ) ) ;
#25899 = CARTESIAN_POINT ( 'NONE',  ( -1.054774247047244096, 0.000000000000000000, 0.6520669290800944484 ) ) ;
#25900 = CARTESIAN_POINT ( 'NONE',  ( 0.001132063567009175716, -0.1075630933946832152, 0.08929056810482036144 ) ) ;
#25901 = CARTESIAN_POINT ( 'NONE',  ( 0.06655125492330998815, 0.08353766247256362576, 0.2470096859212614071 ) ) ;
#25902 = CARTESIAN_POINT ( 'NONE',  ( -0.8019270111902717657, 0.1787899950787401604, 1.614173228292692386 ) ) ;
#25903 = CARTESIAN_POINT ( 'NONE',  ( -0.9412147342319837628, -0.1574803149606297803, 1.921751968396409493 ) ) ;
#25904 = ORIENTED_EDGE ( 'NONE', *, *, #23938, .F. ) ;
#25905 = CARTESIAN_POINT ( 'NONE',  ( -0.7185039370078746268, 0.06523048226347956391, 1.641240157480315931 ) ) ;
#25906 = CARTESIAN_POINT ( 'NONE',  ( 0.2018787443954609129, -0.3516577756781031350, -1.037265999283336182 ) ) ;
#25907 = CARTESIAN_POINT ( 'NONE',  ( 0.7495606340400177148, -0.1264236179284866091, 1.429625984198204858 ) ) ;
#25908 = CARTESIAN_POINT ( 'NONE',  ( -1.033464566929134687, 0.06523048226347956391, 0.3567913384751500994 ) ) ;
#25909 = EDGE_LOOP ( 'NONE', ( #17342, #27808, #36724, #5016, #10522, #3602, #29707, #47046, #17673, #616, #12894, #10278 ) ) ;
#25910 = VERTEX_POINT ( 'NONE', #22911 ) ;
#25911 = EDGE_CURVE ( 'NONE', #35669, #21060, #21065, .T. ) ;
#25912 = AXIS2_PLACEMENT_3D ( 'NONE', #18898, #37344, #18430 ) ;
#25913 = ORIENTED_EDGE ( 'NONE', *, *, #14079, .T. ) ;
#25914 = ORIENTED_EDGE ( 'NONE', *, *, #42819, .F. ) ;
#25915 = CARTESIAN_POINT ( 'NONE',  ( -0.07405724077823318263, -0.9576771653005667906, -0.1787899950787401604 ) ) ;
#25916 = CARTESIAN_POINT ( 'NONE',  ( -1.094772975963752103E-17, -0.4483267715997795166, -0.1787899950787401882 ) ) ;
#25917 = CARTESIAN_POINT ( 'NONE',  ( -0.1787899950787401604, -0.9035433070328510174, 0.07405724077823318263 ) ) ;
#25918 = ORIENTED_EDGE ( 'NONE', *, *, #36161, .T. ) ;
#25919 = DIRECTION ( 'NONE',  ( 0.000000000000000000, 0.000000000000000000, -1.000000000000000000 ) ) ;
#25920 = LENGTH_MEASURE_WITH_UNIT ( LENGTH_MEASURE( 0.02539999999999999897 ), #43876 ) ;
#25921 = CARTESIAN_POINT ( 'NONE',  ( 0.8759842519685039353, 0.1787899950787401882, 1.724901574749385880 ) ) ;
#25922 = CARTESIAN_POINT ( 'NONE',  ( 0.1797182628040039087, -0.1806540458035179320, 0.07444174185955046430 ) ) ;
#25923 = CARTESIAN_POINT ( 'NONE',  ( 0.1574803149606300301, 0.1520669291338582751, -0.06523048226347956391 ) ) ;
#25924 = CARTESIAN_POINT ( 'NONE',  ( -0.1787899950787401604, -0.1210629920722208208, 0.07405724077823318263 ) ) ;
#25925 = CARTESIAN_POINT ( 'NONE',  ( 0.2471922904502827645, -0.04197619597984889039, -0.1314166662975417565 ) ) ;
#25926 = CARTESIAN_POINT ( 'NONE',  ( 0.7495606340400177148, -0.1264236179284866091, 0.7554133857730077617 ) ) ;
#25927 = EDGE_CURVE ( 'NONE', #3498, #38566, #45047, .T. ) ;
#25929 = CARTESIAN_POINT ( 'NONE',  ( 0.7185039370078739607, 1.928577636452523993E-17, 1.122047243986960652 ) ) ;
#25928 = CYLINDRICAL_SURFACE ( 'NONE', #15509, 0.1574803149606299191 ) ;
#25931 = CARTESIAN_POINT ( 'NONE',  ( -0.9193554356332743760, -0.1704440316159954449, 1.988959660599587398 ) ) ;
#25930 = CARTESIAN_POINT ( 'NONE',  ( -0.3980944881889741382, 0.7681739484881655589, -0.04983111751016786051 ) ) ;
#25932 = CARTESIAN_POINT ( 'NONE',  ( 0.3727034120734909473, 4.616380251121755931E-17, 0.000000000000000000 ) ) ;
#25933 = CARTESIAN_POINT ( 'NONE',  ( 0.8019270111902717657, -0.1787899950787401604, 1.904527559001354398 ) ) ;
#25935 = PLANE ( 'NONE',  #36931 ) ;
#25934 = DIRECTION ( 'NONE',  ( 1.822029033848725028E-16, 0.000000000000000000, 1.000000000000000000 ) ) ;
#25936 = EDGE_CURVE ( 'NONE', #740, #22900, #9756, .T. ) ;
#25937 = FACE_OUTER_BOUND ( 'NONE', #46914, .T. ) ;
#25938 = CARTESIAN_POINT ( 'NONE',  ( 0.07405724077823318263, -0.3080708660879689087, 0.1787899950787401604 ) ) ;
#25939 = CYLINDRICAL_SURFACE ( 'NONE', #40747, 0.1574803149606299191 ) ;
#25940 = CARTESIAN_POINT ( 'NONE',  ( -0.07405724077823318263, -1.149606299158835387, -0.1787899950787401604 ) ) ;
#25941 = CARTESIAN_POINT ( 'NONE',  ( 0.8759842519685039353, 0.1787899950787401882, 0.2731299212060791515 ) ) ;
#25942 = CARTESIAN_POINT ( 'NONE',  ( 0.1610681406158918083, 0.07955616528309404634, -0.1377952308554367400 ) ) ;
#25943 = CARTESIAN_POINT ( 'NONE',  ( 1.054774247047244540, 0.07405724077823318263, 0.5757874015210393548 ) ) ;
#25944 = CARTESIAN_POINT ( 'NONE',  ( -0.8019270111902717657, 0.1787899950787401604, 1.609251968450173376 ) ) ;
#25945 = ORIENTED_EDGE ( 'NONE', *, *, #18938, .F. ) ;
#25946 = CARTESIAN_POINT ( 'NONE',  ( -0.8019270111902717657, 0.1787899950787401604, 1.141732283410804349 ) ) ;
#25947 = CARTESIAN_POINT ( 'NONE',  ( 1.033464566929133799, 1.928577636452524610E-17, 4.498031496062992574 ) ) ;
#25948 = AXIS2_PLACEMENT_3D ( 'NONE', #24339, #41807, #9725 ) ;
#25949 = CARTESIAN_POINT ( 'NONE',  ( 0.1113553986120547346, -1.213582677057826853, -0.1113553986120547346 ) ) ;
#25950 = CARTESIAN_POINT ( 'NONE',  ( 0.9500414927467378812, -0.1787899950787401604, 1.904527559001354398 ) ) ;
#25951 = CARTESIAN_POINT ( 'NONE',  ( -1.054774247047244540, 0.07405724077823318263, 1.048228346402928723 ) ) ;
#25952 = DIRECTION ( 'NONE',  ( -5.159318851433039196E-16, -0.6156614753256609562, -0.7880107536067197938 ) ) ;
#25953 = CARTESIAN_POINT ( 'NONE',  ( -0.2559055118110236116, -0.1477471161312049197, -0.1122047244094488277 ) ) ;
#25954 = CARTESIAN_POINT ( 'NONE',  ( 0.9500414927467377701, -0.1787899950787401604, 0.4133858267178901480 ) ) ;
#25955 = CARTESIAN_POINT ( 'NONE',  ( -1.054774247047244540, -0.07405724077823318263, 0.2559055117572600624 ) ) ;
#25956 = CARTESIAN_POINT ( 'NONE',  ( 0.8107537697050253289, -0.1574803149606297803, 1.680610236112946687 ) ) ;
#25957 = VECTOR ( 'NONE', #27289, 39.37007874015748854 ) ;
#25958 = CARTESIAN_POINT ( 'NONE',  ( -0.8759842519685039353, 0.1574803149606299191, 0.8759842518609765039 ) ) ;
#25959 = CONICAL_SURFACE ( 'NONE', #19825, 0.2559055118110236116, 0.7853981633974518317 ) ;
#25960 = CARTESIAN_POINT ( 'NONE',  ( -0.9500414927467377701, -0.1787899950787401604, 1.865157480261198097 ) ) ;
#25961 = VERTEX_POINT ( 'NONE', #23862 ) ;
#25962 = CARTESIAN_POINT ( 'NONE',  ( 1.002407869896990045, -0.1264236179284866091, 1.946358267662771757 ) ) ;
#25963 = LINE ( 'NONE', #32705, #27523 ) ;
#25964 = CARTESIAN_POINT ( 'NONE',  ( 0.1264236179284866091, -1.527190897363096544, -0.1264236179284866091 ) ) ;
#25965 = VERTEX_POINT ( 'NONE', #4433 ) ;
#25966 = CARTESIAN_POINT ( 'NONE',  ( 0.1787899950787401604, -0.3326771653005671237, -0.07405724077823318263 ) ) ;
#25967 = CARTESIAN_POINT ( 'NONE',  ( -1.033464566929133799, 0.000000000000000000, 0.2854330708661417804 ) ) ;
#25968 = VERTEX_POINT ( 'NONE', #12141 ) ;
#25969 = CARTESIAN_POINT ( 'NONE',  ( 1.002407869896990045, -0.1264236179284866091, 1.158956692859621995 ) ) ;
#25970 = CARTESIAN_POINT ( 'NONE',  ( -0.7185039370078739607, 1.928577636452523993E-17, 0.8464566928058583350 ) ) ;
#25971 = CARTESIAN_POINT ( 'NONE',  ( 0.9412147342319837628, 0.1574803149606300301, 1.385334645561763445 ) ) ;
#25972 = CIRCLE ( 'NONE', #5294, 0.1013779527559055538 ) ;
#25973 = CARTESIAN_POINT ( 'NONE',  ( 0.8759842519685039353, -0.1787899950787401882, 0.2091535432533232486 ) ) ;
#25974 = EDGE_CURVE ( 'NONE', #9411, #47093, #6374, .T. ) ;
#25975 = CARTESIAN_POINT ( 'NONE',  ( -1.094772975963752103E-17, -1.629429133804503937, -0.1787899950787401882 ) ) ;
#25976 = CARTESIAN_POINT ( 'NONE',  ( -1.094772975963752103E-17, -1.663877952702141672, -0.1787899950787401882 ) ) ;
#25977 = APPLICATION_PROTOCOL_DEFINITION ( 'draft international standard', 'automotive_design', 1998, #15971 ) ;
#25978 = EDGE_LOOP ( 'NONE', ( #40775, #40638, #13940, #31900 ) ) ;
#25979 = ( BOUNDED_CURVE ( )  B_SPLINE_CURVE ( 2, ( #17361, #46121, #35595, #42981, #45882, #42517, #38473, #28173, #38932 ),
 .UNSPECIFIED., .F., .T. ) 
 B_SPLINE_CURVE_WITH_KNOTS ( ( 3, 2, 2, 2, 3 ),
 ( 0.1000000000000000056, 0.1024999999999999939, 0.1049999999999999961, 0.1074999999999999983, 0.1100000000000000006 ),
 .UNSPECIFIED. ) 
 CURVE ( )  GEOMETRIC_REPRESENTATION_ITEM ( )  RATIONAL_B_SPLINE_CURVE ( ( 1.000000000000000000, 0.9238795325112869605, 1.000000000000000000, 0.9238795325112869605, 1.000000000000000000, 0.9238795325112869605, 1.000000000000000000, 0.9238795325112869605, 1.000000000000000000 ) ) 
 REPRESENTATION_ITEM ( '' )  ) ;
#25980 = CARTESIAN_POINT ( 'NONE',  ( -0.6971942568897648851, 0.07405724077823318263, 0.5561023621509617598 ) ) ;
#25981 = CARTESIAN_POINT ( 'NONE',  ( 0.8107537697050254399, 0.1574803149606300301, 0.3764763779527559029 ) ) ;
#25983 = CARTESIAN_POINT ( 'NONE',  ( -0.7121474872820316993, -0.03261578266289449912, 1.983871201520547300 ) ) ;
#25982 = CARTESIAN_POINT ( 'NONE',  ( 0.1797182628040039087, -1.361756408008243824, 0.07444174185955046430 ) ) ;
#25984 = LINE ( 'NONE', #40566, #30986 ) ;
#25985 = CARTESIAN_POINT ( 'NONE',  ( 0.7495606340400177148, 0.1264236179284866091, 1.419783464513165505 ) ) ;
#25986 = CARTESIAN_POINT ( 'NONE',  ( 1.054774247047244540, 0.07405724077823318263, 1.678149606245448622 ) ) ;
#25987 = DIRECTION ( 'NONE',  ( 1.822029033848725028E-16, 0.000000000000000000, 1.000000000000000000 ) ) ;
#25988 = EDGE_CURVE ( 'NONE', #21943, #19046, #31997, .T. ) ;
#25990 = CARTESIAN_POINT ( 'NONE',  ( -0.7904050636569344146, 0.1360127284603924458, 1.980115632570861983 ) ) ;
#25989 = CARTESIAN_POINT ( 'NONE',  ( 0.8759842519685039353, -0.1574803149606299191, 0.8956692912310552090 ) ) ;
#25991 = CARTESIAN_POINT ( 'NONE',  ( 0.9873396505805591694, -0.1113553986120547346, 0.8218503935932598425 ) ) ;
#25993 = FACE_OUTER_BOUND ( 'NONE', #35522, .T. ) ;
#25992 = CARTESIAN_POINT ( 'NONE',  ( -0.06523048226347956391, -0.8124999998924731237, -0.1574803149606300301 ) ) ;
#25994 = DIRECTION ( 'NONE',  ( 0.000000000000000000, -1.000000000000000000, 0.000000000000000000 ) ) ;
#25995 = CARTESIAN_POINT ( 'NONE',  ( 1.002407869896990045, -0.1264236179284866091, 0.3321850393163153226 ) ) ;
#25996 = CARTESIAN_POINT ( 'NONE',  ( 0.7331143493074542272, -0.08920476175640286443, 0.03937008031052523227 ) ) ;
#25997 = CARTESIAN_POINT ( 'NONE',  ( -1.033464566929134687, 0.06523048226347956391, 1.705216535433070613 ) ) ;
#25998 = DIRECTION ( 'NONE',  ( 0.000000000000000000, -1.000000000000000000, 0.000000000000000000 ) ) ;
#25999 = CARTESIAN_POINT ( 'NONE',  ( 0.5717220857807087109, 1.205361022782824954E-17, -0.09842519685039370636 ) ) ;
#26000 = CARTESIAN_POINT ( 'NONE',  ( 0.7646288533564489232, -0.1113553986120547346, 0.5757874014672763607 ) ) ;
#26001 = ORIENTED_EDGE ( 'NONE', *, *, #35178, .F. ) ;
#26002 = LINE ( 'NONE', #29871, #39087 ) ;
#26003 = CARTESIAN_POINT ( 'NONE',  ( -0.1661139969171220310, -0.4376765877502337143, -0.9700607378021975924 ) ) ;
#26004 = ORIENTED_EDGE ( 'NONE', *, *, #11594, .T. ) ;
#26005 = CARTESIAN_POINT ( 'NONE',  ( 0.9412147342319837628, 0.1574803149606300301, 0.2928149606299214613 ) ) ;
#26006 = CARTESIAN_POINT ( 'NONE',  ( 0.1270800023317771588, -0.1043745182444627967, 0.1270800023317771588 ) ) ;
#26007 = CARTESIAN_POINT ( 'NONE',  ( -0.7185039370078739607, 1.928577636452523993E-17, 0.2952755904436539236 ) ) ;
#26008 = CARTESIAN_POINT ( 'NONE',  ( -0.9412147342319837628, 0.1574803149606300301, 0.4798228345381422844 ) ) ;
#26009 = CARTESIAN_POINT ( 'NONE',  ( -0.8107537697050254399, 0.1574803149606300301, 1.596948818897636624 ) ) ;
#26010 = CARTESIAN_POINT ( 'NONE',  ( 0.9500414927467378812, -0.1787899950787401604, 1.628937007820252303 ) ) ;
#26011 = DIRECTION ( 'NONE',  ( -0.000000000000000000, 1.000000000000000000, -0.000000000000000000 ) ) ;
#26013 = CARTESIAN_POINT ( 'NONE',  ( 1.033464566929134687, 0.06523048226347956391, 1.665846456692914312 ) ) ;
#26012 = CARTESIAN_POINT ( 'NONE',  ( 0.1579024634500803825, -0.1385691271449887019, 0.04084555919664353829 ) ) ;
#26014 = CARTESIAN_POINT ( 'NONE',  ( 1.033464566929133799, 1.928577636452524610E-17, 4.498031496062992574 ) ) ;
#26015 = CARTESIAN_POINT ( 'NONE',  ( -0.8019270111902716547, -0.1787899950787401604, 0.04921259837143338728 ) ) ;
#26016 = CARTESIAN_POINT ( 'NONE',  ( 0.1264236179284866091, -0.1432086613635592531, 0.1264236179284866091 ) ) ;
#26017 = CARTESIAN_POINT ( 'NONE',  ( 0.8759842519685039353, -0.1574803149606299191, 1.328740157372787278 ) ) ;
#26018 = EDGE_LOOP ( 'NONE', ( #10782, #7108, #31485, #4141 ) ) ;
#26019 = ( BOUNDED_CURVE ( )  B_SPLINE_CURVE ( 2, ( #24543, #17115, #39145, #10173, #20703, #35344, #13079, #28396, #46338 ),
 .UNSPECIFIED., .F., .F. ) 
 B_SPLINE_CURVE_WITH_KNOTS ( ( 3, 2, 2, 2, 3 ),
 ( 0.3900000000000000133, 0.3925000000000000155, 0.3950000000000000178, 0.3975000000000000200, 0.4000000000000000222 ),
 .UNSPECIFIED. ) 
 CURVE ( )  GEOMETRIC_REPRESENTATION_ITEM ( )  RATIONAL_B_SPLINE_CURVE ( ( 1.000000000000000000, 0.9238795325112869605, 1.000000000000000000, 0.9238795325112869605, 1.000000000000000000, 0.9238795325112869605, 1.000000000000000000, 0.9238795325112869605, 1.000000000000000000 ) ) 
 REPRESENTATION_ITEM ( '' )  ) ;
#26020 = AXIS2_PLACEMENT_3D ( 'NONE', #37128, #18911, #33568 ) ;
#26021 = ORIENTED_EDGE ( 'NONE', *, *, #22130, .F. ) ;
#26022 = CARTESIAN_POINT ( 'NONE',  ( 0.9500414927467377701, -0.1787899950787401604, 0.8464566928596233275 ) ) ;
#26023 = CARTESIAN_POINT ( 'NONE',  ( 0.1113553986120547346, 0.08562992136736949367, -0.1113553986120547346 ) ) ;
#26024 = CARTESIAN_POINT ( 'NONE',  ( -0.9500414927467378812, -0.1787899950787401604, 1.279527559001355286 ) ) ;
#26025 = EDGE_LOOP ( 'NONE', ( #29759, #16409 ) ) ;
#26026 = CARTESIAN_POINT ( 'NONE',  ( -0.2559055118110236116, -0.05426249550635786623, -0.03952467149259050738 ) ) ;
#26027 = AXIS2_PLACEMENT_3D ( 'NONE', #2716, #4711, #42011 ) ;
#26028 = CARTESIAN_POINT ( 'NONE',  ( -0.8759842519685039353, -0.1787899950787401882, 0.1747047243556852092 ) ) ;
#26029 = DIRECTION ( 'NONE',  ( 0.000000000000000000, -1.000000000000000000, 0.000000000000000000 ) ) ;
#26030 = CYLINDRICAL_SURFACE ( 'NONE', #15215, 0.1003937007874011050 ) ;
#26031 = CARTESIAN_POINT ( 'NONE',  ( 0.1264236179284866091, -0.7890019209851437676, 0.1264236179284866091 ) ) ;
#26032 = ORIENTED_EDGE ( 'NONE', *, *, #37271, .T. ) ;
#26033 = CARTESIAN_POINT ( 'NONE',  ( 0.000000000000000000, 0.4668427075568346574, -0.7022306805398661478 ) ) ;
#26034 = ORIENTED_EDGE ( 'NONE', *, *, #22414, .F. ) ;
#26035 = CARTESIAN_POINT ( 'NONE',  ( 0.8759842519685039353, 0.1787899950787401882, 1.016240157426551161 ) ) ;
#26036 = EDGE_CURVE ( 'NONE', #40552, #12346, #25979, .T. ) ;
#26037 = CARTESIAN_POINT ( 'NONE',  ( 0.000000000000000000, 0.000000000000000000, 0.09842519685039370636 ) ) ;
#26038 = CARTESIAN_POINT ( 'NONE',  ( -0.6971942568897626646, -0.07405724077823297447, 0.7529527558517473684 ) ) ;
#26039 = ADVANCED_FACE ( 'NONE', ( #13319 ), #24107, .F. ) ;
#26040 = EDGE_CURVE ( 'NONE', #6663, #43060, #331, .T. ) ;
#26041 = CARTESIAN_POINT ( 'NONE',  ( -0.9500414927467377701, 0.1787899950787401604, 1.845472440891119392 ) ) ;
#26042 = CARTESIAN_POINT ( 'NONE',  ( -0.1787899950787401604, -0.5196850393163150450, -0.07405724077823318263 ) ) ;
#26043 = EDGE_LOOP ( 'NONE', ( #13518, #4271, #18111, #2609, #4671, #31359 ) ) ;
#26044 = CIRCLE ( 'NONE', #27587, 0.07874015748031489015 ) ;
#26045 = CARTESIAN_POINT ( 'NONE',  ( -0.6971942568897637749, 2.189545951927499583E-17, 0.04675196845017354913 ) ) ;
#26046 = CARTESIAN_POINT ( 'NONE',  ( -0.9412147342319837628, -0.1574803149606297803, 0.9079724409448818312 ) ) ;
#26047 = DIRECTION ( 'NONE',  ( 1.000000000000000000, 0.000000000000000000, -0.000000000000000000 ) ) ;
#26048 = CARTESIAN_POINT ( 'NONE',  ( -0.1797182628040039365, -1.064020187535801298, 0.000000000000000000 ) ) ;
#26049 = CARTESIAN_POINT ( 'NONE',  ( 0.7185039370078739607, 0.000000000000000000, 4.498031496062992574 ) ) ;
#26050 = CARTESIAN_POINT ( 'NONE',  ( -1.033464566929133799, 0.000000000000000000, 1.456692913278299084 ) ) ;
#26051 = CARTESIAN_POINT ( 'NONE',  ( 1.054774247047244096, 0.000000000000000000, 0.8932086613635591421 ) ) ;
#26052 = AXIS2_PLACEMENT_3D ( 'NONE', #6164, #31134, #31369 ) ;
#26053 = CARTESIAN_POINT ( 'NONE',  ( 0.8070866141732283561, -0.0009842519685049383633, 0.7574803149606299524 ) ) ;
#26054 = CARTESIAN_POINT ( 'NONE',  ( 0.7185039370078739607, 1.928577636452523993E-17, 1.407480314960629864 ) ) ;
#26055 = CARTESIAN_POINT ( 'NONE',  ( 0.7128155616400300154, -0.03638212410272396308, 1.983943496710521837 ) ) ;
#26056 = CIRCLE ( 'NONE', #30654, 0.1574803149606299191 ) ;
#26057 = DIRECTION ( 'NONE',  ( 7.083454193571959410E-15, 0.000000000000000000, 1.000000000000000000 ) ) ;
#26059 = CARTESIAN_POINT ( 'NONE',  ( 0.1555213372790610893, 0.1050481006241530957, 0.09364190366146164790 ) ) ;
#26058 = CARTESIAN_POINT ( 'NONE',  ( 1.054774247047244540, -0.07405724077823318263, 0.8464566928596233275 ) ) ;
#26060 = CARTESIAN_POINT ( 'NONE',  ( -1.094772975963752103E-17, -0.7189960629383621571, -0.1787899950787401882 ) ) ;
#26061 = EDGE_LOOP ( 'NONE', ( #9198, #23128, #9707, #6201, #17630, #4518, #45374, #11786, #34566, #31801, #8038 ) ) ;
#26062 = FACE_OUTER_BOUND ( 'NONE', #9711, .T. ) ;
#26063 = DIRECTION ( 'NONE',  ( 0.000000000000000000, -1.000000000000000000, 0.000000000000000000 ) ) ;
#26064 = CARTESIAN_POINT ( 'NONE',  ( 1.002407869896990045, 0.1264236179284866091, 1.168799212544661348 ) ) ;
#26065 = CARTESIAN_POINT ( 'NONE',  ( 0.000000000000000000, 0.6241017553149685870, 0.3240160679609074834 ) ) ;
#26066 = CARTESIAN_POINT ( 'NONE',  ( -0.1574803149606299191, -1.681102362204724532, 0.000000000000000000 ) ) ;
#26067 = DIRECTION ( 'NONE',  ( 0.000000000000000000, 1.000000000000000000, 0.000000000000000000 ) ) ;
#26068 = CYLINDRICAL_SURFACE ( 'NONE', #41995, 0.04921259842519688787 ) ;
#26069 = CARTESIAN_POINT ( 'NONE',  ( -0.8019270111902717657, 0.1787899950787401604, 0.3100393700249766682 ) ) ;
#26070 = ORIENTED_EDGE ( 'NONE', *, *, #33363, .T. ) ;
#26071 = CARTESIAN_POINT ( 'NONE',  ( 1.033464566929133799, 0.000000000000000000, 0.3248031496062992463 ) ) ;
#26072 = CARTESIAN_POINT ( 'NONE',  ( -0.06523048226347956391, -0.2859251967428664831, 0.1574803149606297803 ) ) ;
#26073 = CARTESIAN_POINT ( 'NONE',  ( -1.054774247047244096, 0.000000000000000000, 1.675688976324189117 ) ) ;
#26074 = CARTESIAN_POINT ( 'NONE',  ( -0.9500414927467377701, -0.1787899950787401604, 0.8415354330171020969 ) ) ;
#26075 = CARTESIAN_POINT ( 'NONE',  ( -0.9500414927467378812, 0.1787899950787401604, 0.5462598424659214080 ) ) ;
#26076 = CONICAL_SURFACE ( 'NONE', #7687, 0.08090551181102362266, 0.9599310885968742602 ) ;
#26077 = CARTESIAN_POINT ( 'NONE',  ( -0.7185039370078739607, 1.928577636452523993E-17, 0.09842519674286673292 ) ) ;
#26078 = CARTESIAN_POINT ( 'NONE',  ( 1.033464566929134687, -0.06523048226347956391, 0.9916338582677169944 ) ) ;
#26079 = CARTESIAN_POINT ( 'NONE',  ( 0.1121631700669272619, 0.09842519685039372024, -0.2206756344348396182 ) ) ;
#26080 = CARTESIAN_POINT ( 'NONE',  ( 0.2066929133858268486, -0.5175744617845222662, -0.9076376772307633845 ) ) ;
#26081 = CARTESIAN_POINT ( 'NONE',  ( 0.1787899950787401882, -0.3510097950008925216, -2.189545951927503898E-17 ) ) ;
#26082 = CARTESIAN_POINT ( 'NONE',  ( 0.07338256679960847295, -0.09842519685039370636, 0.1314280838991750133 ) ) ;
#26083 = CARTESIAN_POINT ( 'NONE',  ( -1.033464566929133355, 0.06523048226348168721, 1.892224409341292546 ) ) ;
#26084 = DIRECTION ( 'NONE',  ( -3.469446951953590129E-15, -1.000000000000000000, 0.000000000000000000 ) ) ;
#26085 = PRODUCT ( 'Hook Bracket', 'Hook Bracket', '', ( #31237 ) ) ;
#26086 = ADVANCED_FACE ( 'NONE', ( #6333 ), #6575, .T. ) ;
#26088 = CARTESIAN_POINT ( 'NONE',  ( 0.2559043144403723158, -0.05922267293569646873, -0.04185085927340410905 ) ) ;
#26087 = AXIS2_PLACEMENT_3D ( 'NONE', #42719, #28645, #6076 ) ;
#26089 = CARTESIAN_POINT ( 'NONE',  ( -1.054774247047244540, -0.07405724077823318263, 0.2559055117572600624 ) ) ;
#26090 = EDGE_CURVE ( 'NONE', #43509, #9873, #14786, .T. ) ;
#26091 = B_SPLINE_CURVE_WITH_KNOTS ( 'NONE', 3,
 ( #38866, #9884, #36242, #28590, #39328, #32420, #6504, #3628, #40031, #14190, #40268, #32658, #46996, #7453, #7, #14658, #39790, #21849, #6984, #7226, #43154 ),
 .UNSPECIFIED., .F., .F.,
 ( 4, 2, 1, 1, 2, 2, 2, 1, 1, 1, 2, 2, 4 ),
 ( 0.000000000000000000, 0.1250000000000001388, 0.1875000000000001665, 0.2187500000000002498, 0.2343750000000003053, 0.2500000000000003886, 0.3750000000000004996, 0.4375000000000004996, 0.4687500000000004996, 0.4843750000000006106, 0.4921875000000006661, 0.5000000000000006661, 1.000000000000000000 ),
 .UNSPECIFIED. ) ;
#26092 = ORIENTED_EDGE ( 'NONE', *, *, #28058, .F. ) ;
#26093 = ADVANCED_FACE ( 'NONE', ( #36998, #39626 ), #29631, .F. ) ;
#26094 = CARTESIAN_POINT ( 'NONE',  ( -0.6971942568897648851, -0.07405724077823297447, 1.309055118056473122 ) ) ;
#26095 = ORIENTED_EDGE ( 'NONE', *, *, #11174, .F. ) ;
#26096 = EDGE_CURVE ( 'NONE', #23956, #8667, #22842, .T. ) ;
#26097 = CARTESIAN_POINT ( 'NONE',  ( 0.07405724077823318263, -1.277559055064345861, -0.1787899950787401604 ) ) ;
#26098 = CARTESIAN_POINT ( 'NONE',  ( -0.07405724077823318263, -1.464566929080096225, -0.1787899950787401604 ) ) ;
#26099 = DIRECTION ( 'NONE',  ( -0.002207034709573998596, 0.8344568503083535926, -0.5510688649989696763 ) ) ;
#26100 = CARTESIAN_POINT ( 'NONE',  ( 0.8107537697050253289, 0.1574803149606300301, 0.4158464566929134243 ) ) ;
#26101 = LINE ( 'NONE', #27064, #37773 ) ;
#26102 = CARTESIAN_POINT ( 'NONE',  ( -1.033464566929134687, 0.06523048226347956391, 1.104822834538142340 ) ) ;
#26103 = CARTESIAN_POINT ( 'NONE',  ( 1.054774247047244540, 0.07405724077823318263, 0.4625984251430869665 ) ) ;
#26104 = LINE ( 'NONE', #32177, #6901 ) ;
#26105 = CARTESIAN_POINT ( 'NONE',  ( -0.06523048226347956391, -0.2711614173228347746, -0.1574803149606300301 ) ) ;
#26106 = VERTEX_POINT ( 'NONE', #47316 ) ;
#26107 = CARTESIAN_POINT ( 'NONE',  ( 1.033464566929134687, -0.06523048226347956391, 2.005413385719245323 ) ) ;
#26108 = EDGE_LOOP ( 'NONE', ( #4561, #38853, #36006, #32379 ) ) ;
#26109 = FACE_OUTER_BOUND ( 'NONE', #16588, .T. ) ;
#26110 = CARTESIAN_POINT ( 'NONE',  ( -1.054774247047244096, 0.000000000000000000, 0.8932086613635591421 ) ) ;
#26111 = CARTESIAN_POINT ( 'NONE',  ( 1.033464566929134687, -0.06523048226347956391, 0.9916338582677171054 ) ) ;
#26112 = DIRECTION ( 'NONE',  ( 1.000000000000000000, -3.469446951953614189E-15, 0.000000000000000000 ) ) ;
#26113 = CONICAL_SURFACE ( 'NONE', #5436, 0.2471922904502826812, 0.5235987755982992597 ) ;
#26114 = CARTESIAN_POINT ( 'NONE',  ( -0.1574803149606299191, 0.06245656531175266396, -0.1492449156640648644 ) ) ;
#26115 = CARTESIAN_POINT ( 'NONE',  ( -0.1696281918730704608, -0.08954833399976612485, -0.01761539643617799841 ) ) ;
#26116 = FACE_OUTER_BOUND ( 'NONE', #37685, .T. ) ;
#26118 = CARTESIAN_POINT ( 'NONE',  ( -0.3053406547161471862, 0.05476901150469691559, 1.034474086880956989 ) ) ;
#26117 = AXIS2_PLACEMENT_3D ( 'NONE', #16457, #13336, #30860 ) ;
#26119 = CARTESIAN_POINT ( 'NONE',  ( 1.054774247047244540, 0.07405724077823318263, 0.5364173227808821665 ) ) ;
#26120 = ORIENTED_EDGE ( 'NONE', *, *, #11974, .F. ) ;
#26121 = CARTESIAN_POINT ( 'NONE',  ( 0.8107537697050254399, -0.1574803149606297803, 0.8243110236220465570 ) ) ;
#26122 = CARTESIAN_POINT ( 'NONE',  ( 0.7185039370078739607, 1.928577636452523993E-17, 0.5708661416247566844 ) ) ;
#26123 = CARTESIAN_POINT ( 'NONE',  ( -0.1264236179284866091, -1.501476377898992354, -0.1264236179284866091 ) ) ;
#26124 = CARTESIAN_POINT ( 'NONE',  ( -1.094772975963752103E-17, -0.7632874015210393548, -0.1787899950787401882 ) ) ;
#26125 = AXIS2_PLACEMENT_3D ( 'NONE', #41383, #18660, #33550 ) ;
#26126 = CARTESIAN_POINT ( 'NONE',  ( -0.1574803149606297803, -1.245570866141732624, 0.06523048226347956391 ) ) ;
#26127 = CARTESIAN_POINT ( 'NONE',  ( 0.9873396505805591694, -0.1113553986120547346, 1.136811023514519681 ) ) ;
#26128 = ( BOUNDED_CURVE ( )  B_SPLINE_CURVE ( 2, ( #39647, #107, #28684, #32745, #10213, #24816, #25301, #39416, #43003 ),
 .UNSPECIFIED., .F., .T. ) 
 B_SPLINE_CURVE_WITH_KNOTS ( ( 3, 2, 2, 2, 3 ),
 ( 0.8199999999999999512, 0.8225000000000000089, 0.8249999999999999556, 0.8275000000000000133, 0.8299999999999999600 ),
 .UNSPECIFIED. ) 
 CURVE ( )  GEOMETRIC_REPRESENTATION_ITEM ( )  RATIONAL_B_SPLINE_CURVE ( ( 1.000000000000000000, 0.9238795325112899581, 1.000000000000000000, 0.9238795325112869605, 1.000000000000000000, 0.9238795325112869605, 1.000000000000000000, 0.9238795325112829637, 1.000000000000000000 ) ) 
 REPRESENTATION_ITEM ( '' )  ) ;
#26129 = DIRECTION ( 'NONE',  ( 0.000000000000000000, 0.000000000000000000, -1.000000000000000000 ) ) ;
#26130 = ORIENTED_EDGE ( 'NONE', *, *, #29391, .F. ) ;
#26131 = VERTEX_POINT ( 'NONE', #44170 ) ;
#26132 = VERTEX_POINT ( 'NONE', #6807 ) ;
#26133 = CARTESIAN_POINT ( 'NONE',  ( -0.8759842519685039353, -0.1787899950787401882, 1.749507873961984483 ) ) ;
#26134 = CARTESIAN_POINT ( 'NONE',  ( 0.8759842519685039353, 0.1787899950787401882, 1.690452755851748146 ) ) ;
#26135 = CARTESIAN_POINT ( 'NONE',  ( -0.1574803149606300301, -1.319389763671999782, -0.06523048226347956391 ) ) ;
#26136 = CARTESIAN_POINT ( 'NONE',  ( -0.9500414927467378812, 0.1787899950787401604, 0.8218503936470251681 ) ) ;
#26137 = CARTESIAN_POINT ( 'NONE',  ( -0.05814395269903865904, -0.2619241685425540700, -0.3078067560681180259 ) ) ;
#26138 = CARTESIAN_POINT ( 'NONE',  ( 0.8019270111902717657, -0.1787899950787401604, 0.2903543306548980185 ) ) ;
#26139 = CARTESIAN_POINT ( 'NONE',  ( -0.9500414927467377701, -0.1787899950787401604, 1.274606299158834277 ) ) ;
#26140 = CARTESIAN_POINT ( 'NONE',  ( 0.002794899976001078128, -0.1008940036867598672, 0.1008370195737266495 ) ) ;
#26141 = DIRECTION ( 'NONE',  ( 1.822029033848725028E-16, 0.000000000000000000, 1.000000000000000000 ) ) ;
#26142 = CARTESIAN_POINT ( 'NONE',  ( -0.6971942568897648851, 0.07405724077823318263, 1.619094488135213838 ) ) ;
#26143 = CARTESIAN_POINT ( 'NONE',  ( -0.8107537697050253289, 0.1574803149606300301, 1.823326771546016856 ) ) ;
#26144 = ORIENTED_EDGE ( 'NONE', *, *, #29340, .T. ) ;
#26145 = DIRECTION ( 'NONE',  ( 0.000000000000000000, 0.6156614753256609562, 0.7880107536067200158 ) ) ;
#26146 = CARTESIAN_POINT ( 'NONE',  ( -0.9873396505805591694, 0.1113553986120547346, 1.550196850393700920 ) ) ;
#26147 = CARTESIAN_POINT ( 'NONE',  ( 0.7185039370078739607, 1.928577636452523993E-17, 0.9645669290263307882 ) ) ;
#26148 = CARTESIAN_POINT ( 'NONE',  ( 0.8759842519685039353, 0.1787899950787401882, 1.572342519631275692 ) ) ;
#26149 = CARTESIAN_POINT ( 'NONE',  ( -0.1602016258198147580, -0.09842519685039370636, -0.1931405315332122008 ) ) ;
#26150 = DIRECTION ( 'NONE',  ( 1.822029033848725028E-16, 0.000000000000000000, 1.000000000000000000 ) ) ;
#26151 = ORIENTED_EDGE ( 'NONE', *, *, #14364, .F. ) ;
#26152 = EDGE_CURVE ( 'NONE', #42269, #28928, #25984, .T. ) ;
#26153 = AXIS2_PLACEMENT_3D ( 'NONE', #24295, #38893, #46783 ) ;
#26154 = ORIENTED_EDGE ( 'NONE', *, *, #2644, .T. ) ;
#26155 = ( CONVERSION_BASED_UNIT ( 'INCH', #22538 ) LENGTH_UNIT ( ) NAMED_UNIT ( #24356 ) ) ;
#26156 = EDGE_LOOP ( 'NONE', ( #1024, #4280, #17329 ) ) ;
#26157 = CIRCLE ( 'NONE', #37596, 0.04921259842519686706 ) ;
#26158 = EDGE_CURVE ( 'NONE', #31350, #13767, #22327, .T. ) ;
#26159 = AXIS2_PLACEMENT_3D ( 'NONE', #10257, #43528, #10743 ) ;
#26160 = CARTESIAN_POINT ( 'NONE',  ( 0.1264236179284866091, -0.8863188975840314843, -0.1264236179284866091 ) ) ;
#26161 = CARTESIAN_POINT ( 'NONE',  ( 0.1264236179284866091, -0.4630905511273386010, 0.1264236179284866091 ) ) ;
#26162 = CARTESIAN_POINT ( 'NONE',  ( -0.07405724077823318263, -1.134842519631275914, 0.1787899950787401604 ) ) ;
#26163 = ORIENTED_EDGE ( 'NONE', *, *, #26287, .F. ) ;
#26164 = SURFACE_SIDE_STYLE ('',( #43875 ) ) ;
#26165 = ( NAMED_UNIT ( * ) PLANE_ANGLE_UNIT ( ) SI_UNIT ( $, .RADIAN. ) ) ;
#26166 = CARTESIAN_POINT ( 'NONE',  ( -0.07444174185955065859, -0.3233705812365890719, -0.1797182628040039087 ) ) ;
#26167 = CARTESIAN_POINT ( 'NONE',  ( 0.2341188618547038192, 0.1603256443482194427, -0.2993662881638891604 ) ) ;
#26168 = CARTESIAN_POINT ( 'NONE',  ( -0.1264236179284866091, -0.03986220467064590517, 0.1264236179284866091 ) ) ;
#26169 = DIRECTION ( 'NONE',  ( 0.000000000000000000, 0.000000000000000000, -1.000000000000000000 ) ) ;
#26170 = CARTESIAN_POINT ( 'NONE',  ( 0.9500414927467378812, -0.1787899950787401604, 0.8021653542769460188 ) ) ;
#26172 = ( LENGTH_UNIT ( ) NAMED_UNIT ( * ) SI_UNIT ( $, .METRE. ) ) ;
#26171 = FILL_AREA_STYLE_COLOUR ( '', #13215 ) ;
#26174 = CARTESIAN_POINT ( 'NONE',  ( -0.2066929133858267931, -0.9875035750853327077, -1.463737590216208861 ) ) ;
#26173 = PLANE ( 'NONE',  #4270 ) ;
#26175 = CARTESIAN_POINT ( 'NONE',  ( 0.8107537697050254399, 0.1574803149606300301, 0.4552165354330711677 ) ) ;
#26176 = CARTESIAN_POINT ( 'NONE',  ( 0.7495606340400177148, -0.1264236179284866091, 1.783956692859621995 ) ) ;
#26177 = CARTESIAN_POINT ( 'NONE',  ( 0.8759842519685039353, 0.000000000000000000, 1.990649606245448844 ) ) ;
#26178 = ORIENTED_EDGE ( 'NONE', *, *, #35766, .T. ) ;
#26179 = AXIS2_PLACEMENT_3D ( 'NONE', #24451, #13440, #6699 ) ;
#26180 = CARTESIAN_POINT ( 'NONE',  ( 0.8107537697050234415, -0.1574803149606297803, 0.03690944881889771101 ) ) ;
#26181 = CARTESIAN_POINT ( 'NONE',  ( -1.181162989532618060E-16, -0.3937007874015746034, -0.3937007874015748254 ) ) ;
#26183 = CARTESIAN_POINT ( 'NONE',  ( -0.1787899950787401604, -0.2391732282926934683, 0.07405724077823318263 ) ) ;
#26182 = CARTESIAN_POINT ( 'NONE',  ( 0.1574803149606300301, -0.9404527557979834862, -0.06523048226347956391 ) ) ;
#26184 = CARTESIAN_POINT ( 'NONE',  ( -0.7185039370078739607, 1.928577636452523993E-17, 0.1870078740157480324 ) ) ;
#26185 = CARTESIAN_POINT ( 'NONE',  ( 0.1264236179284866091, -1.166830708607653477, 0.1264236179284866091 ) ) ;
#26186 = CARTESIAN_POINT ( 'NONE',  ( 0.9500414927467378812, -0.1787899950787401604, 0.1771653542769452139 ) ) ;
#26187 = CARTESIAN_POINT ( 'NONE',  ( 0.1636096891713402501, 0.08042878232803850336, -0.1393067576844427280 ) ) ;
#26188 = CONICAL_SURFACE ( 'NONE', #2414, 0.1377952755905513804, 0.9599310885968808105 ) ;
#26189 = CARTESIAN_POINT ( 'NONE',  ( -0.7495606340400177148, 0.1264236179284866091, 1.808562992072220377 ) ) ;
#26190 = EDGE_LOOP ( 'NONE', ( #33713, #35860, #29167, #23061, #1312, #13644 ) ) ;
#26191 = CARTESIAN_POINT ( 'NONE',  ( -0.9500414927467378812, 0.1787899950787401604, 1.215551181048599272 ) ) ;
#26192 = CARTESIAN_POINT ( 'NONE',  ( -0.7185039370078739607, 0.000000000000000000, -2.869337061179095023E-17 ) ) ;
#26193 = CARTESIAN_POINT ( 'NONE',  ( 0.6971942568897637749, 2.189545951927499583E-17, 1.306594488135212728 ) ) ;
#26194 = TOROIDAL_SURFACE ( 'NONE', #11664, 0.01968503937007873988, 0.009842519685039369942 ) ;
#26195 = AXIS2_PLACEMENT_3D ( 'NONE', #6407, #21019, #35667 ) ;
#26196 = CARTESIAN_POINT ( 'NONE',  ( 0.7495606340400177148, 0.1264236179284866091, 1.966043307032850462 ) ) ;
#26197 = CARTESIAN_POINT ( 'NONE',  ( -0.7495606340400177148, -0.1264236179284866091, 0.9916338582139527791 ) ) ;
#26198 = CARTESIAN_POINT ( 'NONE',  ( -0.09591045553298832571, -0.09842280622452256877, -0.1509607186031187431 ) ) ;
#26199 = CARTESIAN_POINT ( 'NONE',  ( -0.05642593091638983815, -0.2629167058585551442, -0.05524818609633137811 ) ) ;
#26200 = CARTESIAN_POINT ( 'NONE',  ( 0.8019270111902716547, -0.1787899950787401604, 0.4872047243556847929 ) ) ;
#26201 = CARTESIAN_POINT ( 'NONE',  ( -0.6971942568897648851, 0.07405724077823318263, 0.3937007873478114983 ) ) ;
#26202 = CARTESIAN_POINT ( 'NONE',  ( -0.8759842519685039353, -0.1787899950787401882, 0.7997047243556849594 ) ) ;
#26203 = ORIENTED_EDGE ( 'NONE', *, *, #13858, .F. ) ;
#26204 = ORIENTED_EDGE ( 'NONE', *, *, #45808, .F. ) ;
#26205 = CARTESIAN_POINT ( 'NONE',  ( -0.8107537697050254399, 0.1574803149606300301, 1.360728346456693050 ) ) ;
#26206 = VERTEX_POINT ( 'NONE', #18780 ) ;
#26207 = CARTESIAN_POINT ( 'NONE',  ( -0.8759842519685039353, 0.1574803149606299191, 0.2165354330708661457 ) ) ;
#26208 = CARTESIAN_POINT ( 'NONE',  ( 1.054774247047244096, 0.000000000000000000, 1.090059055064346527 ) ) ;
#26209 = DIRECTION ( 'NONE',  ( 0.000000000000000000, 0.000000000000000000, -1.000000000000000000 ) ) ;
#26210 = ORIENTED_EDGE ( 'NONE', *, *, #37653, .T. ) ;
#26211 = CARTESIAN_POINT ( 'NONE',  ( 0.7495606340400177148, 0.1264236179284866091, 1.966043307032850462 ) ) ;
#26212 = ADVANCED_FACE ( 'NONE', ( #3211 ), #3427, .T. ) ;
#26213 = CARTESIAN_POINT ( 'NONE',  ( -0.8759842519685039353, 0.1787899950787401882, 0.07135826766277185429 ) ) ;
#26214 = CARTESIAN_POINT ( 'NONE',  ( -0.1264236179284866091, -1.389395621772545608, 0.1264236179284866091 ) ) ;
#26215 = EDGE_LOOP ( 'NONE', ( #12670, #33126, #40916, #29870 ) ) ;
#26216 = CARTESIAN_POINT ( 'NONE',  ( -0.1787899950787401604, -0.4360236219934807145, -0.07405724077823318263 ) ) ;
#26217 = CARTESIAN_POINT ( 'NONE',  ( -0.3010010101267347471, -0.07503014570242728942, 0.7260258031100994547 ) ) ;
#26218 = ORIENTED_EDGE ( 'NONE', *, *, #30192, .F. ) ;
#26219 = CARTESIAN_POINT ( 'NONE',  ( 1.002407869896990045, -0.1264236179284866091, 1.198326771599779628 ) ) ;
#26220 = AXIS2_PLACEMENT_3D ( 'NONE', #44119, #30032, #11795 ) ;
#26221 = CARTESIAN_POINT ( 'NONE',  ( -0.1377952755905511861, 0.1564960629921283985, 0.8070866141732283561 ) ) ;
#26222 = CARTESIAN_POINT ( 'NONE',  ( 0.008625679036690871507, -0.08625453335776224473, -0.1261914363111028836 ) ) ;
#26223 = CARTESIAN_POINT ( 'NONE',  ( 1.002407869896990045, 0.1264236179284866091, 0.1451771653005673179 ) ) ;
#26224 = CIRCLE ( 'NONE', #7048, 0.2362204724409449064 ) ;
#26225 = VECTOR ( 'NONE', #11098, 39.37007874015748143 ) ;
#26226 = CARTESIAN_POINT ( 'NONE',  ( -0.07405724077823318263, -1.784448818843874962, -0.1787899950787401604 ) ) ;
#26227 = CARTESIAN_POINT ( 'NONE',  ( 3.284318927891251994E-17, -1.683562992072220599, 0.1787899950787401882 ) ) ;
#26228 = APPLICATION_PROTOCOL_DEFINITION ( 'draft international standard', 'automotive_design', 1998, #13765 ) ;
#26229 = CARTESIAN_POINT ( 'NONE',  ( -0.8759842519685039353, -0.1574803149606299191, 1.131889763672000004 ) ) ;
#26230 = ORIENTED_EDGE ( 'NONE', *, *, #18187, .T. ) ;
#26231 = CARTESIAN_POINT ( 'NONE',  ( -0.6971942568897648851, 0.07405724077823318263, 0.5954724408911187261 ) ) ;
#26232 = CARTESIAN_POINT ( 'NONE',  ( -0.1113553986120547346, -0.7706692913385826404, 0.1113553986120547346 ) ) ;
#26233 = CARTESIAN_POINT ( 'NONE',  ( -0.1797182628040039365, -1.418350896197218436, 0.000000000000000000 ) ) ;
#26234 = DIRECTION ( 'NONE',  ( 0.000000000000000000, 0.000000000000000000, 1.000000000000000000 ) ) ;
#26235 = CARTESIAN_POINT ( 'NONE',  ( 0.8759842519685039353, -0.1787899950787401882, 1.434547244040724534 ) ) ;
#26236 = CARTESIAN_POINT ( 'NONE',  ( 0.8759842519685039353, 0.1787899950787401882, 1.724901574749385880 ) ) ;
#26237 = CARTESIAN_POINT ( 'NONE',  ( -0.9412147342319837628, -0.1574803149606297803, 1.646161417215307843 ) ) ;
#26239 = CARTESIAN_POINT ( 'NONE',  ( -0.7444854923987453965, 0.09565579475716033675, 1.981284257674885918 ) ) ;
#26238 = FACE_OUTER_BOUND ( 'NONE', #27086, .T. ) ;
#26240 = DIRECTION ( 'NONE',  ( 0.000000000000000000, 1.000000000000000000, 0.000000000000000000 ) ) ;
#26241 = DIRECTION ( 'NONE',  ( -1.000000000000000000, 0.000000000000000000, 0.000000000000000000 ) ) ;
#26242 = LINE ( 'NONE', #8003, #23976 ) ;
#26243 = CARTESIAN_POINT ( 'NONE',  ( 0.6971942568897626646, -0.07405724077823297447, 0.3198818897100162983 ) ) ;
#26244 = CARTESIAN_POINT ( 'NONE',  ( -0.7646288533564489232, -0.1113553986120547346, 1.717519684931842594 ) ) ;
#26245 = CARTESIAN_POINT ( 'NONE',  ( 0.5555748031496103856, 0.7681739484881628943, -0.04983111751016747887 ) ) ;
#26246 = DIRECTION ( 'NONE',  ( 0.000000000000000000, -0.000000000000000000, 1.000000000000000000 ) ) ;
#26247 = CARTESIAN_POINT ( 'NONE',  ( -0.6971942568897637749, 2.189545951927499583E-17, 1.262303149552535420 ) ) ;
#26248 = CARTESIAN_POINT ( 'NONE',  ( 0.9412147342319837628, 0.1574803149606300301, 0.6373031494987718704 ) ) ;
#26249 = EDGE_LOOP ( 'NONE', ( #36414, #26144, #35729, #10633, #7330 ) ) ;
#26250 = CARTESIAN_POINT ( 'NONE',  ( -1.033464566929133799, 0.000000000000000000, 0.1968503935932602311 ) ) ;
#26251 = CARTESIAN_POINT ( 'NONE',  ( -0.1884454360679181650, -0.3999716016534896057, -0.9995191014872203406 ) ) ;
#26252 = VERTEX_POINT ( 'NONE', #33203 ) ;
#26253 = CARTESIAN_POINT ( 'NONE',  ( 0.07444174185955046430, -0.05270128989800624414, -0.1797182628040039087 ) ) ;
#26254 = CARTESIAN_POINT ( 'NONE',  ( -0.8759842519685039353, -0.1574803149606299191, 0.3051181101286932762 ) ) ;
#26255 = CARTESIAN_POINT ( 'NONE',  ( -0.07405724077823318263, -1.257874015694269376, 0.1787899950787401604 ) ) ;
#26256 = CARTESIAN_POINT ( 'NONE',  ( 0.4453382816733590377, 4.766607801171850497E-17, 0.000000000000000000 ) ) ;
#26257 = CARTESIAN_POINT ( 'NONE',  ( 0.6971942568897648851, -0.07405724077823297447, 1.658464566875369472 ) ) ;
#26258 = CARTESIAN_POINT ( 'NONE',  ( -0.7185039370078746268, 0.06523048226347956391, 1.129429133858268042 ) ) ;
#26259 = DIRECTION ( 'NONE',  ( 1.822029033848725028E-16, 0.000000000000000000, 1.000000000000000000 ) ) ;
#26261 = CARTESIAN_POINT ( 'NONE',  ( 0.7185039370078746268, 0.06523048226347956391, 1.680610236220472009 ) ) ;
#26260 = CARTESIAN_POINT ( 'NONE',  ( 0.1594510458733827685, -0.09722652869640824314, 0.1125335630252017605 ) ) ;
#26262 = CARTESIAN_POINT ( 'NONE',  ( 0.6971942568897626646, -0.07405724077823297447, 0.04921259837143338728 ) ) ;
#26263 = CARTESIAN_POINT ( 'NONE',  ( -0.9500414927467377701, -0.1787899950787401604, 0.05413385821395302888 ) ) ;
#26264 = CARTESIAN_POINT ( 'NONE',  ( -0.1787899950787401604, -0.1161417322297011862, 0.07405724077823318263 ) ) ;
#26265 = ORIENTED_EDGE ( 'NONE', *, *, #6011, .F. ) ;
#26266 = AXIS2_PLACEMENT_3D ( 'NONE', #7486, #36966, #18743 ) ;
#26267 = CARTESIAN_POINT ( 'NONE',  ( -0.1574803149606297803, 0.09301181102362202080, 0.06523048226347956391 ) ) ;
#26268 = CARTESIAN_POINT ( 'NONE',  ( 0.2088134963345943673, -0.06712557525760230737, -0.1648743713627059404 ) ) ;
#26269 = ADVANCED_FACE ( 'NONE', ( #17841 ), #25277, .T. ) ;
#26270 = CARTESIAN_POINT ( 'NONE',  ( 0.8759842519685039353, -0.1787899950787401882, 0.9227362204186770889 ) ) ;
#26271 = CARTESIAN_POINT ( 'NONE',  ( -1.054774247047244540, 0.07405724077823318263, 1.520669291284818758 ) ) ;
#26272 = CARTESIAN_POINT ( 'NONE',  ( -0.06523048226347956391, -0.1038385825696382520, -0.1574803149606300301 ) ) ;
#26273 = CARTESIAN_POINT ( 'NONE',  ( -0.8759842519685039353, 0.1787899950787401882, 1.257381889710015743 ) ) ;
#26274 = EDGE_CURVE ( 'NONE', #18566, #22479, #36361, .T. ) ;
#26275 = VECTOR ( 'NONE', #43952, 39.37007874015748143 ) ;
#26276 = ORIENTED_EDGE ( 'NONE', *, *, #42281, .F. ) ;
#26277 = ADVANCED_FACE ( 'NONE', ( #32958 ), #14141, .F. ) ;
#26278 = CARTESIAN_POINT ( 'NONE',  ( -1.054774247047244096, 0.000000000000000000, 0.3026574802611972648 ) ) ;
#26279 = CARTESIAN_POINT ( 'NONE',  ( 0.000000000000000000, -0.09842519685039370636, 0.000000000000000000 ) ) ;
#26280 = DIRECTION ( 'NONE',  ( 0.000000000000000000, 0.000000000000000000, -1.000000000000000000 ) ) ;
#26281 = CARTESIAN_POINT ( 'NONE',  ( 0.1787899950787401604, -0.9784704249221527483, -0.07405724077823318263 ) ) ;
#26282 = AXIS2_PLACEMENT_3D ( 'NONE', #44451, #9419, #16606 ) ;
#26283 = ORIENTED_EDGE ( 'NONE', *, *, #22561, .F. ) ;
#26284 = CARTESIAN_POINT ( 'NONE',  ( 0.07405724077823318263, 0.02657480320336980464, -0.1787899950787401604 ) ) ;
#26285 = ORIENTED_EDGE ( 'NONE', *, *, #10183, .F. ) ;
#26286 = ORIENTED_EDGE ( 'NONE', *, *, #24724, .T. ) ;
#26287 = EDGE_CURVE ( 'NONE', #26963, #30980, #39865, .T. ) ;
#26288 = FACE_OUTER_BOUND ( 'NONE', #24066, .T. ) ;
#26289 = EDGE_CURVE ( 'NONE', #31847, #12102, #14649, .T. ) ;
#26290 = DIRECTION ( 'NONE',  ( 0.000000000000000000, 0.000000000000000000, -1.000000000000000000 ) ) ;
#26291 = CARTESIAN_POINT ( 'NONE',  ( -0.1264236179284866091, -0.4729330708123779536, 0.1264236179284866091 ) ) ;
#26292 = AXIS2_PLACEMENT_3D ( 'NONE', #34593, #5584, #1743 ) ;
#26293 = CARTESIAN_POINT ( 'NONE',  ( -1.054774247047244540, 0.07405724077823318263, 0.2263779527021417270 ) ) ;
#26294 = CARTESIAN_POINT ( 'NONE',  ( -1.033464566929134687, -0.06523048226347956391, 0.8341535433070870198 ) ) ;
#26295 = DIRECTION ( 'NONE',  ( 0.000000000000000000, -1.000000000000000000, 0.000000000000000000 ) ) ;
#26296 = CARTESIAN_POINT ( 'NONE',  ( 0.1797182628040039365, -1.004965069425564961, -2.200913952912460540E-17 ) ) ;
#26297 = LINE ( 'NONE', #40854, #22541 ) ;
#26298 = CARTESIAN_POINT ( 'NONE',  ( -0.9412147342319837628, -0.1574803149606297803, 1.567421259734991690 ) ) ;
#26299 = CARTESIAN_POINT ( 'NONE',  ( 0.7495606340400177148, -0.1264236179284866091, 0.8784448818360000022 ) ) ;
#26300 = PRODUCT_DEFINITION_FORMATION_WITH_SPECIFIED_SOURCE ( 'ANY', '', #14590, .NOT_KNOWN. ) ;
#26301 = AXIS2_PLACEMENT_3D ( 'NONE', #12979, #4815, #41694 ) ;
#26302 = CARTESIAN_POINT ( 'NONE',  ( 0.8759842519685039353, 0.000000000000000000, 4.498031496062992574 ) ) ;
#26304 = CARTESIAN_POINT ( 'NONE',  ( 0.7185039370078766252, -0.06523048226348168721, 1.557578740049954558 ) ) ;
#26303 = CARTESIAN_POINT ( 'NONE',  ( 0.7100943080231756355, -0.01414046681897546467, 1.983520156233079756 ) ) ;
#26305 = DIRECTION ( 'NONE',  ( -0.5735764363510518216, 0.8191520442889876907, 1.003171929053519693E-16 ) ) ;
#26306 = CARTESIAN_POINT ( 'NONE',  ( -0.1574803149606300301, -0.6894685038294798840, -0.06523048226347956391 ) ) ;
#26307 = ( BOUNDED_CURVE ( )  B_SPLINE_CURVE ( 2, ( #30754, #12058, #19458, #37683, #34338, #11582, #33645, #16127, #8673 ),
 .UNSPECIFIED., .F., .F. ) 
 B_SPLINE_CURVE_WITH_KNOTS ( ( 3, 2, 2, 2, 3 ),
 ( 0.9599999999999999645, 0.9625000000000000222, 0.9649999999999999689, 0.9675000000000000266, 0.9699999999999999734 ),
 .UNSPECIFIED. ) 
 CURVE ( )  GEOMETRIC_REPRESENTATION_ITEM ( )  RATIONAL_B_SPLINE_CURVE ( ( 1.000000000000000000, 0.9238795325112869605, 1.000000000000000000, 0.9238795325112869605, 1.000000000000000000, 0.9238795325112869605, 1.000000000000000000, 0.9238795325112799661, 1.000000000000000000 ) ) 
 REPRESENTATION_ITEM ( '' )  ) ;
#26309 = CARTESIAN_POINT ( 'NONE',  ( 0.1564636162838604350, 0.1073287318776763866, 0.09487486835524192030 ) ) ;
#26308 = CARTESIAN_POINT ( 'NONE',  ( 0.7495606340400177148, -0.1264236179284866091, 0.8735236219934803259 ) ) ;
#26310 = CARTESIAN_POINT ( 'NONE',  ( 0.1787899950787401604, -0.7312992125446612368, 0.07405724077823318263 ) ) ;
#26311 = ORIENTED_EDGE ( 'NONE', *, *, #38358, .F. ) ;
#26312 = DIRECTION ( 'NONE',  ( -0.000000000000000000, 0.000000000000000000, -1.000000000000000000 ) ) ;
#26313 = CYLINDRICAL_SURFACE ( 'NONE', #1469, 0.2559055118110236116 ) ;
#26314 = CARTESIAN_POINT ( 'NONE',  ( 0.8759842519685039353, 0.1787899950787401882, 1.213090551127338435 ) ) ;
#26315 = ADVANCED_FACE ( 'NONE', ( #30098 ), #4158, .T. ) ;
#26316 = DIRECTION ( 'NONE',  ( -1.000000000000000000, 0.000000000000000000, 0.000000000000000000 ) ) ;
#26317 = CARTESIAN_POINT ( 'NONE',  ( -0.06523048226347956391, -1.713090551181103649, 0.1574803149606297803 ) ) ;
#26318 = CARTESIAN_POINT ( 'NONE',  ( 0.1602931993194444682, 0.1591122789105269553, 0.000000000000000000 ) ) ;
#26319 = ORIENTED_EDGE ( 'NONE', *, *, #17844, .T. ) ;
#26320 = CYLINDRICAL_SURFACE ( 'NONE', #36727, 0.1574803149606299191 ) ;
#26321 = CARTESIAN_POINT ( 'NONE',  ( -0.8019270111902717657, -0.1787899950787401604, 0.2460629920722207375 ) ) ;
#26322 = ORIENTED_EDGE ( 'NONE', *, *, #46789, .T. ) ;
#26323 = ORIENTED_EDGE ( 'NONE', *, *, #34982, .F. ) ;
#26324 = EDGE_CURVE ( 'NONE', #19773, #39762, #15687, .T. ) ;
#26325 = CARTESIAN_POINT ( 'NONE',  ( 0.1574803149606300301, 0.1126968503937008370, -0.06523048226347956391 ) ) ;
#26326 = CARTESIAN_POINT ( 'NONE',  ( 0.06523048226347956391, -0.3203740156405044948, 0.1574803149606297803 ) ) ;
#26327 = CARTESIAN_POINT ( 'NONE',  ( -1.054774247047244096, 0.000000000000000000, 1.872539370024976391 ) ) ;
#26328 = CARTESIAN_POINT ( 'NONE',  ( -0.6971942568897626646, -0.07405724077823297447, 0.4822834645131655606 ) ) ;
#26329 = CARTESIAN_POINT ( 'NONE',  ( -1.033464566929134687, -0.06523048226347956391, 0.6766732283464570452 ) ) ;
#26330 = CARTESIAN_POINT ( 'NONE',  ( 0.7185039370078746268, 0.06523048226347956391, 0.4109251967428667052 ) ) ;
#26331 = FACE_BOUND ( 'NONE', #33025, .T. ) ;
#26332 = CARTESIAN_POINT ( 'NONE',  ( -1.033464566929133799, 0.000000000000000000, 1.978346456692913646 ) ) ;
#26333 = CARTESIAN_POINT ( 'NONE',  ( -0.2984108399384686749, 0.08463831125274406952, -0.7312429817199896931 ) ) ;
#26334 = CARTESIAN_POINT ( 'NONE',  ( -0.1787899950787401604, -0.6093759367331758048, -0.07405724077823318263 ) ) ;
#26335 = CARTESIAN_POINT ( 'NONE',  ( -0.06320621770493051184, -0.08956000428219212939, 0.2147707455372145635 ) ) ;
#26336 = CYLINDRICAL_SURFACE ( 'NONE', #22607, 0.1574803149606299191 ) ;
#26337 = CARTESIAN_POINT ( 'NONE',  ( -0.9873396505805591694, -0.1113553986120547346, 1.176181102254677313 ) ) ;
#26338 = CARTESIAN_POINT ( 'NONE',  ( -0.9500414927467378812, 0.1787899950787401604, 0.2657480314422993595 ) ) ;
#26339 = CARTESIAN_POINT ( 'NONE',  ( 0.1787899950787401604, -1.770793259567822853, 0.07405724077823318263 ) ) ;
#26340 = ORIENTED_EDGE ( 'NONE', *, *, #8755, .T. ) ;
#26341 = CARTESIAN_POINT ( 'NONE',  ( 0.2471911544649836034, -0.08539615244825589369, 0.06152421978428734145 ) ) ;
#26342 = CARTESIAN_POINT ( 'NONE',  ( -0.7495606340400177148, -0.1264236179284866091, 1.547736220418677089 ) ) ;
#26343 = EDGE_LOOP ( 'NONE', ( #3173, #26367, #29498, #27969 ) ) ;
#26344 = CARTESIAN_POINT ( 'NONE',  ( -0.1787899950787401882, -1.343996062938362268, 0.000000000000000000 ) ) ;
#26345 = CARTESIAN_POINT ( 'NONE',  ( 3.284318927891251994E-17, -1.604822834591905556, 0.1787899950787401882 ) ) ;
#26346 = DIRECTION ( 'NONE',  ( 0.000000000000000000, 0.000000000000000000, -1.000000000000000000 ) ) ;
#26347 = ( NAMED_UNIT ( * ) PLANE_ANGLE_UNIT ( ) SI_UNIT ( $, .RADIAN. ) ) ;
#26348 = CARTESIAN_POINT ( 'NONE',  ( 0.9412147342319837628, -0.1574803149606297803, 0.4355314960629916299 ) ) ;
#26349 = DIRECTION ( 'NONE',  ( 0.000000000000000000, 0.000000000000000000, 1.000000000000000000 ) ) ;
#26350 = CARTESIAN_POINT ( 'NONE',  ( -0.7646288533564489232, -0.1113553986120547346, 1.126968503829480328 ) ) ;
#26351 = CARTESIAN_POINT ( 'NONE',  ( 1.054774247047244540, -0.07405724077823318263, 0.4970472440407249226 ) ) ;
#26352 = DIRECTION ( 'NONE',  ( 1.000000000000000000, -0.000000000000000000, -0.000000000000000000 ) ) ;
#26353 = CARTESIAN_POINT ( 'NONE',  ( -0.1574803149606297803, -0.3006889763779526104, 0.06523048226347956391 ) ) ;
#26354 = CARTESIAN_POINT ( 'NONE',  ( 0.9873396505805591694, 0.1113553986120547346, 1.973425196742866206 ) ) ;
#26355 = ORIENTED_EDGE ( 'NONE', *, *, #43327, .F. ) ;
#26356 = AXIS2_PLACEMENT_3D ( 'NONE', #3101, #2852, #10802 ) ;
#26357 = DIRECTION ( 'NONE',  ( -3.469446951953616950E-15, -0.7880107536067223473, 0.6156614753256577366 ) ) ;
#26358 = CARTESIAN_POINT ( 'NONE',  ( -0.8759842519685039353, 0.1787899950787401882, 1.021161417269070837 ) ) ;
#26359 = CARTESIAN_POINT ( 'NONE',  ( 0.7646288533564489232, -0.1113553986120547346, 1.018700787401574770 ) ) ;
#26360 = FACE_OUTER_BOUND ( 'NONE', #38562, .T. ) ;
#26361 = CARTESIAN_POINT ( 'NONE',  ( -0.7646288533564489232, -0.1113553986120547346, 0.8218503937007874960 ) ) ;
#26362 = CARTESIAN_POINT ( 'NONE',  ( -0.1560601414942001663, -0.08956156883362471899, 0.05573596787081475795 ) ) ;
#26363 = ORIENTED_EDGE ( 'NONE', *, *, #30093, .F. ) ;
#26364 = CARTESIAN_POINT ( 'NONE',  ( 0.1563808587774279391, -0.02736954274996897599, -0.1403846824214370070 ) ) ;
#26365 = ORIENTED_EDGE ( 'NONE', *, *, #18015, .F. ) ;
#26366 = EDGE_CURVE ( 'NONE', #8447, #30077, #8703, .T. ) ;
#26367 = ORIENTED_EDGE ( 'NONE', *, *, #29660, .F. ) ;
#26368 = DIRECTION ( 'NONE',  ( 1.822029033848725028E-16, 0.000000000000000000, 1.000000000000000000 ) ) ;
#26369 = CARTESIAN_POINT ( 'NONE',  ( 0.9412147342319837628, 0.1574803149606300301, 1.149114173120819427 ) ) ;
#26370 = CARTESIAN_POINT ( 'NONE',  ( 0.1787899950787401882, -1.516240157426551161, -2.189545951927503898E-17 ) ) ;
#26371 = CARTESIAN_POINT ( 'NONE',  ( 3.284318927891251994E-17, -0.9010826771115905132, 0.1787899950787401882 ) ) ;
#26372 = CARTESIAN_POINT ( 'NONE',  ( 0.06523048226347956391, -1.156988188976378229, 0.1574803149606297803 ) ) ;
#26373 = CARTESIAN_POINT ( 'NONE',  ( 0.9412147342319837628, -0.1574803149606297803, 1.173720472333417586 ) ) ;
#26374 = EDGE_CURVE ( 'NONE', #14529, #28682, #38172, .T. ) ;
#26375 = CARTESIAN_POINT ( 'NONE',  ( 0.9873396505805591694, 0.1113553986120547346, 1.825787401574803237 ) ) ;
#26376 = UNCERTAINTY_MEASURE_WITH_UNIT (LENGTH_MEASURE( 1.000000000000000082E-05 ), #21793, 'distance_accuracy_value', 'NONE') ;
#26377 = ORIENTED_EDGE ( 'NONE', *, *, #39739, .F. ) ;
#26378 = CARTESIAN_POINT ( 'NONE',  ( -0.6971942568897637749, 2.189545951927499583E-17, 1.700295275536787498 ) ) ;
#26379 = EDGE_CURVE ( 'NONE', #13566, #2118, #39360, .T. ) ;
#26380 = CARTESIAN_POINT ( 'NONE',  ( 1.054774247047244540, 0.07405724077823318263, 1.643700787347811998 ) ) ;
#26381 = CARTESIAN_POINT ( 'NONE',  ( 1.033464566929133799, 0.000000000000000000, 0.1673228346456692994 ) ) ;
#26382 = CARTESIAN_POINT ( 'NONE',  ( 0.8019270111902717657, -0.1787899950787401604, 0.2509842519147403861 ) ) ;
#26383 = EDGE_CURVE ( 'NONE', #36909, #11736, #44722, .T. ) ;
#26384 = CARTESIAN_POINT ( 'NONE',  ( -0.6971942568897648851, -0.07405724077823297447, 1.186023621993481658 ) ) ;
#26385 = CARTESIAN_POINT ( 'NONE',  ( -0.6971942568897626646, 0.07405724077823318263, 0.9448818897100165204 ) ) ;
#26386 = CARTESIAN_POINT ( 'NONE',  ( -0.7495606340400177148, 0.1264236179284866091, 0.08120078734781142893 ) ) ;
#26387 = DIRECTION ( 'NONE',  ( 1.000000000000000000, 0.000000000000000000, -1.822029033848725275E-16 ) ) ;
#26388 = CARTESIAN_POINT ( 'NONE',  ( -0.8019270111902717657, -0.1787899950787401604, 1.550196850339937926 ) ) ;
#26389 = CARTESIAN_POINT ( 'NONE',  ( -1.033464566929134687, 0.06523048226347956391, 1.813484251860976393 ) ) ;
#26390 = ORIENTED_EDGE ( 'NONE', *, *, #2264, .T. ) ;
#26391 = CARTESIAN_POINT ( 'NONE',  ( -0.9873396505805591694, 0.1113553986120547346, 1.668307086614173373 ) ) ;
#26392 = CARTESIAN_POINT ( 'NONE',  ( 0.4151545546392377273, -0.09842519685039370636, 1.205361022782828805E-17 ) ) ;
#26393 = CARTESIAN_POINT ( 'NONE',  ( 0.8759842519685039353, -0.1787899950787401882, 1.631397637741511808 ) ) ;
#26394 = CARTESIAN_POINT ( 'NONE',  ( -0.04623149810832708623, -0.09851382820108051108, 0.1526845614456639744 ) ) ;
#26395 = DIRECTION ( 'NONE',  ( 0.000000000000000000, 0.000000000000000000, -1.000000000000000000 ) ) ;
#26396 = CARTESIAN_POINT ( 'NONE',  ( -0.2559118981538488491, 0.03129849267415509700, -0.3138669400184891378 ) ) ;
#26397 = VERTEX_POINT ( 'NONE', #30785 ) ;
#26398 = AXIS2_PLACEMENT_3D ( 'NONE', #32773, #33007, #26518 ) ;
#26399 = ORIENTED_EDGE ( 'NONE', *, *, #18356, .T. ) ;
#26400 = AXIS2_PLACEMENT_3D ( 'NONE', #1473, #41952, #9159 ) ;
#26401 = AXIS2_PLACEMENT_3D ( 'NONE', #12800, #32614, #29030 ) ;
#26402 = CARTESIAN_POINT ( 'NONE',  ( 0.07405724077823318263, -0.8444881889226140137, -0.1787899950787401604 ) ) ;
#26403 = CARTESIAN_POINT ( 'NONE',  ( 0.1787899950787401604, -1.041338582623402287, -0.07405724077823318263 ) ) ;
#26404 = ORIENTED_EDGE ( 'NONE', *, *, #10481, .T. ) ;
#26405 = CARTESIAN_POINT ( 'NONE',  ( -1.033464566929133799, 0.000000000000000000, 0.07874015737278799998 ) ) ;
#26406 = CARTESIAN_POINT ( 'NONE',  ( 0.07444174185955046430, -0.2889217623389510603, -0.1797182628040039087 ) ) ;
#26407 = CARTESIAN_POINT ( 'NONE',  ( 0.06523048226347956391, 0.1176181102362205133, -0.1574803149606300301 ) ) ;
#26408 = CARTESIAN_POINT ( 'NONE',  ( -0.1787899950787401604, -0.04724409443442544737, -0.07405724077823318263 ) ) ;
#26409 = LINE ( 'NONE', #4552, #40617 ) ;
#26410 = CARTESIAN_POINT ( 'NONE',  ( 0.8019270111902717657, -0.1787899950787401604, 0.7578740156942689321 ) ) ;
#26411 = ( BOUNDED_CURVE ( )  B_SPLINE_CURVE ( 2, ( #36201, #14619, #46962, #211, #32853, #29521, #14861, #35948, #14150 ),
 .UNSPECIFIED., .F., .T. ) 
 B_SPLINE_CURVE_WITH_KNOTS ( ( 3, 2, 2, 2, 3 ),
 ( 0.01499999999999999944, 0.01750000000000000167, 0.02000000000000000042, 0.02249999999999999917, 0.02500000000000000139 ),
 .UNSPECIFIED. ) 
 CURVE ( )  GEOMETRIC_REPRESENTATION_ITEM ( )  RATIONAL_B_SPLINE_CURVE ( ( 1.000000000000000000, 0.9238795325112869605, 1.000000000000000000, 0.9238795325112869605, 1.000000000000000000, 0.9238795325112869605, 1.000000000000000000, 0.9238795325112869605, 1.000000000000000000 ) ) 
 REPRESENTATION_ITEM ( '' )  ) ;
#26412 = FILL_AREA_STYLE ('',( #26171 ) ) ;
#26413 = CARTESIAN_POINT ( 'NONE',  ( 0.000000000000000000, 0.09842519685039370636, 0.000000000000000000 ) ) ;
#26414 = LINE ( 'NONE', #496, #36132 ) ;
#26415 = CARTESIAN_POINT ( 'NONE',  ( 1.054774247047244096, 0.000000000000000000, 1.877460629867496067 ) ) ;
#26416 = ORIENTED_EDGE ( 'NONE', *, *, #18459, .F. ) ;
#26417 = CARTESIAN_POINT ( 'NONE',  ( 0.8107537697050253289, 0.1574803149606300301, 0.1402559055118110520 ) ) ;
#26418 = LINE ( 'NONE', #41691, #8378 ) ;
#26420 = CARTESIAN_POINT ( 'NONE',  ( -0.1264236179284866091, -0.1973425196312759700, 0.1264236179284866091 ) ) ;
#26419 = CARTESIAN_POINT ( 'NONE',  ( 0.1113553986120547346, -0.9478346455617638888, 0.1113553986120547346 ) ) ;
#26421 = CARTESIAN_POINT ( 'NONE',  ( -1.033464566929133799, 0.000000000000000000, 0.5511811022546772021 ) ) ;
#26422 = CARTESIAN_POINT ( 'NONE',  ( -0.1787899950787401604, -1.262795275536788386, -0.07405724077823318263 ) ) ;
#26423 = CARTESIAN_POINT ( 'NONE',  ( 1.002407869896990045, 0.1264236179284866091, 0.2682086613635594752 ) ) ;
#26424 = ADVANCED_FACE ( 'NONE', ( #27190 ), #19489, .T. ) ;
#26425 = CARTESIAN_POINT ( 'NONE',  ( -0.8070866141732283561, 0.000000000000000000, 0.7574803149606299524 ) ) ;
#26426 = CARTESIAN_POINT ( 'NONE',  ( -1.002407869896990045, 0.1264236179284866091, 1.680610236166708793 ) ) ;
#26427 = VERTEX_POINT ( 'NONE', #26708 ) ;
#26428 = CIRCLE ( 'NONE', #44748, 0.08090551181102362266 ) ;
#26429 = CARTESIAN_POINT ( 'NONE',  ( -1.002407869896990045, 0.1264236179284866091, 1.291830708607653477 ) ) ;
#26430 = CARTESIAN_POINT ( 'NONE',  ( 0.7185039370078739607, 1.928577636452523993E-17, 1.013779527559055094 ) ) ;
#26431 = TOROIDAL_SURFACE ( 'NONE', #21026, 0.2007874015748031815, 0.01968503937007873988 ) ;
#26432 = CARTESIAN_POINT ( 'NONE',  ( -0.9500414927467378812, -0.1787899950787401604, 0.4921259841982048577 ) ) ;
#26433 = CARTESIAN_POINT ( 'NONE',  ( 1.002407869896990045, -0.1264236179284866091, 1.906988188922614125 ) ) ;
#26434 = CARTESIAN_POINT ( 'NONE',  ( -0.8019270111902717657, 0.1787899950787401604, 1.058070866087969186 ) ) ;
#26435 = ADVANCED_FACE ( 'NONE', ( #15444 ), #40800, .F. ) ;
#26436 = CARTESIAN_POINT ( 'NONE',  ( -0.1192973132712141088, -0.09842522298280542703, -0.1331694143430761090 ) ) ;
#26437 = DIRECTION ( 'NONE',  ( 1.000000000000000000, 0.000000000000000000, -1.822029033848725275E-16 ) ) ;
#26438 = CARTESIAN_POINT ( 'NONE',  ( 0.6971942568897637749, 2.189545951927499583E-17, 0.4404527558517480901 ) ) ;
#26439 = CARTESIAN_POINT ( 'NONE',  ( -0.7495606340400177148, -0.1264236179284866091, 0.4404527558517480901 ) ) ;
#26440 = VERTEX_POINT ( 'NONE', #33669 ) ;
#26441 = CARTESIAN_POINT ( 'NONE',  ( -0.1787899950787401604, -0.08661417317458304510, -0.07405724077823318263 ) ) ;
#26442 = CARTESIAN_POINT ( 'NONE',  ( -0.8107537697050253289, 0.1574803149606300301, 0.1796259842519684069 ) ) ;
#26443 = CARTESIAN_POINT ( 'NONE',  ( 0.8019270111902716547, -0.1787899950787401604, 1.195866141678520345 ) ) ;
#26444 = CARTESIAN_POINT ( 'NONE',  ( -0.2006330517481570708, -0.09851385263128563385, -0.1463975219237275693 ) ) ;
#26445 = ORIENTED_EDGE ( 'NONE', *, *, #1198, .T. ) ;
#26446 = CARTESIAN_POINT ( 'NONE',  ( -0.8107537697050254399, -0.1574803149606297803, 1.296751968503936592 ) ) ;
#26447 = DIRECTION ( 'NONE',  ( -1.000000000000000000, 0.000000000000000000, 0.000000000000000000 ) ) ;
#26448 = CARTESIAN_POINT ( 'NONE',  ( -0.9412147342319837628, -0.1574803149606297803, 0.1993110236220472509 ) ) ;
#26449 = CARTESIAN_POINT ( 'NONE',  ( 0.1787899950787401882, -1.453371999725301178, -2.189545951927503898E-17 ) ) ;
#26450 = ORIENTED_EDGE ( 'NONE', *, *, #6617, .F. ) ;
#26451 = DIRECTION ( 'NONE',  ( -0.000000000000000000, 1.000000000000000000, 0.000000000000000000 ) ) ;
#26452 = CARTESIAN_POINT ( 'NONE',  ( -0.1787899950787401604, -0.4753937007336378473, -0.07405724077823318263 ) ) ;
#26453 = CARTESIAN_POINT ( 'NONE',  ( -1.033464566929134687, 0.06523048226347956391, 1.695374015640504828 ) ) ;
#26454 = VERTEX_POINT ( 'NONE', #5100 ) ;
#26455 = CARTESIAN_POINT ( 'NONE',  ( 0.8759842519685039353, -0.1787899950787401882, 1.311515747977732405 ) ) ;
#26456 = AXIS2_PLACEMENT_3D ( 'NONE', #29986, #29749, #11500 ) ;
#26457 = CARTESIAN_POINT ( 'NONE',  ( 0.7646288533564489232, 0.1113553986120547346, 1.599409448818897683 ) ) ;
#26458 = EDGE_CURVE ( 'NONE', #7920, #28768, #30256, .T. ) ;
#26459 = DIRECTION ( 'NONE',  ( 0.000000000000000000, 0.000000000000000000, 1.000000000000000000 ) ) ;
#26460 = CARTESIAN_POINT ( 'NONE',  ( -0.1264236179284866091, -0.2465551180564728440, -0.1264236179284866091 ) ) ;
#26461 = CARTESIAN_POINT ( 'NONE',  ( 0.4330708661417322913, 0.000000000000000000, -1.186023622047243986 ) ) ;
#26462 = CARTESIAN_POINT ( 'NONE',  ( 0.7495606340400177148, 0.1264236179284866091, 1.532972440891118060 ) ) ;
#26463 = AXIS2_PLACEMENT_3D ( 'NONE', #9056, #13371, #38526 ) ;
#26464 = AXIS2_PLACEMENT_3D ( 'NONE', #37987, #5145, #19768 ) ;
#26465 = CARTESIAN_POINT ( 'NONE',  ( 0.07405724077823318263, 0.1288130396447769721, -0.1787899950787401604 ) ) ;
#26466 = CARTESIAN_POINT ( 'NONE',  ( -0.1787899950787401604, -1.730314960576156968, 0.07405724077823318263 ) ) ;
#26467 = DIRECTION ( 'NONE',  ( -1.000000000000000000, 3.469446951953614189E-15, 0.000000000000000000 ) ) ;
#26468 = CARTESIAN_POINT ( 'NONE',  ( -1.054774247047244540, -0.07405724077823318263, 0.6938976377415124741 ) ) ;
#26470 = CARTESIAN_POINT ( 'NONE',  ( 1.033464566929134687, -0.06523048226347956391, 0.3124999998924728462 ) ) ;
#26469 = CARTESIAN_POINT ( 'NONE',  ( 0.1574803149606300301, -0.7140748031496056969, -0.06523048226347956391 ) ) ;
#26471 = CARTESIAN_POINT ( 'NONE',  ( -0.07444174185955065859, -1.465102864701155916, -0.1797182628040039087 ) ) ;
#26472 = CARTESIAN_POINT ( 'NONE',  ( -0.1113553986120547346, -0.05216535422318158144, 0.1113553986120547346 ) ) ;
#26473 = CARTESIAN_POINT ( 'NONE',  ( 0.5555748031496114958, 1.061695335278752150, -0.02376411959061622975 ) ) ;
#26474 = CARTESIAN_POINT ( 'NONE',  ( 1.054774247047244540, 0.07405724077823318263, 1.874999999946236784 ) ) ;
#26475 = CARTESIAN_POINT ( 'NONE',  ( 0.7185039370078739607, 1.928577636452523993E-17, 0.1476377952755905387 ) ) ;
#26476 = CARTESIAN_POINT ( 'NONE',  ( -0.1296641775163210608, 0.9382165298418947419, -1.070508272602715083 ) ) ;
#26477 = FACE_OUTER_BOUND ( 'NONE', #20848, .T. ) ;
#26479 = CARTESIAN_POINT ( 'NONE',  ( -0.9412147342319837628, -0.1574803149606297803, 1.026082677165353729 ) ) ;
#26478 = CARTESIAN_POINT ( 'NONE',  ( 0.06523048226347956391, -0.8174212597349923559, -0.1574803149606300301 ) ) ;
#26480 = CARTESIAN_POINT ( 'NONE',  ( -0.7185039370078739607, 1.928577636452523993E-17, 0.2165354329633393804 ) ) ;
#26481 = CARTESIAN_POINT ( 'NONE',  ( 0.6971942568897626646, 0.07405724077823318263, 0.3149606298674962890 ) ) ;
#26482 = ADVANCED_FACE ( 'NONE', ( #1267 ), #19724, .T. ) ;
#26483 = FACE_OUTER_BOUND ( 'NONE', #33883, .T. ) ;
#26484 = DIRECTION ( 'NONE',  ( -1.000000000000000000, 0.000000000000000000, 0.000000000000000000 ) ) ;
#26485 = CARTESIAN_POINT ( 'NONE',  ( 1.033464566929134687, 0.06523048226347956391, 0.5930118109160945616 ) ) ;
#26486 = ORIENTED_EDGE ( 'NONE', *, *, #405, .T. ) ;
#26487 = CARTESIAN_POINT ( 'NONE',  ( -0.7495606340400177148, -0.1264236179284866091, 1.075295275536787276 ) ) ;
#26488 = CARTESIAN_POINT ( 'NONE',  ( 1.033464566929133799, 0.000000000000000000, 1.387795275590551158 ) ) ;
#26489 = CARTESIAN_POINT ( 'NONE',  ( 0.7646288533564489232, 0.1113553986120547346, 0.6938976377952755792 ) ) ;
#26490 = ORIENTED_EDGE ( 'NONE', *, *, #27645, .F. ) ;
#26491 = CARTESIAN_POINT ( 'NONE',  ( -0.1270800023317771588, -0.08468947887438406374, -0.1270800023317771588 ) ) ;
#26492 = CARTESIAN_POINT ( 'NONE',  ( 3.284318927891251994E-17, -1.216043307032850462, 0.1787899950787401882 ) ) ;
#26493 = CARTESIAN_POINT ( 'NONE',  ( 0.6195511811023624027, 0.9842519685039365918, -0.7135826771653542844 ) ) ;
#26494 = CARTESIAN_POINT ( 'NONE',  ( 1.002407869896990045, -0.1264236179284866091, 1.592027559001354398 ) ) ;
#26495 = CARTESIAN_POINT ( 'NONE',  ( -0.7646288533564489232, 0.1113553986120547346, 1.205708661417322913 ) ) ;
#26496 = CIRCLE ( 'NONE', #45562, 0.009842519685039382085 ) ;
#26497 = EDGE_CURVE ( 'NONE', #33652, #33104, #44019, .T. ) ;
#26498 = FACE_OUTER_BOUND ( 'NONE', #6123, .T. ) ;
#26500 = CARTESIAN_POINT ( 'NONE',  ( 1.033464566929133799, 1.928577636452524610E-17, 4.498031496062991685 ) ) ;
#26499 = CARTESIAN_POINT ( 'NONE',  ( -0.1574803149606299191, 0.05118110236220472370, 0.000000000000000000 ) ) ;
#26501 = CARTESIAN_POINT ( 'NONE',  ( -1.033464566929133799, 0.000000000000000000, 0.5118110235145196807 ) ) ;
#26502 = UNCERTAINTY_MEASURE_WITH_UNIT (LENGTH_MEASURE( 1.000000000000000082E-05 ), #15376, 'distance_accuracy_value', 'NONE') ;
#26503 = CARTESIAN_POINT ( 'NONE',  ( -0.07405724077823318263, -0.1899606298674962612, 0.1787899950787401604 ) ) ;
#26504 = VERTEX_POINT ( 'NONE', #34361 ) ;
#26505 = DIRECTION ( 'NONE',  ( 1.000000000000000000, 0.000000000000000000, -1.822029033848725275E-16 ) ) ;
#26506 = CARTESIAN_POINT ( 'NONE',  ( -1.002407869896990045, 0.1264236179284866091, 1.562499999946236118 ) ) ;
#26507 = CARTESIAN_POINT ( 'NONE',  ( 0.1574803149606300301, -0.1186023620971974196, 0.06523048226347956391 ) ) ;
#26508 = VECTOR ( 'NONE', #17415, 39.37007874015748143 ) ;
#26509 = ORIENTED_EDGE ( 'NONE', *, *, #21586, .T. ) ;
#26510 = CARTESIAN_POINT ( 'NONE',  ( -0.7495606340400177148, 0.1264236179284866091, 0.2780511810485988278 ) ) ;
#26511 = DIRECTION ( 'NONE',  ( 0.000000000000000000, 0.000000000000000000, -1.000000000000000000 ) ) ;
#26512 = CARTESIAN_POINT ( 'NONE',  ( -0.7646288533564489232, -0.1113553986120547346, 1.874999999892472458 ) ) ;
#26513 = CARTESIAN_POINT ( 'NONE',  ( -0.07405724077823318263, -0.9538641257095545889, 0.1787899950787401604 ) ) ;
#26514 = ORIENTED_EDGE ( 'NONE', *, *, #42513, .T. ) ;
#26515 = CARTESIAN_POINT ( 'NONE',  ( -1.094772975963752103E-17, 0.06840551186478720236, -0.1787899950787401882 ) ) ;
#26516 = ORIENTED_EDGE ( 'NONE', *, *, #25159, .T. ) ;
#26517 = VERTEX_POINT ( 'NONE', #782 ) ;
#26518 = DIRECTION ( 'NONE',  ( 1.000000000000000000, 0.000000000000000000, 0.000000000000000000 ) ) ;
#26519 = CARTESIAN_POINT ( 'NONE',  ( 1.033464566929133799, 1.928577636452524610E-17, 4.498031496062992574 ) ) ;
#26520 = CARTESIAN_POINT ( 'NONE',  ( 0.3906197235759846786, -3.032960542342102697E-32, 0.09842519685039370636 ) ) ;
#26521 = CARTESIAN_POINT ( 'NONE',  ( 0.7185039370078739607, 1.928577636452523993E-17, 1.437007873908220601 ) ) ;
#26522 = AXIS2_PLACEMENT_3D ( 'NONE', #8491, #11639, #44900 ) ;
#26523 = CARTESIAN_POINT ( 'NONE',  ( -0.8019270111902716547, -0.1787899950787401604, 0.1722440944344256208 ) ) ;
#26524 = CARTESIAN_POINT ( 'NONE',  ( -0.8759842519685039353, 0.1574803149606299191, 0.9645669291338583307 ) ) ;
#26525 = CARTESIAN_POINT ( 'NONE',  ( -0.7185039370078739607, 0.000000000000000000, -2.869337061179095023E-17 ) ) ;
#26526 = DIRECTION ( 'NONE',  ( 0.000000000000000000, 1.000000000000000000, 0.000000000000000000 ) ) ;
#26527 = CARTESIAN_POINT ( 'NONE',  ( 0.1270800023317771588, -1.078783967063360327, -0.1270800023317771588 ) ) ;
#26528 = CARTESIAN_POINT ( 'NONE',  ( 0.1372385047410485115, 0.1299212598425196485, -0.09687705708535346294 ) ) ;
#26529 = CARTESIAN_POINT ( 'NONE',  ( -0.9412147342319837628, 0.1574803149606300301, 1.464074803042079598 ) ) ;
#26530 = ADVANCED_FACE ( 'NONE', ( #41034 ), #8228, .T. ) ;
#26531 = CARTESIAN_POINT ( 'NONE',  ( 1.002407869896990045, -0.1264236179284866091, 0.9670275590013542866 ) ) ;
#26532 = CARTESIAN_POINT ( 'NONE',  ( 0.7185039370078739607, 1.928577636452523993E-17, 0.5314960628845992741 ) ) ;
#26533 = CARTESIAN_POINT ( 'NONE',  ( 1.033464566929133799, 0.000000000000000000, 1.427165354330708569 ) ) ;
#26535 = CARTESIAN_POINT ( 'NONE',  ( 0.1321676148590689159, 0.1299212598425196763, -0.1026092226670043267 ) ) ;
#26534 = CARTESIAN_POINT ( 'NONE',  ( 0.7101297187648138998, 0.003597347259315822592, 1.983202747004803257 ) ) ;
#26536 = CARTESIAN_POINT ( 'NONE',  ( 0.1502414035307333140, -0.4075443641102559078, -0.9311509272141711424 ) ) ;
#26537 = CARTESIAN_POINT ( 'NONE',  ( 1.033464566929134687, -0.06523048226347956391, 0.7947834645669290543 ) ) ;
#26538 = EDGE_CURVE ( 'NONE', #14442, #36086, #11298, .T. ) ;
#26540 = FACE_OUTER_BOUND ( 'NONE', #7375, .T. ) ;
#26539 = CARTESIAN_POINT ( 'NONE',  ( 1.054774247047244096, 0.000000000000000000, 0.7701771653005669016 ) ) ;
#26541 = CARTESIAN_POINT ( 'NONE',  ( 0.6971942568897648851, 0.07405724077823318263, 1.815944881835999780 ) ) ;
#26542 = CARTESIAN_POINT ( 'NONE',  ( -0.1787899950787401604, -0.7854330708123791194, 0.07405724077823318263 ) ) ;
#26543 = DIRECTION ( 'NONE',  ( 0.8191520442889861364, 0.000000000000000000, 0.5735764363510541530 ) ) ;
#26544 = ORIENTED_EDGE ( 'NONE', *, *, #11655, .F. ) ;
#26545 = CARTESIAN_POINT ( 'NONE',  ( -0.9412147342319837628, 0.1574803149606300301, 0.8439960629921254842 ) ) ;
#26546 = DIRECTION ( 'NONE',  ( 0.000000000000000000, -0.6156614753256598460, -0.7880107536067206819 ) ) ;
#26547 = CARTESIAN_POINT ( 'NONE',  ( -0.7185039370078746268, 0.06523048226347956391, 0.1353346455617644717 ) ) ;
#26548 = CARTESIAN_POINT ( 'NONE',  ( 1.002407869896990045, -0.1264236179284866091, 1.158956692859621995 ) ) ;
#26549 = ADVANCED_FACE ( 'NONE', ( #13898 ), #39747, .T. ) ;
#26550 = CARTESIAN_POINT ( 'NONE',  ( -0.8759842519685039353, 0.1574803149606299191, 1.043307086614173151 ) ) ;
#26551 = CARTESIAN_POINT ( 'NONE',  ( -9.642888182262618425E-18, -1.730314960629921517, -0.1574803149606299191 ) ) ;
#26552 = CARTESIAN_POINT ( 'NONE',  ( 1.033464566929134687, 0.06523048226347956391, 1.301673228238930502 ) ) ;
#26553 = CARTESIAN_POINT ( 'NONE',  ( 1.350095158311321523E-16, -0.3937007874015746034, 0.2952755905511816326 ) ) ;
#26554 = EDGE_CURVE ( 'NONE', #3517, #37608, #30628, .T. ) ;
#26555 = CARTESIAN_POINT ( 'NONE',  ( -0.6971942568897637749, 2.189545951927499583E-17, 0.5142716534895434011 ) ) ;
#26556 = ORIENTED_EDGE ( 'NONE', *, *, #37009, .F. ) ;
#26557 = FACE_OUTER_BOUND ( 'NONE', #25075, .T. ) ;
#26558 = CARTESIAN_POINT ( 'NONE',  ( -1.002407869896990045, 0.1264236179284866091, 0.3026574802611972648 ) ) ;
#26559 = ORIENTED_EDGE ( 'NONE', *, *, #18600, .T. ) ;
#26560 = CARTESIAN_POINT ( 'NONE',  ( 0.1264236179284866091, -1.555610236166708571, -0.1264236179284866091 ) ) ;
#26561 = B_SPLINE_CURVE_WITH_KNOTS ( 'NONE', 3,
 ( #2599, #21048, #14115, #36403, #17232, #17929, #10288, #32815, #46448, #24897, #24425, #14581, #3561, #39026, #13630, #43328, #42832, #35910, #6194, #32584 ),
 .UNSPECIFIED., .F., .F.,
 ( 4, 1, 1, 1, 1, 1, 2, 2, 1, 1, 1, 2, 2, 4 ),
 ( 0.000000000000000000, 0.2499999999999993894, 0.3749999999999990008, 0.4374999999999987788, 0.4687499999999986122, 0.4843749999999986122, 0.4921874999999985012, 0.4999999999999984457, 0.6249999999999980016, 0.6874999999999978906, 0.7187499999999977796, 0.7343749999999978906, 0.7499999999999980016, 1.000000000000000000 ),
 .UNSPECIFIED. ) ;
#26562 = CARTESIAN_POINT ( 'NONE',  ( -0.6971942568897637749, 2.189545951927499583E-17, 1.774114173174582643 ) ) ;
#26563 = CARTESIAN_POINT ( 'NONE',  ( -0.6971942568897648851, -0.07405724077823297447, 0.8316929133320636325 ) ) ;
#26564 = CARTESIAN_POINT ( 'NONE',  ( -0.7495606340400177148, 0.1264236179284866091, 0.5142716534895434011 ) ) ;
#26565 = DIRECTION ( 'NONE',  ( 0.000000000000000000, 0.000000000000000000, 1.000000000000000000 ) ) ;
#26566 = CARTESIAN_POINT ( 'NONE',  ( -0.1502419002556872329, -0.4075443641102559633, -0.9311509272141712534 ) ) ;
#26567 = CARTESIAN_POINT ( 'NONE',  ( -0.9873396505805591694, 0.1113553986120547346, 0.3198818896562523606 ) ) ;
#26568 = LINE ( 'NONE', #26799, #44286 ) ;
#26569 = CARTESIAN_POINT ( 'NONE',  ( -0.1787899950787401604, -0.4912657005127034071, -0.07405724077823318263 ) ) ;
#26570 = CARTESIAN_POINT ( 'NONE',  ( 0.05749879812895779263, -0.08956009822529961695, 0.2100333487722925163 ) ) ;
#26571 = FACE_OUTER_BOUND ( 'NONE', #30446, .T. ) ;
#26572 = CARTESIAN_POINT ( 'NONE',  ( 0.7646288533564489232, -0.1113553986120547346, 1.924212598425196985 ) ) ;
#26573 = LINE ( 'NONE', #37320, #5782 ) ;
#26574 = CARTESIAN_POINT ( 'NONE',  ( -0.6971942568897637749, 2.189545951927499583E-17, 0.2780511810485988278 ) ) ;
#26575 = CARTESIAN_POINT ( 'NONE',  ( 0.1787899950787401604, -1.805242078465460809, -0.07405724077823318263 ) ) ;
#26576 = VERTEX_POINT ( 'NONE', #21558 ) ;
#26577 = DIRECTION ( 'NONE',  ( 0.000000000000000000, -0.6156614753256598460, -0.7880107536067206819 ) ) ;
#26578 = ORIENTED_EDGE ( 'NONE', *, *, #264, .F. ) ;
#26579 = CARTESIAN_POINT ( 'NONE',  ( -0.8019270111902716547, 0.1787899950787401604, 1.496062992072220599 ) ) ;
#26580 = VERTEX_POINT ( 'NONE', #32375 ) ;
#26581 = CARTESIAN_POINT ( 'NONE',  ( -0.1787899950787401882, -1.265255905458047225, 0.000000000000000000 ) ) ;
#26582 = CARTESIAN_POINT ( 'NONE',  ( -1.094772975963752103E-17, -1.545767716481669218, -0.1787899950787401882 ) ) ;
#26583 = AXIS2_PLACEMENT_3D ( 'NONE', #5238, #45480, #20099 ) ;
#26584 = ( BOUNDED_CURVE ( )  B_SPLINE_CURVE ( 2, ( #599, #33482, #29900, #1315, #22183, #40846, #11196, #37270, #33248 ),
 .UNSPECIFIED., .F., .F. ) 
 B_SPLINE_CURVE_WITH_KNOTS ( ( 3, 2, 2, 2, 3 ),
 ( 0.5899999999999999689, 0.5925000000000000266, 0.5949999999999999734, 0.5975000000000000311, 0.5999999999999999778 ),
 .UNSPECIFIED. ) 
 CURVE ( )  GEOMETRIC_REPRESENTATION_ITEM ( )  RATIONAL_B_SPLINE_CURVE ( ( 1.000000000000000000, 0.9238795325112869605, 1.000000000000000000, 0.9238795325112869605, 1.000000000000000000, 0.9238795325112869605, 1.000000000000000000, 0.9238795325112869605, 1.000000000000000000 ) ) 
 REPRESENTATION_ITEM ( '' )  ) ;
#26585 = DIRECTION ( 'NONE',  ( 0.5735764363510447161, -0.8191520442889925757, 1.003171929053525486E-16 ) ) ;
#26586 = DIRECTION ( 'NONE',  ( -1.000000000000000000, 0.000000000000000000, 0.000000000000000000 ) ) ;
#26587 = CARTESIAN_POINT ( 'NONE',  ( 0.9873396505805591694, 0.1113553986120547346, 0.5265748031496062520 ) ) ;
#26588 = CARTESIAN_POINT ( 'NONE',  ( -0.1377952755905509363, 0.000000000000000000, -0.1436967020037460685 ) ) ;
#26589 = CARTESIAN_POINT ( 'NONE',  ( -0.8759842519685039353, -0.1574803149606299191, 1.013779527451527551 ) ) ;
#26590 = ADVANCED_FACE ( 'NONE', ( #36194 ), #10800, .F. ) ;
#26591 = DIRECTION ( 'NONE',  ( -1.000000000000000000, 0.000000000000000000, 0.000000000000000000 ) ) ;
#26592 = VERTEX_POINT ( 'NONE', #6934 ) ;
#26593 = CARTESIAN_POINT ( 'NONE',  ( 0.9412147342319837628, -0.1574803149606297803, 1.961122047136568014 ) ) ;
#26594 = ORIENTED_EDGE ( 'NONE', *, *, #39799, .F. ) ;
#26595 = CYLINDRICAL_SURFACE ( 'NONE', #19189, 0.1574803149606299191 ) ;
#26596 = CARTESIAN_POINT ( 'NONE',  ( -0.8019270111902716547, 0.1787899950787401604, 1.062992125930488418 ) ) ;
#26597 = CARTESIAN_POINT ( 'NONE',  ( 0.9412147342319837628, 0.1574803149606300301, 0.8833661417322832277 ) ) ;
#26598 = CARTESIAN_POINT ( 'NONE',  ( 1.033464566929134687, 0.06523048226347956391, 1.350885826771654141 ) ) ;
#26599 = FACE_OUTER_BOUND ( 'NONE', #41146, .T. ) ;
#26600 = CARTESIAN_POINT ( 'NONE',  ( -0.1690299954235125468, -0.08956068868289060458, -0.02622682328975086199 ) ) ;
#26601 = VERTEX_POINT ( 'NONE', #6219 ) ;
#26602 = DIRECTION ( 'NONE',  ( 1.822029033848725028E-16, 0.000000000000000000, 1.000000000000000000 ) ) ;
#26603 = DIRECTION ( 'NONE',  ( 0.000000000000000000, -1.000000000000000000, 0.000000000000000000 ) ) ;
#26604 = CARTESIAN_POINT ( 'NONE',  ( 0.9500414927467378812, 0.1787899950787401604, 0.6988188975840318173 ) ) ;
#26605 = ORIENTED_EDGE ( 'NONE', *, *, #16090, .T. ) ;
#26606 = EDGE_CURVE ( 'NONE', #15855, #25548, #27435, .T. ) ;
#26607 = LINE ( 'NONE', #41639, #1309 ) ;
#26608 = CARTESIAN_POINT ( 'NONE',  ( -0.1787899950787401604, -1.617125984198204414, -0.07405724077823318263 ) ) ;
#26609 = CARTESIAN_POINT ( 'NONE',  ( 0.07405724077823318263, -0.8838582676627719792, -0.1787899950787401604 ) ) ;
#26610 = CARTESIAN_POINT ( 'NONE',  ( -0.06523048226347956391, -1.176673228346457156, -0.1574803149606300301 ) ) ;
#26611 = CARTESIAN_POINT ( 'NONE',  ( 0.8759842519685039353, 0.1574803149606299191, 1.072834645561763889 ) ) ;
#26612 = DIRECTION ( 'NONE',  ( 0.000000000000000000, 0.000000000000000000, -1.000000000000000000 ) ) ;
#26613 = ORIENTED_EDGE ( 'NONE', *, *, #5038, .T. ) ;
#26614 = ORIENTED_EDGE ( 'NONE', *, *, #16427, .F. ) ;
#26615 = CARTESIAN_POINT ( 'NONE',  ( -0.7495606340400177148, -0.1264236179284866091, 1.783956692859621995 ) ) ;
#26616 = CARTESIAN_POINT ( 'NONE',  ( 0.7495606340400177148, 0.1264236179284866091, 1.695374015694267822 ) ) ;
#26617 = CARTESIAN_POINT ( 'NONE',  ( -1.181162989532618060E-16, 0.000000000000000000, -0.3937007874015748254 ) ) ;
#26618 = CARTESIAN_POINT ( 'NONE',  ( -0.9500414927467378812, 0.1787899950787401604, 1.446850393647023614 ) ) ;
#26619 = CARTESIAN_POINT ( 'NONE',  ( 0.1574803149606299746, -0.9875035750853327077, -1.463737590216208861 ) ) ;
#26620 = CARTESIAN_POINT ( 'NONE',  ( -0.6971942568897648851, 0.07405724077823318263, 1.181102362150960428 ) ) ;
#26621 = CARTESIAN_POINT ( 'NONE',  ( -0.6971942568897637749, 2.189545951927499583E-17, 0.9079724408911180600 ) ) ;
#26622 = VECTOR ( 'NONE', #41289, 39.37007874015748854 ) ;
#26623 = CARTESIAN_POINT ( 'NONE',  ( -1.002407869896990045, 0.1264236179284866091, 0.1107283464029293202 ) ) ;
#26624 = CARTESIAN_POINT ( 'NONE',  ( 0.09934514972678533395, 0.09575019180979006672, 0.2280761219286985830 ) ) ;
#26625 = CARTESIAN_POINT ( 'NONE',  ( -1.054774247047244540, 0.07405724077823318263, 1.643700787347811998 ) ) ;
#26626 = CARTESIAN_POINT ( 'NONE',  ( -0.7495606340400177148, -0.1264236179284866091, 0.05167322829269323931 ) ) ;
#26627 = DIRECTION ( 'NONE',  ( -7.216634497304837451E-16, -0.6156614753256588468, -0.7880107536067216811 ) ) ;
#26628 = CARTESIAN_POINT ( 'NONE',  ( -0.8107537697050253289, -0.1574803149606297803, 1.572342519685040685 ) ) ;
#26629 = CARTESIAN_POINT ( 'NONE',  ( -0.7185039370078739607, 1.928577636452523993E-17, 0.9350393700787401619 ) ) ;
#26630 = CARTESIAN_POINT ( 'NONE',  ( 0.6971942568897648851, -0.07405724077823297447, 1.624015747977732849 ) ) ;
#26631 = CARTESIAN_POINT ( 'NONE',  ( -0.2232765723780838485, -0.09842519685039370636, 0.08144284342645886909 ) ) ;
#26632 = CARTESIAN_POINT ( 'NONE',  ( -7.957671378281915615E-17, 0.1574803149606340824, -0.3937007874015748254 ) ) ;
#26633 = DIRECTION ( 'NONE',  ( 1.000000000000000000, 0.000000000000000000, 0.000000000000000000 ) ) ;
#26634 = ORIENTED_EDGE ( 'NONE', *, *, #15795, .F. ) ;
#26635 = VERTEX_POINT ( 'NONE', #21805 ) ;
#26636 = ORIENTED_EDGE ( 'NONE', *, *, #46737, .F. ) ;
#26637 = CARTESIAN_POINT ( 'NONE',  ( -0.7495606340400177148, 0.1264236179284866091, 1.183562992072220599 ) ) ;
#26638 = EDGE_LOOP ( 'NONE', ( #24537, #10644, #9734, #46109 ) ) ;
#26639 = EDGE_CURVE ( 'NONE', #43013, #25222, #4920, .T. ) ;
#26640 = CARTESIAN_POINT ( 'NONE',  ( 0.1787899950787401604, -0.9281496062454495100, -0.07405724077823318263 ) ) ;
#26641 = EDGE_CURVE ( 'NONE', #23712, #21986, #29106, .T. ) ;
#26642 = CARTESIAN_POINT ( 'NONE',  ( 0.1264236179284866091, -1.038877952702141672, -0.1264236179284866091 ) ) ;
#26643 = CIRCLE ( 'NONE', #10662, 0.1787899950787401049 ) ;
#26644 = FACE_OUTER_BOUND ( 'NONE', #22239, .T. ) ;
#26645 = ( CONVERSION_BASED_UNIT ( 'INCH', #38343 ) LENGTH_UNIT ( ) NAMED_UNIT ( #35386 ) ) ;
#26646 = CARTESIAN_POINT ( 'NONE',  ( -0.1797182628040039087, -0.3578194001342265285, -0.07444174185955065859 ) ) ;
#26647 = EDGE_CURVE ( 'NONE', #11821, #47083, #35782, .T. ) ;
#26648 = EDGE_CURVE ( 'NONE', #38550, #3105, #31735, .T. ) ;
#26649 = CARTESIAN_POINT ( 'NONE',  ( -0.9412147342319837628, 0.1574803149606300301, 0.1353346456692914035 ) ) ;
#26650 = CARTESIAN_POINT ( 'NONE',  ( 0.9500414927467378812, 0.1787899950787401604, 0.7775590550643479704 ) ) ;
#26651 = AXIS2_PLACEMENT_3D ( 'NONE', #29055, #14167, #43373 ) ;
#26653 = DIRECTION ( 'NONE',  ( -0.8660254037844388186, 0.000000000000000000, 0.4999999999999998890 ) ) ;
#26652 = CARTESIAN_POINT ( 'NONE',  ( 0.05652825169351837625, 0.2628576309303346514, -0.05517042925146131011 ) ) ;
#26654 = CARTESIAN_POINT ( 'NONE',  ( -0.9873396505805591694, 0.1113553986120547346, 1.264763779420031486 ) ) ;
#26655 = CARTESIAN_POINT ( 'NONE',  ( 0.1377952755905512694, 0.000000000000000000, -0.3149606299212598381 ) ) ;
#26656 = CARTESIAN_POINT ( 'NONE',  ( 1.054774247047244540, 0.07405724077823318263, 1.840551181048599938 ) ) ;
#26657 = CARTESIAN_POINT ( 'NONE',  ( 0.7185039370078739607, 1.928577636452523993E-17, 0.1476377952755905387 ) ) ;
#26658 = DIRECTION ( 'NONE',  ( -1.000000000000000000, 0.000000000000000000, 0.000000000000000000 ) ) ;
#26659 = CARTESIAN_POINT ( 'NONE',  ( -0.1264236179284866091, -0.3646653542769452971, -0.1264236179284866091 ) ) ;
#26660 = CARTESIAN_POINT ( 'NONE',  ( 0.1602931993194444682, -0.1591122789105269553, 0.000000000000000000 ) ) ;
#26661 = CARTESIAN_POINT ( 'NONE',  ( 0.1787899950787401882, -1.161909448765133801, -2.189545951927503898E-17 ) ) ;
#26662 = CARTESIAN_POINT ( 'NONE',  ( 0.7495606340400177148, -0.1264236179284866091, 0.2878937007336381804 ) ) ;
#26663 = CARTESIAN_POINT ( 'NONE',  ( -0.8759842519685039353, -0.1787899950787401882, 1.783956692859621995 ) ) ;
#26664 = EDGE_LOOP ( 'NONE', ( #19991, #26390, #18305, #42024 ) ) ;
#26665 = CARTESIAN_POINT ( 'NONE',  ( -0.6971942568897648851, 0.07405724077823318263, 1.343503936954111744 ) ) ;
#26666 = CARTESIAN_POINT ( 'NONE',  ( 0.9873396505805591694, -0.1113553986120547346, 1.028543307086614123 ) ) ;
#26667 = CARTESIAN_POINT ( 'NONE',  ( -0.6971942568897637749, 2.189545951927499583E-17, 0.5585629920722204877 ) ) ;
#26668 = CARTESIAN_POINT ( 'NONE',  ( 1.002407869896990045, 0.1264236179284866091, 1.956200787347811110 ) ) ;
#26669 = CARTESIAN_POINT ( 'NONE',  ( -0.8019270111902717657, 0.1787899950787401604, 1.136811023568283119 ) ) ;
#26670 = CARTESIAN_POINT ( 'NONE',  ( 0.8759842519685039353, 0.1574803149606299191, 1.545275590443653480 ) ) ;
#26671 = CARTESIAN_POINT ( 'NONE',  ( 0.1618536817989107701, 0.1553100982367987826, -0.01202753685181061002 ) ) ;
#26672 = DIRECTION ( 'NONE',  ( 0.000000000000000000, 0.000000000000000000, -1.000000000000000000 ) ) ;
#26673 = CARTESIAN_POINT ( 'NONE',  ( 0.8759842519685039353, -0.1787899950787401882, 0.5290354330171024300 ) ) ;
#26674 = CARTESIAN_POINT ( 'NONE',  ( -0.9500414927467377701, 0.1787899950787401604, 0.3838582676627718127 ) ) ;
#26675 = EDGE_LOOP ( 'NONE', ( #2248, #38816, #39887, #3367 ) ) ;
#26676 = VECTOR ( 'NONE', #26305, 39.37007874015748143 ) ;
#26677 = DIRECTION ( 'NONE',  ( 0.000000000000000000, 0.000000000000000000, 1.000000000000000000 ) ) ;
#26678 = ORIENTED_EDGE ( 'NONE', *, *, #41245, .T. ) ;
#26679 = ORIENTED_EDGE ( 'NONE', *, *, #12201, .T. ) ;
#26680 = CARTESIAN_POINT ( 'NONE',  ( -0.7646288533564489232, -0.1113553986120547346, 0.1525590551181102428 ) ) ;
#26681 = CARTESIAN_POINT ( 'NONE',  ( 0.8759842519685039353, 0.1787899950787401882, 1.178641732229700922 ) ) ;
#26682 = CARTESIAN_POINT ( 'NONE',  ( -1.054774247047244096, 0.000000000000000000, 1.951279527505291433 ) ) ;
#26683 = ORIENTED_EDGE ( 'NONE', *, *, #41904, .F. ) ;
#26684 = AXIS2_PLACEMENT_3D ( 'NONE', #11763, #4071, #11517 ) ;
#26685 = CARTESIAN_POINT ( 'NONE',  ( 0.2362204724409449064, -0.5708661417322835607, 0.9783464566929134243 ) ) ;
#26686 = FACE_OUTER_BOUND ( 'NONE', #27287, .T. ) ;
#26687 = CARTESIAN_POINT ( 'NONE',  ( 3.284318927891251994E-17, -1.423844440670183120, 0.1787899950787401882 ) ) ;
#26688 = ORIENTED_EDGE ( 'NONE', *, *, #12845, .T. ) ;
#26689 = CARTESIAN_POINT ( 'NONE',  ( 0.07405724077823318263, -0.4458661416785199560, -0.1787899950787401604 ) ) ;
#26690 = CARTESIAN_POINT ( 'NONE',  ( -0.2617501178043717958, -0.1661865978653775666, 0.8535951261345801067 ) ) ;
#26691 = ORIENTED_EDGE ( 'NONE', *, *, #47395, .T. ) ;
#26692 = CARTESIAN_POINT ( 'NONE',  ( 0.8759842519685039353, 0.1574803149606299191, 1.594488188976378007 ) ) ;
#26693 = CARTESIAN_POINT ( 'NONE',  ( 1.033464566929133799, 1.928577636452524610E-17, 4.498031496062992574 ) ) ;
#26694 = ( BOUNDED_CURVE ( )  B_SPLINE_CURVE ( 2, ( #8345, #15568, #22971, #30207, #1621, #45460, #44751, #4988, #19608, #12685, #11969, #45223, #34021, #27310, #9064, #1863, #41860, #23682, #27067, #38293, #30663, #19366, #44985, #26822, #41615, #8822, #23457, #30383, #4685, #44462, #37281, #12391, #11676, #27012, #12144, #23628, #41556, #8053, #23400, #19784, #38239, #5165, #16216, #20019, #34660, #27492, #17363, #12858, #32000, #31777, #21188, #24110, #13772, #42520, #28413, #24561, #13322, #35365, #6577, #35822, #9490, #31075, #39164, #35132, #6097, #2970, #16904, #28176, #2043, #13542, #42737, #42292, #6336, #17134, #45640, #42042, #31544, #38935, #16677, #9245, #46358, #38474, #5645, #9723, #31306, #45884, #552, #15448, #44634, #34140, #19009, #8232, #8707, #1034, #22623, #19728, #4621, #22857, #30328, #23096, #26712, #16158, #8467, #1271, #44400, #5104, #37715, #30551, #45114, #30790, #12332, #27195, #41748, #8953, #13722, #24055, #35314, #41981, #20672, #2452, #34846, #27904, #17079, #35547, #9436, #46069, #23804, #31719, #13273, #46308, #2690, #28127, #28359, #38658, #1991, #5831, #42927, #9187, #16620, #13496, #42686, #20438, #38420, #6284, #35073, #45826, #2222, #9671, #31249, #20907, #16842, #10138, #31482, #9901, #5590, #20197, #24513, #13037, #27673, #42467, #42233, #31017, #24287, #38882, #6045, #39110, #17317, #31955, #46539, #38179, #5341, #19962, #34602, #1753, #16396, #45583, #12805, #27439, #18495, #29579, #14210, #36259, #18264, #32189, #25477, #25220, #21865, #43893, #40283, #32910, #27, #7245, #14677, #33148, #272, #14916, #28612, #24747, #43174, #39342, #10379, #39581, #6759, #13731, #28369, #42938, #10148, #24757, #6534, #2924, #17560, #32198, #12816, #44133, #39820, #40056, #11099, #28622, #11331, #25943, #18732, #36957, #13972, #6772, #32449, #10629, #17671, #21751, #6406, #21018, #10751, #21263, #10017, #36383, #39468, #13842, #35886, #25102, #32068, #3541, #3041, #3288, #25358, #13601, #10262, #6171, #43302, #6644, #36133, #28977, #24867, #46425, #32320, #46898, #24633, #14089, #18152, #32792, #39231, #28732, #21498, #32559, #35434, #35666, #2569, #2803, #28241, #6878, #17909, #43779, #10504, #39694, #47148, #42803, #14332, #17435, #43533, #39939, #47387, #7129, #14561, #28487, #46659, #43056, #17205, #29232, #10981, #31843, #25598, #20790, #29695, #18611, #44939, #18386, #22442, #7371, #33501, #29464, #26539, #7826, #21982, #33270, #36837, #12151, #40169, #11441, #37063, #4215, #36604, #44699, #3762, #11917, #40864, #30391, #393, #30159, #18844, #8293, #33746, #614, #44468, #33027, #29923, #41099, #153, #855, #15045, #15272, #15757, #26058, #37289, #44008, #22685, #4441, #3989, #19073, #11683, #15514, #37534, #40628, #26308, #11212, #19324, #8060, #22921, #25826, #4693, #44236, #33973, #40402, #1099, #7589, #22204, #13106, #38724, #42051, #19792, #5892, #31553, #34426, #24119, #38484, #19560, #34669, #23409, #23873, #45891, #42304, #34911, #5654, #1816, #2054, #12636, #12868, #5174, #15991, #9013, #30614, #27737, #16687, #38246, #46131, #4935, #23635, #41334, #20028, #1335, #9498, #41812, #8534, #26774, #31316, #20504, #1572, #45419, #20264, #23165, #5407, #35141, #37782, #2284, #27501, #16913, #16224, #34206, #16453, #45178, #12399, #31086, #45650, #27020, #41569, #30856, #9253, #8774, #38013, #27260, #17853, #32010, #20733, #46369, #9729, #36065, #6818, #28187, #32496, #42992, #28911, #42746, #46602, #2516, #39878, #10201, #43475, #6108, #24806, #9962, #43240, #32734, #24574, #39173, #6346, #10443, #25040, #17142, #47078, #14272, #3222, #13780, #31786, #42527, #20960, #13331, #10682, #35606, #39637, #25289, #35373, #17373, #27960, #2980, #13550, #39404, #2747, #18088, #24346, #7063, #28427, #21690, #36322, #6586, #38943, #17613, #21201, #35834, #21438, #32258, #46837, #14026, #28672, #3476, #40576, #3709, #15459, #37239, #37010, #14500, #11856, #32968, #33444, #44641, #8241, #15217, #19018, #40807, #4631, #40343, #11153, #19265, #47329, #18557, #93, #14987, #14739, #29411, #7533, #36778, #33214, #338, #22631, #19736, #41275, #8716, #34149, #5597, #27207, #1277, #31028, #20205, #16627, #45836, #13045, #9448, #38671, #29457, #11205, #11433, #14551, #40858, #22680, #40394, #15507, #387, #11908, #22196, #33263, #29688, #22914, #4208, #18141, #10971, #47379, #18838, #33493, #609, #43768, #29913, #44461, #16676, #34659, #37771, #31305, #27729, #42291, #19783, #41324, #1091, #45168, #4684, #9489, #12390, #38004, #24109, #34198, #1325, #44929, #27011, #41555, #1561, #27250, #12143, #26767, #41804, #23627, #38238, #5396, #9722, #5886, #42983, #17133, #17362, #25033, #42519, #39628, #3214, #6576, #31776, #17843, #43466, #46357, #36056, #2734, #10191, #28412, #43228, #2277, #38934, #28661, #35821, #16903, #38716, #14015, #13771, #14263, #24560, #2969, #24336, #21187, #17602, #35364, #32246, #24799, #46827, #32489, #9951, #46592, #6096, #10433, #39392, #6809, #47071, #31999, #2509, #21429, #10672, #13541, #28175, #28905, #20721, #42736, #20493, #6335, #39163, #35131, #20952, #35597, #31543, #46123, #13321, #27952, #22142, #22377, #29860, #32726, #29402, #25279, #14978, #25763, #7759, #551, #43947, #18078, #40333, #11144, #29153, #7521, #7997, #4379, #43708, #36768, #40568, #4156, #7056, #10914, #21682, #25537, #47318, #25986, #37000, #15447, #3928, #18548, #18782, #14493, #33205, #21919, #33436, #44399, #40802, #15208, #11615, #82, #7299, #40105, #36312, #36540, #26236, #3467, #22622, #328, #14730, #3699, #30101, #18323, #44172, #39867, #11374, #32960, #37234, #19008, #33673, #785, #44633, #31248, #11847, #30550, #26946, #23343, #8231, #16395, #41037, #31016, #12568, #1990, #4866, #1752, #37955, #27438, #5340, #41502, #16157, #16619, #37714, #45356, #30327, #45582, #19494, #23572, #4620, #19727, #8466, #8952, #12804, #41980, #19961, #38178, #34364, #34601, #45113, #27194, #34139, #9186, #22856, #23803, #15922, #1270, #12331, #26474, #37473, #8706, #19254, #5103, #33912, #38419, #1503, #1033, #15690, #5589, #20196, #30789, #41747, #34845, #44874, #12087, #26711, #41267, #23095, #46537, #36004, #38880, #35772, #9899, #13959, #39340, #13494, #2688, #28610, #3162, #24285, #31953, #16840, #20670, #20905, #21379, #31717, #42925, #2220, #28357, #10136, #42465, #24745, #35545, #6520, #43172, #17077 ),
 .UNSPECIFIED., .F., .T. ) 
 B_SPLINE_CURVE_WITH_KNOTS ( ( 3, 2, 2, 2, 2, 2, 2, 2, 2, 2, 2, 2, 2, 2, 2, 2, 2, 2, 2, 2, 2, 2, 2, 2, 2, 2, 2, 2, 2, 2, 2, 2, 2, 2, 2, 2, 2, 2, 2, 2, 2, 2, 2, 2, 2, 2, 2, 2, 2, 2, 2, 2, 2, 2, 2, 2, 2, 2, 2, 2, 2, 2, 2, 2, 2, 2, 2, 2, 2, 2, 2, 2, 2, 2, 2, 2, 2, 2, 2, 2, 2, 2, 2, 2, 2, 2, 2, 2, 2, 2, 2, 2, 2, 2, 2, 2, 2, 2, 2, 2, 2, 2, 2, 2, 2, 2, 2, 2, 2, 2, 2, 2, 2, 2, 2, 2, 2, 2, 2, 2, 2, 2, 2, 2, 2, 2, 2, 2, 2, 2, 2, 2, 2, 2, 2, 2, 2, 2, 2, 2, 2, 2, 2, 2, 2, 2, 2, 2, 2, 2, 2, 2, 2, 2, 2, 2, 2, 2, 2, 2, 2, 2, 2, 2, 2, 2, 2, 2, 2, 2, 2, 2, 2, 2, 2, 2, 2, 2, 2, 2, 2, 2, 2, 2, 2, 2, 2, 2, 2, 2, 2, 2, 2, 2, 2, 2, 2, 2, 2, 2, 2, 2, 2, 2, 2, 2, 2, 2, 2, 2, 2, 2, 2, 2, 2, 2, 2, 2, 2, 2, 2, 2, 2, 2, 2, 2, 2, 2, 2, 2, 2, 2, 2, 2, 2, 2, 2, 2, 2, 2, 2, 2, 2, 2, 2, 2, 2, 2, 2, 2, 2, 2, 2, 2, 2, 2, 2, 2, 2, 2, 2, 2, 2, 2, 2, 2, 2, 2, 2, 2, 2, 2, 2, 2, 2, 2, 2, 2, 2, 2, 2, 2, 2, 2, 2, 2, 2, 2, 2, 2, 2, 2, 2, 2, 2, 2, 2, 2, 2, 2, 2, 2, 2, 2, 2, 2, 2, 2, 2, 2, 2, 2, 2, 2, 2, 2, 2, 2, 2, 2, 2, 2, 2, 2, 2, 2, 2, 2, 2, 2, 2, 2, 2, 2, 2, 2, 2, 2, 2, 2, 2, 2, 2, 2, 2, 2, 2, 2, 2, 2, 2, 2, 2, 2, 2, 2, 2, 2, 2, 2, 2, 2, 2, 2, 2, 2, 2, 2, 2, 2, 2, 2, 2, 2, 2, 2, 2, 2, 2, 2, 2, 2, 2, 2, 2, 2, 2, 2, 2, 2, 2, 2, 2, 2, 2, 2, 2, 3 ),
 ( 0.008749999973727599911, 0.01000000000000000021, 0.01250000000000000069, 0.01499999999999999944, 0.01750000000000000167, 0.02000000000000000042, 0.02249999999999999917, 0.02500000000000000139, 0.02750000000000000014, 0.02999999999999999889, 0.03250000000000000111, 0.03500000000000000333, 0.03749999999999999861, 0.04000000000000000083, 0.04250000000000000305, 0.04499999999999999833, 0.04750000000000000056, 0.05000000000000000278, 0.05249999999999999806, 0.05500000000000000028, 0.05750000000000000250, 0.05999999999999999778, 0.06250000000000000000, 0.06500000000000000222, 0.06750000000000000444, 0.07000000000000000666, 0.07250000000000000888, 0.07500000000000001110, 0.07750000000000001332, 0.08000000000000001554, 0.08250000000000001776, 0.08500000000000001998, 0.08749999999999999445, 0.08999999999999999667, 0.09249999999999999889, 0.09500000000000000111, 0.09750000000000000333, 0.1000000000000000056, 0.1025000000000000078, 0.1050000000000000100, 0.1075000000000000122, 0.1100000000000000144, 0.1125000000000000167, 0.1150000000000000189, 0.1174999999999999933, 0.1199999999999999956, 0.1224999999999999978, 0.1250000000000000000, 0.1275000000000000022, 0.1300000000000000044, 0.1325000000000000067, 0.1350000000000000089, 0.1375000000000000111, 0.1399999999999999856, 0.1424999999999999878, 0.1449999999999999900, 0.1474999999999999922, 0.1499999999999999944, 0.1524999999999999967, 0.1549999999999999989, 0.1575000000000000011, 0.1600000000000000033, 0.1625000000000000056, 0.1650000000000000078, 0.1675000000000000100, 0.1700000000000000122, 0.1724999999999999867, 0.1749999999999999889, 0.1774999999999999911, 0.1799999999999999933, 0.1824999999999999956, 0.1849999999999999978, 0.1875000000000000000, 0.1900000000000000022, 0.1925000000000000044, 0.1950000000000000067, 0.1975000000000000089, 0.2000000000000000111, 0.2025000000000000133, 0.2049999999999999878, 0.2074999999999999900, 0.2099999999999999922, 0.2124999999999999944, 0.2149999999999999967, 0.2174999999999999989, 0.2200000000000000011, 0.2225000000000000033, 0.2250000000000000056, 0.2275000000000000078, 0.2300000000000000100, 0.2325000000000000122, 0.2349999999999999867, 0.2374999999999999889, 0.2399999999999999911, 0.2424999999999999933, 0.2449999999999999956, 0.2474999999999999978, 0.2500000000000000000, 0.2525000000000000022, 0.2550000000000000044, 0.2575000000000000067, 0.2600000000000000089, 0.2625000000000000111, 0.2650000000000000133, 0.2675000000000000155, 0.2700000000000000178, 0.2725000000000000200, 0.2750000000000000222, 0.2775000000000000244, 0.2800000000000000266, 0.2824999999999999734, 0.2849999999999999756, 0.2874999999999999778, 0.2899999999999999800, 0.2924999999999999822, 0.2949999999999999845, 0.2974999999999999867, 0.2999999999999999889, 0.3024999999999999911, 0.3049999999999999933, 0.3074999999999999956, 0.3099999999999999978, 0.3125000000000000000, 0.3150000000000000022, 0.3175000000000000044, 0.3200000000000000067, 0.3225000000000000089, 0.3250000000000000111, 0.3275000000000000133, 0.3300000000000000155, 0.3325000000000000178, 0.3350000000000000200, 0.3375000000000000222, 0.3400000000000000244, 0.3425000000000000266, 0.3449999999999999734, 0.3474999999999999756, 0.3499999999999999778, 0.3524999999999999800, 0.3549999999999999822, 0.3574999999999999845, 0.3599999999999999867, 0.3624999999999999889, 0.3649999999999999911, 0.3674999999999999933, 0.3699999999999999956, 0.3724999999999999978, 0.3750000000000000000, 0.3775000000000000022, 0.3800000000000000044, 0.3825000000000000067, 0.3850000000000000089, 0.3875000000000000111, 0.3900000000000000133, 0.3925000000000000155, 0.3950000000000000178, 0.3975000000000000200, 0.4000000000000000222, 0.4025000000000000244, 0.4050000000000000266, 0.4074999999999999734, 0.4099999999999999756, 0.4124999999999999778, 0.4149999999999999800, 0.4174999999999999822, 0.4199999999999999845, 0.4224999999999999867, 0.4249999999999999889, 0.4274999999999999911, 0.4299999999999999933, 0.4324999999999999956, 0.4349999999999999978, 0.4375000000000000000, 0.4400000000000000022, 0.4425000000000000044, 0.4450000000000000067, 0.4475000000000000089, 0.4500000000000000111, 0.4525000000000000133, 0.4550000000000000155, 0.4575000000000000178, 0.4600000000000000200, 0.4625000000000000222, 0.4650000000000000244, 0.4675000000000000266, 0.4699999999999999734, 0.4724999999999999756, 0.4749999999999999778, 0.4774999999999999800, 0.4799999999999999822, 0.4824999999999999845, 0.4849999999999999867, 0.4874999999999999889, 0.4899999999999999911, 0.4924999999999999933, 0.4949999999999999956, 0.4974999999999999978, 0.5000000000000000000, 0.5024999999999999467, 0.5050000000000000044, 0.5074999999999999512, 0.5100000000000000089, 0.5124999999999999556, 0.5150000000000000133, 0.5174999999999999600, 0.5200000000000000178, 0.5224999999999999645, 0.5250000000000000222, 0.5274999999999999689, 0.5300000000000000266, 0.5324999999999999734, 0.5350000000000000311, 0.5374999999999999778, 0.5400000000000000355, 0.5424999999999999822, 0.5450000000000000400, 0.5474999999999999867, 0.5500000000000000444, 0.5524999999999999911, 0.5550000000000000488, 0.5574999999999999956, 0.5600000000000000533, 0.5625000000000000000, 0.5649999999999999467, 0.5675000000000000044, 0.5699999999999999512, 0.5725000000000000089, 0.5749999999999999556, 0.5775000000000000133, 0.5799999999999999600, 0.5825000000000000178, 0.5849999999999999645, 0.5875000000000000222, 0.5899999999999999689, 0.5925000000000000266, 0.5949999999999999734, 0.5975000000000000311, 0.5999999999999999778, 0.6025000000000000355, 0.6049999999999999822, 0.6075000000000000400, 0.6099999999999999867, 0.6125000000000000444, 0.6149999999999999911, 0.6175000000000000488, 0.6199999999999999956, 0.6225000000000000533, 0.6250000000000000000, 0.6274999999999999467, 0.6300000000000000044, 0.6324999999999999512, 0.6350000000000000089, 0.6374999999999999556, 0.6400000000000000133, 0.6424999999999999600, 0.6450000000000000178, 0.6474999999999999645, 0.6500000000000000222, 0.6524999999999999689, 0.6550000000000000266, 0.6574999999999999734, 0.6600000000000000311, 0.6624999999999999778, 0.6650000000000000355, 0.6674999999999999822, 0.6700000000000000400, 0.6724999999999999867, 0.6750000000000000444, 0.6774999999999999911, 0.6800000000000000488, 0.6824999999999999956, 0.6850000000000000533, 0.6875000000000000000, 0.6899999999999999467, 0.6925000000000000044, 0.6949999999999999512, 0.6975000000000000089, 0.6999999999999999556, 0.7025000000000000133, 0.7049999999999999600, 0.7075000000000000178, 0.7099999999999999645, 0.7125000000000000222, 0.7149999999999999689, 0.7175000000000000266, 0.7199999999999999734, 0.7225000000000000311, 0.7249999999999999778, 0.7275000000000000355, 0.7299999999999999822, 0.7325000000000000400, 0.7349999999999999867, 0.7375000000000000444, 0.7399999999999999911, 0.7425000000000000488, 0.7449999999999999956, 0.7474999999999999423, 0.7500000000000000000, 0.7524999999999999467, 0.7550000000000000044, 0.7574999999999999512, 0.7600000000000000089, 0.7624999999999999556, 0.7649999999999999023, 0.7674999999999999600, 0.7700000000000000178, 0.7724999999999999645, 0.7750000000000000222, 0.7774999999999999689, 0.7800000000000000266, 0.7824999999999998623, 0.7850000000000000311, 0.7874999999999999778, 0.7900000000000000355, 0.7924999999999999822, 0.7950000000000000400, 0.7974999999999999867, 0.8000000000000000444, 0.8024999999999999911, 0.8050000000000000488, 0.8074999999999999956, 0.8100000000000000533, 0.8125000000000000000, 0.8149999999999999467, 0.8175000000000000044, 0.8199999999999999512, 0.8225000000000000089, 0.8249999999999999556, 0.8275000000000000133, 0.8299999999999999600, 0.8325000000000000178, 0.8349999999999999645, 0.8375000000000000222, 0.8399999999999999689, 0.8425000000000000266, 0.8449999999999999734, 0.8475000000000000311, 0.8499999999999999778, 0.8525000000000000355, 0.8549999999999999822, 0.8575000000000000400, 0.8599999999999999867, 0.8625000000000000444, 0.8649999999999999911, 0.8675000000000000488, 0.8699999999999999956, 0.8725000000000000533, 0.8750000000000000000, 0.8774999999999999467, 0.8800000000000000044, 0.8824999999999999512, 0.8850000000000000089, 0.8874999999999999556, 0.8900000000000000133, 0.8924999999999999600, 0.8950000000000000178, 0.8974999999999999645, 0.9000000000000000222, 0.9024999999999999689, 0.9050000000000000266, 0.9074999999999999734, 0.9100000000000000311, 0.9124999999999999778, 0.9150000000000000355, 0.9174999999999999822, 0.9200000000000000400, 0.9224999999999999867, 0.9250000000000000444, 0.9274999999999999911, 0.9300000000000000488, 0.9324999999999999956, 0.9350000000000000533, 0.9375000000000000000, 0.9399999999999999467, 0.9425000000000000044, 0.9449999999999999512, 0.9475000000000000089, 0.9499999999999999556, 0.9525000000000000133, 0.9549999999999999600, 0.9575000000000000178, 0.9599999999999999645, 0.9625000000000000222, 0.9649999999999999689, 0.9675000000000000266, 0.9699999999999999734, 0.9725000000000000311, 0.9749999999999999778, 0.9775000000000000355, 0.9799999999999999822, 0.9825000000000000400, 0.9849999999999999867, 0.9875000000000000444, 0.9899999999999999911, 0.9925000000000000488, 0.9949999999999999956, 0.9975000000000000533, 1.000000000000000000 ),
 .UNSPECIFIED. ) 
 CURVE ( )  GEOMETRIC_REPRESENTATION_ITEM ( )  RATIONAL_B_SPLINE_CURVE ( ( 0.9619397662556429252, 0.9619397654556960386, 1.000000000000000000, 0.9238795325112869605, 1.000000000000000000, 0.9238795325112869605, 1.000000000000000000, 0.9238795325112869605, 1.000000000000000000, 0.9238795325112869605, 1.000000000000000000, 0.9238795325112869605, 1.000000000000000000, 0.9238795325112869605, 1.000000000000000000, 0.9238795325112869605, 1.000000000000000000, 0.9238795325112869605, 1.000000000000000000, 0.9238795325112869605, 1.000000000000000000, 0.9238795325112869605, 1.000000000000000000, 0.9238795325112869605, 1.000000000000000000, 0.9238795325112869605, 1.000000000000000000, 0.9238795325112869605, 1.000000000000000000, 0.9238795325112869605, 1.000000000000000000, 0.9238795325112869605, 1.000000000000000000, 0.9238795325112869605, 1.000000000000000000, 0.9238795325112869605, 1.000000000000000000, 0.9238795325112869605, 1.000000000000000000, 0.9238795325112869605, 1.000000000000000000, 0.9238795325112869605, 1.000000000000000000, 0.9238795325112869605, 1.000000000000000000, 0.9238795325112869605, 1.000000000000000000, 0.9238795325112869605, 1.000000000000000000, 0.9238795325112869605, 1.000000000000000000, 0.9238795325112869605, 1.000000000000000000, 0.9238795325112869605, 1.000000000000000000, 0.9238795325112869605, 1.000000000000000000, 0.9238795325112869605, 1.000000000000000000, 0.9238795325112869605, 1.000000000000000000, 0.9238795325112869605, 1.000000000000000000, 0.9238795325112869605, 1.000000000000000000, 0.9238795325112869605, 1.000000000000000000, 0.9238795325112869605, 1.000000000000000000, 0.9238795325112869605, 1.000000000000000000, 0.9238795325112869605, 1.000000000000000000, 0.9238795325112869605, 1.000000000000000000, 0.9238795325112869605, 1.000000000000000000, 0.9238795325112869605, 1.000000000000000000, 0.9238795325112869605, 1.000000000000000000, 0.9238795325112869605, 1.000000000000000000, 0.9238795325112869605, 1.000000000000000000, 0.9238795325112869605, 1.000000000000000000, 0.9238795325112869605, 1.000000000000000000, 0.9238795325112869605, 1.000000000000000000, 0.9238795325112869605, 1.000000000000000000, 0.9238795325112869605, 1.000000000000000000, 0.9238795325112869605, 1.000000000000000000, 0.9238795325112869605, 1.000000000000000000, 0.9238795325112869605, 1.000000000000000000, 0.9238795325112869605, 1.000000000000000000, 0.9238795325112869605, 1.000000000000000000, 0.9238795325112869605, 1.000000000000000000, 0.9238795325112869605, 1.000000000000000000, 0.9238795325112869605, 1.000000000000000000, 0.9238795325112869605, 1.000000000000000000, 0.9238795325112869605, 1.000000000000000000, 0.9238795325112869605, 1.000000000000000000, 0.9238795325112869605, 1.000000000000000000, 0.9238795325112869605, 1.000000000000000000, 0.9238795325112869605, 1.000000000000000000, 0.9238795325112869605, 1.000000000000000000, 0.9238795325112869605, 1.000000000000000000, 0.9238795325112869605, 1.000000000000000000, 0.9238795325112869605, 1.000000000000000000, 0.9238795325112869605, 1.000000000000000000, 0.9238795325112869605, 1.000000000000000000, 0.9238795325112869605, 1.000000000000000000, 0.9238795325112869605, 1.000000000000000000, 0.9238795325112869605, 1.000000000000000000, 0.9238795325112869605, 1.000000000000000000, 0.9238795325112869605, 1.000000000000000000, 0.9238795325112869605, 1.000000000000000000, 0.9238795325112869605, 1.000000000000000000, 0.9238795325112869605, 1.000000000000000000, 0.9238795325112869605, 1.000000000000000000, 0.9238795325112869605, 1.000000000000000000, 0.9238795325112869605, 1.000000000000000000, 0.9238795325112869605, 1.000000000000000000, 0.9238795325112869605, 1.000000000000000000, 0.9238795325112869605, 1.000000000000000000, 0.9238795325112869605, 1.000000000000000000, 0.9238795325112869605, 1.000000000000000000, 0.9238795325112869605, 1.000000000000000000, 0.9238795325112869605, 1.000000000000000000, 0.9238795325112869605, 1.000000000000000000, 0.9238795325112869605, 1.000000000000000000, 0.9238795325112869605, 1.000000000000000000, 0.9238795325112869605, 1.000000000000000000, 0.9238795325112869605, 1.000000000000000000, 0.9238795325112869605, 1.000000000000000000, 0.9238795325112869605, 1.000000000000000000, 0.9238795325112869605, 1.000000000000000000, 0.9238795325112869605, 1.000000000000000000, 0.9238795325112869605, 1.000000000000000000, 0.9238795325112869605, 1.000000000000000000, 0.9238795325112869605, 1.000000000000000000, 0.9238795325112869605, 1.000000000000000000, 0.9238795325112869605, 1.000000000000000000, 0.9238795325112869605, 1.000000000000000000, 0.9238795325112869605, 1.000000000000000000, 0.9238795325112869605, 1.000000000000000000, 0.9238795325112869605, 1.000000000000000000, 0.9238795325112869605, 1.000000000000000000, 0.9238795325112869605, 1.000000000000000000, 0.9238795325112869605, 1.000000000000000000, 0.9238795325112869605, 1.000000000000000000, 0.9238795325112869605, 1.000000000000000000, 0.9238795325112869605, 1.000000000000000000, 0.9238795325112869605, 1.000000000000000000, 0.9238795325112869605, 1.000000000000000000, 0.9238795325112869605, 1.000000000000000000, 0.9238795325112869605, 1.000000000000000000, 0.9238795325112869605, 1.000000000000000000, 0.9238795325112869605, 1.000000000000000000, 0.9238795325112869605, 1.000000000000000000, 0.9238795325112869605, 1.000000000000000000, 0.9238795325112869605, 1.000000000000000000, 0.9238795325112869605, 1.000000000000000000, 0.9238795325112869605, 1.000000000000000000, 0.9238795325112869605, 1.000000000000000000, 0.9238795325112869605, 1.000000000000000000, 0.9238795325112869605, 1.000000000000000000, 0.9238795325112869605, 1.000000000000000000, 0.9238795325112869605, 1.000000000000000000, 0.9238795325112869605, 1.000000000000000000, 0.9238795325112869605, 1.000000000000000000, 0.9238795325112869605, 1.000000000000000000, 0.9238795325112869605, 1.000000000000000000, 0.9238795325112869605, 1.000000000000000000, 0.9238795325112869605, 1.000000000000000000, 0.9238795325112869605, 1.000000000000000000, 0.9238795325112869605, 1.000000000000000000, 0.9238795325112869605, 1.000000000000000000, 0.9238795325112869605, 1.000000000000000000, 0.9238795325112869605, 1.000000000000000000, 0.9238795325112869605, 1.000000000000000000, 0.9238795325112869605, 1.000000000000000000, 0.9238795325112869605, 1.000000000000000000, 0.9238795325112869605, 1.000000000000000000, 0.9238795325112869605, 1.000000000000000000, 0.9238795325112869605, 1.000000000000000000, 0.9238795325112869605, 1.000000000000000000, 0.9238795325112869605, 1.000000000000000000, 0.9238795325112869605, 1.000000000000000000, 0.9238795325112869605, 1.000000000000000000, 0.9238795325112869605, 1.000000000000000000, 0.9238795325112869605, 1.000000000000000000, 0.9238795325112869605, 1.000000000000000000, 0.9238795325112869605, 1.000000000000000000, 0.9238795325112869605, 1.000000000000000000, 0.9238795325112869605, 1.000000000000000000, 0.9238795325112869605, 1.000000000000000000, 0.9238795325112869605, 1.000000000000000000, 0.9238795325112869605, 1.000000000000000000, 0.9238795325112869605, 1.000000000000000000, 0.9238795325112869605, 1.000000000000000000, 0.9238795325112869605, 1.000000000000000000, 0.9238795325112869605, 1.000000000000000000, 0.9238795325112869605, 1.000000000000000000, 0.9238795325112869605, 1.000000000000000000, 0.9238795325112869605, 1.000000000000000000, 0.9238795325112869605, 1.000000000000000000, 0.9238795325112869605, 1.000000000000000000, 0.9238795325112869605, 1.000000000000000000, 0.9238795325112869605, 1.000000000000000000, 0.9238795325112869605, 1.000000000000000000, 0.9238795325112869605, 1.000000000000000000, 0.9238795325112869605, 1.000000000000000000, 0.9238795325112869605, 1.000000000000000000, 0.9238795325112869605, 1.000000000000000000, 0.9238795325112869605, 1.000000000000000000, 0.9238795325112869605, 1.000000000000000000, 0.9238795325112869605, 1.000000000000000000, 0.9238795325112869605, 1.000000000000000000, 0.9238795325112869605, 1.000000000000000000, 0.9238795325112869605, 1.000000000000000000, 0.9238795325112869605, 1.000000000000000000, 0.9238795325112869605, 1.000000000000000000, 0.9238795325112869605, 1.000000000000000000, 0.9238795325112869605, 1.000000000000000000, 0.9238795325112869605, 1.000000000000000000, 0.9238795325112869605, 1.000000000000000000, 0.9238795325112869605, 1.000000000000000000, 0.9238795325112869605, 1.000000000000000000, 0.9238795325112869605, 1.000000000000000000, 0.9238795325112869605, 1.000000000000000000, 0.9238795325112869605, 1.000000000000000000, 0.9238795325112869605, 1.000000000000000000, 0.9238795325112869605, 1.000000000000000000, 0.9238795325112869605, 1.000000000000000000, 0.9238795325112869605, 1.000000000000000000, 0.9238795325112869605, 1.000000000000000000, 0.9238795325112869605, 1.000000000000000000, 0.9238795325112869605, 1.000000000000000000, 0.9238795325112869605, 1.000000000000000000, 0.9238795325112869605, 1.000000000000000000, 0.9238795325112869605, 1.000000000000000000, 0.9238795325112869605, 1.000000000000000000, 0.9238795325112869605, 1.000000000000000000, 0.9238795325112869605, 1.000000000000000000, 0.9238795325112869605, 1.000000000000000000, 0.9238795325112869605, 1.000000000000000000, 0.9238795325112869605, 1.000000000000000000, 0.9238795325112869605, 1.000000000000000000, 0.9238795325112869605, 1.000000000000000000, 0.9238795325112869605, 1.000000000000000000, 0.9238795325112869605, 1.000000000000000000, 0.9238795325112869605, 1.000000000000000000, 0.9238795325112869605, 1.000000000000000000, 0.9238795325112869605, 1.000000000000000000, 0.9238795325112869605, 1.000000000000000000, 0.9238795325112869605, 1.000000000000000000, 0.9238795325112869605, 1.000000000000000000, 0.9238795325112869605, 1.000000000000000000, 0.9238795325112869605, 1.000000000000000000, 0.9238795325112869605, 1.000000000000000000, 0.9238795325112869605, 1.000000000000000000, 0.9238795325112869605, 1.000000000000000000, 0.9238795325112869605, 1.000000000000000000, 0.9238795325112869605, 1.000000000000000000, 0.9238795325112869605, 1.000000000000000000, 0.9238795325112869605, 1.000000000000000000, 0.9238795325112869605, 1.000000000000000000, 0.9238795325112869605, 1.000000000000000000, 0.9238795325112869605, 1.000000000000000000, 0.9238795325112869605, 1.000000000000000000, 0.9238795325112869605, 1.000000000000000000, 0.9238795325112869605, 1.000000000000000000, 0.9238795325112869605, 1.000000000000000000, 0.9238795325112869605, 1.000000000000000000, 0.9238795325112869605, 1.000000000000000000, 0.9238795325112869605, 1.000000000000000000, 0.9238795325112869605, 1.000000000000000000, 0.9238795325112869605, 1.000000000000000000, 0.9238795325112869605, 1.000000000000000000, 0.9238795325112869605, 1.000000000000000000, 0.9238795325112869605, 1.000000000000000000, 0.9238795325112869605, 1.000000000000000000, 0.9238795325112869605, 1.000000000000000000, 0.9238795325112869605, 1.000000000000000000, 0.9238795325112869605, 1.000000000000000000, 0.9238795325112869605, 1.000000000000000000, 0.9238795325112869605, 1.000000000000000000, 0.9238795325112869605, 1.000000000000000000, 0.9238795325112869605, 1.000000000000000000, 0.9238795325112869605, 1.000000000000000000, 0.9238795325112869605, 1.000000000000000000, 0.9238795325112869605, 1.000000000000000000, 0.9238795325112869605, 1.000000000000000000, 0.9238795325112869605, 1.000000000000000000, 0.9238795325112869605, 1.000000000000000000, 0.9238795325112869605, 1.000000000000000000, 0.9238795325112869605, 1.000000000000000000, 0.9238795325112869605, 1.000000000000000000, 0.9238795325112869605, 1.000000000000000000, 0.9238795325112869605, 1.000000000000000000, 0.9238795325112869605, 1.000000000000000000, 0.9238795325112869605, 1.000000000000000000, 0.9238795325112869605, 1.000000000000000000, 0.9238795325112869605, 1.000000000000000000, 0.9238795325112869605, 1.000000000000000000, 0.9238795325112869605, 1.000000000000000000, 0.9238795325112869605, 1.000000000000000000, 0.9238795325112869605, 1.000000000000000000, 0.9238795325112869605, 1.000000000000000000, 0.9238795325112869605, 1.000000000000000000, 0.9238795325112869605, 1.000000000000000000, 0.9238795325112869605, 1.000000000000000000, 0.9238795325112869605, 1.000000000000000000, 0.9238795325112869605, 1.000000000000000000, 0.9238795325112869605, 1.000000000000000000, 0.9238795325112869605, 1.000000000000000000, 0.9238795325112869605, 1.000000000000000000, 0.9238795325112869605, 1.000000000000000000, 0.9238795325112869605, 1.000000000000000000, 0.9238795325112869605, 1.000000000000000000, 0.9238795325112869605, 1.000000000000000000, 0.9238795325112869605, 1.000000000000000000, 0.9238795325112869605, 1.000000000000000000, 0.9238795325112869605, 1.000000000000000000, 0.9238795325112869605, 1.000000000000000000, 0.9238795325112869605, 1.000000000000000000, 0.9238795325112869605, 1.000000000000000000, 0.9238795325112869605, 1.000000000000000000, 0.9238795325112869605, 1.000000000000000000, 0.9238795325112869605, 1.000000000000000000, 0.9238795325112869605, 1.000000000000000000, 0.9238795325112869605, 1.000000000000000000, 0.9238795325112869605, 1.000000000000000000, 0.9238795325112869605, 1.000000000000000000, 0.9238795325112869605, 1.000000000000000000, 0.9238795325112869605, 1.000000000000000000, 0.9238795325112869605, 1.000000000000000000, 0.9238795325112869605, 1.000000000000000000, 0.9238795325112869605, 1.000000000000000000, 0.9238795325112869605, 1.000000000000000000, 0.9238795325112869605, 1.000000000000000000, 0.9238795325112869605, 1.000000000000000000, 0.9238795325112869605, 1.000000000000000000, 0.9238795325112869605, 1.000000000000000000, 0.9238795325112869605, 1.000000000000000000, 0.9238795325112869605, 1.000000000000000000, 0.9238795325112869605, 1.000000000000000000, 0.9238795325112869605, 1.000000000000000000, 0.9238795325112869605, 1.000000000000000000, 0.9238795325112869605, 1.000000000000000000, 0.9238795325112869605, 1.000000000000000000, 0.9238795325112869605, 1.000000000000000000, 0.9238795325112869605, 1.000000000000000000, 0.9238795325112869605, 1.000000000000000000, 0.9238795325112869605, 1.000000000000000000, 0.9238795325112869605, 1.000000000000000000, 0.9238795325112869605, 1.000000000000000000, 0.9238795325112869605, 1.000000000000000000, 0.9238795325112869605, 1.000000000000000000, 0.9238795325112869605, 1.000000000000000000, 0.9238795325112869605, 1.000000000000000000, 0.9238795325112869605, 1.000000000000000000, 0.9238795325112869605, 1.000000000000000000, 0.9238795325112869605, 1.000000000000000000, 0.9238795325112869605, 1.000000000000000000, 0.9238795325112869605, 1.000000000000000000, 0.9238795325112869605, 1.000000000000000000, 0.9238795325112869605, 1.000000000000000000, 0.9238795325112869605, 1.000000000000000000, 0.9238795325112869605, 1.000000000000000000, 0.9238795325112869605, 1.000000000000000000, 0.9238795325112869605, 1.000000000000000000, 0.9238795325112869605, 1.000000000000000000, 0.9238795325112869605, 1.000000000000000000, 0.9238795325112869605, 1.000000000000000000, 0.9238795325112869605, 1.000000000000000000, 0.9238795325112869605, 1.000000000000000000, 0.9238795325112869605, 1.000000000000000000, 0.9238795325112869605, 1.000000000000000000, 0.9238795325112869605, 1.000000000000000000, 0.9238795325112869605, 1.000000000000000000, 0.9238795325112869605, 1.000000000000000000, 0.9238795325112869605, 1.000000000000000000, 0.9238795325112869605, 1.000000000000000000, 0.9238795325112869605, 1.000000000000000000, 0.9238795325112869605, 1.000000000000000000, 0.9238795325112869605, 1.000000000000000000, 0.9238795325112869605, 1.000000000000000000, 0.9238795325112869605, 1.000000000000000000, 0.9238795325112869605, 1.000000000000000000, 0.9238795325112869605, 1.000000000000000000, 0.9238795325112869605, 1.000000000000000000, 0.9238795325112869605, 1.000000000000000000, 0.9238795325112869605, 1.000000000000000000, 0.9238795325112869605, 1.000000000000000000, 0.9238795325112869605, 1.000000000000000000, 0.9238795325112869605, 1.000000000000000000, 0.9238795325112869605, 1.000000000000000000, 0.9238795325112869605, 1.000000000000000000, 0.9238795325112869605, 1.000000000000000000, 0.9238795325112869605, 1.000000000000000000, 0.9238795325112869605, 1.000000000000000000, 0.9238795325112869605, 1.000000000000000000, 0.9238795325112869605, 1.000000000000000000, 0.9238795325112869605, 1.000000000000000000, 0.9238795325112869605, 1.000000000000000000, 0.9238795325112869605, 1.000000000000000000, 0.9238795325112869605, 1.000000000000000000, 0.9238795325112869605, 1.000000000000000000, 0.9238795325112869605, 1.000000000000000000, 0.9238795325112869605, 1.000000000000000000, 0.9238795325112869605, 1.000000000000000000, 0.9238795325112869605, 1.000000000000000000, 0.9238795325112869605, 1.000000000000000000, 0.9238795325112869605, 1.000000000000000000, 0.9238795325112869605, 1.000000000000000000, 0.9238795325112869605, 1.000000000000000000, 0.9238795325112869605, 1.000000000000000000, 0.9238795325112869605, 1.000000000000000000, 0.9238795325112869605, 1.000000000000000000, 0.9238795325112869605, 1.000000000000000000, 0.9238795325112869605, 1.000000000000000000, 0.9238795325112869605, 1.000000000000000000, 0.9238795325112869605, 1.000000000000000000, 0.9238795325112869605, 1.000000000000000000, 0.9238795325112869605, 1.000000000000000000, 0.9238795325112869605, 1.000000000000000000, 0.9238795325112869605, 1.000000000000000000, 0.9238795325112869605, 1.000000000000000000, 0.9238795325112869605, 1.000000000000000000, 0.9238795325112869605, 1.000000000000000000, 0.9238795325112869605, 1.000000000000000000, 0.9238795325112869605, 1.000000000000000000, 0.9238795325112869605, 1.000000000000000000, 0.9238795325112869605, 1.000000000000000000, 0.9238795325112869605, 1.000000000000000000, 0.9238795325112869605, 1.000000000000000000, 0.9238795325112869605, 1.000000000000000000, 0.9238795325112869605, 1.000000000000000000, 0.9238795325112869605, 1.000000000000000000 ) ) 
 REPRESENTATION_ITEM ( '' )  ) ;
#26695 = EDGE_CURVE ( 'NONE', #42967, #14779, #10558, .T. ) ;
#26696 = CARTESIAN_POINT ( 'NONE',  ( 0.6971942568897626646, 0.07405724077823318263, 0.2362204723871814960 ) ) ;
#26697 = ADVANCED_FACE ( 'NONE', ( #35485 ), #31895, .T. ) ;
#26698 = CARTESIAN_POINT ( 'NONE',  ( 0.1787899950787401882, -1.718011810969858333, -2.189545951927503898E-17 ) ) ;
#26699 = CARTESIAN_POINT ( 'NONE',  ( 0.1264236179284866091, -1.786909448765134023, -0.1264236179284866091 ) ) ;
#26700 = ( CONVERSION_BASED_UNIT ( 'INCH', #15436 ) LENGTH_UNIT ( ) NAMED_UNIT ( #34772 ) ) ;
#26701 = CARTESIAN_POINT ( 'NONE',  ( 0.2395294000716133853, 2.049113738730801466E-17, 1.043307086614172707 ) ) ;
#26702 = EDGE_CURVE ( 'NONE', #5079, #32371, #4496, .T. ) ;
#26703 = CARTESIAN_POINT ( 'NONE',  ( -0.6971942568897648851, -0.07405724077823297447, 0.7185039369541108556 ) ) ;
#26704 = AXIS2_PLACEMENT_3D ( 'NONE', #4382, #15212, #18083 ) ;
#26706 = FILL_AREA_STYLE_COLOUR ( '', #17852 ) ;
#26705 = CARTESIAN_POINT ( 'NONE',  ( -0.06523048226347956391, -0.7288385826771652809, 0.1574803149606297803 ) ) ;
#26707 = CARTESIAN_POINT ( 'NONE',  ( 0.1797182628040039365, -1.477406014307454774, -2.200913952912460540E-17 ) ) ;
#26708 = CARTESIAN_POINT ( 'NONE',  ( 0.4151545546392377273, 1.205361022782824954E-17, -0.09842519685039370636 ) ) ;
#26709 = DIRECTION ( 'NONE',  ( 0.000000000000000000, 0.000000000000000000, 1.000000000000000000 ) ) ;
#26710 = CARTESIAN_POINT ( 'NONE',  ( 0.6971942568897637749, 2.189545951927499583E-17, 1.306594488135212728 ) ) ;
#26711 = CARTESIAN_POINT ( 'NONE',  ( 1.002407869896990045, 0.1264236179284866091, 1.916830708607653477 ) ) ;
#26712 = CARTESIAN_POINT ( 'NONE',  ( 0.7495606340400177148, -0.1264236179284866091, 0.2829724408911185041 ) ) ;
#26714 = ORIENTED_EDGE ( 'NONE', *, *, #20832, .F. ) ;
#26713 = FACE_OUTER_BOUND ( 'NONE', #210, .T. ) ;
#26715 = DIRECTION ( 'NONE',  ( -1.217491584052838080E-15, -0.6156614753256588468, -0.7880107536067214591 ) ) ;
#26716 = DIRECTION ( 'NONE',  ( 1.000000000000000000, 0.000000000000000000, 0.000000000000000000 ) ) ;
#26717 = CARTESIAN_POINT ( 'NONE',  ( -1.094772975963752103E-17, 0.06348425202226751218, -0.1787899950787401882 ) ) ;
#26718 = AXIS2_PLACEMENT_3D ( 'NONE', #1596, #31110, #5439 ) ;
#26720 = CARTESIAN_POINT ( 'NONE',  ( 0.6971942568897626646, -0.07405724077823297447, 0.2805118109698587214 ) ) ;
#26719 = ( BOUNDED_CURVE ( )  B_SPLINE_CURVE ( 2, ( #2703, #17330, #35787, #43184, #10394, #24998, #39594, #6775, #21391 ),
 .UNSPECIFIED., .F., .T. ) 
 B_SPLINE_CURVE_WITH_KNOTS ( ( 3, 2, 2, 2, 3 ),
 ( 0.07000000000000000666, 0.07249999999999999500, 0.07499999999999999722, 0.07749999999999999944, 0.08000000000000000167 ),
 .UNSPECIFIED. ) 
 CURVE ( )  GEOMETRIC_REPRESENTATION_ITEM ( )  RATIONAL_B_SPLINE_CURVE ( ( 1.000000000000000000, 0.9238795325112859613, 1.000000000000000000, 0.9238795325112869605, 1.000000000000000000, 0.9238795325112869605, 1.000000000000000000, 0.9238795325112869605, 1.000000000000000000 ) ) 
 REPRESENTATION_ITEM ( '' )  ) ;
#26721 = DIRECTION ( 'NONE',  ( 0.000000000000000000, 0.000000000000000000, -1.000000000000000000 ) ) ;
#26722 = LINE ( 'NONE', #41277, #15909 ) ;
#26723 = CARTESIAN_POINT ( 'NONE',  ( -0.7646288533564489232, 0.1113553986120547346, 0.7726377952755906220 ) ) ;
#26724 = CARTESIAN_POINT ( 'NONE',  ( -1.002407869896990045, 0.1264236179284866091, 1.326279527505291433 ) ) ;
#26725 = CARTESIAN_POINT ( 'NONE',  ( 0.8759842519685039353, -0.1574803149606299191, 0.6594488187901103027 ) ) ;
#26726 = ORIENTED_EDGE ( 'NONE', *, *, #16678, .F. ) ;
#26727 = CARTESIAN_POINT ( 'NONE',  ( -0.8759842519685039353, -0.1787899950787401882, 1.080216535379306952 ) ) ;
#26728 = LINE ( 'NONE', #15223, #38349 ) ;
#26729 = CARTESIAN_POINT ( 'NONE',  ( 0.8484283389429198019, 0.1740215856901604630, 0.03937008314049554591 ) ) ;
#26730 = ORIENTED_EDGE ( 'NONE', *, *, #43153, .F. ) ;
#26731 = CARTESIAN_POINT ( 'NONE',  ( 0.1797182628040039087, -0.01825247100036840597, -0.07444174185955065859 ) ) ;
#26732 = CARTESIAN_POINT ( 'NONE',  ( -0.1264236179284866091, -1.191437007820251859, -0.1264236179284866091 ) ) ;
#26733 = CARTESIAN_POINT ( 'NONE',  ( -0.8107537697050254399, -0.1574803149606297803, 1.218011811023622437 ) ) ;
#26734 = CARTESIAN_POINT ( 'NONE',  ( 0.8107537697050254399, 0.1574803149606300301, 0.5733267716535435099 ) ) ;
#26736 = CARTESIAN_POINT ( 'NONE',  ( 0.4620708661417344820, 0.6102362204724408601, 0.5167322834645649010 ) ) ;
#26735 = CARTESIAN_POINT ( 'NONE',  ( -0.9873396505805591694, 0.1113553986120547346, 0.9202755905511811330 ) ) ;
#26737 = CARTESIAN_POINT ( 'NONE',  ( 0.7747078557243284314, 0.1515708396127978252, 0.04064907242275175858 ) ) ;
#26738 = ORIENTED_EDGE ( 'NONE', *, *, #21974, .F. ) ;
#26739 = DIRECTION ( 'NONE',  ( 1.000000000000000000, 0.000000000000000000, -1.822029033848725275E-16 ) ) ;
#26740 = CARTESIAN_POINT ( 'NONE',  ( 0.9500414927467377701, 0.1787899950787401604, 0.9399606298674970661 ) ) ;
#26741 = CARTESIAN_POINT ( 'NONE',  ( 0.06523048226347956391, -0.005413385719244615847, 0.1574803149606297803 ) ) ;
#26742 = CARTESIAN_POINT ( 'NONE',  ( -0.6971942568897637749, 2.189545951927499583E-17, 1.267224409395055096 ) ) ;
#26743 = EDGE_CURVE ( 'NONE', #27963, #20645, #43828, .T. ) ;
#26744 = AXIS2_PLACEMENT_3D ( 'NONE', #12093, #11853, #45119 ) ;
#26745 = CARTESIAN_POINT ( 'NONE',  ( -1.002407869896990045, 0.1264236179284866091, 0.3469488188438744070 ) ) ;
#26746 = PLANE ( 'NONE',  #1196 ) ;
#26747 = CARTESIAN_POINT ( 'NONE',  ( 0.7646288533564489232, 0.1113553986120547346, 0.8809055117034961802 ) ) ;
#26748 = CARTESIAN_POINT ( 'NONE',  ( 0.1787899950787401882, -1.059671212323726408, -2.189545951927503898E-17 ) ) ;
#26749 = EDGE_LOOP ( 'NONE', ( #28447, #29047, #38146, #42653 ) ) ;
#26750 = CARTESIAN_POINT ( 'NONE',  ( -0.1787899950787401882, 0.07824803154982658271, 0.000000000000000000 ) ) ;
#26751 = ORIENTED_EDGE ( 'NONE', *, *, #8755, .F. ) ;
#26752 = ORIENTED_EDGE ( 'NONE', *, *, #25281, .F. ) ;
#26753 = CARTESIAN_POINT ( 'NONE',  ( -0.7185039370078739607, 1.928577636452523993E-17, 0.2559055117034968463 ) ) ;
#26754 = VECTOR ( 'NONE', #825, 39.37007874015748143 ) ;
#26755 = DIRECTION ( 'NONE',  ( 0.000000000000000000, 0.000000000000000000, -1.000000000000000000 ) ) ;
#26756 = EDGE_CURVE ( 'NONE', #43268, #10222, #19777, .T. ) ;
#26757 = AXIS2_PLACEMENT_3D ( 'NONE', #40407, #160, #26546 ) ;
#26758 = DIRECTION ( 'NONE',  ( 0.000000000000000000, 0.000000000000000000, 1.000000000000000000 ) ) ;
#26759 = CARTESIAN_POINT ( 'NONE',  ( -0.1787899950787401882, -0.6353346456155275490, 0.000000000000000000 ) ) ;
#26760 = EDGE_CURVE ( 'NONE', #8777, #25198, #38116, .T. ) ;
#26761 = CARTESIAN_POINT ( 'NONE',  ( -0.8759842519685039353, -0.1787899950787401882, 0.2140748030958428971 ) ) ;
#26762 = CARTESIAN_POINT ( 'NONE',  ( -0.8759842519685039353, -0.1574803149606299191, 0.8661417322834645827 ) ) ;
#26763 = DIRECTION ( 'NONE',  ( -1.267059173938978811E-30, -3.652049423109077687E-16, 1.000000000000000000 ) ) ;
#26764 = CARTESIAN_POINT ( 'NONE',  ( -0.1270800023317771588, -0.9902012898980059319, -0.1270800023317771588 ) ) ;
#26765 = DIRECTION ( 'NONE',  ( -0.000000000000000000, 0.000000000000000000, 1.000000000000000000 ) ) ;
#26766 = CARTESIAN_POINT ( 'NONE',  ( 0.6971942568897648851, -0.07405724077823297447, 0.9940944881352130613 ) ) ;
#26767 = CARTESIAN_POINT ( 'NONE',  ( 1.054774247047244540, 0.07405724077823318263, 1.441929133804504604 ) ) ;
#26768 = CARTESIAN_POINT ( 'NONE',  ( 0.1574803149606299191, 0.000000000000000000, -0.3149606299212598381 ) ) ;
#26769 = CARTESIAN_POINT ( 'NONE',  ( 0.9412147342319837628, 0.1574803149606300301, 1.513287401574803681 ) ) ;
#26770 = CARTESIAN_POINT ( 'NONE',  ( 0.7181698300657867184, 0.04631346878887296348, 1.982381534514537247 ) ) ;
#26771 = CARTESIAN_POINT ( 'NONE',  ( 0.8070866141732283561, 0.000000000000000000, -0.8559055118110230342 ) ) ;
#26772 = CARTESIAN_POINT ( 'NONE',  ( -0.1264236179284866091, 0.08316929139234625901, 0.1264236179284866091 ) ) ;
#26773 = LINE ( 'NONE', #16223, #15413 ) ;
#26775 = CARTESIAN_POINT ( 'NONE',  ( -1.033464566929134687, -0.06523048226347956391, 1.424704724409449064 ) ) ;
#26774 = CARTESIAN_POINT ( 'NONE',  ( 0.8759842519685039353, -0.1787899950787401882, 0.9965551180564724554 ) ) ;
#26776 = AXIS2_PLACEMENT_3D ( 'NONE', #46722, #36446, #13908 ) ;
#26777 = CARTESIAN_POINT ( 'NONE',  ( 1.002407869896990045, 0.1264236179284866091, 1.764271653489543290 ) ) ;
#26778 = CARTESIAN_POINT ( 'NONE',  ( -1.094772975963752103E-17, -0.9158464566391496531, -0.1787899950787401882 ) ) ;
#26779 = VERTEX_POINT ( 'NONE', #22028 ) ;
#26780 = CARTESIAN_POINT ( 'NONE',  ( 1.033464566929133799, 0.000000000000000000, 0.4429133858267716439 ) ) ;
#26781 = CARTESIAN_POINT ( 'NONE',  ( -0.1113553986120547346, -1.754921259734992134, -0.1113553986120547346 ) ) ;
#26782 = CARTESIAN_POINT ( 'NONE',  ( -0.7185039370078739607, 1.928577636452523993E-17, 0.05905511800270921846 ) ) ;
#26783 = CARTESIAN_POINT ( 'NONE',  ( 1.054774247047244540, -0.07405724077823318263, 1.082677165300567346 ) ) ;
#26784 = DIRECTION ( 'NONE',  ( 0.000000000000000000, 0.000000000000000000, -1.000000000000000000 ) ) ;
#26786 = AXIS2_PLACEMENT_3D ( 'NONE', #15890, #15182, #44148 ) ;
#26785 = CARTESIAN_POINT ( 'NONE',  ( 0.1113553986120547346, -1.735236220472441193, -0.1113553986120547346 ) ) ;
#26787 = EDGE_CURVE ( 'NONE', #6378, #43013, #11976, .T. ) ;
#26788 = DIRECTION ( 'NONE',  ( 0.000000000000000000, -0.4344452574044149196, 0.9006982393225888561 ) ) ;
#26789 = CARTESIAN_POINT ( 'NONE',  ( -0.8759842519685039353, -0.1574803149606299191, 0.2755905511811023723 ) ) ;
#26790 = CARTESIAN_POINT ( 'NONE',  ( -0.8759842519685039353, -0.1787899950787401882, 0.3272637794737956463 ) ) ;
#26791 = ORIENTED_EDGE ( 'NONE', *, *, #35245, .F. ) ;
#26792 = CARTESIAN_POINT ( 'NONE',  ( 0.1787899950787401882, -1.481791338528913426, -2.189545951927503898E-17 ) ) ;
#26793 = CARTESIAN_POINT ( 'NONE',  ( -0.6971942568897648851, -0.07405724077823297447, 1.855314960576157635 ) ) ;
#26794 = CARTESIAN_POINT ( 'NONE',  ( -0.8019270111902716547, -0.1787899950787401604, 0.8759842519147408302 ) ) ;
#26795 = CARTESIAN_POINT ( 'NONE',  ( -0.8019270111902717657, 0.1787899950787401604, 0.5905511810485987167 ) ) ;
#26796 = CARTESIAN_POINT ( 'NONE',  ( 0.1113553986120547346, -0.04232283453814220803, 0.1113553986120547346 ) ) ;
#26797 = CARTESIAN_POINT ( 'NONE',  ( -0.1586641775163213364, 0.9310112235910580347, -1.064878870394357468 ) ) ;
#26798 = DIRECTION ( 'NONE',  ( 0.000000000000000000, -0.000000000000000000, 1.000000000000000000 ) ) ;
#26799 = CARTESIAN_POINT ( 'NONE',  ( 0.1574803149606299746, 0.4666052258408023845, -0.7025346432751043979 ) ) ;
#26800 = CARTESIAN_POINT ( 'NONE',  ( 0.1787899950787401604, -0.5896908973630964335, 0.07405724077823318263 ) ) ;
#26801 = CARTESIAN_POINT ( 'NONE',  ( -0.05328757346823071589, -0.08955999039829311281, 0.2169276614305941098 ) ) ;
#26802 = CARTESIAN_POINT ( 'NONE',  ( -0.9873396505805591694, 0.1113553986120547346, 1.894685039262551163 ) ) ;
#26803 = CARTESIAN_POINT ( 'NONE',  ( -0.8070866141732283561, 0.000000000000000000, -0.7574803149606299524 ) ) ;
#26804 = EDGE_CURVE ( 'NONE', #29608, #26427, #35817, .T. ) ;
#26805 = ADVANCED_FACE ( 'NONE', ( #30215, #3812, #33082, #44760, #26360 ), #8115, .F. ) ;
#26806 = CARTESIAN_POINT ( 'NONE',  ( 0.2559054582636642317, -0.08442141331286162620, -0.05646086002838572593 ) ) ;
#26807 = CARTESIAN_POINT ( 'NONE',  ( -1.054774247047244540, 0.07405724077823318263, 0.4576771653005669016 ) ) ;
#26808 = CARTESIAN_POINT ( 'NONE',  ( -1.033464566929133799, 0.000000000000000000, 0.4035433070866141780 ) ) ;
#26809 = EDGE_CURVE ( 'NONE', #44045, #38514, #15914, .T. ) ;
#26810 = VECTOR ( 'NONE', #12879, 39.37007874015748143 ) ;
#26811 = CARTESIAN_POINT ( 'NONE',  ( -0.8019270111902716547, -0.1787899950787401604, 1.550196850339938148 ) ) ;
#26812 = EDGE_CURVE ( 'NONE', #24872, #32629, #44065, .T. ) ;
#26813 = CARTESIAN_POINT ( 'NONE',  ( -1.094772975963752103E-17, -1.393208661363559031, -0.1787899950787401882 ) ) ;
#26814 = VECTOR ( 'NONE', #39717, 39.37007874015748143 ) ;
#26815 = CARTESIAN_POINT ( 'NONE',  ( -0.1264236179284866091, -1.531003936954110189, 0.1264236179284866091 ) ) ;
#26816 = CARTESIAN_POINT ( 'NONE',  ( 0.7185039370078739607, 1.928577636452523993E-17, 0.8464566928058583350 ) ) ;
#26817 = CARTESIAN_POINT ( 'NONE',  ( 0.1617601974678946619, -0.07970883846569555564, 0.1380527197741285850 ) ) ;
#26818 = CARTESIAN_POINT ( 'NONE',  ( 0.7185039370078746268, -0.06523048226347956391, 0.4650590551181104093 ) ) ;
#26819 = PLANE ( 'NONE',  #7223 ) ;
#26820 = CARTESIAN_POINT ( 'NONE',  ( -0.7646288533564489232, 0.1113553986120547346, 1.156496062884598608 ) ) ;
#26821 = CARTESIAN_POINT ( 'NONE',  ( 0.8019270111902717657, -0.1787899950787401604, 0.6053149605761579677 ) ) ;
#26822 = CARTESIAN_POINT ( 'NONE',  ( 0.9500414927467377701, -0.1787899950787401604, 0.09350393695411057804 ) ) ;
#26824 = DIRECTION ( 'NONE',  ( -1.000000000000000000, -0.000000000000000000, -0.000000000000000000 ) ) ;
#26823 = CARTESIAN_POINT ( 'NONE',  ( -0.1113553986120547346, -0.3375984251968503491, 0.1113553986120547346 ) ) ;
#26825 = CARTESIAN_POINT ( 'NONE',  ( 1.033464566929133799, 0.000000000000000000, 2.007874015640504162 ) ) ;
#26826 = ORIENTED_EDGE ( 'NONE', *, *, #39484, .T. ) ;
#26827 = CARTESIAN_POINT ( 'NONE',  ( 1.033464566929133799, 0.000000000000000000, 0.04921259842519685318 ) ) ;
#26828 = CARTESIAN_POINT ( 'NONE',  ( -1.002407869896990045, -0.1264236179284866091, 1.124507873961984261 ) ) ;
#26829 = CARTESIAN_POINT ( 'NONE',  ( 0.9873396505805591694, 0.1113553986120547346, 1.117125984251968518 ) ) ;
#26830 = DIRECTION ( 'NONE',  ( 1.000000000000000000, 0.000000000000000000, -1.822029033848725275E-16 ) ) ;
#26831 = CARTESIAN_POINT ( 'NONE',  ( -9.642888182262618425E-18, -0.5393700786326299790, -0.1574803149606299191 ) ) ;
#26832 = DIRECTION ( 'NONE',  ( 1.000000000000000000, 0.000000000000000000, 0.000000000000000000 ) ) ;
#26833 = CARTESIAN_POINT ( 'NONE',  ( 0.7646288533564489232, 0.1113553986120547346, 1.274606299105070839 ) ) ;
#26834 = CARTESIAN_POINT ( 'NONE',  ( -0.1027821604407747752, -0.08956149871714005894, 0.1226111552267875882 ) ) ;
#26835 = ORIENTED_EDGE ( 'NONE', *, *, #12298, .F. ) ;
#26836 = DIRECTION ( 'NONE',  ( -1.000000000000000000, -0.000000000000000000, 0.000000000000000000 ) ) ;
#26837 = CARTESIAN_POINT ( 'NONE',  ( 0.8107537697050254399, -0.1574803149606297803, 0.8636811023622043004 ) ) ;
#26838 = ORIENTED_EDGE ( 'NONE', *, *, #41793, .T. ) ;
#26839 = CARTESIAN_POINT ( 'NONE',  ( 0.2395294000716133853, -0.1968503937007874127, -1.181102362204724310 ) ) ;
#26840 = CARTESIAN_POINT ( 'NONE',  ( -0.1574803149606297803, -0.02509842519685037340, 0.06523048226347956391 ) ) ;
#26841 = CARTESIAN_POINT ( 'NONE',  ( -0.1787899950787401604, -1.656496062938362268, -0.07405724077823318263 ) ) ;
#26842 = CARTESIAN_POINT ( 'NONE',  ( -0.07405724077823318263, -0.9183070865604088251, -0.1787899950787401604 ) ) ;
#26843 = CARTESIAN_POINT ( 'NONE',  ( -0.1574803149606299191, -1.248031496062992129, 0.000000000000000000 ) ) ;
#26844 = CARTESIAN_POINT ( 'NONE',  ( 0.9873396505805591694, 0.1113553986120547346, 1.186023621939716666 ) ) ;
#26845 = EDGE_CURVE ( 'NONE', #36464, #47458, #28210, .T. ) ;
#26846 = CARTESIAN_POINT ( 'NONE',  ( -0.7185039370078739607, 1.928577636452523993E-17, 0.06889763779527559306 ) ) ;
#26847 = CIRCLE ( 'NONE', #42088, 0.09842519685039320676 ) ;
#26848 = UNCERTAINTY_MEASURE_WITH_UNIT (LENGTH_MEASURE( 1.000000000000000082E-05 ), #44575, 'distance_accuracy_value', 'NONE') ;
#26849 = EDGE_LOOP ( 'NONE', ( #15963, #44082, #47102 ) ) ;
#26850 = EDGE_LOOP ( 'NONE', ( #32517, #41774, #8583, #7217 ) ) ;
#26851 = CARTESIAN_POINT ( 'NONE',  ( -0.6971942568897648851, -0.07405724077823297447, 1.702755905458047003 ) ) ;
#26852 = VERTEX_POINT ( 'NONE', #205 ) ;
#26853 = CARTESIAN_POINT ( 'NONE',  ( -0.06073293532415852819, -0.2604299181697397603, -0.3083162604245307525 ) ) ;
#26854 = CARTESIAN_POINT ( 'NONE',  ( 0.8019270111902717657, -0.1787899950787401604, 0.3690944881352128393 ) ) ;
#26855 = AXIS2_PLACEMENT_3D ( 'NONE', #23574, #45116, #5832 ) ;
#26856 = CARTESIAN_POINT ( 'NONE',  ( -0.8019270111902717657, 0.1787899950787401604, 1.451771653489543290 ) ) ;
#26857 = CARTESIAN_POINT ( 'NONE',  ( -0.7646288533564489232, 0.1113553986120547346, 1.510826771546015523 ) ) ;
#26858 = CARTESIAN_POINT ( 'NONE',  ( -1.054774247047244540, -0.07405724077823318263, 1.279527559001355730 ) ) ;
#26859 = AXIS2_PLACEMENT_3D ( 'NONE', #28158, #39144, #35110 ) ;
#26860 = CARTESIAN_POINT ( 'NONE',  ( -0.6971942568897626646, 0.07405724077823318263, 0.08366141726907129483 ) ) ;
#26861 = CYLINDRICAL_SURFACE ( 'NONE', #1540, 0.1377952755905511306 ) ;
#26862 = CARTESIAN_POINT ( 'NONE',  ( -0.6971942568897637749, 2.189545951927499583E-17, 1.739665354276945131 ) ) ;
#26863 = CARTESIAN_POINT ( 'NONE',  ( -1.033464566929133799, 0.000000000000000000, 2.007874015640504162 ) ) ;
#26864 = CARTESIAN_POINT ( 'NONE',  ( -1.033464566929134687, 0.06523048226347956391, 1.744586614173228467 ) ) ;
#26865 = EDGE_CURVE ( 'NONE', #40961, #21477, #46513, .T. ) ;
#26866 = CARTESIAN_POINT ( 'NONE',  ( 0.6971942568897648851, 0.07405724077823318263, 1.540354330654897685 ) ) ;
#26867 = CARTESIAN_POINT ( 'NONE',  ( -0.2086866875178732261, -0.09842519685039370636, -0.1330263174222271749 ) ) ;
#26868 = FACE_OUTER_BOUND ( 'NONE', #44989, .T. ) ;
#26869 = EDGE_CURVE ( 'NONE', #28934, #3606, #14854, .T. ) ;
#26870 = ORIENTED_EDGE ( 'NONE', *, *, #13885, .F. ) ;
#26871 = CARTESIAN_POINT ( 'NONE',  ( -0.8759842519685039353, -0.1787899950787401882, 1.158956692859621995 ) ) ;
#26872 = ORIENTED_EDGE ( 'NONE', *, *, #28769, .T. ) ;
#26873 = CARTESIAN_POINT ( 'NONE',  ( 3.284318927891251994E-17, -0.8617125983714329918, 0.1787899950787401882 ) ) ;
#26874 = CARTESIAN_POINT ( 'NONE',  ( 0.1787899950787401604, -1.120078740103715997, -0.07405724077823318263 ) ) ;
#26875 = VECTOR ( 'NONE', #34205, 39.37007874015748143 ) ;
#26876 = EDGE_CURVE ( 'NONE', #43147, #37245, #41910, .T. ) ;
#26877 = PRODUCT_RELATED_PRODUCT_CATEGORY ( 'part', '', ( #9398 ) ) ;
#26878 = DIRECTION ( 'NONE',  ( -1.000000000000000000, 0.000000000000000000, 0.000000000000000000 ) ) ;
#26879 = CARTESIAN_POINT ( 'NONE',  ( -0.1270800023317771588, -0.3898075891106047575, 0.1270800023317771588 ) ) ;
#26880 = CARTESIAN_POINT ( 'NONE',  ( 0.1113553986120547346, 0.1053149606299212532, 0.1113553986120547346 ) ) ;
#26881 = AXIS2_PLACEMENT_3D ( 'NONE', #27277, #34926, #41827 ) ;
#26882 = DIRECTION ( 'NONE',  ( 1.000000000000000000, 0.000000000000000000, 0.000000000000000000 ) ) ;
#26883 = CARTESIAN_POINT ( 'NONE',  ( 1.054774247047244540, -0.07405724077823318263, 0.8464566928596233275 ) ) ;
#26884 = AXIS2_PLACEMENT_3D ( 'NONE', #16113, #27148, #16574 ) ;
#26886 = CARTESIAN_POINT ( 'NONE',  ( -6.669550765781891660E-19, 0.1126122229446088890, 0.08054045948776612784 ) ) ;
#26885 = DIRECTION ( 'NONE',  ( -1.000000000000000000, 0.000000000000000000, 0.000000000000000000 ) ) ;
#26887 = CARTESIAN_POINT ( 'NONE',  ( 0.7185039370078739607, 1.928577636452523993E-17, 0.09842519674286673292 ) ) ;
#26888 = CARTESIAN_POINT ( 'NONE',  ( 0.9873396505805591694, 0.1113553986120547346, 0.1722440944881890035 ) ) ;
#26889 = CARTESIAN_POINT ( 'NONE',  ( 0.000000000000000000, 0.09842519685039370636, 0.000000000000000000 ) ) ;
#26891 = CARTESIAN_POINT ( 'NONE',  ( 0.07405724077823318263, -0.4261811023084413064, 0.1787899950787401604 ) ) ;
#26890 = CARTESIAN_POINT ( 'NONE',  ( 0.06523048226347956391, -0.9896653542231822476, 0.1574803149606297803 ) ) ;
#26892 = DIRECTION ( 'NONE',  ( -0.000000000000000000, -0.000000000000000000, -1.000000000000000000 ) ) ;
#26893 = CARTESIAN_POINT ( 'NONE',  ( 0.1787899950787401604, -1.243110236166709459, 0.07405724077823318263 ) ) ;
#26894 = CARTESIAN_POINT ( 'NONE',  ( 1.002407869896990045, 0.1264236179284866091, 0.3075787401037169411 ) ) ;
#26895 = CARTESIAN_POINT ( 'NONE',  ( -0.9500414927467378812, 0.1787899950787401604, 1.683070866087970074 ) ) ;
#26896 = VERTEX_POINT ( 'NONE', #22256 ) ;
#26897 = CARTESIAN_POINT ( 'NONE',  ( -1.054774247047244540, 0.07405724077823318263, 1.368110236166710125 ) ) ;
#26898 = CARTESIAN_POINT ( 'NONE',  ( -0.9412147342319837628, 0.1574803149606300301, 1.316437007874015519 ) ) ;
#26899 = CARTESIAN_POINT ( 'NONE',  ( 0.9500414927467378812, -0.1787899950787401604, 1.318897637741511364 ) ) ;
#26900 = CARTESIAN_POINT ( 'NONE',  ( -0.8019270111902717657, 0.1787899950787401604, 1.215551181048599272 ) ) ;
#26901 = EDGE_CURVE ( 'NONE', #19079, #22837, #11491, .T. ) ;
#26902 = CARTESIAN_POINT ( 'NONE',  ( 1.033464566929133799, 0.000000000000000000, 1.535433070758614127 ) ) ;
#26903 = CARTESIAN_POINT ( 'NONE',  ( -0.1190585826237822442, -0.09842520615623508162, -0.1333826362739909122 ) ) ;
#26904 = CARTESIAN_POINT ( 'NONE',  ( 2.892866454678787531E-17, 0.06102362204724409711, 0.1574803149606299191 ) ) ;
#26905 = CARTESIAN_POINT ( 'NONE',  ( 0.9500414927467377701, -0.1787899950787401604, 0.4527559054580477249 ) ) ;
#26906 = CARTESIAN_POINT ( 'NONE',  ( -1.054774247047244096, 0.000000000000000000, 0.3764763778989925203 ) ) ;
#26907 = VERTEX_POINT ( 'NONE', #4265 ) ;
#26908 = AXIS2_PLACEMENT_3D ( 'NONE', #27436, #41978, #46065 ) ;
#26909 = CYLINDRICAL_SURFACE ( 'NONE', #26786, 0.09842519685039370636 ) ;
#26910 = ORIENTED_EDGE ( 'NONE', *, *, #14466, .T. ) ;
#26911 = ORIENTED_EDGE ( 'NONE', *, *, #42538, .F. ) ;
#26912 = CARTESIAN_POINT ( 'NONE',  ( -0.7185039370078739607, 1.928577636452523993E-17, 0.2263779527559055260 ) ) ;
#26913 = EDGE_CURVE ( 'NONE', #2855, #860, #18240, .T. ) ;
#26914 = CARTESIAN_POINT ( 'NONE',  ( 0.6971942568897648851, -0.07405724077823297447, 1.151574803095843036 ) ) ;
#26915 = CARTESIAN_POINT ( 'NONE',  ( -0.7495606340400177148, -0.1264236179284866091, 1.975885826717889815 ) ) ;
#26916 = CARTESIAN_POINT ( 'NONE',  ( -1.033464566929133799, 0.000000000000000000, 1.978346456692913646 ) ) ;
#26917 = CIRCLE ( 'NONE', #22300, 0.2471922904502826812 ) ;
#26918 = VERTEX_POINT ( 'NONE', #42107 ) ;
#26919 = CIRCLE ( 'NONE', #13892, 0.02900000000000001882 ) ;
#26920 = CARTESIAN_POINT ( 'NONE',  ( 1.054774247047244096, 0.000000000000000000, 1.990649606245448844 ) ) ;
#26921 = AXIS2_PLACEMENT_3D ( 'NONE', #25818, #40397, #7583 ) ;
#26922 = CARTESIAN_POINT ( 'NONE',  ( -0.7495606340400177148, 0.1264236179284866091, 0.9473425196312755814 ) ) ;
#26923 = CARTESIAN_POINT ( 'NONE',  ( -0.8759842519685039353, -0.1574803149606299191, 0.3149606299212598381 ) ) ;
#26924 = CARTESIAN_POINT ( 'NONE',  ( 1.033464566929134687, -0.06523048226347956391, 0.3223425196850392971 ) ) ;
#26925 = CARTESIAN_POINT ( 'NONE',  ( -0.07405724077823318263, -1.480438928859160619, -0.1787899950787401604 ) ) ;
#26926 = ORIENTED_EDGE ( 'NONE', *, *, #6371, .F. ) ;
#26927 = CARTESIAN_POINT ( 'NONE',  ( -0.1787899950787401882, -0.4729330708123779536, 0.000000000000000000 ) ) ;
#26928 = CARTESIAN_POINT ( 'NONE',  ( 0.2871444924769515628, 0.9382165298418956301, -1.070508272602716637 ) ) ;
#26929 = ORIENTED_EDGE ( 'NONE', *, *, #22082, .F. ) ;
#26930 = CARTESIAN_POINT ( 'NONE',  ( 0.9500414927467378812, -0.1787899950787401604, 1.313976377898992132 ) ) ;
#26931 = CARTESIAN_POINT ( 'NONE',  ( 0.7185039370078739607, 1.928577636452523993E-17, 0.8956692913385826404 ) ) ;
#26932 = CARTESIAN_POINT ( 'NONE',  ( -0.8759842519685039353, 0.000000000000000000, 0.000000000000000000 ) ) ;
#26933 = CARTESIAN_POINT ( 'NONE',  ( 0.003857550520879598089, -0.09763768210237290524, -0.1064941629723520911 ) ) ;
#26934 = CARTESIAN_POINT ( 'NONE',  ( 0.6971942568897637749, 2.189545951927499583E-17, 1.577263779473795369 ) ) ;
#26935 = CARTESIAN_POINT ( 'NONE',  ( 1.054774247047244540, -0.07405724077823318263, 0.1377952755367876370 ) ) ;
#26936 = CARTESIAN_POINT ( 'NONE',  ( 0.07405724077823318263, -1.710629921206078041, -0.1787899950787401604 ) ) ;
#26937 = CARTESIAN_POINT ( 'NONE',  ( -0.8107537697050254399, 0.1574803149606300301, 1.744586614065703145 ) ) ;
#26938 = AXIS2_PLACEMENT_3D ( 'NONE', #859, #156, #19078 ) ;
#26939 = CARTESIAN_POINT ( 'NONE',  ( -0.9500414927467377701, 0.1787899950787401604, 0.6249999999462356737 ) ) ;
#26941 = DIRECTION ( 'NONE',  ( 1.822029033848725028E-16, 0.000000000000000000, 1.000000000000000000 ) ) ;
#26940 = CARTESIAN_POINT ( 'NONE',  ( 0.1113553986120547346, -0.7116141732283465249, -0.1113553986120547346 ) ) ;
#26942 = CARTESIAN_POINT ( 'NONE',  ( 0.1270800023317771588, -1.590594990685407328, -0.1270800023317771588 ) ) ;
#26943 = CARTESIAN_POINT ( 'NONE',  ( -0.7646288533564489232, -0.1113553986120547346, 1.599409448711369919 ) ) ;
#26944 = DIRECTION ( 'NONE',  ( -1.000000000000000000, 0.000000000000000000, 0.000000000000000000 ) ) ;
#26945 = CARTESIAN_POINT ( 'NONE',  ( 0.6971942568897648851, -0.07405724077823297447, 1.309055118056472899 ) ) ;
#26946 = CARTESIAN_POINT ( 'NONE',  ( 0.6971942568897637749, 2.189545951927499583E-17, 1.774114173174582643 ) ) ;
#26947 = APPLICATION_CONTEXT ( 'automotive_design' ) ;
#26948 = ORIENTED_EDGE ( 'NONE', *, *, #38948, .F. ) ;
#26949 = CIRCLE ( 'NONE', #5514, 0.1574803149606299191 ) ;
#26950 = CIRCLE ( 'NONE', #12421, 0.08090551181102362266 ) ;
#26952 = ORIENTED_EDGE ( 'NONE', *, *, #9535, .F. ) ;
#26951 = DIRECTION ( 'NONE',  ( 0.000000000000000000, 1.000000000000000000, 0.000000000000000000 ) ) ;
#26953 = CARTESIAN_POINT ( 'NONE',  ( -0.7646288533564489232, 0.1113553986120547346, 1.520669291338582640 ) ) ;
#26954 = CARTESIAN_POINT ( 'NONE',  ( 0.000000000000000000, 0.4003652867858630282, 0.7276473417831955670 ) ) ;
#26956 = CARTESIAN_POINT ( 'NONE',  ( 0.1264236179284866091, 0.09793307091990532953, -0.1264236179284866091 ) ) ;
#26955 = CARTESIAN_POINT ( 'NONE',  ( 0.1113553986120547346, -0.8592519683964094934, -0.1113553986120547346 ) ) ;
#26957 = CARTESIAN_POINT ( 'NONE',  ( 0.8759842519685039353, -0.1574803149606299191, 0.5019685038294811052 ) ) ;
#26958 = CARTESIAN_POINT ( 'NONE',  ( 1.054774247047244540, -0.07405724077823318263, 0.4921259841982048577 ) ) ;
#26959 = CARTESIAN_POINT ( 'NONE',  ( -0.8075642815980649258, 0.1651804164989427171, 0.03937007874015843040 ) ) ;
#26960 = DIRECTION ( 'NONE',  ( 1.822029033848725028E-16, 0.000000000000000000, 1.000000000000000000 ) ) ;
#26961 = CARTESIAN_POINT ( 'NONE',  ( -0.8759842519685039353, -0.1787899950787401882, 1.311515747977732405 ) ) ;
#26962 = CARTESIAN_POINT ( 'NONE',  ( 0.8759842519685039353, -0.1574803149606299191, 0.8562992124908976876 ) ) ;
#26963 = VERTEX_POINT ( 'NONE', #15810 ) ;
#26964 = CARTESIAN_POINT ( 'NONE',  ( -1.002407869896990045, -0.1264236179284866091, 1.085137795221826629 ) ) ;
#26965 = CARTESIAN_POINT ( 'NONE',  ( 1.033464566929133799, 0.000000000000000000, 0.6791338582677166613 ) ) ;
#26966 = ORIENTED_EDGE ( 'NONE', *, *, #2630, .T. ) ;
#26967 = CARTESIAN_POINT ( 'NONE',  ( -0.7646288533564489232, -0.1113553986120547346, 0.5757874014672763607 ) ) ;
#26968 = DIRECTION ( 'NONE',  ( 1.000000000000000000, -3.469446951953626022E-15, -0.000000000000000000 ) ) ;
#26969 = CARTESIAN_POINT ( 'NONE',  ( 1.054774247047244096, 0.000000000000000000, 1.636318897584031484 ) ) ;
#26970 = CARTESIAN_POINT ( 'NONE',  ( -1.033464566929134687, 0.06523048226347956391, 1.272145669291338432 ) ) ;
#26971 = ADVANCED_FACE ( 'NONE', ( #38543 ), #9555, .T. ) ;
#26972 = CARTESIAN_POINT ( 'NONE',  ( -0.7185039370078739607, 1.928577636452523993E-17, 1.043307086506645831 ) ) ;
#26974 = CARTESIAN_POINT ( 'NONE',  ( 0.7646288533564489232, 0.1113553986120547346, 1.953740157480315043 ) ) ;
#26973 = LINE ( 'NONE', #5366, #32654 ) ;
#26975 = CARTESIAN_POINT ( 'NONE',  ( 0.9412147342319837628, -0.1574803149606297803, 1.449311023514519681 ) ) ;
#26976 = ORIENTED_EDGE ( 'NONE', *, *, #25166, .T. ) ;
#26977 = ORIENTED_EDGE ( 'NONE', *, *, #21262, .T. ) ;
#26978 = EDGE_CURVE ( 'NONE', #7386, #26132, #31376, .T. ) ;
#26979 = CARTESIAN_POINT ( 'NONE',  ( -0.03598878106637547203, -0.09842522444525984848, 0.1542999736886214723 ) ) ;
#26980 = ORIENTED_EDGE ( 'NONE', *, *, #36217, .F. ) ;
#26981 = EDGE_CURVE ( 'NONE', #36211, #42479, #16738, .T. ) ;
#26982 = CARTESIAN_POINT ( 'NONE',  ( -0.9500414927467377701, -0.1787899950787401604, 1.589566929080094226 ) ) ;
#26983 = CARTESIAN_POINT ( 'NONE',  ( -0.1574803149606297803, -0.05462598414444141265, 0.06523048226347956391 ) ) ;
#26984 = CARTESIAN_POINT ( 'NONE',  ( -0.9500414927467378812, -0.1787899950787401604, 1.318897637741511364 ) ) ;
#26985 = VERTEX_POINT ( 'NONE', #20088 ) ;
#26986 = EDGE_CURVE ( 'NONE', #41944, #7400, #38068, .T. ) ;
#26987 = AXIS2_PLACEMENT_3D ( 'NONE', #39804, #46768, #44118 ) ;
#26988 = ( BOUNDED_CURVE ( )  B_SPLINE_CURVE ( 2, ( #16102, #7941, #15630, #41686, #22557, #8890, #18952, #19192, #33852 ),
 .UNSPECIFIED., .F., .T. ) 
 B_SPLINE_CURVE_WITH_KNOTS ( ( 3, 2, 2, 2, 3 ),
 ( 0.6300000000000000044, 0.6324999999999999512, 0.6350000000000000089, 0.6374999999999999556, 0.6400000000000000133 ),
 .UNSPECIFIED. ) 
 CURVE ( )  GEOMETRIC_REPRESENTATION_ITEM ( )  RATIONAL_B_SPLINE_CURVE ( ( 1.000000000000000000, 0.9238795325112869605, 1.000000000000000000, 0.9238795325112869605, 1.000000000000000000, 0.9238795325112869605, 1.000000000000000000, 0.9238795325112869605, 1.000000000000000000 ) ) 
 REPRESENTATION_ITEM ( '' )  ) ;
#26989 = AXIS2_PLACEMENT_3D ( 'NONE', #41390, #8590, #31143 ) ;
#26990 = CARTESIAN_POINT ( 'NONE',  ( -0.1184675242425147629, -0.5708661417322835607, 1.713085361781126803 ) ) ;
#26991 = CARTESIAN_POINT ( 'NONE',  ( -0.6971942568897626646, -0.07405724077823297447, 0.3641732282926931630 ) ) ;
#26992 = CARTESIAN_POINT ( 'NONE',  ( 0.8107537697050254399, 0.1574803149606300301, 1.862696850286174710 ) ) ;
#26993 = CARTESIAN_POINT ( 'NONE',  ( 0.9412147342319837628, 0.1574803149606300301, 0.8735236219397174429 ) ) ;
#26994 = CARTESIAN_POINT ( 'NONE',  ( 3.284318927891251994E-17, -1.030143653268608128, 0.1787899950787401882 ) ) ;
#26995 = ORIENTED_EDGE ( 'NONE', *, *, #11594, .F. ) ;
#26996 = CARTESIAN_POINT ( 'NONE',  ( -0.1264236179284866091, -0.005413385773008149403, -0.1264236179284866091 ) ) ;
#26997 = ORIENTED_EDGE ( 'NONE', *, *, #30136, .T. ) ;
#26998 = ORIENTED_EDGE ( 'NONE', *, *, #4210, .T. ) ;
#26999 = AXIS2_PLACEMENT_3D ( 'NONE', #46079, #2002, #13281 ) ;
#27000 = CARTESIAN_POINT ( 'NONE',  ( 0.8107537697050254399, 0.1574803149606300301, 1.744586614065703145 ) ) ;
#27001 = DIRECTION ( 'NONE',  ( 0.000000000000000000, 1.000000000000000000, 0.000000000000000000 ) ) ;
#27002 = CARTESIAN_POINT ( 'NONE',  ( 0.07405724077823318263, -0.6476377952218281830, -0.1787899950787401604 ) ) ;
#27003 = ( BOUNDED_CURVE ( )  B_SPLINE_CURVE ( 2, ( #26965, #19508, #18795, #14995, #4641, #11864, #26489, #41051, #22875 ),
 .UNSPECIFIED., .F., .T. ) 
 B_SPLINE_CURVE_WITH_KNOTS ( ( 3, 2, 2, 2, 3 ),
 ( 0.3400000000000000244, 0.3425000000000000266, 0.3449999999999999734, 0.3474999999999999756, 0.3499999999999999778 ),
 .UNSPECIFIED. ) 
 CURVE ( )  GEOMETRIC_REPRESENTATION_ITEM ( )  RATIONAL_B_SPLINE_CURVE ( ( 1.000000000000000000, 0.9238795325112869605, 1.000000000000000000, 0.9238795325112869605, 1.000000000000000000, 0.9238795325112869605, 1.000000000000000000, 0.9238795325112849621, 1.000000000000000000 ) ) 
 REPRESENTATION_ITEM ( '' )  ) ;
#27004 = CARTESIAN_POINT ( 'NONE',  ( -1.054774247047244540, -0.07405724077823318263, 0.2608267715997797387 ) ) ;
#27005 = CARTESIAN_POINT ( 'NONE',  ( -0.8107537697050253289, 0.1574803149606300301, 0.9670275590551186129 ) ) ;
#27006 = LINE ( 'NONE', #26525, #30050 ) ;
#27007 = LINE ( 'NONE', #34194, #33286 ) ;
#27008 = CARTESIAN_POINT ( 'NONE',  ( 0.1270800023317771588, -1.088626486748399680, 0.1270800023317771588 ) ) ;
#27009 = CARTESIAN_POINT ( 'NONE',  ( 0.1442072231542519400, 0.1299212598425196763, -0.08784906043161684608 ) ) ;
#27010 = CARTESIAN_POINT ( 'NONE',  ( 0.9500414927467378812, 0.1787899950787401604, 0.8612204723871809131 ) ) ;
#27011 = CARTESIAN_POINT ( 'NONE',  ( 0.8759842519685039353, -0.1787899950787401882, 1.429625984198204858 ) ) ;
#27012 = CARTESIAN_POINT ( 'NONE',  ( 0.6971942568897626646, 0.07405724077823318263, 0.1181102361667090567 ) ) ;
#27013 = DIRECTION ( 'NONE',  ( 0.000000000000000000, 1.000000000000000000, 0.000000000000000000 ) ) ;
#27014 = CARTESIAN_POINT ( 'NONE',  ( 0.8759842519685039353, -0.1574803149606299191, 1.574803149606299302 ) ) ;
#27016 = DIRECTION ( 'NONE',  ( 6.679788269418529283E-17, -1.000000000000000000, 0.000000000000000000 ) ) ;
#27015 = CARTESIAN_POINT ( 'NONE',  ( 0.7462404686856282110, -0.1095783846369325631, 1.985475001373030901 ) ) ;
#27017 = CARTESIAN_POINT ( 'NONE',  ( 0.5057057357416000487, -3.032960542342102697E-32, 0.09842519685039370636 ) ) ;
#27018 = AXIS2_PLACEMENT_3D ( 'NONE', #8580, #41380, #44987 ) ;
#27019 = CARTESIAN_POINT ( 'NONE',  ( 0.1574803149606300023, 0.3648440108500931589, -3.619166627704266670 ) ) ;
#27020 = CARTESIAN_POINT ( 'NONE',  ( 1.054774247047244096, 0.000000000000000000, 1.045767716481669440 ) ) ;
#27021 = CARTESIAN_POINT ( 'NONE',  ( 0.6971942568897637749, 2.189545951927499583E-17, 1.779035433017102319 ) ) ;
#27022 = CARTESIAN_POINT ( 'NONE',  ( 0.7646288533564489232, 0.1113553986120547346, 0.3297244093412917687 ) ) ;
#27023 = ORIENTED_EDGE ( 'NONE', *, *, #26812, .T. ) ;
#27024 = CARTESIAN_POINT ( 'NONE',  ( 0.000000000000000000, -0.09842519685039370636, 0.000000000000000000 ) ) ;
#27025 = ( GEOMETRIC_REPRESENTATION_CONTEXT ( 3 ) GLOBAL_UNCERTAINTY_ASSIGNED_CONTEXT ( ( #2936 ) ) GLOBAL_UNIT_ASSIGNED_CONTEXT ( ( #19423, #19894, #30259 ) ) REPRESENTATION_CONTEXT ( 'NONE', 'WORKASPACE' ) ) ;
#27027 = DIRECTION ( 'NONE',  ( 1.000000000000000000, 0.000000000000000000, -4.336808689942014778E-16 ) ) ;
#27026 = AXIS2_PLACEMENT_3D ( 'NONE', #11096, #25719, #502 ) ;
#27028 = CARTESIAN_POINT ( 'NONE',  ( -0.1574803149606299191, -1.671259842412157415, 0.000000000000000000 ) ) ;
#27029 = CARTESIAN_POINT ( 'NONE',  ( -0.7185039370078746268, -0.06523048226347956391, 0.1402559054042841202 ) ) ;
#27030 = CARTESIAN_POINT ( 'NONE',  ( 0.9500414927467378812, 0.1787899950787401604, 1.131889763725763665 ) ) ;
#27031 = CARTESIAN_POINT ( 'NONE',  ( -1.033464566929134687, 0.06523048226347956391, 1.035925196850394192 ) ) ;
#27032 = CARTESIAN_POINT ( 'NONE',  ( -0.1574803149606297803, -1.757381889763778959, 0.06523048226347956391 ) ) ;
#27033 = DIRECTION ( 'NONE',  ( 0.000000000000000000, -1.000000000000000000, 0.000000000000000000 ) ) ;
#27034 = EDGE_CURVE ( 'NONE', #24360, #28387, #36615, .T. ) ;
#27035 = CARTESIAN_POINT ( 'NONE',  ( -0.8019270111902717657, -0.1787899950787401604, 0.5610236219934807700 ) ) ;
#27036 = CARTESIAN_POINT ( 'NONE',  ( 0.9873396505805591694, 0.1113553986120547346, 0.2509842519685039353 ) ) ;
#27037 = CARTESIAN_POINT ( 'NONE',  ( -0.7495606340400177148, -0.1264236179284866091, 0.3223425196312759144 ) ) ;
#27038 = ORIENTED_EDGE ( 'NONE', *, *, #24684, .F. ) ;
#27040 = CARTESIAN_POINT ( 'NONE',  ( 0.1264236179284866091, -1.604822834591905556, 0.1264236179284866091 ) ) ;
#27039 = CARTESIAN_POINT ( 'NONE',  ( -0.1113553986120547346, -0.3671259841444414196, 0.1113553986120547346 ) ) ;
#27041 = ADVANCED_FACE ( 'NONE', ( #27320 ), #5708, .F. ) ;
#27042 = CARTESIAN_POINT ( 'NONE',  ( -1.054774247047244540, -0.07405724077823318263, 0.5757874015210394658 ) ) ;
#27043 = DIRECTION ( 'NONE',  ( 0.000000000000000000, -0.9771240687918510970, -0.2126700594528006527 ) ) ;
#27044 = CARTESIAN_POINT ( 'NONE',  ( 0.4755220087074803481, -0.09842519685039370636, 1.205361022782828805E-17 ) ) ;
#27045 = CARTESIAN_POINT ( 'NONE',  ( -0.2066929133858267931, -0.2274162997038020051, -0.9219983537151217323 ) ) ;
#27046 = CARTESIAN_POINT ( 'NONE',  ( -0.1787899950787401882, -0.5281751493316008128, 0.000000000000000000 ) ) ;
#27047 = CARTESIAN_POINT ( 'NONE',  ( 0.1549696564520381958, -0.08956042623435592209, -0.1209032005300702678 ) ) ;
#27048 = CARTESIAN_POINT ( 'NONE',  ( 0.8107537697050254399, -0.1574803149606297803, 1.926673228346456490 ) ) ;
#27049 = PLANE ( 'NONE',  #43218 ) ;
#27050 = CARTESIAN_POINT ( 'NONE',  ( 0.2559054708194526406, -0.07549683194480610871, -0.05060588599970165802 ) ) ;
#27051 = CARTESIAN_POINT ( 'NONE',  ( -0.8019270111902717657, 0.1787899950787401604, 0.4675196849856070869 ) ) ;
#27052 = CARTESIAN_POINT ( 'NONE',  ( -0.9873396505805591694, -0.1113553986120547346, 0.3986220472440945017 ) ) ;
#27053 = VECTOR ( 'NONE', #19844, 39.37007874015748854 ) ;
#27054 = ORIENTED_EDGE ( 'NONE', *, *, #36697, .F. ) ;
#27055 = CARTESIAN_POINT ( 'NONE',  ( 0.2471918495545273320, -0.09442133267706712130, 0.03395794428076722576 ) ) ;
#27056 = VECTOR ( 'NONE', #35018, 39.37007874015748854 ) ;
#27057 = CARTESIAN_POINT ( 'NONE',  ( 0.1264236179284866091, -1.565452755851747924, 0.1264236179284866091 ) ) ;
#27058 = VERTEX_POINT ( 'NONE', #34479 ) ;
#27059 = CARTESIAN_POINT ( 'NONE',  ( -0.1787899950787401604, -1.612204724355685403, 0.07405724077823318263 ) ) ;
#27060 = CIRCLE ( 'NONE', #6359, 0.4724409448818900348 ) ;
#27061 = CARTESIAN_POINT ( 'NONE',  ( 0.7646288533564489232, -0.1113553986120547346, 0.1919291338582677087 ) ) ;
#27062 = CARTESIAN_POINT ( 'NONE',  ( 0.8107537697050254399, 0.1574803149606300301, 0.9670275590551187239 ) ) ;
#27063 = CARTESIAN_POINT ( 'NONE',  ( 1.033464566929134687, 0.06523048226347956391, 0.4453740157480309270 ) ) ;
#27064 = CARTESIAN_POINT ( 'NONE',  ( 0.000000000000000000, 1.205361022782826802E-17, -0.09842519685039370636 ) ) ;
#27065 = CARTESIAN_POINT ( 'NONE',  ( -1.033464566929133799, 0.000000000000000000, 1.299212598317669221 ) ) ;
#27066 = CARTESIAN_POINT ( 'NONE',  ( 0.8019270111902717657, -0.1787899950787401604, 0.5265748030958428139 ) ) ;
#27067 = CARTESIAN_POINT ( 'NONE',  ( 0.6971942568897637749, 2.189545951927499583E-17, 0.08120078734781142893 ) ) ;
#27069 = DIRECTION ( 'NONE',  ( 1.000000000000000000, 0.000000000000000000, -1.822029033848725275E-16 ) ) ;
#27068 = CARTESIAN_POINT ( 'NONE',  ( -0.1113553986120547346, -0.4655511811023622104, -0.1113553986120547346 ) ) ;
#27070 = CARTESIAN_POINT ( 'NONE',  ( -0.7646288533564489232, 0.1113553986120547346, 1.195866141624756018 ) ) ;
#27071 = EDGE_LOOP ( 'NONE', ( #24911, #20242, #36388, #37066 ) ) ;
#27072 = LINE ( 'NONE', #16506, #27722 ) ;
#27073 = CARTESIAN_POINT ( 'NONE',  ( -1.054774247047244540, -0.07405724077823318263, 1.087598425143086578 ) ) ;
#27074 = CARTESIAN_POINT ( 'NONE',  ( 0.8759842519685039353, 0.1574803149606299191, 1.161417322834645605 ) ) ;
#27075 = DIRECTION ( 'NONE',  ( 1.217491584052838080E-15, 0.6156614753256588468, 0.7880107536067214591 ) ) ;
#27076 = CARTESIAN_POINT ( 'NONE',  ( -0.9873396505805591694, 0.1113553986120547346, 0.7135826770578268530 ) ) ;
#27077 = DIRECTION ( 'NONE',  ( 0.000000000000000000, -1.000000000000000000, 0.000000000000000000 ) ) ;
#27078 = DIRECTION ( 'NONE',  ( 0.000000000000000000, -1.000000000000000000, 0.000000000000000000 ) ) ;
#27079 = CARTESIAN_POINT ( 'NONE',  ( 1.033464566929133799, 0.000000000000000000, 0.3543307085538902057 ) ) ;
#27080 = CARTESIAN_POINT ( 'NONE',  ( -0.1787899950787401882, -0.5516732282926929409, 0.000000000000000000 ) ) ;
#27081 = FACE_OUTER_BOUND ( 'NONE', #45358, .T. ) ;
#27082 = ORIENTED_EDGE ( 'NONE', *, *, #23162, .T. ) ;
#27083 = CARTESIAN_POINT ( 'NONE',  ( -0.3980944881889753040, 0.4370297686271548687, 0.6367018223237034258 ) ) ;
#27084 = CARTESIAN_POINT ( 'NONE',  ( -0.8759842519685039353, 0.1574803149606299191, 1.122047244094488194 ) ) ;
#27085 = VECTOR ( 'NONE', #32376, 39.37007874015748143 ) ;
#27086 = EDGE_LOOP ( 'NONE', ( #14222, #32136, #30114, #28793, #357, #23118, #15815 ) ) ;
#27087 = LINE ( 'NONE', #22988, #20304 ) ;
#27088 = DIRECTION ( 'NONE',  ( -1.000000000000000000, 0.000000000000000000, 0.000000000000000000 ) ) ;
#27089 = CARTESIAN_POINT ( 'NONE',  ( -0.1264236179284866091, -1.649114173174582643, 0.1264236179284866091 ) ) ;
#27090 = CARTESIAN_POINT ( 'NONE',  ( -1.094772975963752103E-17, -0.8813976377415118080, -0.1787899950787401882 ) ) ;
#27091 = CARTESIAN_POINT ( 'NONE',  ( -0.06523048226347956391, -1.294783464566929165, -0.1574803149606300301 ) ) ;
#27092 = CARTESIAN_POINT ( 'NONE',  ( 0.9873396505805591694, 0.1113553986120547346, 1.146653543199559033 ) ) ;
#27093 = CARTESIAN_POINT ( 'NONE',  ( 0.1637370714319410780, 0.07819377357278597951, -0.1401549625175002034 ) ) ;
#27094 = EDGE_CURVE ( 'NONE', #28164, #40149, #42695, .T. ) ;
#27095 = CARTESIAN_POINT ( 'NONE',  ( -1.054774247047244096, 0.000000000000000000, 0.4552165353793071745 ) ) ;
#27096 = ORIENTED_EDGE ( 'NONE', *, *, #31462, .T. ) ;
#27097 = ORIENTED_EDGE ( 'NONE', *, *, #39010, .F. ) ;
#27098 = CARTESIAN_POINT ( 'NONE',  ( -0.7495606340400177148, -0.1264236179284866091, 1.823326771599779406 ) ) ;
#27099 = CARTESIAN_POINT ( 'NONE',  ( 0.7495606340400177148, -0.1264236179284866091, 1.862696850339937038 ) ) ;
#27100 = EDGE_LOOP ( 'NONE', ( #11633, #34124, #7506, #28698 ) ) ;
#27101 = CARTESIAN_POINT ( 'NONE',  ( 0.06523048226347956391, -1.383366141624756018, 0.1574803149606297803 ) ) ;
#27102 = CARTESIAN_POINT ( 'NONE',  ( -1.054774247047244540, -0.07405724077823318263, 0.8907480314422986378 ) ) ;
#27104 = CARTESIAN_POINT ( 'NONE',  ( 0.06523048226347956391, -0.005413385719244616714, 0.1574803149606297803 ) ) ;
#27103 = TOROIDAL_SURFACE ( 'NONE', #17111, 0.3444881889763780070, 0.1574803149606299191 ) ;
#27105 = CARTESIAN_POINT ( 'NONE',  ( 0.6971942568897626646, 0.07405724077823318263, 0.4773622046706456068 ) ) ;
#27106 = CARTESIAN_POINT ( 'NONE',  ( -1.054774247047244540, 0.07405724077823318263, 1.363188976324188895 ) ) ;
#27107 = CARTESIAN_POINT ( 'NONE',  ( 0.05036568513383885698, 0.2664124483477642302, -0.3061783854718803100 ) ) ;
#27108 = CARTESIAN_POINT ( 'NONE',  ( -0.8019270111902716547, 0.1787899950787401604, 1.373031496009229357 ) ) ;
#27109 = EDGE_CURVE ( 'NONE', #43976, #32565, #30672, .T. ) ;
#27110 = CARTESIAN_POINT ( 'NONE',  ( -0.8759842519685039353, -0.1787899950787401882, 0.09596456687537047170 ) ) ;
#27111 = CARTESIAN_POINT ( 'NONE',  ( 0.8759842519685039353, -0.1574803149606299191, 1.574803149606299302 ) ) ;
#27112 = CARTESIAN_POINT ( 'NONE',  ( -0.6971942568897648851, 0.07405724077823318263, 1.697834645615527771 ) ) ;
#27113 = CARTESIAN_POINT ( 'NONE',  ( -0.6971942568897637749, 2.189545951927499583E-17, 0.04675196845017354913 ) ) ;
#27114 = CARTESIAN_POINT ( 'NONE',  ( -0.7185039370078746268, -0.06523048226347956391, 1.724901574803149762 ) ) ;
#27115 = CIRCLE ( 'NONE', #21740, 0.09842519685039370636 ) ;
#27116 = PLANE ( 'NONE',  #5988 ) ;
#27117 = CARTESIAN_POINT ( 'NONE',  ( 0.8759842519685039353, -0.1787899950787401882, 1.592027559001354398 ) ) ;
#27118 = CARTESIAN_POINT ( 'NONE',  ( 0.2071770260006893793, -0.09842519685039370636, -0.0004133995244056677112 ) ) ;
#27119 = CYLINDRICAL_SURFACE ( 'NONE', #13425, 0.1003937007874011050 ) ;
#27120 = VERTEX_POINT ( 'NONE', #16510 ) ;
#27121 = VERTEX_POINT ( 'NONE', #20324 ) ;
#27122 = CARTESIAN_POINT ( 'NONE',  ( 0.1264236179284866091, -1.004429133804503937, -0.1264236179284866091 ) ) ;
#27123 = EDGE_CURVE ( 'NONE', #5917, #3060, #13163, .T. ) ;
#27124 = CARTESIAN_POINT ( 'NONE',  ( 0.07405724077823318263, -1.115157480261196987, -0.1787899950787401604 ) ) ;
#27125 = CARTESIAN_POINT ( 'NONE',  ( -0.1377952755905511861, -1.331775896911328393E-15, -0.8070866141732283561 ) ) ;
#27126 = CARTESIAN_POINT ( 'NONE',  ( 0.9500414927467378812, -0.1787899950787401604, 0.4084645668753704717 ) ) ;
#27127 = CARTESIAN_POINT ( 'NONE',  ( 0.1797182628040039365, -0.4144138883232031390, -2.200913952912460540E-17 ) ) ;
#27128 = CARTESIAN_POINT ( 'NONE',  ( -0.7185039370078746268, 0.06523048226347956391, 0.7652559054042838982 ) ) ;
#27129 = CARTESIAN_POINT ( 'NONE',  ( -0.06523048226347956391, 0.01919291338582680348, 0.1574803149606297803 ) ) ;
#27130 = AXIS2_PLACEMENT_3D ( 'NONE', #42569, #28474, #2330 ) ;
#27131 = CARTESIAN_POINT ( 'NONE',  ( -0.07405724077823318263, -0.1702755904974175283, -0.1787899950787401604 ) ) ;
#27132 = CARTESIAN_POINT ( 'NONE',  ( 0.000000000000000000, -0.5708661417322835607, 0.9783464566929134243 ) ) ;
#27133 = CARTESIAN_POINT ( 'NONE',  ( 0.8759842519685039353, 0.1787899950787401882, 0.8981299212060788184 ) ) ;
#27134 = CARTESIAN_POINT ( 'NONE',  ( -0.9412147342319837628, -0.1574803149606297803, 1.567421259734991690 ) ) ;
#27135 = AXIS2_PLACEMENT_3D ( 'NONE', #12256, #38117, #23269 ) ;
#27136 = DIRECTION ( 'NONE',  ( 0.000000000000000000, 0.000000000000000000, -1.000000000000000000 ) ) ;
#27137 = CARTESIAN_POINT ( 'NONE',  ( 0.6971942568897637749, 2.189545951927499583E-17, 1.936515747977732405 ) ) ;
#27138 = EDGE_CURVE ( 'NONE', #40089, #4124, #42359, .T. ) ;
#27139 = CARTESIAN_POINT ( 'NONE',  ( 0.9412147342319837628, -0.1574803149606297803, 0.1993110236220472509 ) ) ;
#27140 = DIRECTION ( 'NONE',  ( -0.000000000000000000, 0.7880107536067207930, -0.6156614753256597350 ) ) ;
#27141 = CARTESIAN_POINT ( 'NONE',  ( -0.1264236179284866091, -0.4729330708123779536, 0.1264236179284866091 ) ) ;
#27142 = LINE ( 'NONE', #31196, #13231 ) ;
#27143 = DIRECTION ( 'NONE',  ( 0.000000000000000000, 0.000000000000000000, 1.000000000000000000 ) ) ;
#27144 = EDGE_CURVE ( 'NONE', #460, #35241, #30439, .T. ) ;
#27145 = CARTESIAN_POINT ( 'NONE',  ( -0.7495606340400177148, 0.1264236179284866091, 1.690452755851748146 ) ) ;
#27146 = ORIENTED_EDGE ( 'NONE', *, *, #11179, .F. ) ;
#27147 = CARTESIAN_POINT ( 'NONE',  ( -0.7495606340400177148, -0.1264236179284866091, 1.350885826717889815 ) ) ;
#27148 = DIRECTION ( 'NONE',  ( 0.000000000000000000, 0.000000000000000000, 1.000000000000000000 ) ) ;
#27149 = CARTESIAN_POINT ( 'NONE',  ( 0.9500414927467378812, -0.1787899950787401604, 1.397637795221827295 ) ) ;
#27150 = CARTESIAN_POINT ( 'NONE',  ( -1.002407869896990045, 0.1264236179284866091, 1.168799212544661348 ) ) ;
#27151 = CARTESIAN_POINT ( 'NONE',  ( 0.9873396505805591694, 0.1113553986120547346, 1.540354330601133803 ) ) ;
#27152 = CARTESIAN_POINT ( 'NONE',  ( 0.03914454236661495806, -0.09842447277515208037, -0.1744522088443405949 ) ) ;
#27153 = CARTESIAN_POINT ( 'NONE',  ( 1.033464566929134687, 0.06523048226347956391, 0.04183070855389029591 ) ) ;
#27154 = CARTESIAN_POINT ( 'NONE',  ( 1.054774247047244540, 0.07405724077823318263, 0.5807086613635594752 ) ) ;
#27155 = CARTESIAN_POINT ( 'NONE',  ( -0.6971942568897648851, 0.07405724077823318263, 0.4330708660879683536 ) ) ;
#27156 = ADVANCED_FACE ( 'NONE', ( #12456 ), #1155, .T. ) ;
#27157 = CARTESIAN_POINT ( 'NONE',  ( 0.1878058820402545848, -0.07958416565541145959, -0.1770032286854512915 ) ) ;
#27158 = EDGE_CURVE ( 'NONE', #17345, #11957, #7921, .T. ) ;
#27159 = LINE ( 'NONE', #41712, #45104 ) ;
#27160 = ORIENTED_EDGE ( 'NONE', *, *, #46629, .T. ) ;
#27161 = CARTESIAN_POINT ( 'NONE',  ( -0.7185039370078746268, 0.06523048226347956391, 0.3026574803149607029 ) ) ;
#27162 = DIRECTION ( 'NONE',  ( 0.000000000000000000, 0.6156614753256602901, 0.7880107536067203489 ) ) ;
#27163 = CARTESIAN_POINT ( 'NONE',  ( -0.8107537697050254399, 0.1574803149606300301, 0.4847440943806614055 ) ) ;
#27164 = VECTOR ( 'NONE', #34341, 39.37007874015748143 ) ;
#27165 = AXIS2_PLACEMENT_3D ( 'NONE', #33260, #15036, #40391 ) ;
#27166 = EDGE_LOOP ( 'NONE', ( #11865, #41302, #21458, #28360 ) ) ;
#27167 = CARTESIAN_POINT ( 'NONE',  ( -0.6971942568897626646, -0.07405724077823297447, 0.9153543306548987957 ) ) ;
#27168 = DIRECTION ( 'NONE',  ( 0.000000000000000000, 0.000000000000000000, -1.000000000000000000 ) ) ;
#27169 = CARTESIAN_POINT ( 'NONE',  ( -0.6971942568897637749, 2.189545951927499583E-17, 0.04183070860765386589 ) ) ;
#27170 = EDGE_LOOP ( 'NONE', ( #46482, #38306, #30372, #12288, #9167, #25428 ) ) ;
#27171 = DIRECTION ( 'NONE',  ( 1.822029033848725028E-16, 0.000000000000000000, 1.000000000000000000 ) ) ;
#27172 = CARTESIAN_POINT ( 'NONE',  ( -0.1264236179284866091, -0.4680118109698582773, 0.1264236179284866091 ) ) ;
#27173 = CARTESIAN_POINT ( 'NONE',  ( -0.2927617443614862758, -0.1024931984611135161, 1.008690095761477723 ) ) ;
#27174 = ORIENTED_EDGE ( 'NONE', *, *, #13429, .F. ) ;
#27175 = CARTESIAN_POINT ( 'NONE',  ( 0.6971942568897648851, 0.07405724077823318263, 1.299212598371432215 ) ) ;
#27176 = CARTESIAN_POINT ( 'NONE',  ( 1.033464566929133799, 0.000000000000000000, 0.8759842519685039353 ) ) ;
#27177 = CARTESIAN_POINT ( 'NONE',  ( 0.1377952755905512139, 0.1574803149606299191, 0.7057086614173228023 ) ) ;
#27178 = DIRECTION ( 'NONE',  ( -0.5735764363510518216, -0.8191520442889876907, 0.000000000000000000 ) ) ;
#27179 = CARTESIAN_POINT ( 'NONE',  ( 1.002407869896990045, -0.1264236179284866091, 1.592027559001354398 ) ) ;
#27180 = CARTESIAN_POINT ( 'NONE',  ( -0.07405724077823318263, 0.1337342994872968427, -0.1787899950787401604 ) ) ;
#27181 = CARTESIAN_POINT ( 'NONE',  ( 0.1787899950787401604, -1.789370078686394194, -0.07405724077823318263 ) ) ;
#27182 = APPLICATION_PROTOCOL_DEFINITION ( 'draft international standard', 'automotive_design', 1998, #42846 ) ;
#27183 = EDGE_CURVE ( 'NONE', #29873, #37690, #8833, .T. ) ;
#27184 = CARTESIAN_POINT ( 'NONE',  ( 0.1720202176924468251, -0.09842519685039369248, 0.03783562498418870101 ) ) ;
#27185 = CARTESIAN_POINT ( 'NONE',  ( 1.002407869896990045, 0.1264236179284866091, 0.5388779527021417826 ) ) ;
#27186 = CARTESIAN_POINT ( 'NONE',  ( -1.002407869896990045, 0.1264236179284866091, 0.6619094487651338010 ) ) ;
#27188 = DIRECTION ( 'NONE',  ( 0.000000000000000000, -1.000000000000000000, 0.000000000000000000 ) ) ;
#27187 = CARTESIAN_POINT ( 'NONE',  ( -0.06523048226347956391, -0.8075787401574794355, 0.1574803149606297803 ) ) ;
#27189 = CARTESIAN_POINT ( 'NONE',  ( -0.07444174185955065859, -1.583213100921627703, -0.1797182628040039087 ) ) ;
#27190 = FACE_OUTER_BOUND ( 'NONE', #2201, .T. ) ;
#27191 = VECTOR ( 'NONE', #24196, 39.37007874015748143 ) ;
#27192 = DIRECTION ( 'NONE',  ( 1.000000000000000000, 0.000000000000000000, 0.000000000000000000 ) ) ;
#27193 = CARTESIAN_POINT ( 'NONE',  ( 1.002407869896990045, -0.1264236179284866091, 1.439468503883244210 ) ) ;
#27194 = CARTESIAN_POINT ( 'NONE',  ( 0.6971942568897648851, -0.07405724077823297447, 1.855314960576157635 ) ) ;
#27195 = CARTESIAN_POINT ( 'NONE',  ( 0.8019270111902716547, 0.1787899950787401604, 0.3100393700249766682 ) ) ;
#27196 = EDGE_CURVE ( 'NONE', #3799, #25562, #2153, .T. ) ;
#27197 = AXIS2_PLACEMENT_3D ( 'NONE', #23670, #2314, #23910 ) ;
#27198 = VECTOR ( 'NONE', #43139, 39.37007874015748143 ) ;
#27199 = CARTESIAN_POINT ( 'NONE',  ( -1.033464566929133799, 0.000000000000000000, 0.1574803148531029595 ) ) ;
#27200 = LINE ( 'NONE', #38426, #13618 ) ;
#27201 = DIRECTION ( 'NONE',  ( -0.8191520442889798082, 1.003171929053510079E-16, 0.5735764363510631458 ) ) ;
#27203 = CARTESIAN_POINT ( 'NONE',  ( -0.1264236179284866091, 0.02903543312462964626, -0.1264236179284866091 ) ) ;
#27202 = CARTESIAN_POINT ( 'NONE',  ( -0.1574803149606300301, -0.8863188975302678241, -0.06523048226347956391 ) ) ;
#27204 = DIRECTION ( 'NONE',  ( -1.000000000000000000, 0.000000000000000000, 0.000000000000000000 ) ) ;
#27205 = CARTESIAN_POINT ( 'NONE',  ( 0.7495606340400177148, 0.1264236179284866091, 0.5093503936470236138 ) ) ;
#27206 = CARTESIAN_POINT ( 'NONE',  ( 0.8759842519685039353, -0.1574803149606300579, 0.03937007874015747977 ) ) ;
#27208 = CARTESIAN_POINT ( 'NONE',  ( 0.8759842519685039353, -0.1574803149606299191, 1.958661417215307177 ) ) ;
#27207 = CARTESIAN_POINT ( 'NONE',  ( 0.6971942568897648851, -0.07405724077823297447, 1.304133858213953667 ) ) ;
#27209 = CARTESIAN_POINT ( 'NONE',  ( -0.7646288533564489232, -0.1113553986120547346, 1.323818897530267602 ) ) ;
#27210 = CARTESIAN_POINT ( 'NONE',  ( 0.9873396505805591694, 0.1113553986120547346, 0.7529527557979842634 ) ) ;
#27211 = VERTEX_POINT ( 'NONE', #24631 ) ;
#27212 = FACE_OUTER_BOUND ( 'NONE', #19767, .T. ) ;
#27213 = ORIENTED_EDGE ( 'NONE', *, *, #18770, .T. ) ;
#27214 = CARTESIAN_POINT ( 'NONE',  ( 0.1787899950787401882, -1.363681102308440973, -2.189545951927503898E-17 ) ) ;
#27215 = CARTESIAN_POINT ( 'NONE',  ( -0.9412147342319837628, 0.1574803149606300301, 0.5585629920184573827 ) ) ;
#27216 = LINE ( 'NONE', #41767, #34047 ) ;
#27217 = CARTESIAN_POINT ( 'NONE',  ( -0.8759842519685039353, 0.1574803149606299191, 1.200787401574803237 ) ) ;
#27218 = CARTESIAN_POINT ( 'NONE',  ( -0.1377952755905511584, 0.1564960629921283985, -0.9074803149606294195 ) ) ;
#27219 = CARTESIAN_POINT ( 'NONE',  ( 1.033464566929133799, 0.000000000000000000, 1.938976377952756014 ) ) ;
#27220 = CARTESIAN_POINT ( 'NONE',  ( 0.8107537697050254399, 0.1574803149606300301, 0.3666338581601893964 ) ) ;
#27221 = CARTESIAN_POINT ( 'NONE',  ( 1.033464566929134687, -0.06523048226347956391, 1.454232283357038691 ) ) ;
#27222 = EDGE_LOOP ( 'NONE', ( #23645, #27937, #32117, #31046 ) ) ;
#27223 = VERTEX_POINT ( 'NONE', #46190 ) ;
#27224 = FACE_OUTER_BOUND ( 'NONE', #13168, .T. ) ;
#27225 = ORIENTED_EDGE ( 'NONE', *, *, #35720, .T. ) ;
#27226 = CARTESIAN_POINT ( 'NONE',  ( -0.6971942568897648851, -0.07405724077823297447, 1.540354330654897685 ) ) ;
#27227 = CARTESIAN_POINT ( 'NONE',  ( -0.06523048226347956391, -0.01033464556176428781, 0.1574803149606297803 ) ) ;
#27228 = CARTESIAN_POINT ( 'NONE',  ( -0.6971942568897637749, 2.189545951927499583E-17, 1.385334645615527549 ) ) ;
#27229 = ORIENTED_EDGE ( 'NONE', *, *, #29449, .T. ) ;
#27230 = CARTESIAN_POINT ( 'NONE',  ( -0.7646288533564489232, 0.1113553986120547346, 0.2509842518609771700 ) ) ;
#27231 = CARTESIAN_POINT ( 'NONE',  ( 0.4736248074375818407, 1.488499961090669288, -0.3513258257898456138 ) ) ;
#27232 = CIRCLE ( 'NONE', #41699, 0.1574803149606291142 ) ;
#27233 = DIRECTION ( 'NONE',  ( 1.000000000000000000, 0.000000000000000000, 0.000000000000000000 ) ) ;
#27234 = CARTESIAN_POINT ( 'NONE',  ( 0.1787899950787401604, -0.9440216060245140151, 0.07405724077823318263 ) ) ;
#27235 = ORIENTED_EDGE ( 'NONE', *, *, #43324, .F. ) ;
#27236 = CARTESIAN_POINT ( 'NONE',  ( 0.1264236179284866091, 0.1028543307624250058, -0.1264236179284866091 ) ) ;
#27237 = ORIENTED_EDGE ( 'NONE', *, *, #31027, .T. ) ;
#27238 = ORIENTED_EDGE ( 'NONE', *, *, #30395, .F. ) ;
#27239 = CARTESIAN_POINT ( 'NONE',  ( 1.033464566929134687, 0.06523048226347956391, 1.734744094380662904 ) ) ;
#27240 = CYLINDRICAL_SURFACE ( 'NONE', #10837, 0.1574803149606299191 ) ;
#27241 = CARTESIAN_POINT ( 'NONE',  ( 0.7646288533564489232, -0.1113553986120547346, 1.806102362204724532 ) ) ;
#27242 = CARTESIAN_POINT ( 'NONE',  ( -0.1787899950787401604, -0.6722440944344262315, 0.07405724077823318263 ) ) ;
#27243 = ADVANCED_FACE ( 'NONE', ( #21497 ), #24369, .T. ) ;
#27244 = ADVANCED_FACE ( 'NONE', ( #14087 ), #31608, .T. ) ;
#27245 = CARTESIAN_POINT ( 'NONE',  ( -0.6971942568897626646, 0.07405724077823318263, 0.2411417322297010890 ) ) ;
#27246 = CARTESIAN_POINT ( 'NONE',  ( -0.7185039370078746268, -0.06523048226347956391, 1.094980314960628975 ) ) ;
#27247 = CARTESIAN_POINT ( 'NONE',  ( 0.1797182628040039087, -1.204276093047611740, 0.07444174185955046430 ) ) ;
#27248 = CARTESIAN_POINT ( 'NONE',  ( 0.1746219128791692832, 0.1299212598425196763, 0.02006551292331004710 ) ) ;
#27249 = CARTESIAN_POINT ( 'NONE',  ( 1.054774247047244096, 0.000000000000000000, 1.129429133804503937 ) ) ;
#27250 = CARTESIAN_POINT ( 'NONE',  ( 1.054774247047244540, -0.07405724077823318263, 1.437007873961985593 ) ) ;
#27251 = EDGE_CURVE ( 'NONE', #8310, #7448, #12848, .T. ) ;
#27252 = EDGE_CURVE ( 'NONE', #18121, #22721, #17711, .T. ) ;
#27253 = CYLINDRICAL_SURFACE ( 'NONE', #13789, 0.09842519685039370636 ) ;
#27254 = CARTESIAN_POINT ( 'NONE',  ( 0.7185039370078746268, 0.06523048226347956391, 1.601870078740158077 ) ) ;
#27256 = CARTESIAN_POINT ( 'NONE',  ( -0.1578366172103670140, -0.2043672459941665021, -0.3136338785705618526 ) ) ;
#27255 = CARTESIAN_POINT ( 'NONE',  ( 0.7523722263184977610, 0.1050276425381515832, 1.981051316850578781 ) ) ;
#27257 = DIRECTION ( 'NONE',  ( -3.469446951953614189E-15, -1.000000000000000000, 0.000000000000000000 ) ) ;
#27258 = CARTESIAN_POINT ( 'NONE',  ( 0.1574803149606300301, -0.7436023620971976555, -0.06523048226347956391 ) ) ;
#27259 = LINE ( 'NONE', #4692, #39839 ) ;
#27260 = CARTESIAN_POINT ( 'NONE',  ( 0.7495606340400177148, 0.1264236179284866091, 1.060531496009228247 ) ) ;
#27261 = CARTESIAN_POINT ( 'NONE',  ( 1.054774247047244540, -0.07405724077823318263, 1.796259842465920853 ) ) ;
#27262 = CARTESIAN_POINT ( 'NONE',  ( 0.9412147342319837628, 0.1574803149606300301, 0.2829724408373550104 ) ) ;
#27263 = ORIENTED_EDGE ( 'NONE', *, *, #33845, .T. ) ;
#27264 = DIRECTION ( 'NONE',  ( 3.469446951953626022E-15, 1.000000000000000000, 0.000000000000000000 ) ) ;
#27265 = CARTESIAN_POINT ( 'NONE',  ( 1.015010158765895509, 0.08643607152993285081, 0.03936569692628689304 ) ) ;
#27266 = AXIS2_PLACEMENT_3D ( 'NONE', #27427, #1981, #5328 ) ;
#27267 = TOROIDAL_SURFACE ( 'NONE', #33383, 0.3444881889763780070, 0.1574803149606299191 ) ;
#27268 = CARTESIAN_POINT ( 'NONE',  ( 0.1113553986120547346, -1.735236220364913429, 0.1113553986120547346 ) ) ;
#27269 = CARTESIAN_POINT ( 'NONE',  ( -0.9412147342319837628, -0.1574803149606297803, 0.2682086613097960370 ) ) ;
#27270 = DIRECTION ( 'NONE',  ( 0.000000000000000000, -1.000000000000000000, 0.000000000000000000 ) ) ;
#27271 = CARTESIAN_POINT ( 'NONE',  ( 0.9500414927467378812, 0.1787899950787401604, 1.328740157426552049 ) ) ;
#27272 = CARTESIAN_POINT ( 'NONE',  ( 0.7646288533564489232, 0.1113553986120547346, 1.235236220364913207 ) ) ;
#27273 = CARTESIAN_POINT ( 'NONE',  ( 0.1787899950787401882, 0.09793307091990532953, -2.189545951927503898E-17 ) ) ;
#27274 = CARTESIAN_POINT ( 'NONE',  ( -1.033464566929133355, 0.06523048226348168721, 1.862696850393700476 ) ) ;
#27275 = ( BOUNDED_CURVE ( )  B_SPLINE_CURVE ( 2, ( #37177, #10861, #18263, #32672, #22089, #36713, #47260, #32909, #29095 ),
 .UNSPECIFIED., .F., .T. ) 
 B_SPLINE_CURVE_WITH_KNOTS ( ( 3, 2, 2, 2, 3 ),
 ( 0.04000000000000000083, 0.04250000000000000305, 0.04499999999999999833, 0.04750000000000000056, 0.05000000000000000278 ),
 .UNSPECIFIED. ) 
 CURVE ( )  GEOMETRIC_REPRESENTATION_ITEM ( )  RATIONAL_B_SPLINE_CURVE ( ( 1.000000000000000000, 0.9238795325112869605, 1.000000000000000000, 0.9238795325112869605, 1.000000000000000000, 0.9238795325112869605, 1.000000000000000000, 0.9238795325112869605, 1.000000000000000000 ) ) 
 REPRESENTATION_ITEM ( '' )  ) ;
#27276 = CARTESIAN_POINT ( 'NONE',  ( -1.054774247047244540, 0.07405724077823318263, 0.5757874015210394658 ) ) ;
#27277 = CARTESIAN_POINT ( 'NONE',  ( -0.6195511811023656223, 0.6102362204724408601, 0.5167322834645649010 ) ) ;
#27278 = VERTEX_POINT ( 'NONE', #10502 ) ;
#27279 = FACE_OUTER_BOUND ( 'NONE', #10392, .T. ) ;
#27280 = VERTEX_POINT ( 'NONE', #17670 ) ;
#27282 = CARTESIAN_POINT ( 'NONE',  ( 0.1787899950787401882, -1.560531496009228247, -2.189545951927503898E-17 ) ) ;
#27281 = CARTESIAN_POINT ( 'NONE',  ( 0.06523048226347956391, -0.3597440943806616831, 0.1574803149606297803 ) ) ;
#27283 = CARTESIAN_POINT ( 'NONE',  ( -0.6971942568897637749, 2.189545951927499583E-17, 1.031003936954110189 ) ) ;
#27284 = CARTESIAN_POINT ( 'NONE',  ( -0.8019270111902717657, 0.1787899950787401604, 1.845472440891119392 ) ) ;
#27285 = VERTEX_POINT ( 'NONE', #25100 ) ;
#27286 = CARTESIAN_POINT ( 'NONE',  ( -0.6971942568897626646, 0.07405724077823318263, 0.6742125983714335469 ) ) ;
#27287 = EDGE_LOOP ( 'NONE', ( #14512, #34743 ) ) ;
#27288 = CYLINDRICAL_SURFACE ( 'NONE', #33742, 0.09842519685039370636 ) ;
#27289 = DIRECTION ( 'NONE',  ( 0.000000000000000000, -0.6156614753256597350, -0.7880107536067206819 ) ) ;
#27290 = CARTESIAN_POINT ( 'NONE',  ( 0.1787899950787401604, -0.5847696375205770902, -0.07405724077823318263 ) ) ;
#27291 = CARTESIAN_POINT ( 'NONE',  ( -0.1179609706914375999, -0.08956081431181496522, -0.1345230454816687127 ) ) ;
#27292 = CARTESIAN_POINT ( 'NONE',  ( 1.033464566929133799, 0.000000000000000000, 0.4822834645669291653 ) ) ;
#27293 = AXIS2_PLACEMENT_3D ( 'NONE', #18719, #36486, #15387 ) ;
#27294 = ( BOUNDED_CURVE ( )  B_SPLINE_CURVE ( 2, ( #19277, #4893, #33934, #16414, #34164, #1774, #1056, #44899, #12111 ),
 .UNSPECIFIED., .F., .T. ) 
 B_SPLINE_CURVE_WITH_KNOTS ( ( 3, 2, 2, 2, 3 ),
 ( 0.5600000000000000533, 0.5625000000000000000, 0.5649999999999999467, 0.5675000000000000044, 0.5699999999999999512 ),
 .UNSPECIFIED. ) 
 CURVE ( )  GEOMETRIC_REPRESENTATION_ITEM ( )  RATIONAL_B_SPLINE_CURVE ( ( 1.000000000000000000, 0.9238795325112869605, 1.000000000000000000, 0.9238795325112869605, 1.000000000000000000, 0.9238795325112869605, 1.000000000000000000, 0.9238795325112829637, 1.000000000000000000 ) ) 
 REPRESENTATION_ITEM ( '' )  ) ;
#27295 = CARTESIAN_POINT ( 'NONE',  ( -1.002407869896990045, -0.1264236179284866091, 0.5290354330171024300 ) ) ;
#27296 = CARTESIAN_POINT ( 'NONE',  ( 1.033464566929133799, 0.000000000000000000, 1.230314960629921295 ) ) ;
#27297 = ORIENTED_EDGE ( 'NONE', *, *, #38937, .T. ) ;
#27298 = CARTESIAN_POINT ( 'NONE',  ( -1.054774247047244096, 0.000000000000000000, 1.523129921206078707 ) ) ;
#27299 = CARTESIAN_POINT ( 'NONE',  ( 0.1787899950787401604, -1.484251968450174930, 0.07405724077823318263 ) ) ;
#27300 = DIRECTION ( 'NONE',  ( 0.000000000000000000, 0.000000000000000000, -1.000000000000000000 ) ) ;
#27301 = EDGE_CURVE ( 'NONE', #18385, #5685, #6877, .T. ) ;
#27302 = DIRECTION ( 'NONE',  ( 0.000000000000000000, 0.000000000000000000, 1.000000000000000000 ) ) ;
#27303 = CARTESIAN_POINT ( 'NONE',  ( -0.3161444924769509779, 0.9382165298418940758, -1.070508272602715749 ) ) ;
#27304 = ADVANCED_BREP_SHAPE_REPRESENTATION ( 'U-Bolt', ( #5043, #20860 ), #15520 ) ;
#27305 = ORIENTED_EDGE ( 'NONE', *, *, #8162, .F. ) ;
#27306 = CARTESIAN_POINT ( 'NONE',  ( -1.100456976456230270E-17, -0.7589020772995805908, -0.1797182628040039365 ) ) ;
#27307 = PLANE ( 'NONE',  #22475 ) ;
#27308 = CARTESIAN_POINT ( 'NONE',  ( -0.7646288533564489232, 0.1113553986120547346, 1.313976377845228249 ) ) ;
#27309 = CARTESIAN_POINT ( 'NONE',  ( 0.7495606340400177148, 0.1264236179284866091, 0.5930118109698583329 ) ) ;
#27310 = CARTESIAN_POINT ( 'NONE',  ( 0.9500414927467377701, 0.1787899950787401604, 0.06889763774151215492 ) ) ;
#27312 = DIRECTION ( 'NONE',  ( 1.822029033848725028E-16, 0.000000000000000000, 1.000000000000000000 ) ) ;
#27311 = CARTESIAN_POINT ( 'NONE',  ( 0.1574803149606300301, -0.4778543307086612346, -0.06523048226347956391 ) ) ;
#27313 = CARTESIAN_POINT ( 'NONE',  ( 0.1574803149606299191, 0.5288907983920094757, -0.7507079620615707549 ) ) ;
#27314 = ORIENTED_EDGE ( 'NONE', *, *, #10785, .F. ) ;
#27315 = ADVANCED_FACE ( 'NONE', ( #17432 ), #32067, .F. ) ;
#27316 = CARTESIAN_POINT ( 'NONE',  ( 0.1377952755905509641, 1.687505431895956722E-17, -0.2219368594840610276 ) ) ;
#27317 = CARTESIAN_POINT ( 'NONE',  ( -0.7495606340400177148, 0.1264236179284866091, 1.104822834591905556 ) ) ;
#27318 = CARTESIAN_POINT ( 'NONE',  ( 0.8107537697050253289, -0.1574803149606297803, 1.099901574803150650 ) ) ;
#27319 = CARTESIAN_POINT ( 'NONE',  ( -0.8905975117434016264, -0.1743539442039271081, 1.988441309659580769 ) ) ;
#27320 = FACE_OUTER_BOUND ( 'NONE', #35216, .T. ) ;
#27322 = DIRECTION ( 'NONE',  ( 0.000000000000000000, 0.000000000000000000, 1.000000000000000000 ) ) ;
#27321 = DIRECTION ( 'NONE',  ( -1.000000000000000000, 0.000000000000000000, 0.000000000000000000 ) ) ;
#27323 = CARTESIAN_POINT ( 'NONE',  ( 0.7185039370078714072, 0.06523048226347728795, 1.277066929026331232 ) ) ;
#27324 = CARTESIAN_POINT ( 'NONE',  ( 0.3246033735368759610, -0.09842519685039370636, 1.205361022782828805E-17 ) ) ;
#27325 = CARTESIAN_POINT ( 'NONE',  ( 0.1787899950787401604, -0.4950787401037172186, 0.07405724077823318263 ) ) ;
#27326 = DIRECTION ( 'NONE',  ( 0.000000000000000000, 0.000000000000000000, 1.000000000000000000 ) ) ;
#27327 = ORIENTED_EDGE ( 'NONE', *, *, #8633, .F. ) ;
#27328 = CARTESIAN_POINT ( 'NONE',  ( 0.8759842519685039353, -0.1574803149606299191, 0.8661417322834645827 ) ) ;
#27329 = CARTESIAN_POINT ( 'NONE',  ( 1.054774247047244096, 0.000000000000000000, 0.7308070865604093802 ) ) ;
#27330 = ORIENTED_EDGE ( 'NONE', *, *, #33573, .T. ) ;
#27331 = DIRECTION ( 'NONE',  ( 1.822029033848725028E-16, 0.000000000000000000, 1.000000000000000000 ) ) ;
#27332 = CARTESIAN_POINT ( 'NONE',  ( 0.000000000000000000, 0.000000000000000000, 0.000000000000000000 ) ) ;
#27333 = B_SPLINE_CURVE_WITH_KNOTS ( 'NONE', 3,
 ( #17915, #10266, #21504, #2810, #24642, #42811, #25363, #39945, #20564, #35673, #17441, #32569 ),
 .UNSPECIFIED., .F., .F.,
 ( 4, 2, 2, 2, 2, 4 ),
 ( 0.000000000000000000, 0.2499999999999998335, 0.3749999999999997780, 0.4374999999999997224, 0.4999999999999996669, 1.000000000000000000 ),
 .UNSPECIFIED. ) ;
#27334 = CARTESIAN_POINT ( 'NONE',  ( -0.07405724077823318263, -1.764763779473795813, 0.1787899950787401604 ) ) ;
#27335 = CARTESIAN_POINT ( 'NONE',  ( -0.1264236179284866091, -0.9453740156942677109, 0.1264236179284866091 ) ) ;
#27336 = CARTESIAN_POINT ( 'NONE',  ( -0.06523048226347956391, -1.437499999999999334, 0.1574803149606297803 ) ) ;
#27337 = CARTESIAN_POINT ( 'NONE',  ( 0.7185039370078746268, 0.06523048226347956391, 1.237696850286174044 ) ) ;
#27338 = DIRECTION ( 'NONE',  ( 0.5735764363510447161, -0.8191520442889925757, 1.003171929053525486E-16 ) ) ;
#27339 = ORIENTED_EDGE ( 'NONE', *, *, #35575, .T. ) ;
#27340 = ORIENTED_EDGE ( 'NONE', *, *, #3195, .T. ) ;
#27341 = CARTESIAN_POINT ( 'NONE',  ( -1.002407869896990045, 0.1264236179284866091, 1.961122047190330786 ) ) ;
#27342 = CARTESIAN_POINT ( 'NONE',  ( 1.002407869896990045, -0.1264236179284866091, 1.911909448765133801 ) ) ;
#27343 = ORIENTED_EDGE ( 'NONE', *, *, #1012, .F. ) ;
#27344 = CARTESIAN_POINT ( 'NONE',  ( -1.054774247047244540, 0.07405724077823318263, 0.8956692912848198684 ) ) ;
#27345 = CARTESIAN_POINT ( 'NONE',  ( 0.7185039370078739607, 1.928577636452523993E-17, 1.486220472440944906 ) ) ;
#27346 = CARTESIAN_POINT ( 'NONE',  ( 0.8759842519685039353, -0.1787899950787401882, 0.3715551180564728440 ) ) ;
#27347 = CARTESIAN_POINT ( 'NONE',  ( -0.7495606340400177148, 0.1264236179284866091, 1.336122047190330786 ) ) ;
#27348 = CARTESIAN_POINT ( 'NONE',  ( 0.000000000000000000, 0.09842519685039370636, 0.000000000000000000 ) ) ;
#27349 = CARTESIAN_POINT ( 'NONE',  ( -0.6971942568897626646, 0.07405724077823318263, 0.9842519684501742638 ) ) ;
#27350 = EDGE_CURVE ( 'NONE', #36971, #3855, #20530, .T. ) ;
#27351 = CARTESIAN_POINT ( 'NONE',  ( -1.002407869896990045, -0.1264236179284866091, 0.1402559054580474474 ) ) ;
#27352 = PLANE ( 'NONE',  #38284 ) ;
#27353 = CARTESIAN_POINT ( 'NONE',  ( -0.8759842519685039353, 0.1787899950787401882, 1.769192913332062966 ) ) ;
#27354 = CARTESIAN_POINT ( 'NONE',  ( -0.8019270111902717657, 0.1787899950787401604, 0.03937007868639399305 ) ) ;
#27355 = CARTESIAN_POINT ( 'NONE',  ( -0.1550283333641100658, 0.09383642490574128914, 0.1959274208663538963 ) ) ;
#27356 = CARTESIAN_POINT ( 'NONE',  ( -0.8107537697050253289, -0.1574803149606297803, 1.769192913385826404 ) ) ;
#27357 = CARTESIAN_POINT ( 'NONE',  ( -0.8759842519685039353, 0.1574803149606299191, 0.2952755905511810774 ) ) ;
#27358 = CARTESIAN_POINT ( 'NONE',  ( 1.054774247047244540, 0.07405724077823318263, 1.722440944828126153 ) ) ;
#27359 = CARTESIAN_POINT ( 'NONE',  ( 0.2037090642851917544, -0.09842519685039370636, 0.05108520076791897568 ) ) ;
#27360 = CARTESIAN_POINT ( 'NONE',  ( -1.033464566929133799, 0.000000000000000000, 0.2362204723334177248 ) ) ;
#27361 = AXIS2_PLACEMENT_3D ( 'NONE', #4273, #7418, #40229 ) ;
#27362 = ORIENTED_EDGE ( 'NONE', *, *, #6330, .F. ) ;
#27363 = ORIENTED_EDGE ( 'NONE', *, *, #21368, .F. ) ;
#27364 = CARTESIAN_POINT ( 'NONE',  ( 0.07405724077823318263, -1.001968503883243988, -0.1787899950787401604 ) ) ;
#27365 = CARTESIAN_POINT ( 'NONE',  ( -0.07405724077823318263, -0.4704724408911186706, 0.1787899950787401604 ) ) ;
#27366 = CARTESIAN_POINT ( 'NONE',  ( 0.07405724077823318263, -1.154527559001354842, -0.1787899950787401604 ) ) ;
#27367 = EDGE_CURVE ( 'NONE', #13443, #15682, #40412, .T. ) ;
#27368 = CARTESIAN_POINT ( 'NONE',  ( 0.000000000000000000, 0.09842519685039370636, 0.2471922904502826812 ) ) ;
#27369 = CARTESIAN_POINT ( 'NONE',  ( 0.8759842519685039353, -0.1787899950787401882, 0.4060039369541102450 ) ) ;
#27370 = CARTESIAN_POINT ( 'NONE',  ( 0.1270800023317771588, -0.4882327859609983944, -0.1270800023317771588 ) ) ;
#27371 = CARTESIAN_POINT ( 'NONE',  ( -0.1574803149606297803, -1.786909448711370585, 0.06523048226347956391 ) ) ;
#27372 = CARTESIAN_POINT ( 'NONE',  ( -1.033464566929133799, 0.000000000000000000, 0.8661417321759370402 ) ) ;
#27373 = CARTESIAN_POINT ( 'NONE',  ( -0.1574803149606300301, -0.06938976377952764396, -0.06523048226347956391 ) ) ;
#27374 = CARTESIAN_POINT ( 'NONE',  ( 0.1787899950787401604, -0.1407480314422995815, -0.07405724077823318263 ) ) ;
#27375 = EDGE_CURVE ( 'NONE', #42942, #3332, #17997, .T. ) ;
#27376 = CARTESIAN_POINT ( 'NONE',  ( 0.8019270111902717657, 0.1787899950787401604, 0.8612204723871809131 ) ) ;
#27378 = CARTESIAN_POINT ( 'NONE',  ( 0.2759478392031582961, -0.5708661417322835607, 1.214596435718460654 ) ) ;
#27377 = CARTESIAN_POINT ( 'NONE',  ( 0.08568752866847809124, 0.2460225145194667729, -0.03726912461315685238 ) ) ;
#27379 = CARTESIAN_POINT ( 'NONE',  ( 0.8759842519685039353, 0.1787899950787401882, 1.926673228292693052 ) ) ;
#27380 = ORIENTED_EDGE ( 'NONE', *, *, #38409, .F. ) ;
#27381 = CARTESIAN_POINT ( 'NONE',  ( 0.8759842519685039353, -0.1574803149606299191, 0.3838582676090082635 ) ) ;
#27382 = CARTESIAN_POINT ( 'NONE',  ( 0.1787899950787401882, -0.4975393700249764461, -2.189545951927503898E-17 ) ) ;
#27383 = FACE_OUTER_BOUND ( 'NONE', #28400, .T. ) ;
#27385 = VECTOR ( 'NONE', #15460, 39.37007874015748143 ) ;
#27384 = CARTESIAN_POINT ( 'NONE',  ( 0.07405724077823318263, -1.430118110182456714, -0.1787899950787401604 ) ) ;
#27386 = CARTESIAN_POINT ( 'NONE',  ( -0.7495606340400177148, 0.1264236179284866091, 1.847933070812378009 ) ) ;
#27387 = EDGE_LOOP ( 'NONE', ( #45965, #30422, #920, #36753 ) ) ;
#27388 = VERTEX_POINT ( 'NONE', #42802 ) ;
#27389 = CARTESIAN_POINT ( 'NONE',  ( -0.7495606340400177148, 0.1264236179284866091, 1.341043307032850462 ) ) ;
#27390 = CARTESIAN_POINT ( 'NONE',  ( 0.8019270111902717657, -0.1787899950787401604, 1.392716535379308285 ) ) ;
#27391 = CARTESIAN_POINT ( 'NONE',  ( -0.8019270111902717657, -0.1787899950787401604, 0.5265748030958428139 ) ) ;
#27392 = CARTESIAN_POINT ( 'NONE',  ( 1.054774247047244540, 0.07405724077823318263, 0.06889763774151215492 ) ) ;
#27393 = CARTESIAN_POINT ( 'NONE',  ( -1.002407869896990045, -0.1264236179284866091, 1.198326771599779628 ) ) ;
#27394 = DIRECTION ( 'NONE',  ( -1.000000000000000000, 0.000000000000000000, 0.000000000000000000 ) ) ;
#27395 = CARTESIAN_POINT ( 'NONE',  ( -0.9412147342319837628, 0.1574803149606300301, 1.345964566821607589 ) ) ;
#27396 = CARTESIAN_POINT ( 'NONE',  ( 1.002407869896990045, -0.1264236179284866091, 0.6520669290800944484 ) ) ;
#27397 = CARTESIAN_POINT ( 'NONE',  ( -0.9500414927467377701, 0.1787899950787401604, 0.5413385826234012876 ) ) ;
#27398 = CARTESIAN_POINT ( 'NONE',  ( -0.7495606340400177148, -0.1264236179284866091, 0.8341535432533228045 ) ) ;
#27399 = EDGE_CURVE ( 'NONE', #27120, #32643, #3303, .T. ) ;
#27400 = CARTESIAN_POINT ( 'NONE',  ( 4.681852760415787419E-17, -0.03219022224904102836, 0.2854330708661417804 ) ) ;
#27401 = ADVANCED_BREP_SHAPE_REPRESENTATION ( 'Base Plate', ( #20717, #20860 ), #14766 ) ;
#27402 = DIRECTION ( 'NONE',  ( 0.000000000000000000, 0.000000000000000000, 1.000000000000000000 ) ) ;
#27403 = ORIENTED_EDGE ( 'NONE', *, *, #40234, .T. ) ;
#27404 = FACE_OUTER_BOUND ( 'NONE', #5927, .T. ) ;
#27405 = CARTESIAN_POINT ( 'NONE',  ( -0.7185039370078746268, 0.06523048226347956391, 0.3420275590551182798 ) ) ;
#27406 = CARTESIAN_POINT ( 'NONE',  ( -0.2038129627511063025, -0.09851385024907242938, 0.1181531328361742073 ) ) ;
#27407 = CARTESIAN_POINT ( 'NONE',  ( -0.8107537697050254399, -0.1574803149606297803, 1.966043307086614567 ) ) ;
#27408 = VERTEX_POINT ( 'NONE', #8058 ) ;
#27409 = CARTESIAN_POINT ( 'NONE',  ( -1.033464566929133799, 0.000000000000000000, 1.309055118110236338 ) ) ;
#27410 = ( BOUNDED_CURVE ( )  B_SPLINE_CURVE ( 2, ( #38755, #39442, #6623, #28459, #17179, #16943, #31342, #27990, #5684 ),
 .UNSPECIFIED., .F., .T. ) 
 B_SPLINE_CURVE_WITH_KNOTS ( ( 3, 2, 2, 2, 3 ),
 ( 0.3099999999999999978, 0.3125000000000000000, 0.3150000000000000022, 0.3175000000000000044, 0.3200000000000000067 ),
 .UNSPECIFIED. ) 
 CURVE ( )  GEOMETRIC_REPRESENTATION_ITEM ( )  RATIONAL_B_SPLINE_CURVE ( ( 1.000000000000000000, 0.9238795325112869605, 1.000000000000000000, 0.9238795325112869605, 1.000000000000000000, 0.9238795325112869605, 1.000000000000000000, 0.9238795325112869605, 1.000000000000000000 ) ) 
 REPRESENTATION_ITEM ( '' )  ) ;
#27411 = CARTESIAN_POINT ( 'NONE',  ( -1.054774247047244096, 0.000000000000000000, 0.1008858267178899676 ) ) ;
#27412 = VERTEX_POINT ( 'NONE', #392 ) ;
#27413 = CARTESIAN_POINT ( 'NONE',  ( -0.7185039370078746268, 0.06523048226347977208, 0.1747047243019218821 ) ) ;
#27414 = CARTESIAN_POINT ( 'NONE',  ( -1.094772975963752103E-17, -0.5221456692375747721, -0.1787899950787401882 ) ) ;
#27415 = CARTESIAN_POINT ( 'NONE',  ( -0.2802233088437623976, -0.1328339237432898945, 0.9783027062435790677 ) ) ;
#27416 = ORIENTED_EDGE ( 'NONE', *, *, #12746, .T. ) ;
#27417 = CARTESIAN_POINT ( 'NONE',  ( 1.054774247047244540, 0.07405724077823318263, 1.323818897584032817 ) ) ;
#27418 = CARTESIAN_POINT ( 'NONE',  ( 0.8759842519685039353, 0.1574803149606299191, 0.8858267716535432879 ) ) ;
#27419 = AXIS2_PLACEMENT_3D ( 'NONE', #39066, #27394, #13675 ) ;
#27420 = CARTESIAN_POINT ( 'NONE',  ( -0.1787899950787401882, -0.2416338582139531399, 0.000000000000000000 ) ) ;
#27421 = EDGE_CURVE ( 'NONE', #18854, #33098, #22441, .T. ) ;
#27422 = CARTESIAN_POINT ( 'NONE',  ( 1.033464566929133355, 0.06523048226348168721, 1.862696850393700476 ) ) ;
#27423 = CARTESIAN_POINT ( 'NONE',  ( 0.6971942568897626646, -0.07405724077823297447, 0.2411417322297011168 ) ) ;
#27424 = CARTESIAN_POINT ( 'NONE',  ( 3.284318927891251994E-17, -0.006521606024514312559, 0.1787899950787401882 ) ) ;
#27425 = CARTESIAN_POINT ( 'NONE',  ( -0.1264236179284866091, 0.1471456693451021758, -0.1264236179284866091 ) ) ;
#27426 = PRODUCT_CONTEXT ( 'NONE', #42846, 'mechanical' ) ;
#27427 = CARTESIAN_POINT ( 'NONE',  ( -0.8759842519685039353, 0.000000000000000000, 0.000000000000000000 ) ) ;
#27428 = EDGE_CURVE ( 'NONE', #183, #29781, #5979, .T. ) ;
#27429 = CARTESIAN_POINT ( 'NONE',  ( 1.054774247047244096, 0.000000000000000000, 0.4552165353793071745 ) ) ;
#27430 = CARTESIAN_POINT ( 'NONE',  ( -0.6971942568897637749, 2.189545951927499583E-17, 0.7947834645131652831 ) ) ;
#27432 = CARTESIAN_POINT ( 'NONE',  ( -1.033464566929133799, 0.000000000000000000, 0.8366141732283465249 ) ) ;
#27431 = CARTESIAN_POINT ( 'NONE',  ( 0.06523048226347956391, -0.9060039370078742937, -0.1574803149606300301 ) ) ;
#27434 = CARTESIAN_POINT ( 'NONE',  ( -0.7750584684036548877, -0.1381424679723168569, 1.986199844405018622 ) ) ;
#27433 = CARTESIAN_POINT ( 'NONE',  ( 0.07444174185955046430, -1.627504439504305456, -0.1797182628040039087 ) ) ;
#27435 = LINE ( 'NONE', #17488, #17952 ) ;
#27436 = CARTESIAN_POINT ( 'NONE',  ( 0.2871444924769515628, 0.9382165298418956301, -1.070508272602716637 ) ) ;
#27437 = CARTESIAN_POINT ( 'NONE',  ( 1.054774247047244096, 0.000000000000000000, 1.523129921206078707 ) ) ;
#27438 = CARTESIAN_POINT ( 'NONE',  ( 0.9500414927467377701, 0.1787899950787401604, 1.801181102308441861 ) ) ;
#27439 = CARTESIAN_POINT ( 'NONE',  ( 0.6971942568897648851, 0.07405724077823318263, 0.4724409448281262636 ) ) ;
#27440 = CYLINDRICAL_SURFACE ( 'NONE', #13827, 0.1377952755905510751 ) ;
#27441 = DIRECTION ( 'NONE',  ( 0.000000000000000000, 0.000000000000000000, 1.000000000000000000 ) ) ;
#27442 = CARTESIAN_POINT ( 'NONE',  ( 1.033464566929133799, 1.928577636452524610E-17, 4.498031496062992574 ) ) ;
#27443 = CARTESIAN_POINT ( 'NONE',  ( 0.1787899950787401604, -0.02755905506434671789, 0.07405724077823318263 ) ) ;
#27444 = CARTESIAN_POINT ( 'NONE',  ( 0.9500414927467378812, 0.1787899950787401604, 0.5019685038832442103 ) ) ;
#27445 = CARTESIAN_POINT ( 'NONE',  ( 0.7543354620012772127, -0.1135047374312812413, 0.03937368211677726160 ) ) ;
#27446 = CARTESIAN_POINT ( 'NONE',  ( -0.8759842519685039353, -0.1574803149606299191, 0.7480314960629921295 ) ) ;
#27447 = CARTESIAN_POINT ( 'NONE',  ( 0.7646288533564489232, 0.1113553986120547346, 0.8513779527559054427 ) ) ;
#27448 = VECTOR ( 'NONE', #22978, 39.37007874015748143 ) ;
#27449 = CARTESIAN_POINT ( 'NONE',  ( -0.6971942568897648851, 0.07405724077823318263, 1.299212598371432215 ) ) ;
#27450 = CARTESIAN_POINT ( 'NONE',  ( 0.9873396505805591694, -0.1113553986120547346, 0.8612204723334173639 ) ) ;
#27451 = ORIENTED_EDGE ( 'NONE', *, *, #26901, .F. ) ;
#27452 = DIRECTION ( 'NONE',  ( 0.000000000000000000, -0.2432573283306595224, 0.9699617890481201377 ) ) ;
#27453 = CARTESIAN_POINT ( 'NONE',  ( 0.8759842519685039353, -0.1787899950787401882, 1.040846456639149764 ) ) ;
#27454 = ORIENTED_EDGE ( 'NONE', *, *, #44389, .F. ) ;
#27455 = CARTESIAN_POINT ( 'NONE',  ( -0.07405724077823318263, -1.390748031442299082, -0.1787899950787401604 ) ) ;
#27456 = CARTESIAN_POINT ( 'NONE',  ( -0.8107537697050253289, -0.1574803149606297803, 0.6176181101286932762 ) ) ;
#27457 = CARTESIAN_POINT ( 'NONE',  ( -0.7185039370078739607, 1.928577636452523993E-17, 1.210629921259842590 ) ) ;
#27458 = CARTESIAN_POINT ( 'NONE',  ( -1.033464566929133799, 0.000000000000000000, 1.062992125876724314 ) ) ;
#27459 = CARTESIAN_POINT ( 'NONE',  ( 0.1496320939568084596, 0.2091027599425386019, -0.3142669362052408211 ) ) ;
#27460 = CARTESIAN_POINT ( 'NONE',  ( 1.054774247047244540, -0.07405724077823318263, 0.1820866141194649179 ) ) ;
#27461 = CARTESIAN_POINT ( 'NONE',  ( 0.8759842519685039353, -0.1574803149606299191, 1.446850393593259732 ) ) ;
#27462 = VERTEX_POINT ( 'NONE', #40863 ) ;
#27463 = ORIENTED_EDGE ( 'NONE', *, *, #45870, .T. ) ;
#27464 = CARTESIAN_POINT ( 'NONE',  ( 1.033464566929133799, 0.000000000000000000, 1.102362204616881947 ) ) ;
#27465 = DIRECTION ( 'NONE',  ( -5.887603434621237738E-15, 0.7880107536067220142, -0.6156614753256581807 ) ) ;
#27466 = CARTESIAN_POINT ( 'NONE',  ( 1.002407869896990045, 0.1264236179284866091, 0.7012795275052913224 ) ) ;
#27467 = CARTESIAN_POINT ( 'NONE',  ( -0.9500414927467377701, -0.1787899950787401604, 1.628937007820252303 ) ) ;
#27468 = CARTESIAN_POINT ( 'NONE',  ( 0.1113553986120547346, -0.1899606298137326843, -0.1113553986120547346 ) ) ;
#27469 = ORIENTED_EDGE ( 'NONE', *, *, #12247, .T. ) ;
#27470 = CARTESIAN_POINT ( 'NONE',  ( 0.6195511811023618476, 0.8070866141732275789, 0.5854071585544579071 ) ) ;
#27471 = DIRECTION ( 'NONE',  ( 0.000000000000000000, 0.9771240687918550938, 0.2126700594527823895 ) ) ;
#27472 = CARTESIAN_POINT ( 'NONE',  ( 0.1787899950787401604, -1.140871999725301844, 0.07405724077823318263 ) ) ;
#27473 = ORIENTED_EDGE ( 'NONE', *, *, #40609, .F. ) ;
#27474 = CARTESIAN_POINT ( 'NONE',  ( -0.07405724077823318263, -0.1259842519147404416, -0.1787899950787401604 ) ) ;
#27475 = ORIENTED_EDGE ( 'NONE', *, *, #12527, .T. ) ;
#27476 = EDGE_CURVE ( 'NONE', #38318, #17227, #33498, .T. ) ;
#27477 = ORIENTED_EDGE ( 'NONE', *, *, #22672, .T. ) ;
#27478 = DIRECTION ( 'NONE',  ( 0.000000000000000000, 0.2126700594527800581, -0.9771240687918557599 ) ) ;
#27479 = DIRECTION ( 'NONE',  ( -1.000000000000000000, 3.469446951953613794E-15, 0.000000000000000000 ) ) ;
#27480 = ADVANCED_FACE ( 'NONE', ( #40401 ), #19071, .F. ) ;
#27481 = CIRCLE ( 'NONE', #39661, 0.009842519685039354330 ) ;
#27482 = CARTESIAN_POINT ( 'NONE',  ( 0.7185039370078746268, 0.06523048226347956391, 1.838090551181102539 ) ) ;
#27483 = CARTESIAN_POINT ( 'NONE',  ( -1.094772975963752103E-17, -0.6451771653005667906, -0.1787899950787401882 ) ) ;
#27484 = ADVANCED_FACE ( 'NONE', ( #10979 ), #853, .T. ) ;
#27485 = VECTOR ( 'NONE', #44439, 39.37007874015748143 ) ;
#27486 = EDGE_CURVE ( 'NONE', #11723, #14042, #3537, .T. ) ;
#27487 = CARTESIAN_POINT ( 'NONE',  ( -0.9500414927467377701, -0.1787899950787401604, 0.2952755904974176948 ) ) ;
#27488 = CARTESIAN_POINT ( 'NONE',  ( -0.9412147342319837628, -0.1574803149606297803, 0.9867125984251976512 ) ) ;
#27489 = CARTESIAN_POINT ( 'NONE',  ( 0.1797182628040039365, -1.123075305646037636, -2.200913952912460540E-17 ) ) ;
#27490 = CARTESIAN_POINT ( 'NONE',  ( 1.033464566929133799, 0.000000000000000000, 0.4035433070866141780 ) ) ;
#27491 = CARTESIAN_POINT ( 'NONE',  ( 0.6971942568897648851, 0.07405724077823318263, 1.146653543253323582 ) ) ;
#27492 = CARTESIAN_POINT ( 'NONE',  ( 0.9500414927467377701, 0.1787899950787401604, 0.1476377952218271561 ) ) ;
#27493 = CARTESIAN_POINT ( 'NONE',  ( 1.033464566929134687, 0.06523048226347956391, 1.626476377952756458 ) ) ;
#27495 = DIRECTION ( 'NONE',  ( -1.144917494144692682E-16, 5.091027988365947196E-31, -1.000000000000000000 ) ) ;
#27494 = CARTESIAN_POINT ( 'NONE',  ( 0.8087737571802944281, 0.1451870484244744686, 1.979707226920621066 ) ) ;
#27496 = CARTESIAN_POINT ( 'NONE',  ( 0.1638066838320702268, -0.08057055941993987447, -0.1395522756397764574 ) ) ;
#27497 = CARTESIAN_POINT ( 'NONE',  ( -0.1377952755905511584, 0.1574803149606320007, -0.9084645669291337988 ) ) ;
#27498 = CARTESIAN_POINT ( 'NONE',  ( -0.1113553986120547346, -0.7312992124908976876, -0.1113553986120547346 ) ) ;
#27499 = CARTESIAN_POINT ( 'NONE',  ( -0.7646288533564489232, -0.1113553986120547346, 1.638779527451527551 ) ) ;
#27500 = CARTESIAN_POINT ( 'NONE',  ( 0.9412147342319837628, -0.1574803149606297803, 1.656003937007873628 ) ) ;
#27501 = CARTESIAN_POINT ( 'NONE',  ( 0.6971942568897648851, 0.07405724077823318263, 1.023622047190330342 ) ) ;
#27502 = CARTESIAN_POINT ( 'NONE',  ( 0.8019270111902716547, 0.1787899950787401604, 1.850393700733638624 ) ) ;
#27503 = CARTESIAN_POINT ( 'NONE',  ( 1.033464566929134687, 0.06523048226347956391, 0.3567913384751500994 ) ) ;
#27504 = ORIENTED_EDGE ( 'NONE', *, *, #18556, .T. ) ;
#27505 = CARTESIAN_POINT ( 'NONE',  ( 0.7185039370078739607, 1.928577636452523993E-17, 1.240157480207432883 ) ) ;
#27506 = DIRECTION ( 'NONE',  ( -1.000000000000000000, 0.000000000000000000, 0.000000000000000000 ) ) ;
#27507 = CARTESIAN_POINT ( 'NONE',  ( -0.1574803149606299191, -1.631889763672000004, 0.000000000000000000 ) ) ;
#27508 = CARTESIAN_POINT ( 'NONE',  ( -0.7646288533564489232, -0.1113553986120547346, 0.2608267715460165226 ) ) ;
#27509 = CARTESIAN_POINT ( 'NONE',  ( 0.6971942568897648851, -0.07405724077823297447, 1.264763779473795813 ) ) ;
#27510 = CARTESIAN_POINT ( 'NONE',  ( 0.06648378651154265850, -0.08350519546685050698, 0.2470477387547700132 ) ) ;
#27511 = CARTESIAN_POINT ( 'NONE',  ( 0.1787899950787401604, 0.09547244099864542199, 0.07405724077823318263 ) ) ;
#27512 = DIRECTION ( 'NONE',  ( 0.3420201433256624401, 1.150791560227853721E-16, 0.9396926207859106484 ) ) ;
#27513 = AXIS2_PLACEMENT_3D ( 'NONE', #5593, #33677, #12336 ) ;
#27514 = CARTESIAN_POINT ( 'NONE',  ( -0.8019270111902717657, -0.1787899950787401604, 0.6003937007336380693 ) ) ;
#27515 = DIRECTION ( 'NONE',  ( -0.000000000000000000, 0.8660254037844384856, 0.5000000000000003331 ) ) ;
#27516 = CARTESIAN_POINT ( 'NONE',  ( 0.1574803149606299191, 0.1473293504822035527, -0.5595480905233944924 ) ) ;
#27517 = CYLINDRICAL_SURFACE ( 'NONE', #2532, 0.1787899950787401049 ) ;
#27518 = CARTESIAN_POINT ( 'NONE',  ( -0.07405724077823318263, -1.572834645615527327, 0.1787899950787401604 ) ) ;
#27519 = CARTESIAN_POINT ( 'NONE',  ( -1.054774247047244540, 0.07405724077823318263, 1.013779527505291878 ) ) ;
#27520 = CARTESIAN_POINT ( 'NONE',  ( -0.7185039370078746268, -0.06523048226347956391, 0.03198818897637801389 ) ) ;
#27521 = ORIENTED_EDGE ( 'NONE', *, *, #19646, .F. ) ;
#27522 = EDGE_CURVE ( 'NONE', #2766, #4172, #22613, .T. ) ;
#27523 = VECTOR ( 'NONE', #21411, 39.37007874015748143 ) ;
#27524 = CARTESIAN_POINT ( 'NONE',  ( -0.9500414927467378812, 0.1787899950787401604, 0.7431102361667091261 ) ) ;
#27525 = VERTEX_POINT ( 'NONE', #22202 ) ;
#27526 = DIRECTION ( 'NONE',  ( 0.000000000000000000, 0.000000000000000000, 1.000000000000000000 ) ) ;
#27527 = CARTESIAN_POINT ( 'NONE',  ( -0.1968503937007874127, 0.09275486626281861935, -0.1104648588920805335 ) ) ;
#27528 = CARTESIAN_POINT ( 'NONE',  ( 3.284318927891251994E-17, -0.6364428658670335803, 0.1787899950787401882 ) ) ;
#27529 = ORIENTED_EDGE ( 'NONE', *, *, #47454, .F. ) ;
#27530 = CARTESIAN_POINT ( 'NONE',  ( -0.04408878395971095598, -0.08956088549465768267, -0.1785915423567586424 ) ) ;
#27531 = CARTESIAN_POINT ( 'NONE',  ( 0.7185039370078739607, 1.928577636452523993E-17, 1.919291338582677309 ) ) ;
#27532 = EDGE_CURVE ( 'NONE', #30877, #5618, #1424, .T. ) ;
#27533 = ORIENTED_EDGE ( 'NONE', *, *, #39094, .F. ) ;
#27534 = CARTESIAN_POINT ( 'NONE',  ( -0.07117121207836790697, -0.08956324299011318713, 0.1404802767937309016 ) ) ;
#27535 = CARTESIAN_POINT ( 'NONE',  ( -0.8759842519685039353, 0.1787899950787401882, 0.4650590550643464716 ) ) ;
#27536 = CARTESIAN_POINT ( 'NONE',  ( 0.000000000000000000, 0.1473293504822035527, -0.9532488779249704836 ) ) ;
#27537 = EDGE_LOOP ( 'NONE', ( #15128, #19259 ) ) ;
#27538 = CARTESIAN_POINT ( 'NONE',  ( -0.9500414927467377701, 0.1787899950787401604, 1.687992125930489307 ) ) ;
#27539 = CARTESIAN_POINT ( 'NONE',  ( -0.1264236179284866091, -1.427657480261196987, -0.1264236179284866091 ) ) ;
#27540 = CARTESIAN_POINT ( 'NONE',  ( -0.7185039370078739607, 1.928577636452523993E-17, 0.8464566928058583350 ) ) ;
#27541 = CIRCLE ( 'NONE', #45095, 0.08090551181102362266 ) ;
#27542 = CARTESIAN_POINT ( 'NONE',  ( 0.1633669211492204676, -0.08028893826450952953, 0.1390634969805222276 ) ) ;
#27543 = CARTESIAN_POINT ( 'NONE',  ( -1.100456976456230270E-17, -0.7195319985594232914, -0.1797182628040039365 ) ) ;
#27544 = CARTESIAN_POINT ( 'NONE',  ( 0.7185039370078760701, -0.06523048226348075740, 0.9375000000000002220 ) ) ;
#27545 = CARTESIAN_POINT ( 'NONE',  ( -0.9412147342319837628, -0.1574803149606297803, 1.213090551073576107 ) ) ;
#27547 = FACE_OUTER_BOUND ( 'NONE', #13364, .T. ) ;
#27546 = CARTESIAN_POINT ( 'NONE',  ( -0.06523048226347956391, -0.4926181102362205966, 0.1574803149606297803 ) ) ;
#27548 = CARTESIAN_POINT ( 'NONE',  ( -0.8759842519685039353, 0.1574803149606299191, 1.190944881782236342 ) ) ;
#27549 = ORIENTED_EDGE ( 'NONE', *, *, #23511, .F. ) ;
#27550 = CARTESIAN_POINT ( 'NONE',  ( 0.9873396505805591694, 0.1113553986120547346, 1.579724409341291214 ) ) ;
#27551 = CARTESIAN_POINT ( 'NONE',  ( -0.8019270111902716547, 0.1787899950787401604, 1.102362204670646495 ) ) ;
#27552 = CARTESIAN_POINT ( 'NONE',  ( 1.033464566929133799, 0.000000000000000000, 1.151574803149606474 ) ) ;
#27554 = CYLINDRICAL_SURFACE ( 'NONE', #2501, 0.09842519685039370636 ) ;
#27553 = FACE_OUTER_BOUND ( 'NONE', #8627, .T. ) ;
#27555 = AXIS2_PLACEMENT_3D ( 'NONE', #31279, #35340, #2482 ) ;
#27556 = CARTESIAN_POINT ( 'NONE',  ( 0.000000000000000000, 0.000000000000000000, -0.04012007874015743186 ) ) ;
#27557 = CARTESIAN_POINT ( 'NONE',  ( -9.642888182262618425E-18, -0.5787401573727873894, -0.1574803149606299191 ) ) ;
#27558 = ( BOUNDED_CURVE ( )  B_SPLINE_CURVE ( 2, ( #25284, #334, #8002, #32730, #11380, #22627, #25991, #7303, #22380 ),
 .UNSPECIFIED., .F., .F. ) 
 B_SPLINE_CURVE_WITH_KNOTS ( ( 3, 2, 2, 2, 3 ),
 ( 0.3900000000000000133, 0.3925000000000000155, 0.3950000000000000178, 0.3975000000000000200, 0.4000000000000000222 ),
 .UNSPECIFIED. ) 
 CURVE ( )  GEOMETRIC_REPRESENTATION_ITEM ( )  RATIONAL_B_SPLINE_CURVE ( ( 1.000000000000000000, 0.9238795325112869605, 1.000000000000000000, 0.9238795325112869605, 1.000000000000000000, 0.9238795325112869605, 1.000000000000000000, 0.9238795325112869605, 1.000000000000000000 ) ) 
 REPRESENTATION_ITEM ( '' )  ) ;
#27560 = CYLINDRICAL_SURFACE ( 'NONE', #10947, 0.09842519685039370636 ) ;
#27559 = CARTESIAN_POINT ( 'NONE',  ( 0.8759842519685039353, 0.1574803149606299191, 0.1771653543307086520 ) ) ;
#27561 = CARTESIAN_POINT ( 'NONE',  ( 1.033464566929134687, 0.06523048226347956391, 1.262303149498772425 ) ) ;
#27562 = CARTESIAN_POINT ( 'NONE',  ( -0.07405724077823318263, -0.5836614172690718361, 0.1787899950787401604 ) ) ;
#27563 = DIRECTION ( 'NONE',  ( 0.000000000000000000, 0.000000000000000000, -1.000000000000000000 ) ) ;
#27564 = ORIENTED_EDGE ( 'NONE', *, *, #18438, .T. ) ;
#27565 = CARTESIAN_POINT ( 'NONE',  ( -0.9500414927467378812, 0.1787899950787401604, 1.058070866087969186 ) ) ;
#27566 = CARTESIAN_POINT ( 'NONE',  ( 0.6971942568897626646, 0.07405724077823318263, 0.8267716534895444003 ) ) ;
#27567 = DIRECTION ( 'NONE',  ( 1.822029033848725028E-16, 0.000000000000000000, 1.000000000000000000 ) ) ;
#27568 = CARTESIAN_POINT ( 'NONE',  ( 0.7646288533564489232, -0.1113553986120547346, 0.9005905511811023167 ) ) ;
#27569 = CARTESIAN_POINT ( 'NONE',  ( -0.1787899950787401882, -1.654035433017102319, 0.000000000000000000 ) ) ;
#27570 = CARTESIAN_POINT ( 'NONE',  ( 0.1264236179284866091, -1.043799212544661348, -0.1264236179284866091 ) ) ;
#27571 = CARTESIAN_POINT ( 'NONE',  ( -0.1113553986120547346, -1.321850393700787496, 0.1113553986120547346 ) ) ;
#27572 = LINE ( 'NONE', #34495, #13016 ) ;
#27573 = ORIENTED_EDGE ( 'NONE', *, *, #31586, .F. ) ;
#27574 = EDGE_LOOP ( 'NONE', ( #7478, #2591, #37340, #38910 ) ) ;
#27575 = CARTESIAN_POINT ( 'NONE',  ( -0.7495606340400177148, -0.1264236179284866091, 1.980807086560409491 ) ) ;
#27576 = CARTESIAN_POINT ( 'NONE',  ( 0.6971942568897637749, 2.189545951927499583E-17, 1.818405511757259729 ) ) ;
#27577 = VERTEX_POINT ( 'NONE', #29229 ) ;
#27578 = CARTESIAN_POINT ( 'NONE',  ( 0.7185039370078739607, 1.928577636452523993E-17, 1.761811023622047223 ) ) ;
#27579 = CARTESIAN_POINT ( 'NONE',  ( 0.7495606340400177148, 0.1264236179284866091, 0.4355314960092284138 ) ) ;
#27580 = CARTESIAN_POINT ( 'NONE',  ( -0.8759842519685039353, -0.1787899950787401882, 1.311515747977732405 ) ) ;
#27581 = CARTESIAN_POINT ( 'NONE',  ( 1.033464566929133799, 1.928577636452524610E-17, 4.498031496062992574 ) ) ;
#27582 = EDGE_CURVE ( 'NONE', #26592, #38268, #42476, .T. ) ;
#27583 = CARTESIAN_POINT ( 'NONE',  ( -0.6971942568897648851, -0.07405724077823297447, 0.9891732282926934960 ) ) ;
#27584 = CARTESIAN_POINT ( 'NONE',  ( -1.054774247047244096, 0.000000000000000000, 0.3026574802611972648 ) ) ;
#27585 = ( BOUNDED_CURVE ( )  B_SPLINE_CURVE ( 2, ( #33406, #5073, #36972, #11818, #25958, #40539, #23301, #7728, #44370 ),
 .UNSPECIFIED., .F., .F. ) 
 B_SPLINE_CURVE_WITH_KNOTS ( ( 3, 2, 2, 2, 3 ),
 ( 0.4199999999999999845, 0.4224999999999999867, 0.4249999999999999889, 0.4274999999999999911, 0.4299999999999999933 ),
 .UNSPECIFIED. ) 
 CURVE ( )  GEOMETRIC_REPRESENTATION_ITEM ( )  RATIONAL_B_SPLINE_CURVE ( ( 1.000000000000000000, 0.9238795325112869605, 1.000000000000000000, 0.9238795325112869605, 1.000000000000000000, 0.9238795325112869605, 1.000000000000000000, 0.9238795325112869605, 1.000000000000000000 ) ) 
 REPRESENTATION_ITEM ( '' )  ) ;
#27586 = ADVANCED_FACE ( 'NONE', ( #29692 ), #35856, .T. ) ;
#27587 = AXIS2_PLACEMENT_3D ( 'NONE', #3302, #32803, #43313 ) ;
#27588 = CARTESIAN_POINT ( 'NONE',  ( -0.1944374611862008662, 0.07559918600398901622, -0.1731745503097413541 ) ) ;
#27589 = CARTESIAN_POINT ( 'NONE',  ( -0.9500414927467378812, 0.1787899950787401604, 1.766732283410803461 ) ) ;
#27590 = CARTESIAN_POINT ( 'NONE',  ( 0.7185039370078778465, -0.06523048226348396317, 1.400098425089323140 ) ) ;
#27591 = CARTESIAN_POINT ( 'NONE',  ( -0.8107537697050253289, -0.1574803149606297803, 1.729822834645670548 ) ) ;
#27592 = DIRECTION ( 'NONE',  ( 0.000000000000000000, 0.000000000000000000, -1.000000000000000000 ) ) ;
#27593 = CARTESIAN_POINT ( 'NONE',  ( -0.1787899950787401882, -0.2525845981504984405, 0.000000000000000000 ) ) ;
#27594 = CARTESIAN_POINT ( 'NONE',  ( 0.7495606340400177148, -0.1264236179284866091, 1.705216535379307174 ) ) ;
#27595 = CARTESIAN_POINT ( 'NONE',  ( -0.01791361388587468795, -0.09842519685039370636, 0.2243562948544858549 ) ) ;
#27596 = CARTESIAN_POINT ( 'NONE',  ( -0.7646288533564489232, -0.1113553986120547346, 0.7332677164279054471 ) ) ;
#27597 = EDGE_CURVE ( 'NONE', #44020, #5354, #20788, .T. ) ;
#27598 = EDGE_CURVE ( 'NONE', #22876, #32133, #36642, .T. ) ;
#27599 = ORIENTED_EDGE ( 'NONE', *, *, #141, .T. ) ;
#27600 = VERTEX_POINT ( 'NONE', #31311 ) ;
#27601 = CARTESIAN_POINT ( 'NONE',  ( -0.7495606340400177148, -0.1264236179284866091, 1.154035433017102319 ) ) ;
#27602 = CARTESIAN_POINT ( 'NONE',  ( 0.1787899950787401882, -1.048720472387181024, -2.189545951927503898E-17 ) ) ;
#27603 = CARTESIAN_POINT ( 'NONE',  ( -0.07405724077823318263, -1.188976377898991688, -0.1787899950787401604 ) ) ;
#27604 = CARTESIAN_POINT ( 'NONE',  ( 0.2519685039370078705, -0.08090551181102362266, 0.000000000000000000 ) ) ;
#27605 = LENGTH_MEASURE_WITH_UNIT ( LENGTH_MEASURE( 0.02539999999999999897 ), #5761 ) ;
#27606 = CARTESIAN_POINT ( 'NONE',  ( -1.100456976456230270E-17, -0.4439414473783212522, -0.1797182628040039365 ) ) ;
#27607 = CARTESIAN_POINT ( 'NONE',  ( 0.06523048226347956391, 0.07824803149606307517, -0.1574803149606300301 ) ) ;
#27608 = CARTESIAN_POINT ( 'NONE',  ( 0.8759842519685039353, 0.1787899950787401882, 0.9768700786863937502 ) ) ;
#27609 = AXIS2_PLACEMENT_3D ( 'NONE', #4824, #37913, #18345 ) ;
#27611 = CARTESIAN_POINT ( 'NONE',  ( 0.004280036809617362818, 0.09642780928091415626, 0.1085877958707450186 ) ) ;
#27610 = CARTESIAN_POINT ( 'NONE',  ( 0.8759842519685039353, 0.1574803149606299191, 0.6102362204724409711 ) ) ;
#27612 = CARTESIAN_POINT ( 'NONE',  ( 0.9412147342319837628, 0.1574803149606300301, 0.04675196839640998608 ) ) ;
#27613 = ORIENTED_EDGE ( 'NONE', *, *, #24792, .T. ) ;
#27614 = CARTESIAN_POINT ( 'NONE',  ( 1.033464566929134687, -0.06523048226347956391, 0.2042322834645668717 ) ) ;
#27615 = CARTESIAN_POINT ( 'NONE',  ( 0.7646288533564489232, 0.1113553986120547346, 0.7234251967428662056 ) ) ;
#27616 = CARTESIAN_POINT ( 'NONE',  ( 0.07405724077823318263, -0.5049212597887556830, 0.1787899950787401604 ) ) ;
#27617 = CARTESIAN_POINT ( 'NONE',  ( -0.005244590715618953347, 1.099487083487562522, -0.04739565599252126837 ) ) ;
#27618 = AXIS2_PLACEMENT_3D ( 'NONE', #21773, #2825, #43085 ) ;
#27619 = CARTESIAN_POINT ( 'NONE',  ( -0.07405724077823318263, -1.464566929080096225, -0.1787899950787401604 ) ) ;
#27620 = CARTESIAN_POINT ( 'NONE',  ( 1.054774247047244096, 0.000000000000000000, 0.3813976377415121966 ) ) ;
#27621 = DIRECTION ( 'NONE',  ( 1.000000000000000000, 0.000000000000000000, -1.822029033848725275E-16 ) ) ;
#27622 = CARTESIAN_POINT ( 'NONE',  ( -1.002407869896990045, 0.1264236179284866091, 1.956200787347811110 ) ) ;
#27623 = EDGE_LOOP ( 'NONE', ( #34280, #21169, #44109, #32156, #8118 ) ) ;
#27624 = VERTEX_POINT ( 'NONE', #27017 ) ;
#27625 = CARTESIAN_POINT ( 'NONE',  ( -0.8759842519685039353, 0.1787899950787401882, 1.493602362150960650 ) ) ;
#27626 = CARTESIAN_POINT ( 'NONE',  ( 0.3302522695077432791, 4.466152701071653354E-17, 0.000000000000000000 ) ) ;
#27627 = CARTESIAN_POINT ( 'NONE',  ( 0.9500414927467378812, -0.1787899950787401604, 1.476377952702141449 ) ) ;
#27628 = PLANE ( 'NONE',  #47401 ) ;
#27629 = CARTESIAN_POINT ( 'NONE',  ( -0.9500414927467378812, -0.1787899950787401604, 0.6889763778989935750 ) ) ;
#27630 = CARTESIAN_POINT ( 'NONE',  ( 0.6971942568897626646, 0.07405724077823318263, 0.1230314960092287191 ) ) ;
#27631 = CARTESIAN_POINT ( 'NONE',  ( -0.8019270111902717657, -0.1787899950787401604, 1.190944881836001112 ) ) ;
#27632 = CARTESIAN_POINT ( 'NONE',  ( 0.1327893737652135475, -0.09842568101169199557, -0.1197263300370822597 ) ) ;
#27633 = DIRECTION ( 'NONE',  ( 1.000000000000000000, -3.469446951953625627E-15, -0.000000000000000000 ) ) ;
#27634 = CARTESIAN_POINT ( 'NONE',  ( 0.7495606340400177148, -0.1264236179284866091, 0.5634842519147401640 ) ) ;
#27635 = CARTESIAN_POINT ( 'NONE',  ( -0.8019270111902716547, 0.1787899950787401604, 0.5462598424659214080 ) ) ;
#27636 = CARTESIAN_POINT ( 'NONE',  ( -0.7185039370078739607, 1.928577636452523993E-17, 0.2952755904436539236 ) ) ;
#27637 = EDGE_CURVE ( 'NONE', #25679, #42397, #40442, .T. ) ;
#27638 = CARTESIAN_POINT ( 'NONE',  ( 0.7185039370078692977, 0.06523048226347515077, 1.670767716427905780 ) ) ;
#27639 = EDGE_LOOP ( 'NONE', ( #19222, #46154, #26322 ) ) ;
#27640 = VERTEX_POINT ( 'NONE', #15753 ) ;
#27641 = CARTESIAN_POINT ( 'NONE',  ( -1.033464566929134687, -0.06523048226347956391, 0.3223425196850393526 ) ) ;
#27642 = CARTESIAN_POINT ( 'NONE',  ( 0.9500414927467377701, 0.1787899950787401604, 1.294291338528913204 ) ) ;
#27643 = CARTESIAN_POINT ( 'NONE',  ( 0.1605511194595065083, -0.09851384859890432999, 0.1447744158249297253 ) ) ;
#27644 = ORIENTED_EDGE ( 'NONE', *, *, #11875, .F. ) ;
#27645 = EDGE_CURVE ( 'NONE', #44070, #3164, #2728, .T. ) ;
#27646 = CARTESIAN_POINT ( 'NONE',  ( -0.7185039370078746268, -0.06523048226347956391, 0.5437992125984247860 ) ) ;
#27647 = CARTESIAN_POINT ( 'NONE',  ( -0.6971942568897637749, 2.189545951927499583E-17, 0.9128937007336377363 ) ) ;
#27648 = CARTESIAN_POINT ( 'NONE',  ( -1.094772975963752103E-17, -1.601009795000891911, -0.1787899950787401882 ) ) ;
#27649 = ORIENTED_EDGE ( 'NONE', *, *, #5061, .F. ) ;
#27650 = CYLINDRICAL_SURFACE ( 'NONE', #21179, 0.1574803149606299191 ) ;
#27651 = CARTESIAN_POINT ( 'NONE',  ( 0.07405724077823318263, -0.5787401574265509385, 0.1787899950787401604 ) ) ;
#27652 = CARTESIAN_POINT ( 'NONE',  ( -0.7646288533564489232, -0.1113553986120547346, 0.07381889763779526936 ) ) ;
#27653 = ORIENTED_EDGE ( 'NONE', *, *, #38521, .F. ) ;
#27654 = CARTESIAN_POINT ( 'NONE',  ( 0.6971942568897648851, -0.07405724077823297447, 1.461614173174583753 ) ) ;
#27655 = VECTOR ( 'NONE', #32263, 39.37007874015748143 ) ;
#27656 = CARTESIAN_POINT ( 'NONE',  ( -0.1089815878282069106, 0.2325720113816387991, -0.3144321013757216399 ) ) ;
#27657 = CARTESIAN_POINT ( 'NONE',  ( -0.1787899950787401604, -0.3622047243556850704, -0.07405724077823318263 ) ) ;
#27658 = CARTESIAN_POINT ( 'NONE',  ( -0.1787899950787401604, -0.7509842519147402751, -0.07405724077823318263 ) ) ;
#27659 = CARTESIAN_POINT ( 'NONE',  ( 0.8759842519685039353, 0.1574803149606299191, 1.820866141624755796 ) ) ;
#27660 = AXIS2_PLACEMENT_3D ( 'NONE', #32557, #18608, #11679 ) ;
#27661 = CARTESIAN_POINT ( 'NONE',  ( 0.1787899950787401604, 0.04515162232194235709, -0.07405724077823318263 ) ) ;
#27662 = CARTESIAN_POINT ( 'NONE',  ( 0.07405724077823318263, 0.1250000000537635492, 0.1787899950787401604 ) ) ;
#27663 = CARTESIAN_POINT ( 'NONE',  ( 0.2821522309711287368, -0.08090551181102362266, 1.098083891755157578E-17 ) ) ;
#27664 = CARTESIAN_POINT ( 'NONE',  ( -0.8759842519685039353, 0.1787899950787401882, 0.7455708660879684091 ) ) ;
#27666 = DIRECTION ( 'NONE',  ( -1.000000000000000000, 0.000000000000000000, 0.000000000000000000 ) ) ;
#27665 = CARTESIAN_POINT ( 'NONE',  ( -0.1574803149606299191, -0.9724409448818898127, 0.000000000000000000 ) ) ;
#27668 = CARTESIAN_POINT ( 'NONE',  ( -0.8039169694696064461, -0.1563771033850889780, 1.986832772479788956 ) ) ;
#27667 = CARTESIAN_POINT ( 'NONE',  ( 0.1797182628040039365, -1.634886329268084637, -2.200913952912460540E-17 ) ) ;
#27669 = CARTESIAN_POINT ( 'NONE',  ( 0.1787899950787401604, -0.3720472440407247561, -0.07405724077823318263 ) ) ;
#27670 = CARTESIAN_POINT ( 'NONE',  ( -1.033464566929134687, 0.06523048226347956391, 1.026082677057828185 ) ) ;
#27671 = CARTESIAN_POINT ( 'NONE',  ( 0.8759842519685039353, 0.1787899950787401882, 1.454232283410803017 ) ) ;
#27672 = CARTESIAN_POINT ( 'NONE',  ( 0.1378230750848531139, 0.09774221684002680488, -0.2058608813653597380 ) ) ;
#27673 = CARTESIAN_POINT ( 'NONE',  ( 0.8759842519685039353, 0.1787899950787401882, 0.4256889763241890057 ) ) ;
#27675 = EDGE_LOOP ( 'NONE', ( #15655, #23291, #7196, #26514, #24784, #37505 ) ) ;
#27674 = FACE_OUTER_BOUND ( 'NONE', #18983, .T. ) ;
#27676 = DIRECTION ( 'NONE',  ( 1.822029033848725028E-16, 0.000000000000000000, 1.000000000000000000 ) ) ;
#27678 = CARTESIAN_POINT ( 'NONE',  ( 0.1787899950787401604, 0.01181102367581077402, 0.07405724077823318263 ) ) ;
#27677 = CARTESIAN_POINT ( 'NONE',  ( 0.1574803149606300301, -0.8617125983176697757, -0.06523048226347956391 ) ) ;
#27679 = CARTESIAN_POINT ( 'NONE',  ( 0.6971942568897626646, 0.07405724077823318263, 0.3937007873478115538 ) ) ;
#27680 = CARTESIAN_POINT ( 'NONE',  ( -0.1264236179284866091, -0.9010826771115905132, 0.1264236179284866091 ) ) ;
#27681 = FACE_OUTER_BOUND ( 'NONE', #26018, .T. ) ;
#27682 = VECTOR ( 'NONE', #12690, 39.37007874015748143 ) ;
#27683 = DIRECTION ( 'NONE',  ( -3.478357113474434231E-15, -1.000000000000000000, 0.000000000000000000 ) ) ;
#27684 = CARTESIAN_POINT ( 'NONE',  ( -0.7495606340400177148, -0.1264236179284866091, 1.385334645615527549 ) ) ;
#27685 = CARTESIAN_POINT ( 'NONE',  ( 0.7185039370078739607, 1.928577636452523993E-17, 0.8464566928058583350 ) ) ;
#27686 = ORIENTED_EDGE ( 'NONE', *, *, #44499, .T. ) ;
#27687 = DIRECTION ( 'NONE',  ( -1.000000000000000000, 0.000000000000000000, 0.000000000000000000 ) ) ;
#27688 = CARTESIAN_POINT ( 'NONE',  ( 1.002407869896990045, -0.1264236179284866091, 1.045767716481669440 ) ) ;
#27689 = ORIENTED_EDGE ( 'NONE', *, *, #47327, .T. ) ;
#27690 = CARTESIAN_POINT ( 'NONE',  ( -1.094772975963752103E-17, -1.393208661363559031, -0.1787899950787401882 ) ) ;
#27691 = CARTESIAN_POINT ( 'NONE',  ( -0.9412147342319837628, 0.1574803149606300301, 0.6373031494987718704 ) ) ;
#27692 = AXIS2_PLACEMENT_3D ( 'NONE', #6325, #42031, #20945 ) ;
#27693 = DIRECTION ( 'NONE',  ( 0.000000000000000000, 0.000000000000000000, 1.000000000000000000 ) ) ;
#27694 = CARTESIAN_POINT ( 'NONE',  ( 1.002407869896990045, 0.1264236179284866091, 1.680610236166708793 ) ) ;
#27695 = CARTESIAN_POINT ( 'NONE',  ( -0.7646288533564489232, 0.1113553986120547346, 1.323818897637795367 ) ) ;
#27697 = DIRECTION ( 'NONE',  ( -1.000000000000000000, 0.000000000000000000, 0.000000000000000000 ) ) ;
#27696 = CYLINDRICAL_SURFACE ( 'NONE', #28831, 0.1574803149606299191 ) ;
#27698 = CARTESIAN_POINT ( 'NONE',  ( 0.7495606340400177148, -0.1264236179284866091, 0.2091535432533232486 ) ) ;
#27699 = CARTESIAN_POINT ( 'NONE',  ( -0.6971942568897626646, 0.07405724077823318263, 0.1181102361667090567 ) ) ;
#27700 = CIRCLE ( 'NONE', #39088, 0.1574803149606300579 ) ;
#27701 = CARTESIAN_POINT ( 'NONE',  ( 0.7185039370078746268, -0.06523048226347956391, 1.400098425089323140 ) ) ;
#27702 = EDGE_LOOP ( 'NONE', ( #186, #5371, #24352, #17147 ) ) ;
#27703 = ORIENTED_EDGE ( 'NONE', *, *, #39963, .T. ) ;
#27704 = ( BOUNDED_CURVE ( )  B_SPLINE_CURVE ( 2, ( #34038, #12466, #40692, #40927, #1163, #44531, #1395, #30447, #16055 ),
 .UNSPECIFIED., .F., .T. ) 
 B_SPLINE_CURVE_WITH_KNOTS ( ( 3, 2, 2, 2, 3 ),
 ( 0.6400000000000000133, 0.6424999999999999600, 0.6450000000000000178, 0.6474999999999999645, 0.6500000000000000222 ),
 .UNSPECIFIED. ) 
 CURVE ( )  GEOMETRIC_REPRESENTATION_ITEM ( )  RATIONAL_B_SPLINE_CURVE ( ( 1.000000000000000000, 0.9238795325112869605, 1.000000000000000000, 0.9238795325112869605, 1.000000000000000000, 0.9238795325112869605, 1.000000000000000000, 0.9238795325112869605, 1.000000000000000000 ) ) 
 REPRESENTATION_ITEM ( '' )  ) ;
#27705 = EDGE_CURVE ( 'NONE', #20094, #26504, #23633, .T. ) ;
#27706 = CARTESIAN_POINT ( 'NONE',  ( -0.05938635157341645016, -0.07958416565545690935, -0.2511462791696849051 ) ) ;
#27707 = ORIENTED_EDGE ( 'NONE', *, *, #36274, .F. ) ;
#27708 = CARTESIAN_POINT ( 'NONE',  ( -0.7495606340400177148, -0.1264236179284866091, 1.660925196796630088 ) ) ;
#27709 = VERTEX_POINT ( 'NONE', #12395 ) ;
#27710 = DIRECTION ( 'NONE',  ( -0.000000000000000000, 1.000000000000000000, -0.000000000000000000 ) ) ;
#27711 = CARTESIAN_POINT ( 'NONE',  ( 0.1264236179284866091, -1.064592472166246084, 0.1264236179284866091 ) ) ;
#27712 = VERTEX_POINT ( 'NONE', #4932 ) ;
#27713 = CARTESIAN_POINT ( 'NONE',  ( 0.07405724077823318263, -0.1702755904974175283, -0.1787899950787401604 ) ) ;
#27714 = ORIENTED_EDGE ( 'NONE', *, *, #41797, .F. ) ;
#27715 = CARTESIAN_POINT ( 'NONE',  ( -0.9873396505805591694, -0.1113553986120547346, 1.412401574695621997 ) ) ;
#27716 = CARTESIAN_POINT ( 'NONE',  ( -1.033464566929134687, -0.06523048226347956391, 1.464074803149607140 ) ) ;
#27717 = CIRCLE ( 'NONE', #37632, 0.1377952755905509641 ) ;
#27718 = CARTESIAN_POINT ( 'NONE',  ( 0.8759842519685039353, -0.1574803149606299191, 1.850393700787401619 ) ) ;
#27719 = AXIS2_PLACEMENT_3D ( 'NONE', #28108, #42668, #16822 ) ;
#27720 = VECTOR ( 'NONE', #7309, 39.37007874015748143 ) ;
#27721 = CARTESIAN_POINT ( 'NONE',  ( 0.1787899950787401604, -0.5787401574265509385, 0.07405724077823318263 ) ) ;
#27722 = VECTOR ( 'NONE', #42102, 39.37007874015748143 ) ;
#27723 = EDGE_CURVE ( 'NONE', #21023, #24385, #45889, .T. ) ;
#27724 = CARTESIAN_POINT ( 'NONE',  ( -0.8759842519685039353, 0.1787899950787401882, 0.3124999999462365619 ) ) ;
#27725 = CARTESIAN_POINT ( 'NONE',  ( -0.9412147342319837628, 0.1574803149606300301, 1.080216535433071501 ) ) ;
#27726 = CARTESIAN_POINT ( 'NONE',  ( 0.07444174185955046430, -1.155063494622414977, -0.1797182628040039087 ) ) ;
#27727 = CARTESIAN_POINT ( 'NONE',  ( -0.1528603379500407256, 0.2072402749985339798, -0.03001342526389673415 ) ) ;
#27728 = CARTESIAN_POINT ( 'NONE',  ( 0.8019270111902717657, -0.1787899950787401604, 1.077755905458048113 ) ) ;
#27729 = CARTESIAN_POINT ( 'NONE',  ( 1.002407869896990045, -0.1264236179284866091, 1.395177165300567124 ) ) ;
#27730 = CARTESIAN_POINT ( 'NONE',  ( 0.8107537697050234415, -0.1574803149606297803, 0.2337598425196851515 ) ) ;
#27731 = CARTESIAN_POINT ( 'NONE',  ( 0.7646288533564489232, 0.1113553986120547346, 1.599409448818897683 ) ) ;
#27733 = CARTESIAN_POINT ( 'NONE',  ( 0.4620708661417328167, 0.1864803149606299448, -0.7135826771653542844 ) ) ;
#27732 = CARTESIAN_POINT ( 'NONE',  ( 0.8217027200616507931, 0.1498728102447202670, 1.979429313789683453 ) ) ;
#27734 = CARTESIAN_POINT ( 'NONE',  ( -1.033464566929133799, 0.000000000000000000, 1.968503936900346529 ) ) ;
#27735 = CARTESIAN_POINT ( 'NONE',  ( 3.284318927891251994E-17, 0.1274606299750234428, 0.1787899950787401882 ) ) ;
#27736 = LINE ( 'NONE', #42302, #34523 ) ;
#27737 = CARTESIAN_POINT ( 'NONE',  ( 1.054774247047244096, 0.000000000000000000, 0.9670275590013542866 ) ) ;
#27738 = CARTESIAN_POINT ( 'NONE',  ( 0.6971942568897648851, 0.07405724077823318263, 1.973425196796630088 ) ) ;
#27739 = CARTESIAN_POINT ( 'NONE',  ( -0.8759842519685039353, -0.1787899950787401882, 1.154035433017102319 ) ) ;
#27740 = CARTESIAN_POINT ( 'NONE',  ( 0.8107537697050234415, -0.1574803149606297803, 0.3026574802074335491 ) ) ;
#27741 = ORIENTED_EDGE ( 'NONE', *, *, #7200, .T. ) ;
#27742 = EDGE_CURVE ( 'NONE', #5728, #5617, #38009, .T. ) ;
#27743 = CARTESIAN_POINT ( 'NONE',  ( -0.7185039370078739607, 0.000000000000000000, -2.869337061179095023E-17 ) ) ;
#27744 = CARTESIAN_POINT ( 'NONE',  ( 1.032458411528080156, 0.03144513627025335295, 0.03936974531083359263 ) ) ;
#27745 = CARTESIAN_POINT ( 'NONE',  ( 1.033464566929134687, 0.06523048226347956391, 0.2485236220472441526 ) ) ;
#27746 = CARTESIAN_POINT ( 'NONE',  ( 0.1574803149606299191, -1.651574803042078710, -1.928577636452523993E-17 ) ) ;
#27747 = CARTESIAN_POINT ( 'NONE',  ( -1.033464566929134687, 0.06523048226347956391, 0.3174212597349925224 ) ) ;
#27748 = CARTESIAN_POINT ( 'NONE',  ( 0.005686768416161533217, -0.1458881524272479802, 0.02291217744961116659 ) ) ;
#27749 = AXIS2_PLACEMENT_3D ( 'NONE', #46711, #2392, #43592 ) ;
#27750 = ORIENTED_EDGE ( 'NONE', *, *, #32438, .T. ) ;
#27751 = CARTESIAN_POINT ( 'NONE',  ( 0.1574803149606299746, 0.000000000000000000, -0.2952755905511806334 ) ) ;
#27752 = CARTESIAN_POINT ( 'NONE',  ( -9.642888182262618425E-18, -1.769685039370078705, -0.1574803149606299191 ) ) ;
#27753 = CARTESIAN_POINT ( 'NONE',  ( 0.1822895153388602307, 2.589602477342551251E-17, 0.2114570894355444486 ) ) ;
#27754 = VECTOR ( 'NONE', #36136, 39.37007874015748143 ) ;
#27755 = ADVANCED_FACE ( 'NONE', ( #9250 ), #34422, .T. ) ;
#27756 = CARTESIAN_POINT ( 'NONE',  ( -0.7495606340400177148, -0.1264236179284866091, 0.5585629920722204877 ) ) ;
#27757 = CARTESIAN_POINT ( 'NONE',  ( 0.7185039370078739607, 1.928577636452523993E-17, 1.240157480207432883 ) ) ;
#27758 = CARTESIAN_POINT ( 'NONE',  ( -0.05613986198065470251, 0.07767250275969882212, 0.2530207064393422689 ) ) ;
#27759 = ORIENTED_EDGE ( 'NONE', *, *, #25783, .F. ) ;
#27760 = ORIENTED_EDGE ( 'NONE', *, *, #35938, .T. ) ;
#27762 = CARTESIAN_POINT ( 'NONE',  ( 0.1264236179284866091, -1.722933070812378009, 0.1264236179284866091 ) ) ;
#27761 = CARTESIAN_POINT ( 'NONE',  ( 0.1113553986120547346, -0.4261811022546779792, -0.1113553986120547346 ) ) ;
#27763 = CARTESIAN_POINT ( 'NONE',  ( -1.054774247047244540, 0.07405724077823318263, 0.9350393700249758355 ) ) ;
#27764 = VECTOR ( 'NONE', #535, 39.37007874015748143 ) ;
#27765 = AXIS2_PLACEMENT_3D ( 'NONE', #36722, #8178, #981 ) ;
#27766 = ORIENTED_EDGE ( 'NONE', *, *, #27183, .F. ) ;
#27767 = CARTESIAN_POINT ( 'NONE',  ( -1.002407869896990045, 0.1264236179284866091, 0.6225393700249762796 ) ) ;
#27768 = ORIENTED_EDGE ( 'NONE', *, *, #44860, .F. ) ;
#27769 = CARTESIAN_POINT ( 'NONE',  ( -1.003767390250174765E-17, 0.006751761263662639685, -0.1377952755905511861 ) ) ;
#27770 = CARTESIAN_POINT ( 'NONE',  ( -0.1264236179284866091, -0.6807342044497107780, 0.1264236179284866091 ) ) ;
#27771 = VECTOR ( 'NONE', #33267, 39.37007874015748143 ) ;
#27772 = EDGE_LOOP ( 'NONE', ( #3624, #13933, #892, #14164 ) ) ;
#27773 = CARTESIAN_POINT ( 'NONE',  ( 0.2037720324489346591, -0.08956011622649388826, 0.004864851714980023868 ) ) ;
#27774 = DIRECTION ( 'NONE',  ( 0.000000000000000000, 0.000000000000000000, 1.000000000000000000 ) ) ;
#27775 = ORIENTED_EDGE ( 'NONE', *, *, #5744, .T. ) ;
#27776 = DIRECTION ( 'NONE',  ( 0.000000000000000000, -0.6220299971367093672, 0.7829934116339072325 ) ) ;
#27777 = DIRECTION ( 'NONE',  ( 0.000000000000000000, 0.000000000000000000, 1.000000000000000000 ) ) ;
#27778 = CARTESIAN_POINT ( 'NONE',  ( -1.054774247047244540, 0.07405724077823318263, 0.6151574802611965431 ) ) ;
#27779 = CARTESIAN_POINT ( 'NONE',  ( 0.7646288533564489232, 0.1113553986120547346, 1.353346456585388102 ) ) ;
#27780 = VERTEX_POINT ( 'NONE', #27497 ) ;
#27781 = CARTESIAN_POINT ( 'NONE',  ( -1.054774247047244096, 0.000000000000000000, 1.719980314906866203 ) ) ;
#27782 = DIRECTION ( 'NONE',  ( 0.000000000000000000, 0.000000000000000000, 1.000000000000000000 ) ) ;
#27783 = VECTOR ( 'NONE', #24180, 39.37007874015748854 ) ;
#27784 = CARTESIAN_POINT ( 'NONE',  ( -0.7185039370078739607, 1.928577636452523993E-17, 0.5019685039370078705 ) ) ;
#27785 = CARTESIAN_POINT ( 'NONE',  ( 0.07444174185955046430, -0.7613627072208409841, -0.1797182628040039087 ) ) ;
#27786 = CARTESIAN_POINT ( 'NONE',  ( 0.2471922904502827645, 0.09312491272442034729, 0.03902281811272177020 ) ) ;
#27787 = CARTESIAN_POINT ( 'NONE',  ( -0.9412147342319837628, 0.1574803149606300301, 1.227854330601135580 ) ) ;
#27789 = LINE ( 'NONE', #47314, #1780 ) ;
#27788 = CARTESIAN_POINT ( 'NONE',  ( -9.642888182262618425E-18, -0.4704724409448819422, -0.1574803149606299191 ) ) ;
#27790 = AXIS2_PLACEMENT_3D ( 'NONE', #1218, #16342, #15869 ) ;
#27791 = DIRECTION ( 'NONE',  ( -1.000000000000000000, 0.000000000000000000, 0.000000000000000000 ) ) ;
#27792 = ORIENTED_EDGE ( 'NONE', *, *, #24514, .T. ) ;
#27793 = EDGE_CURVE ( 'NONE', #7162, #46787, #1330, .T. ) ;
#27794 = CARTESIAN_POINT ( 'NONE',  ( 0.04756641494945763188, 0.3740157480314960647, 1.120507485783946766 ) ) ;
#27795 = CARTESIAN_POINT ( 'NONE',  ( 0.9873396505805591694, -0.1113553986120547346, 1.107283464566929165 ) ) ;
#27796 = DIRECTION ( 'NONE',  ( -1.000000000000000000, -6.679788269418529283E-17, 0.000000000000000000 ) ) ;
#27797 = DIRECTION ( 'NONE',  ( 0.000000000000000000, 0.7880107536067203489, -0.6156614753256604011 ) ) ;
#27799 = CARTESIAN_POINT ( 'NONE',  ( 1.033464566929134687, -0.06523048226347956391, 1.690452755797985152 ) ) ;
#27798 = DIRECTION ( 'NONE',  ( 0.000000000000000000, 0.000000000000000000, -1.000000000000000000 ) ) ;
#27800 = CARTESIAN_POINT ( 'NONE',  ( -0.7185039370078739607, 1.928577636452523993E-17, 0.9645669290263307882 ) ) ;
#27801 = CARTESIAN_POINT ( 'NONE',  ( -0.07405724077823318263, -0.5442913385289138706, 0.1787899950787401604 ) ) ;
#27802 = FACE_OUTER_BOUND ( 'NONE', #26675, .T. ) ;
#27803 = ORIENTED_EDGE ( 'NONE', *, *, #8155, .T. ) ;
#27804 = AXIS2_PLACEMENT_3D ( 'NONE', #9313, #34478, #23936 ) ;
#27805 = EDGE_CURVE ( 'NONE', #28092, #8495, #25404, .T. ) ;
#27806 = CARTESIAN_POINT ( 'NONE',  ( -0.8070866141732283561, -0.0009842519685049383633, -0.6590551181102368705 ) ) ;
#27807 = CARTESIAN_POINT ( 'NONE',  ( 0.8759842519685039353, -0.1787899950787401882, 0.7603346456155274380 ) ) ;
#27808 = ORIENTED_EDGE ( 'NONE', *, *, #21354, .T. ) ;
#27809 = CARTESIAN_POINT ( 'NONE',  ( 0.7646288533564489232, -0.1113553986120547346, 1.294291338582677309 ) ) ;
#27810 = CARTESIAN_POINT ( 'NONE',  ( 0.000000000000000000, 0.000000000000000000, -0.3001770169643759867 ) ) ;
#27811 = CARTESIAN_POINT ( 'NONE',  ( 3.284318927891251994E-17, -1.644192913332062966, 0.1787899950787401882 ) ) ;
#27812 = CARTESIAN_POINT ( 'NONE',  ( 0.1787899950787401604, -1.124999999946237228, -0.07405724077823318263 ) ) ;
#27813 = CARTESIAN_POINT ( 'NONE',  ( 0.1574803149606300301, -1.383366141732283561, -0.06523048226347956391 ) ) ;
#27814 = CARTESIAN_POINT ( 'NONE',  ( 0.7646288533564489232, 0.1113553986120547346, 1.235236220364913207 ) ) ;
#27815 = CARTESIAN_POINT ( 'NONE',  ( 0.1527640389977631963, 0.1337207259432474371, -0.04397945982240433066 ) ) ;
#27816 = ORIENTED_EDGE ( 'NONE', *, *, #8059, .T. ) ;
#27817 = CARTESIAN_POINT ( 'NONE',  ( -0.6971942568897637749, 2.189545951927499583E-17, 1.897145669237574772 ) ) ;
#27818 = ORIENTED_EDGE ( 'NONE', *, *, #43762, .F. ) ;
#27819 = CARTESIAN_POINT ( 'NONE',  ( 2.892866454678787531E-17, -1.385826771546015745, 0.1574803149606299191 ) ) ;
#27820 = CARTESIAN_POINT ( 'NONE',  ( -0.8759842519685039353, -0.1787899950787401882, 1.587106299158834721 ) ) ;
#27821 = CARTESIAN_POINT ( 'NONE',  ( -0.8759842519685039353, 0.1787899950787401882, 0.3124999999462365619 ) ) ;
#27822 = AXIS2_PLACEMENT_3D ( 'NONE', #747, #44597, #22812 ) ;
#27823 = B_SPLINE_CURVE_WITH_KNOTS ( 'NONE', 3,
 ( #1194, #33593, #44560, #11779, #22773, #26396, #951, #15610, #4358, #12307, #15669, #45687, #2555, #16954, #41852, #1855, #23449 ),
 .UNSPECIFIED., .F., .F.,
 ( 4, 2, 2, 2, 2, 1, 2, 2, 4 ),
 ( 0.000000000000000000, 0.1249999999999997502, 0.1874999999999995837, 0.2499999999999993894, 0.3749999999999990563, 0.4374999999999988343, 0.4687499999999987232, 0.4999999999999986122, 1.000000000000000000 ),
 .UNSPECIFIED. ) ;
#27824 = CARTESIAN_POINT ( 'NONE',  ( -7.957671378281915615E-17, 0.1574803149606340824, -0.3937007874015748254 ) ) ;
#27825 = CARTESIAN_POINT ( 'NONE',  ( -0.8759842519685039353, -0.1787899950787401882, 1.788877952702141672 ) ) ;
#27826 = CARTESIAN_POINT ( 'NONE',  ( 0.05612302249891599343, -0.07766248740294799668, -0.2530304272095452167 ) ) ;
#27827 = CARTESIAN_POINT ( 'NONE',  ( -0.8107537697050253289, 0.1574803149606300301, 1.754429133858266932 ) ) ;
#27828 = CARTESIAN_POINT ( 'NONE',  ( 0.2559053678971339174, 0.03992796258515165370, -0.03403288757427402195 ) ) ;
#27829 = CARTESIAN_POINT ( 'NONE',  ( 0.07405724077823318263, -0.2648877477567979088, -0.1787899950787401604 ) ) ;
#27830 = CARTESIAN_POINT ( 'NONE',  ( 1.054774247047244540, -0.07405724077823318263, 1.678149606245448622 ) ) ;
#27831 = CARTESIAN_POINT ( 'NONE',  ( -0.05991043469119292086, -0.09842519685039370636, -0.1769877046850827085 ) ) ;
#27832 = CARTESIAN_POINT ( 'NONE',  ( -0.1574803149606297803, 0.01427165354330708555, 0.06523048226347956391 ) ) ;
#27833 = CARTESIAN_POINT ( 'NONE',  ( -0.9412147342319837628, 0.1574803149606300301, 0.04675196839640998608 ) ) ;
#27834 = CIRCLE ( 'NONE', #45394, 0.09842519685039370636 ) ;
#27835 = ORIENTED_EDGE ( 'NONE', *, *, #6591, .F. ) ;
#27836 = CARTESIAN_POINT ( 'NONE',  ( -0.6971942568897648851, 0.07405724077823318263, 1.225393700733637514 ) ) ;
#27837 = ORIENTED_EDGE ( 'NONE', *, *, #28166, .T. ) ;
#27838 = CARTESIAN_POINT ( 'NONE',  ( 3.284318927891251994E-17, -1.289862204670645607, 0.1787899950787401882 ) ) ;
#27839 = ( BOUNDED_CURVE ( )  B_SPLINE_CURVE ( 2, ( #16911, #2975, #6582, #27957, #28668, #6341, #21433, #42525, #20955 ),
 .UNSPECIFIED., .F., .F. ) 
 B_SPLINE_CURVE_WITH_KNOTS ( ( 3, 2, 2, 2, 3 ),
 ( 0.3699999999999999956, 0.3724999999999999978, 0.3750000000000000000, 0.3775000000000000022, 0.3800000000000000044 ),
 .UNSPECIFIED. ) 
 CURVE ( )  GEOMETRIC_REPRESENTATION_ITEM ( )  RATIONAL_B_SPLINE_CURVE ( ( 1.000000000000000000, 0.9238795325112869605, 1.000000000000000000, 0.9238795325112869605, 1.000000000000000000, 0.9238795325112869605, 1.000000000000000000, 0.9238795325112869605, 1.000000000000000000 ) ) 
 REPRESENTATION_ITEM ( '' )  ) ;
#27840 = PLANE ( 'NONE',  #7975 ) ;
#27841 = CARTESIAN_POINT ( 'NONE',  ( -0.1797182628040039087, -0.5103784552523373819, 0.07444174185955065859 ) ) ;
#27842 = CARTESIAN_POINT ( 'NONE',  ( -1.033464566929134687, -0.06523048226347956391, 0.8636811022546767580 ) ) ;
#27843 = CARTESIAN_POINT ( 'NONE',  ( -1.033464566929133799, 0.000000000000000000, 0.6791338582677166613 ) ) ;
#27844 = CARTESIAN_POINT ( 'NONE',  ( 0.06523048226347956391, 0.06348425196850393526, 0.1574803149606297803 ) ) ;
#27845 = ADVANCED_FACE ( 'NONE', ( #41563 ), #34203, .T. ) ;
#27846 = CARTESIAN_POINT ( 'NONE',  ( 0.6971942568897637749, 2.189545951927499583E-17, 0.9079724408911180600 ) ) ;
#27847 = EDGE_CURVE ( 'NONE', #17869, #46334, #16685, .T. ) ;
#27848 = CARTESIAN_POINT ( 'NONE',  ( 0.6971942568897648851, -0.07405724077823297447, 1.978346456639149320 ) ) ;
#27849 = ADVANCED_FACE ( 'NONE', ( #41330 ), #8531, .T. ) ;
#27850 = EDGE_LOOP ( 'NONE', ( #37096, #15491, #35288, #5074 ) ) ;
#27851 = EDGE_CURVE ( 'NONE', #32629, #27408, #45175, .T. ) ;
#27852 = CARTESIAN_POINT ( 'NONE',  ( 0.9873396505805591694, -0.1113553986120547346, 0.3887795274515282729 ) ) ;
#27853 = CARTESIAN_POINT ( 'NONE',  ( 0.1264236179284866091, -0.6500984251430865779, -0.1264236179284866091 ) ) ;
#27854 = CARTESIAN_POINT ( 'NONE',  ( -0.1264236179284866091, -1.334153543253322916, 0.1264236179284866091 ) ) ;
#27855 = ( BOUNDED_CURVE ( )  B_SPLINE_CURVE ( 2, ( #34502, #24420, #39021, #9578, #38323, #16991, #38799, #1656, #34282 ),
 .UNSPECIFIED., .F., .F. ) 
 B_SPLINE_CURVE_WITH_KNOTS ( ( 3, 2, 2, 2, 3 ),
 ( 0.2700000000000000178, 0.2725000000000000200, 0.2750000000000000222, 0.2775000000000000244, 0.2800000000000000266 ),
 .UNSPECIFIED. ) 
 CURVE ( )  GEOMETRIC_REPRESENTATION_ITEM ( )  RATIONAL_B_SPLINE_CURVE ( ( 1.000000000000000000, 0.9238795325112869605, 1.000000000000000000, 0.9238795325112869605, 1.000000000000000000, 0.9238795325112869605, 1.000000000000000000, 0.9238795325112869605, 1.000000000000000000 ) ) 
 REPRESENTATION_ITEM ( '' )  ) ;
#27856 = CARTESIAN_POINT ( 'NONE',  ( -1.002407869896990045, 0.1264236179284866091, 1.838090551127338657 ) ) ;
#27857 = ORIENTED_EDGE ( 'NONE', *, *, #43772, .T. ) ;
#27858 = ORIENTED_EDGE ( 'NONE', *, *, #6862, .T. ) ;
#27859 = ( BOUNDED_CURVE ( )  B_SPLINE_CURVE ( 2, ( #30125, #43972, #33464, #4411, #43736, #7551, #3494, #4181, #36798 ),
 .UNSPECIFIED., .F., .T. ) 
 B_SPLINE_CURVE_WITH_KNOTS ( ( 3, 2, 2, 2, 3 ),
 ( 0.1799999999999999933, 0.1824999999999999956, 0.1849999999999999978, 0.1875000000000000000, 0.1900000000000000022 ),
 .UNSPECIFIED. ) 
 CURVE ( )  GEOMETRIC_REPRESENTATION_ITEM ( )  RATIONAL_B_SPLINE_CURVE ( ( 1.000000000000000000, 0.9238795325112869605, 1.000000000000000000, 0.9238795325112869605, 1.000000000000000000, 0.9238795325112869605, 1.000000000000000000, 0.9238795325112869605, 1.000000000000000000 ) ) 
 REPRESENTATION_ITEM ( '' )  ) ;
#27860 = CARTESIAN_POINT ( 'NONE',  ( -1.054774247047244540, 0.07405724077823318263, 1.525590551127340433 ) ) ;
#27861 = CARTESIAN_POINT ( 'NONE',  ( -0.9412147342319837628, -0.1574803149606297803, 0.9079724409448817202 ) ) ;
#27862 = CARTESIAN_POINT ( 'NONE',  ( -0.9500414927467378812, 0.1787899950787401604, 0.7037401574265510495 ) ) ;
#27863 = DIRECTION ( 'NONE',  ( 0.000000000000000000, 0.000000000000000000, -1.000000000000000000 ) ) ;
#27864 = CARTESIAN_POINT ( 'NONE',  ( 0.8019270111902716547, -0.1787899950787401604, 0.6840551180564720113 ) ) ;
#27865 = CARTESIAN_POINT ( 'NONE',  ( -0.7495606340400177148, -0.1264236179284866091, 0.5979330708123780092 ) ) ;
#27866 = CARTESIAN_POINT ( 'NONE',  ( 0.1796295154111492431, -0.08412760742822553151, 0.1817225848801442278 ) ) ;
#27867 = CARTESIAN_POINT ( 'NONE',  ( 0.1113553986120547346, -0.09153543307086613179, 0.1113553986120547346 ) ) ;
#27868 = ORIENTED_EDGE ( 'NONE', *, *, #26760, .T. ) ;
#27869 = CARTESIAN_POINT ( 'NONE',  ( -0.7185039370078739607, 1.928577636452523993E-17, 0.3444881889763780070 ) ) ;
#27870 = CARTESIAN_POINT ( 'NONE',  ( 0.6971942568897637749, 2.189545951927499583E-17, 1.385334645615527549 ) ) ;
#27871 = CARTESIAN_POINT ( 'NONE',  ( 0.2074532133938310763, -0.09851384671466711929, 0.02027945527772259671 ) ) ;
#27872 = APPLICATION_CONTEXT ( 'automotive_design' ) ;
#27873 = ORIENTED_EDGE ( 'NONE', *, *, #5406, .F. ) ;
#27874 = CIRCLE ( 'NONE', #34776, 0.1377952755905509363 ) ;
#27875 = FACE_OUTER_BOUND ( 'NONE', #23420, .T. ) ;
#27876 = CARTESIAN_POINT ( 'NONE',  ( -0.1264236179284866091, -1.596088535158372235, -0.1264236179284866091 ) ) ;
#27877 = ORIENTED_EDGE ( 'NONE', *, *, #42984, .T. ) ;
#27878 = CARTESIAN_POINT ( 'NONE',  ( -0.7185039370078692977, 0.06523048226347515077, 1.395177165246803908 ) ) ;
#27879 = CARTESIAN_POINT ( 'NONE',  ( 0.1264236179284866091, -0.6550196849856062542, 0.1264236179284866091 ) ) ;
#27880 = CARTESIAN_POINT ( 'NONE',  ( 0.7185039370078746268, -0.06523048226347956391, 0.3863188976377952000 ) ) ;
#27881 = VERTEX_POINT ( 'NONE', #9494 ) ;
#27882 = CARTESIAN_POINT ( 'NONE',  ( 0.6971942568897648851, 0.07405724077823318263, 1.377952755851748146 ) ) ;
#27883 = CARTESIAN_POINT ( 'NONE',  ( 0.1787899950787401604, -0.3031496062454492879, 0.07405724077823318263 ) ) ;
#27884 = CARTESIAN_POINT ( 'NONE',  ( -0.07405724077823318263, -0.7559055117572593963, -0.1787899950787401604 ) ) ;
#27885 = CARTESIAN_POINT ( 'NONE',  ( 0.1644020957507539848, -0.08115590401245571794, -0.1405661490837558925 ) ) ;
#27886 = DIRECTION ( 'NONE',  ( 0.000000000000000000, 0.000000000000000000, -1.000000000000000000 ) ) ;
#27887 = CARTESIAN_POINT ( 'NONE',  ( 0.7495606340400177148, -0.1264236179284866091, 1.700295275536787498 ) ) ;
#27888 = CARTESIAN_POINT ( 'NONE',  ( 0.7495606340400177148, -0.1264236179284866091, 0.2436023621509610382 ) ) ;
#27889 = AXIS2_PLACEMENT_3D ( 'NONE', #3803, #656, #39976 ) ;
#27890 = CARTESIAN_POINT ( 'NONE',  ( -0.1787899950787401604, 0.06483666169202111085, 0.07405724077823318263 ) ) ;
#27891 = CARTESIAN_POINT ( 'NONE',  ( 0.07405724077823318263, 0.04625984257344856188, 0.1787899950787401604 ) ) ;
#27892 = FACE_OUTER_BOUND ( 'NONE', #40243, .T. ) ;
#27893 = CARTESIAN_POINT ( 'NONE',  ( 0.9500414927467378812, -0.1787899950787401604, 0.4872047243556847929 ) ) ;
#27894 = EDGE_CURVE ( 'NONE', #27975, #5683, #29780, .T. ) ;
#27895 = CARTESIAN_POINT ( 'NONE',  ( -1.002407869896990045, 0.1264236179284866091, 0.8587598424659212970 ) ) ;
#27897 = CARTESIAN_POINT ( 'NONE',  ( 0.8759842519685039353, 0.1574803149606299191, 0.08858267705782735257 ) ) ;
#27896 = CARTESIAN_POINT ( 'NONE',  ( -0.06523048226347956391, -0.8223425196850393526, -0.1574803149606300301 ) ) ;
#27898 = CARTESIAN_POINT ( 'NONE',  ( -0.1270800023317771588, -1.620122549740525386, -0.1270800023317771588 ) ) ;
#27899 = CARTESIAN_POINT ( 'NONE',  ( -0.1574803149606300301, -0.5319881888688510196, -0.06523048226347956391 ) ) ;
#27900 = CARTESIAN_POINT ( 'NONE',  ( -0.1264236179284866091, -0.3892716534895436786, 0.1264236179284866091 ) ) ;
#27901 = CARTESIAN_POINT ( 'NONE',  ( 0.8019270111902717657, 0.1787899950787401604, 1.456692913332062744 ) ) ;
#27903 = CARTESIAN_POINT ( 'NONE',  ( 0.2559055118110236116, 0.06940437565852064505, -0.3096270012539200644 ) ) ;
#27902 = FACE_OUTER_BOUND ( 'NONE', #5566, .T. ) ;
#27904 = CARTESIAN_POINT ( 'NONE',  ( 1.054774247047244540, -0.07405724077823318263, 0.3346456692375752162 ) ) ;
#27905 = ORIENTED_EDGE ( 'NONE', *, *, #23313, .T. ) ;
#27906 = EDGE_CURVE ( 'NONE', #8711, #13468, #9727, .T. ) ;
#27907 = CARTESIAN_POINT ( 'NONE',  ( -0.1377952755905511306, 1.687505431895958263E-17, -0.3149606299212598381 ) ) ;
#27908 = CARTESIAN_POINT ( 'NONE',  ( 0.1631814734428348734, -0.2012842543237225446, -0.3131151337379049493 ) ) ;
#27909 = CARTESIAN_POINT ( 'NONE',  ( 0.1264236179284866091, -0.06938976372576398377, 0.1264236179284866091 ) ) ;
#27910 = CARTESIAN_POINT ( 'NONE',  ( 0.9500414927467378812, 0.1787899950787401604, 0.4625984251430869665 ) ) ;
#27911 = CARTESIAN_POINT ( 'NONE',  ( 0.07405724077823318263, -0.8789370078202529690, -0.1787899950787401604 ) ) ;
#27912 = FACE_OUTER_BOUND ( 'NONE', #33281, .T. ) ;
#27913 = CARTESIAN_POINT ( 'NONE',  ( -1.002407869896990045, -0.1264236179284866091, 1.395177165300567124 ) ) ;
#27914 = VERTEX_POINT ( 'NONE', #27734 ) ;
#27915 = DIRECTION ( 'NONE',  ( 0.000000000000000000, 0.000000000000000000, -1.000000000000000000 ) ) ;
#27916 = CARTESIAN_POINT ( 'NONE',  ( 1.054774247047244096, 0.000000000000000000, 1.050688976324189117 ) ) ;
#27917 = EDGE_LOOP ( 'NONE', ( #35350, #12064, #34170, #41133, #17352, #44804 ) ) ;
#27918 = VECTOR ( 'NONE', #21110, 39.37007874015748854 ) ;
#27919 = CARTESIAN_POINT ( 'NONE',  ( -0.1113553986120547346, -1.085629921152315047, -0.1113553986120547346 ) ) ;
#27920 = CARTESIAN_POINT ( 'NONE',  ( -0.7185039370078746268, -0.06523048226347956391, 0.4945866140657015353 ) ) ;
#27921 = DIRECTION ( 'NONE',  ( -1.000000000000000000, 0.000000000000000000, 0.000000000000000000 ) ) ;
#27922 = DIRECTION ( 'NONE',  ( 0.000000000000000000, 0.000000000000000000, 1.000000000000000000 ) ) ;
#27923 = CARTESIAN_POINT ( 'NONE',  ( 0.8759842519685039353, 0.1787899950787401882, 0.1550196849856066983 ) ) ;
#27924 = CARTESIAN_POINT ( 'NONE',  ( 0.9873396505805591694, -0.1113553986120547346, 1.451771653435779408 ) ) ;
#27925 = ORIENTED_EDGE ( 'NONE', *, *, #42442, .T. ) ;
#27926 = ORIENTED_EDGE ( 'NONE', *, *, #7094, .F. ) ;
#27927 = CARTESIAN_POINT ( 'NONE',  ( 0.07405724077823318263, 0.08562992131360593062, 0.1787899950787401604 ) ) ;
#27928 = AXIS2_PLACEMENT_3D ( 'NONE', #12349, #26968, #12593 ) ;
#27929 = CARTESIAN_POINT ( 'NONE',  ( -1.054774247047244540, 0.07405724077823318263, 1.678149606245448622 ) ) ;
#27930 = ORIENTED_EDGE ( 'NONE', *, *, #27793, .T. ) ;
#27931 = ORIENTED_EDGE ( 'NONE', *, *, #20661, .F. ) ;
#27932 = DIRECTION ( 'NONE',  ( -0.000000000000000000, 0.6156614753256597350, 0.7880107536067206819 ) ) ;
#27933 = LINE ( 'NONE', #46573, #6053 ) ;
#27934 = CARTESIAN_POINT ( 'NONE',  ( -0.1787899950787401882, -1.158096409174120156, 0.000000000000000000 ) ) ;
#27935 = ORIENTED_EDGE ( 'NONE', *, *, #28594, .F. ) ;
#27936 = CARTESIAN_POINT ( 'NONE',  ( -0.1264236179284866091, -0.07431102356828367395, 0.1264236179284866091 ) ) ;
#27937 = ORIENTED_EDGE ( 'NONE', *, *, #45312, .T. ) ;
#27938 = ORIENTED_EDGE ( 'NONE', *, *, #23511, .T. ) ;
#27939 = CARTESIAN_POINT ( 'NONE',  ( -0.2559055118110235005, -0.1351184156184602747, -0.2957496633320546020 ) ) ;
#27940 = CARTESIAN_POINT ( 'NONE',  ( -0.9873396505805591694, -0.1113553986120547346, 1.461614173228346525 ) ) ;
#27941 = CARTESIAN_POINT ( 'NONE',  ( 0.7646288533564489232, 0.1113553986120547346, 1.796259842519684957 ) ) ;
#27942 = AXIS2_PLACEMENT_3D ( 'NONE', #26617, #465, #41172 ) ;
#27943 = AXIS2_PLACEMENT_3D ( 'NONE', #15502, #41320, #40620 ) ;
#27944 = VECTOR ( 'NONE', #12565, 39.37007874015748143 ) ;
#27945 = ORIENTED_EDGE ( 'NONE', *, *, #28485, .F. ) ;
#27946 = ADVANCED_FACE ( 'NONE', ( #24569 ), #42988, .T. ) ;
#27947 = CARTESIAN_POINT ( 'NONE',  ( -0.6971942568897637749, 2.189545951927499583E-17, 0.3223425196312759144 ) ) ;
#27948 = CARTESIAN_POINT ( 'NONE',  ( -1.033464566929133799, 0.000000000000000000, 0.9940944881889764995 ) ) ;
#27949 = CARTESIAN_POINT ( 'NONE',  ( -0.1797182628040039087, -1.219039872575171213, 0.07444174185955065859 ) ) ;
#27950 = CARTESIAN_POINT ( 'NONE',  ( -0.09357655176633561389, 0.2414677849102764839, -0.03395687952545718702 ) ) ;
#27951 = CARTESIAN_POINT ( 'NONE',  ( 0.7495606340400177148, 0.1264236179284866091, 1.104822834591905556 ) ) ;
#27952 = CARTESIAN_POINT ( 'NONE',  ( 0.8019270111902716547, 0.1787899950787401604, 1.609251968450173598 ) ) ;
#27953 = CYLINDRICAL_SURFACE ( 'NONE', #2390, 0.1574803149606299191 ) ;
#27954 = ADVANCED_FACE ( 'NONE', ( #17847 ), #28181, .T. ) ;
#27956 = DIRECTION ( 'NONE',  ( 1.144917494144692682E-16, 2.347476851301873061E-33, 1.000000000000000000 ) ) ;
#27955 = CARTESIAN_POINT ( 'NONE',  ( 0.7625151755711149226, 0.1152071623345953810, 1.980784476798966853 ) ) ;
#27957 = CARTESIAN_POINT ( 'NONE',  ( 0.8107537697050254399, -0.1574803149606297803, 0.7750984250893222516 ) ) ;
#27958 = ( BOUNDED_CURVE ( )  B_SPLINE_CURVE ( 2, ( #4161, #44403, #19499, #34143, #1274, #11619, #15926, #30556, #13274 ),
 .UNSPECIFIED., .F., .T. ) 
 B_SPLINE_CURVE_WITH_KNOTS ( ( 3, 2, 2, 2, 3 ),
 ( 0.7099999999999999645, 0.7125000000000000222, 0.7149999999999999689, 0.7175000000000000266, 0.7199999999999999734 ),
 .UNSPECIFIED. ) 
 CURVE ( )  GEOMETRIC_REPRESENTATION_ITEM ( )  RATIONAL_B_SPLINE_CURVE ( ( 1.000000000000000000, 0.9238795325112939549, 1.000000000000000000, 0.9238795325112869605, 1.000000000000000000, 0.9238795325112869605, 1.000000000000000000, 0.9238795325112869605, 1.000000000000000000 ) ) 
 REPRESENTATION_ITEM ( '' )  ) ;
#27959 = CARTESIAN_POINT ( 'NONE',  ( -0.8759842519685039353, -0.1574803149606299191, 0.6988188975302678241 ) ) ;
#27960 = CARTESIAN_POINT ( 'NONE',  ( 1.054774247047244540, 0.07405724077823318263, 1.166338582623402731 ) ) ;
#27961 = CARTESIAN_POINT ( 'NONE',  ( 0.6971942568897648851, -0.07405724077823297447, 1.938976377898990799 ) ) ;
#27962 = CARTESIAN_POINT ( 'NONE',  ( 0.7185039370078746268, -0.06523048226347956391, 0.3764763778452286935 ) ) ;
#27963 = VERTEX_POINT ( 'NONE', #35828 ) ;
#27964 = CARTESIAN_POINT ( 'NONE',  ( 1.002407869896990045, -0.1264236179284866091, 1.990649606245448844 ) ) ;
#27965 = CARTESIAN_POINT ( 'NONE',  ( 1.033949376711145174, 0.01198047669008794891, 0.03936939612278594902 ) ) ;
#27966 = CARTESIAN_POINT ( 'NONE',  ( -1.033464566929134687, 0.06523048226347956391, 0.1993110235145201248 ) ) ;
#27967 = CARTESIAN_POINT ( 'NONE',  ( 0.1728472449644665732, -0.09617745053770661301, -0.07999999089250650619 ) ) ;
#27968 = CARTESIAN_POINT ( 'NONE',  ( 1.002407869896990045, 0.1264236179284866091, 1.365649606245448844 ) ) ;
#27969 = ORIENTED_EDGE ( 'NONE', *, *, #9854, .T. ) ;
#27971 = CARTESIAN_POINT ( 'NONE',  ( -0.7646288533564489232, -0.1113553986120547346, 0.2214566928058590567 ) ) ;
#27970 = CARTESIAN_POINT ( 'NONE',  ( 0.09431337879938411772, -0.09445537554013619386, 0.2309807168374905517 ) ) ;
#27972 = CARTESIAN_POINT ( 'NONE',  ( -0.07405724077823318263, 0.07086614178604697112, -0.1787899950787401604 ) ) ;
#27973 = CARTESIAN_POINT ( 'NONE',  ( 0.2372856289813619346, 0.04209688371796207335, 0.1484361490989228038 ) ) ;
#27974 = LINE ( 'NONE', #34686, #60 ) ;
#27975 = VERTEX_POINT ( 'NONE', #42299 ) ;
#27976 = EDGE_LOOP ( 'NONE', ( #9375, #44605, #43116, #45625 ) ) ;
#27977 = CARTESIAN_POINT ( 'NONE',  ( -0.7495606340400177148, -0.1264236179284866091, 1.345964566875370139 ) ) ;
#27978 = CARTESIAN_POINT ( 'NONE',  ( -0.1787899950787401604, -1.622047244040725866, -0.07405724077823318263 ) ) ;
#27979 = CARTESIAN_POINT ( 'NONE',  ( -0.8019270111902717657, -0.1787899950787401604, 1.038385826717890259 ) ) ;
#27980 = CIRCLE ( 'NONE', #5754, 0.1377952755905509363 ) ;
#27981 = TOROIDAL_SURFACE ( 'NONE', #11896, 0.7972440944881888925, 0.009842519685039369942 ) ;
#27982 = CARTESIAN_POINT ( 'NONE',  ( -1.002407869896990045, -0.1264236179284866091, 1.946358267662771757 ) ) ;
#27983 = ORIENTED_EDGE ( 'NONE', *, *, #38037, .F. ) ;
#27984 = CARTESIAN_POINT ( 'NONE',  ( -0.6971942568897626646, 0.07405724077823318263, 0.7135826771115916234 ) ) ;
#27985 = EDGE_CURVE ( 'NONE', #27388, #44020, #46365, .T. ) ;
#27986 = CARTESIAN_POINT ( 'NONE',  ( 0.01230737760510395781, 0.07955613945526338049, -0.1377952755905511861 ) ) ;
#27987 = CARTESIAN_POINT ( 'NONE',  ( -0.1264236179284866091, -0.6905767241347500196, -0.1264236179284866091 ) ) ;
#27988 = ORIENTED_EDGE ( 'NONE', *, *, #9307, .T. ) ;
#27989 = CARTESIAN_POINT ( 'NONE',  ( 0.1783903336175657606, -0.08956053790448267882, -0.08775565328239233465 ) ) ;
#27990 = CARTESIAN_POINT ( 'NONE',  ( -1.033464566929134687, -0.06523048226347956391, 0.6668307085538908163 ) ) ;
#27991 = ORIENTED_EDGE ( 'NONE', *, *, #38229, .F. ) ;
#27992 = LINE ( 'NONE', #38975, #40147 ) ;
#27993 = CARTESIAN_POINT ( 'NONE',  ( -0.9873396505805591694, -0.1113553986120547346, 1.766732283357039135 ) ) ;
#27994 = CARTESIAN_POINT ( 'NONE',  ( -0.7495606340400177148, -0.1264236179284866091, 0.6766732282926929409 ) ) ;
#27995 = CARTESIAN_POINT ( 'NONE',  ( 0.1574803149606300301, 0.07332677165354323234, -0.06523048226347956391 ) ) ;
#27996 = ORIENTED_EDGE ( 'NONE', *, *, #7622, .T. ) ;
#27997 = AXIS2_PLACEMENT_3D ( 'NONE', #16234, #9022, #34921 ) ;
#27998 = LINE ( 'NONE', #38982, #28008 ) ;
#27999 = EDGE_CURVE ( 'NONE', #10600, #39650, #7629, .T. ) ;
#28000 = CARTESIAN_POINT ( 'NONE',  ( -0.8759842519685039353, 0.1574803149606299191, 0.1279527557979848462 ) ) ;
#28001 = CARTESIAN_POINT ( 'NONE',  ( -0.1574803149606299191, -0.9875035750853327077, -1.463737590216208861 ) ) ;
#28002 = EDGE_LOOP ( 'NONE', ( #31665, #25805, #9881 ) ) ;
#28003 = CARTESIAN_POINT ( 'NONE',  ( -0.1797182628040039087, -0.6678587702129673564, 0.07444174185955065859 ) ) ;
#28004 = CARTESIAN_POINT ( 'NONE',  ( -0.7646288533564489232, 0.1113553986120547346, 0.9694881889763780070 ) ) ;
#28005 = CARTESIAN_POINT ( 'NONE',  ( -0.7646288533564489232, -0.1113553986120547346, 1.166338582569637961 ) ) ;
#28007 = CARTESIAN_POINT ( 'NONE',  ( -0.1713481153329562412, -0.09842519685039370636, -0.04016550290184540267 ) ) ;
#28006 = CARTESIAN_POINT ( 'NONE',  ( -9.642888182262618425E-18, -0.5098425196850393526, -0.1574803149606299191 ) ) ;
#28008 = VECTOR ( 'NONE', #38051, 39.37007874015748854 ) ;
#28009 = AXIS2_PLACEMENT_3D ( 'NONE', #41072, #18818, #26029 ) ;
#28010 = CYLINDRICAL_SURFACE ( 'NONE', #3171, 0.09842519685039370636 ) ;
#28011 = EDGE_LOOP ( 'NONE', ( #30218, #18794, #13975, #20011 ) ) ;
#28012 = CARTESIAN_POINT ( 'NONE',  ( 0.7185039370078714072, 0.06523048226347728795, 1.592027558947592958 ) ) ;
#28013 = EDGE_CURVE ( 'NONE', #4638, #6112, #6814, .T. ) ;
#28014 = CARTESIAN_POINT ( 'NONE',  ( 1.033464566929134687, 0.06523048226347956391, 1.193405511811024278 ) ) ;
#28016 = CARTESIAN_POINT ( 'NONE',  ( -0.7185039370078739607, 1.928577636452523993E-17, 0.8956692913385826404 ) ) ;
#28015 = DIRECTION ( 'NONE',  ( -1.000000000000000000, -0.000000000000000000, 0.000000000000000000 ) ) ;
#28017 = DIRECTION ( 'NONE',  ( 0.000000000000000000, 0.000000000000000000, 1.000000000000000000 ) ) ;
#28019 = DIRECTION ( 'NONE',  ( -1.000000000000000000, 0.000000000000000000, 0.000000000000000000 ) ) ;
#28018 = LINE ( 'NONE', #42580, #22257 ) ;
#28020 = CARTESIAN_POINT ( 'NONE',  ( -0.1625082278952665604, -0.08956041897765029680, -0.06009421481027538842 ) ) ;
#28021 = CARTESIAN_POINT ( 'NONE',  ( 0.1787899950787401882, -0.5713582676627716461, -2.189545951927503898E-17 ) ) ;
#28022 = CARTESIAN_POINT ( 'NONE',  ( 1.033464566929133799, 1.928577636452524610E-17, 4.498031496062992574 ) ) ;
#28023 = ORIENTED_EDGE ( 'NONE', *, *, #15233, .T. ) ;
#28024 = CARTESIAN_POINT ( 'NONE',  ( 0.1562117447733968045, 0.1299212598425196763, 0.09007225877465360742 ) ) ;
#28025 = CARTESIAN_POINT ( 'NONE',  ( 0.000000000000000000, 0.1193342091828950846, -0.06889763779527559306 ) ) ;
#28026 = CARTESIAN_POINT ( 'NONE',  ( 1.054774247047244096, 0.000000000000000000, 0.8882874015210394658 ) ) ;
#28027 = ORIENTED_EDGE ( 'NONE', *, *, #28209, .T. ) ;
#28028 = CARTESIAN_POINT ( 'NONE',  ( -0.03894127257522794067, 0.06746187776206562237, -0.2629503166622473853 ) ) ;
#28029 = CARTESIAN_POINT ( 'NONE',  ( -1.033464566929134687, 0.06523048226347956391, 0.5241141732283461918 ) ) ;
#28030 = CARTESIAN_POINT ( 'NONE',  ( 3.301370929368692659E-17, 0.04818453687364732119, 0.1797182628040039365 ) ) ;
#28031 = CARTESIAN_POINT ( 'NONE',  ( -0.1787899950787401604, -0.9921259841982054128, -0.07405724077823318263 ) ) ;
#28032 = CARTESIAN_POINT ( 'NONE',  ( 0.1574803149606300301, -1.309547244094489082, 0.06523048226347956391 ) ) ;
#28033 = CARTESIAN_POINT ( 'NONE',  ( 0.8107537697050253289, -0.1574803149606297803, 1.286909448711370585 ) ) ;
#28034 = CARTESIAN_POINT ( 'NONE',  ( 0.1637325577037128943, 0.1604625459914952312, 0.002338731188024917394 ) ) ;
#28035 = ORIENTED_EDGE ( 'NONE', *, *, #14309, .F. ) ;
#28036 = CARTESIAN_POINT ( 'NONE',  ( -1.002407869896990045, 0.1264236179284866091, 1.843011810969858333 ) ) ;
#28037 = CARTESIAN_POINT ( 'NONE',  ( 1.002407869896990045, 0.1264236179284866091, 1.921751968450173376 ) ) ;
#28038 = VERTEX_POINT ( 'NONE', #14020 ) ;
#28039 = CARTESIAN_POINT ( 'NONE',  ( 0.1113553986120547346, -1.420275590443653480, 0.1113553986120547346 ) ) ;
#28040 = CARTESIAN_POINT ( 'NONE',  ( -1.033464566929134687, 0.06523048226347956391, 0.4749015746956221085 ) ) ;
#28041 = CARTESIAN_POINT ( 'NONE',  ( -0.9500414927467378812, -0.1787899950787401604, 1.471456692859622217 ) ) ;
#28042 = CONICAL_SURFACE ( 'NONE', #27997, 0.09842519685039370636, 0.9599310885968824758 ) ;
#28043 = CARTESIAN_POINT ( 'NONE',  ( 0.1063536270747394152, 0.2340938383371280740, -0.3144333452974443222 ) ) ;
#28044 = CARTESIAN_POINT ( 'NONE',  ( -0.6971942568897637749, 2.189545951927499583E-17, 1.026082677111590513 ) ) ;
#28045 = CARTESIAN_POINT ( 'NONE',  ( -0.7495606340400177148, -0.1264236179284866091, 0.2091535432533232486 ) ) ;
#28046 = DIRECTION ( 'NONE',  ( -1.000000000000000000, 0.000000000000000000, 0.000000000000000000 ) ) ;
#28047 = CARTESIAN_POINT ( 'NONE',  ( -0.9500414927467378812, -0.1787899950787401604, 1.870078740103715331 ) ) ;
#28048 = CARTESIAN_POINT ( 'NONE',  ( 0.2944196465027555387, 0.09842519685039370636, 0.000000000000000000 ) ) ;
#28049 = CARTESIAN_POINT ( 'NONE',  ( -0.8107537697050253289, -0.1574803149606297803, 1.887303149606301078 ) ) ;
#28050 = CARTESIAN_POINT ( 'NONE',  ( 0.2559052630942058038, 0.07638014557814261363, -0.05128389705078049282 ) ) ;
#28051 = CARTESIAN_POINT ( 'NONE',  ( -0.07405724077823318263, -0.2993365666544354209, -0.1787899950787401604 ) ) ;
#28052 = CARTESIAN_POINT ( 'NONE',  ( 0.08748153575225099676, -0.09842519685039370636, 0.2018362251056389500 ) ) ;
#28053 = CARTESIAN_POINT ( 'NONE',  ( 0.1377952755905511861, 0.1564960629921262614, -0.7066929133858274037 ) ) ;
#28054 = CYLINDRICAL_SURFACE ( 'NONE', #18063, 0.009842519685039376881 ) ;
#28055 = AXIS2_PLACEMENT_3D ( 'NONE', #44116, #36249, #36481 ) ;
#28056 = EDGE_CURVE ( 'NONE', #12116, #27624, #2282, .T. ) ;
#28057 = ORIENTED_EDGE ( 'NONE', *, *, #32279, .F. ) ;
#28058 = EDGE_CURVE ( 'NONE', #31988, #28682, #27839, .T. ) ;
#28059 = ORIENTED_EDGE ( 'NONE', *, *, #43925, .F. ) ;
#28060 = CARTESIAN_POINT ( 'NONE',  ( -0.1787899950787401604, -1.065944881836000224, 0.07405724077823318263 ) ) ;
#28061 = CARTESIAN_POINT ( 'NONE',  ( 0.1787899950787401604, -1.159448818843874074, -0.07405724077823318263 ) ) ;
#28062 = CARTESIAN_POINT ( 'NONE',  ( -0.8070866141732283561, 0.000000000000000000, -0.7574803149606299524 ) ) ;
#28063 = CARTESIAN_POINT ( 'NONE',  ( 0.07444174185955046430, -0.4464020772995807018, -0.1797182628040039087 ) ) ;
#28064 = CARTESIAN_POINT ( 'NONE',  ( -0.9873396505805591694, 0.1113553986120547346, 0.8316929132782993062 ) ) ;
#28065 = CARTESIAN_POINT ( 'NONE',  ( -1.033464566929134687, 0.06523048226347956391, 0.7209645669291341319 ) ) ;
#28066 = CARTESIAN_POINT ( 'NONE',  ( 0.1574803149606299191, -0.007874015748031495954, -1.928577636452523993E-17 ) ) ;
#28067 = EDGE_CURVE ( 'NONE', #27600, #15794, #45031, .T. ) ;
#28068 = CARTESIAN_POINT ( 'NONE',  ( 0.8019270111902717657, 0.1787899950787401604, 0.9793307086076531442 ) ) ;
#28069 = ADVANCED_FACE ( 'NONE', ( #35370 ), #46596, .T. ) ;
#28071 = CARTESIAN_POINT ( 'NONE',  ( 0.1588779435336272472, -0.1435649425735359141, -0.03225083113269787416 ) ) ;
#28070 = CARTESIAN_POINT ( 'NONE',  ( 0.08812199945789689348, 0.2446169721538616060, -0.03618545512906795603 ) ) ;
#28072 = CARTESIAN_POINT ( 'NONE',  ( 0.9412147342319837628, 0.1574803149606300301, 0.1648622046168823629 ) ) ;
#28073 = CARTESIAN_POINT ( 'NONE',  ( 0.8107537697050254399, -0.1574803149606297803, 1.838090551073574774 ) ) ;
#28074 = CARTESIAN_POINT ( 'NONE',  ( -0.8759842519685039353, 0.000000000000000000, 0.000000000000000000 ) ) ;
#28075 = CARTESIAN_POINT ( 'NONE',  ( 0.1264236179284866091, -0.6599409448281259305, 0.1264236179284866091 ) ) ;
#28076 = CARTESIAN_POINT ( 'NONE',  ( 0.07405724077823318263, -1.326771653489542402, 0.1787899950787401604 ) ) ;
#28077 = CARTESIAN_POINT ( 'NONE',  ( 0.6971942568897626646, -0.07405724077823297447, 0.3641732282926931630 ) ) ;
#28078 = CARTESIAN_POINT ( 'NONE',  ( -0.8019270111902717657, 0.1787899950787401604, 1.924212598371433325 ) ) ;
#28079 = VERTEX_POINT ( 'NONE', #13776 ) ;
#28080 = VERTEX_POINT ( 'NONE', #28420 ) ;
#28081 = CARTESIAN_POINT ( 'NONE',  ( -0.9500414927467378812, -0.1787899950787401604, 1.397637795221827295 ) ) ;
#28082 = CARTESIAN_POINT ( 'NONE',  ( 1.054774247047244540, 0.07405724077823318263, 1.564960629867495845 ) ) ;
#28083 = DIRECTION ( 'NONE',  ( 0.000000000000000000, -1.000000000000000000, 0.000000000000000000 ) ) ;
#28084 = CARTESIAN_POINT ( 'NONE',  ( -0.8019270111902717657, 0.1787899950787401604, 0.6299212597887560161 ) ) ;
#28085 = CARTESIAN_POINT ( 'NONE',  ( 0.8019270111902717657, -0.1787899950787401604, 0.1722440944344256208 ) ) ;
#28086 = CARTESIAN_POINT ( 'NONE',  ( 0.1227919659947372816, -0.09843992453377478635, -0.1299906436365789453 ) ) ;
#28087 = FILL_AREA_STYLE_COLOUR ( '', #11719 ) ;
#28088 = CARTESIAN_POINT ( 'NONE',  ( 1.002407869896990045, -0.1264236179284866091, 0.6126968503399370380 ) ) ;
#28089 = CARTESIAN_POINT ( 'NONE',  ( -1.002407869896990045, -0.1264236179284866091, 0.5684055117572598403 ) ) ;
#28090 = CARTESIAN_POINT ( 'NONE',  ( 0.2395294000716133853, 0.000000000000000000, 0.7086614173228351632 ) ) ;
#28091 = CARTESIAN_POINT ( 'NONE',  ( 0.8070866141732283561, 0.000000000000000000, 0.8568897637795275246 ) ) ;
#28092 = VERTEX_POINT ( 'NONE', #39399 ) ;
#28093 = DIRECTION ( 'NONE',  ( 0.000000000000000000, 1.000000000000000000, 0.000000000000000000 ) ) ;
#28094 = CARTESIAN_POINT ( 'NONE',  ( -1.033464566929134687, 0.06523048226347956391, 0.5241141732283461918 ) ) ;
#28095 = CARTESIAN_POINT ( 'NONE',  ( 0.8019270111902716547, -0.1787899950787401604, 1.313976377898992132 ) ) ;
#28096 = CARTESIAN_POINT ( 'NONE',  ( -0.2009589076016815024, -0.09851385032380531592, 0.1224783046148972404 ) ) ;
#28097 = ORIENTED_EDGE ( 'NONE', *, *, #8708, .F. ) ;
#28098 = ADVANCED_FACE ( 'NONE', ( #31549 ), #21195, .T. ) ;
#28099 = DIRECTION ( 'NONE',  ( 1.000000000000000000, 0.000000000000000000, -1.822029033848725275E-16 ) ) ;
#28100 = EDGE_CURVE ( 'NONE', #16297, #9744, #14734, .T. ) ;
#28101 = CARTESIAN_POINT ( 'NONE',  ( -0.07405724077823318263, -1.598549165079632406, -0.1787899950787401604 ) ) ;
#28102 = VERTEX_POINT ( 'NONE', #11147 ) ;
#28103 = CARTESIAN_POINT ( 'NONE',  ( 0.07405724077823318263, -0.5246062991588343882, -0.1787899950787401604 ) ) ;
#28104 = ADVANCED_FACE ( 'NONE', ( #18552 ), #32963, .T. ) ;
#28105 = CARTESIAN_POINT ( 'NONE',  ( 0.8759842519685039353, -0.1574803149606299191, 1.614173228346456712 ) ) ;
#28106 = VERTEX_POINT ( 'NONE', #40572 ) ;
#28107 = CARTESIAN_POINT ( 'NONE',  ( 0.6971942568897637749, 2.189545951927499583E-17, 1.419783464513165505 ) ) ;
#28108 = CARTESIAN_POINT ( 'NONE',  ( 0.4755220087074803481, 4.766607801171850497E-17, 0.000000000000000000 ) ) ;
#28109 = CARTESIAN_POINT ( 'NONE',  ( 0.07405724077823318263, -0.3080708660879689087, 0.1787899950787401604 ) ) ;
#28110 = CARTESIAN_POINT ( 'NONE',  ( 0.1264236179284866091, -0.7632874015210393548, -0.1264236179284866091 ) ) ;
#28111 = CARTESIAN_POINT ( 'NONE',  ( 0.8759842519685039353, 0.000000000000000000, 4.498031496062992574 ) ) ;
#28112 = CARTESIAN_POINT ( 'NONE',  ( 0.1787899950787401604, 0.04023036247942270160, 0.07405724077823318263 ) ) ;
#28113 = CARTESIAN_POINT ( 'NONE',  ( 0.07405724077823318263, 0.06102362210100767403, -0.1787899950787401604 ) ) ;
#28114 = CONTEXT_DEPENDENT_SHAPE_REPRESENTATION ( #22941, #32978 ) ;
#28115 = CARTESIAN_POINT ( 'NONE',  ( 0.2559055118110236671, -0.04912888505753350288, -0.3129193602642642014 ) ) ;
#28116 = CARTESIAN_POINT ( 'NONE',  ( 0.9500414927467378812, 0.1787899950787401604, 0.4625984251430869665 ) ) ;
#28117 = CIRCLE ( 'NONE', #7437, 0.1574803149606299191 ) ;
#28118 = ( BOUNDED_CURVE ( )  B_SPLINE_CURVE ( 2, ( #24853, #9774, #35873, #39216, #28000, #32306, #42788, #13148, #31357 ),
 .UNSPECIFIED., .F., .T. ) 
 B_SPLINE_CURVE_WITH_KNOTS ( ( 3, 2, 2, 2, 3 ),
 ( 0.04000000000000000083, 0.04250000000000000305, 0.04499999999999999833, 0.04750000000000000056, 0.05000000000000000278 ),
 .UNSPECIFIED. ) 
 CURVE ( )  GEOMETRIC_REPRESENTATION_ITEM ( )  RATIONAL_B_SPLINE_CURVE ( ( 1.000000000000000000, 0.9238795325112869605, 1.000000000000000000, 0.9238795325112869605, 1.000000000000000000, 0.9238795325112869605, 1.000000000000000000, 0.9238795325112869605, 1.000000000000000000 ) ) 
 REPRESENTATION_ITEM ( '' )  ) ;
#28119 = CARTESIAN_POINT ( 'NONE',  ( -0.9500414927467377701, -0.1787899950787401604, 0.8070866141194653620 ) ) ;
#28121 = DIRECTION ( 'NONE',  ( -1.000000000000000000, 0.000000000000000000, 0.000000000000000000 ) ) ;
#28120 = CARTESIAN_POINT ( 'NONE',  ( -0.06523048226347956391, -0.9256889763779536651, 0.1574803149606297803 ) ) ;
#28123 = CARTESIAN_POINT ( 'NONE',  ( -0.7885580836502673607, -0.1477104740678956973, 1.986504824066490649 ) ) ;
#28122 = CARTESIAN_POINT ( 'NONE',  ( 0.1797182628040039087, -1.755457195409817928, 0.07444174185955046430 ) ) ;
#28124 = CARTESIAN_POINT ( 'NONE',  ( 0.8019270111902717657, -0.1787899950787401604, 1.510826771599780294 ) ) ;
#28126 = CARTESIAN_POINT ( 'NONE',  ( 0.1629747151065570054, 0.1601846959074193222, 3.793325934747440125E-08 ) ) ;
#28125 = CARTESIAN_POINT ( 'NONE',  ( 0.1711856790334206346, 0.08819060268784824352, -0.1865989729947874209 ) ) ;
#28127 = CARTESIAN_POINT ( 'NONE',  ( 0.6971942568897648851, -0.07405724077823297447, 0.3592519684501735422 ) ) ;
#28128 = ORIENTED_EDGE ( 'NONE', *, *, #23070, .F. ) ;
#28129 = CARTESIAN_POINT ( 'NONE',  ( -0.8070866141732283561, -0.0009842519685049383633, -0.7574803149606299524 ) ) ;
#28130 = DIRECTION ( 'NONE',  ( 0.000000000000000000, -1.000000000000000000, 0.000000000000000000 ) ) ;
#28131 = LINE ( 'NONE', #1997, #28280 ) ;
#28133 = CARTESIAN_POINT ( 'NONE',  ( 0.1787899950787401882, -0.1432086613635592531, -2.189545951927503898E-17 ) ) ;
#28132 = CARTESIAN_POINT ( 'NONE',  ( 0.1574803149606300301, -0.9060039369003467513, 0.06523048226347956391 ) ) ;
#28134 = CARTESIAN_POINT ( 'NONE',  ( 1.002407869896990045, 0.1264236179284866091, 0.5782480314422993040 ) ) ;
#28135 = CARTESIAN_POINT ( 'NONE',  ( -1.094772975963752103E-17, -0.9552165353793071745, -0.1787899950787401882 ) ) ;
#28136 = DIRECTION ( 'NONE',  ( 0.000000000000000000, 1.000000000000000000, 0.000000000000000000 ) ) ;
#28137 = CARTESIAN_POINT ( 'NONE',  ( 0.1377952755905511861, 0.1564960629921262614, -0.8070866141732283561 ) ) ;
#28138 = CARTESIAN_POINT ( 'NONE',  ( -0.6971942568897637749, 2.189545951927499583E-17, 1.498523621993480326 ) ) ;
#28139 = EDGE_LOOP ( 'NONE', ( #42996, #32274, #23486, #29192 ) ) ;
#28140 = CARTESIAN_POINT ( 'NONE',  ( -1.002407869896990045, 0.1264236179284866091, 1.094980314906866203 ) ) ;
#28141 = CARTESIAN_POINT ( 'NONE',  ( -0.3100393700787401619, 3.218313930830148909E-16, -1.043307086614172707 ) ) ;
#28142 = CARTESIAN_POINT ( 'NONE',  ( 0.6971942568897648851, -0.07405724077823297447, 1.033464566875371027 ) ) ;
#28143 = VERTEX_POINT ( 'NONE', #14268 ) ;
#28144 = CARTESIAN_POINT ( 'NONE',  ( 0.7646288533564489232, 0.1113553986120547346, 0.1033464566929133965 ) ) ;
#28145 = CARTESIAN_POINT ( 'NONE',  ( -0.8107537697050253289, 0.1574803149606300301, 1.360728346456693050 ) ) ;
#28146 = CARTESIAN_POINT ( 'NONE',  ( -0.6971942568897626646, -0.07405724077823297447, 0.8316929133320636325 ) ) ;
#28147 = CARTESIAN_POINT ( 'NONE',  ( -0.7027069653493529522, 0.03506913149605040553, 0.03937007874015843734 ) ) ;
#28148 = CARTESIAN_POINT ( 'NONE',  ( 1.054774247047244540, -0.07405724077823318263, 0.1033464566391499029 ) ) ;
#28149 = CARTESIAN_POINT ( 'NONE',  ( -0.9500414927467377701, 0.1787899950787401604, 0.1476377952218271561 ) ) ;
#28150 = CARTESIAN_POINT ( 'NONE',  ( 0.9873396505805591694, -0.1113553986120547346, 1.609251968396409493 ) ) ;
#28151 = ORIENTED_EDGE ( 'NONE', *, *, #8699, .F. ) ;
#28152 = LINE ( 'NONE', #39138, #9176 ) ;
#28153 = ORIENTED_EDGE ( 'NONE', *, *, #7315, .T. ) ;
#28154 = CARTESIAN_POINT ( 'NONE',  ( -0.6971942568897648851, -0.07405724077823297447, 1.776574803095843702 ) ) ;
#28155 = EDGE_CURVE ( 'NONE', #47218, #26504, #5271, .T. ) ;
#28156 = CONICAL_SURFACE ( 'NONE', #40359, 0.09842519685039370636, 0.9599310885968824758 ) ;
#28157 = ADVANCED_FACE ( 'NONE', ( #29864 ), #33209, .F. ) ;
#28158 = CARTESIAN_POINT ( 'NONE',  ( 0.000000000000000000, 0.000000000000000000, -0.07924015748031493223 ) ) ;
#28159 = FACE_OUTER_BOUND ( 'NONE', #2993, .T. ) ;
#28160 = CARTESIAN_POINT ( 'NONE',  ( -0.1264236179284866091, -1.084277511536324790, -0.1264236179284866091 ) ) ;
#28161 = ORIENTED_EDGE ( 'NONE', *, *, #22188, .F. ) ;
#28162 = CARTESIAN_POINT ( 'NONE',  ( -0.1264236179284866091, -0.1628937007336379861, -0.1264236179284866091 ) ) ;
#28163 = EDGE_CURVE ( 'NONE', #7550, #8597, #4163, .T. ) ;
#28164 = VERTEX_POINT ( 'NONE', #43470 ) ;
#28165 = CARTESIAN_POINT ( 'NONE',  ( 0.6971942568897648851, -0.07405724077823297447, 1.067913385773007651 ) ) ;
#28166 = EDGE_CURVE ( 'NONE', #40452, #6613, #44405, .T. ) ;
#28167 = CARTESIAN_POINT ( 'NONE',  ( 0.1574803149606299746, 0.7443365962042343131, -3.523993443072799270 ) ) ;
#28168 = CARTESIAN_POINT ( 'NONE',  ( 0.8107537697050253289, -0.1574803149606297803, 1.847933070866143002 ) ) ;
#28169 = CARTESIAN_POINT ( 'NONE',  ( 0.1797182628040039087, -0.2593942032838327805, 0.07444174185955046430 ) ) ;
#28170 = CARTESIAN_POINT ( 'NONE',  ( 0.1787899950787401882, -0.8124999999462361178, -2.189545951927503898E-17 ) ) ;
#28171 = VECTOR ( 'NONE', #27441, 39.37007874015748143 ) ;
#28172 = CARTESIAN_POINT ( 'NONE',  ( -0.07444174185955065859, -1.332228848953123990, 0.1797182628040039087 ) ) ;
#28173 = CARTESIAN_POINT ( 'NONE',  ( -0.7185039370078746268, 0.06523048226347956391, 0.2239173228346459099 ) ) ;
#28174 = CARTESIAN_POINT ( 'NONE',  ( 0.8759842519685039353, 0.1787899950787401882, 1.099901574749385880 ) ) ;
#28175 = CARTESIAN_POINT ( 'NONE',  ( 0.6971942568897637749, 2.189545951927499583E-17, 1.577263779473795369 ) ) ;
#28176 = CARTESIAN_POINT ( 'NONE',  ( 0.6971942568897626646, -0.07405724077823297447, 0.2017716534895435399 ) ) ;
#28177 = CARTESIAN_POINT ( 'NONE',  ( -1.060626887254335780E-16, -0.0009842519685041700977, -0.4921259842519680183 ) ) ;
#28178 = CARTESIAN_POINT ( 'NONE',  ( 0.8107537697050253289, -0.1574803149606297803, 1.690452755905512916 ) ) ;
#28180 = CARTESIAN_POINT ( 'NONE',  ( -0.8384580214048182878, 0.1542633986724651907, 1.979083352843399535 ) ) ;
#28179 = CARTESIAN_POINT ( 'NONE',  ( 0.7954198352444098452, 0.1386465761046554446, 1.980005308839364320 ) ) ;
#28181 = CYLINDRICAL_SURFACE ( 'NONE', #11370, 0.1864803149606298061 ) ;
#28182 = CARTESIAN_POINT ( 'NONE',  ( -0.7646288533564489232, -0.1113553986120547346, 1.717519684931842594 ) ) ;
#28183 = AXIS2_PLACEMENT_3D ( 'NONE', #39131, #6302, #46557 ) ;
#28184 = CARTESIAN_POINT ( 'NONE',  ( 0.1787899950787401882, -0.02017716530056720692, -2.189545951927503898E-17 ) ) ;
#28185 = CARTESIAN_POINT ( 'NONE',  ( 0.8759842519685039353, -0.1787899950787401882, 0.2091535432533232486 ) ) ;
#28186 = CARTESIAN_POINT ( 'NONE',  ( -1.033464566929133799, 0.000000000000000000, 0.7086614172153071767 ) ) ;
#28187 = CARTESIAN_POINT ( 'NONE',  ( 1.002407869896990045, -0.1264236179284866091, 1.080216535379306952 ) ) ;
#28188 = DIRECTION ( 'NONE',  ( 0.000000000000000000, 0.000000000000000000, -1.000000000000000000 ) ) ;
#28189 = CARTESIAN_POINT ( 'NONE',  ( 0.8759842519685039353, -0.1574803149606299191, 0.4625984250893235838 ) ) ;
#28190 = VERTEX_POINT ( 'NONE', #33439 ) ;
#28191 = DIRECTION ( 'NONE',  ( -5.159318851433039196E-16, -0.6156614753256609562, -0.7880107536067197938 ) ) ;
#28192 = CARTESIAN_POINT ( 'NONE',  ( 0.1574803149606300301, -1.019192913278299528, -0.06523048226347956391 ) ) ;
#28193 = CARTESIAN_POINT ( 'NONE',  ( -1.033464566929134687, 0.06523048226347956391, 0.4355314959554649756 ) ) ;
#28194 = EDGE_LOOP ( 'NONE', ( #17270, #23835, #19369, #37306 ) ) ;
#28195 = CARTESIAN_POINT ( 'NONE',  ( 0.6971942568897648851, 0.07405724077823318263, 1.259842519631276359 ) ) ;
#28196 = FACE_BOUND ( 'NONE', #20810, .T. ) ;
#28197 = CARTESIAN_POINT ( 'NONE',  ( -0.1787899950787401604, -0.03740157474938609478, 0.07405724077823318263 ) ) ;
#28198 = CARTESIAN_POINT ( 'NONE',  ( 0.1588891437628947301, -0.04395497937029503588, -0.1404564352527339355 ) ) ;
#28199 = DIRECTION ( 'NONE',  ( 1.000000000000000000, 0.000000000000000000, 0.000000000000000000 ) ) ;
#28200 = CARTESIAN_POINT ( 'NONE',  ( 0.1644020957507539848, -0.1623118080249112138, 7.560884646099310910E-18 ) ) ;
#28201 = DIRECTION ( 'NONE',  ( -1.000000000000000000, 0.000000000000000000, 0.000000000000000000 ) ) ;
#28202 = ORIENTED_EDGE ( 'NONE', *, *, #32209, .T. ) ;
#28203 = CARTESIAN_POINT ( 'NONE',  ( -0.7495606340400177148, 0.1264236179284866091, 1.414862204670645829 ) ) ;
#28204 = CARTESIAN_POINT ( 'NONE',  ( 0.07405724077823318263, -1.764763779473795813, 0.1787899950787401604 ) ) ;
#28205 = CARTESIAN_POINT ( 'NONE',  ( -0.8019270111902717657, 0.1787899950787401604, 0.9842519684501742638 ) ) ;
#28206 = CARTESIAN_POINT ( 'NONE',  ( -0.8759842519685039353, -0.1787899950787401882, 1.902066929080094448 ) ) ;
#28207 = CARTESIAN_POINT ( 'NONE',  ( -0.8759842519685039353, -0.1787899950787401882, 1.114665354276944909 ) ) ;
#28208 = CARTESIAN_POINT ( 'NONE',  ( -0.6971942568897626646, -0.07405724077823297447, 0.6397637794737947026 ) ) ;
#28209 = EDGE_CURVE ( 'NONE', #15230, #17877, #27481, .T. ) ;
#28210 = CIRCLE ( 'NONE', #9832, 0.2471922904502826812 ) ;
#28211 = CARTESIAN_POINT ( 'NONE',  ( 0.8759842519685039353, -0.1574803149606299191, 1.811023622047244208 ) ) ;
#28212 = CARTESIAN_POINT ( 'NONE',  ( 0.4453382816733590377, 4.766607801171850497E-17, 0.000000000000000000 ) ) ;
#28213 = ORIENTED_EDGE ( 'NONE', *, *, #41797, .T. ) ;
#28214 = CARTESIAN_POINT ( 'NONE',  ( -0.03548959504743665755, -0.08956203235299665943, 0.1510601953534446984 ) ) ;
#28215 = CARTESIAN_POINT ( 'NONE',  ( -0.06008722723381313552, -0.08905839832210296625, 0.1460962461687339564 ) ) ;
#28216 = ORIENTED_EDGE ( 'NONE', *, *, #46512, .F. ) ;
#28217 = FACE_OUTER_BOUND ( 'NONE', #9856, .T. ) ;
#28218 = ADVANCED_FACE ( 'NONE', ( #47075 ), #7764, .F. ) ;
#28219 = CARTESIAN_POINT ( 'NONE',  ( -0.8019270111902717657, 0.1787899950787401604, 0.6643700786863951935 ) ) ;
#28220 = DIRECTION ( 'NONE',  ( -1.000000000000000000, 0.000000000000000000, 0.000000000000000000 ) ) ;
#28221 = VERTEX_POINT ( 'NONE', #87 ) ;
#28222 = CARTESIAN_POINT ( 'NONE',  ( -1.054774247047244540, -0.07405724077823318263, 1.678149606245448622 ) ) ;
#28223 = DIRECTION ( 'NONE',  ( -1.000000000000000000, 0.000000000000000000, 0.000000000000000000 ) ) ;
#28224 = ( BOUNDED_CURVE ( )  B_SPLINE_CURVE ( 2, ( #6383, #17650, #13820, #3015, #14311, #36363, #21472, #42781, #20994 ),
 .UNSPECIFIED., .F., .T. ) 
 B_SPLINE_CURVE_WITH_KNOTS ( ( 3, 2, 2, 2, 3 ),
 ( 0.3800000000000000044, 0.3825000000000000067, 0.3850000000000000089, 0.3875000000000000111, 0.3900000000000000133 ),
 .UNSPECIFIED. ) 
 CURVE ( )  GEOMETRIC_REPRESENTATION_ITEM ( )  RATIONAL_B_SPLINE_CURVE ( ( 1.000000000000000000, 0.9238795325112869605, 1.000000000000000000, 0.9238795325112869605, 1.000000000000000000, 0.9238795325112869605, 1.000000000000000000, 0.9238795325112869605, 1.000000000000000000 ) ) 
 REPRESENTATION_ITEM ( '' )  ) ;
#28225 = CARTESIAN_POINT ( 'NONE',  ( -0.7185039370078732945, -0.06523048226347920309, 0.1796259841444415029 ) ) ;
#28226 = CARTESIAN_POINT ( 'NONE',  ( 0.8759842519685039353, 0.1574803149606299191, 0.6496062992125984925 ) ) ;
#28227 = CARTESIAN_POINT ( 'NONE',  ( 0.1797182628040039365, -0.7293745182444626440, -2.200913952912460540E-17 ) ) ;
#28228 = CARTESIAN_POINT ( 'NONE',  ( 0.2471922904502826812, 0.03219022224904106305, 0.1427165354330708902 ) ) ;
#28229 = CARTESIAN_POINT ( 'NONE',  ( -0.7185039370078746268, -0.06523048226347956391, 1.321358267609009429 ) ) ;
#28230 = CARTESIAN_POINT ( 'NONE',  ( 0.7495606340400177148, 0.1264236179284866091, 0.6717519684501732646 ) ) ;
#28231 = CARTESIAN_POINT ( 'NONE',  ( -0.1574803149606300301, -0.6205708661417322913, -0.06523048226347956391 ) ) ;
#28232 = CARTESIAN_POINT ( 'NONE',  ( 0.2471922904502825702, 0.05534442469270777626, -0.1143959998688843099 ) ) ;
#28233 = VERTEX_POINT ( 'NONE', #40109 ) ;
#28234 = CARTESIAN_POINT ( 'NONE',  ( -0.2559055118110236116, 0.03045100533025396627, -0.03118462788502844932 ) ) ;
#28235 = B_SPLINE_CURVE_WITH_KNOTS ( 'NONE', 3,
 ( #13594, #21011, #28232, #23093, #44631, #31014, #45580, #16155, #44872, #23570, #45354, #11846, #40162, #30549, #4618, #4864, #5101, #7995, #30100, #22620 ),
 .UNSPECIFIED., .F., .F.,
 ( 4, 1, 1, 1, 1, 1, 2, 2, 1, 1, 1, 2, 2, 4 ),
 ( 0.000000000000000000, 0.2499999999999993339, 0.3749999999999988898, 0.4374999999999986677, 0.4687499999999986122, 0.4843749999999986677, 0.4921874999999986122, 0.4999999999999986122, 0.6249999999999983347, 0.6874999999999982236, 0.7187499999999982236, 0.7343749999999982236, 0.7499999999999983347, 1.000000000000000000 ),
 .UNSPECIFIED. ) ;
#28236 = CARTESIAN_POINT ( 'NONE',  ( 0.7185039370078739607, 1.928577636452523993E-17, 1.328740157480315043 ) ) ;
#28238 = FILL_AREA_STYLE ('',( #6641 ) ) ;
#28237 = DIRECTION ( 'NONE',  ( 1.000000000000000000, 0.000000000000000000, 0.000000000000000000 ) ) ;
#28239 = CARTESIAN_POINT ( 'NONE',  ( 0.8759842519685039353, -0.1574803149606299191, 1.968503937007874072 ) ) ;
#28240 = EDGE_CURVE ( 'NONE', #18121, #2766, #7526, .T. ) ;
#28242 = CARTESIAN_POINT ( 'NONE',  ( 0.8107537697050254399, -0.1574803149606297803, 1.680610236112946465 ) ) ;
#28241 = CARTESIAN_POINT ( 'NONE',  ( 1.054774247047244096, 0.000000000000000000, 0.6914370078202519698 ) ) ;
#28243 = VECTOR ( 'NONE', #12632, 39.37007874015748143 ) ;
#28244 = CARTESIAN_POINT ( 'NONE',  ( 0.9412147342319837628, 0.1574803149606300301, 1.552657480314961758 ) ) ;
#28245 = EDGE_LOOP ( 'NONE', ( #2773, #12888, #31562, #47273 ) ) ;
#28246 = CARTESIAN_POINT ( 'NONE',  ( -1.033464566929133799, 0.000000000000000000, 1.072834645669291431 ) ) ;
#28247 = CARTESIAN_POINT ( 'NONE',  ( 0.7646288533564489232, -0.1113553986120547346, 1.727362204724409489 ) ) ;
#28248 = CARTESIAN_POINT ( 'NONE',  ( 0.000000000000000000, 0.000000000000000000, -0.3149606299212598381 ) ) ;
#28249 = CARTESIAN_POINT ( 'NONE',  ( 1.054774247047244096, 0.000000000000000000, 0.8095472440407244230 ) ) ;
#28250 = CARTESIAN_POINT ( 'NONE',  ( 0.8759842519685039353, -0.1574803149606299191, 1.299212598425196985 ) ) ;
#28251 = DIRECTION ( 'NONE',  ( 0.000000000000000000, 1.000000000000000000, 0.000000000000000000 ) ) ;
#28252 = CARTESIAN_POINT ( 'NONE',  ( -0.07444174185955065859, 0.1490703636453008241, -0.1797182628040039087 ) ) ;
#28253 = CARTESIAN_POINT ( 'NONE',  ( 0.07405724077823318263, -1.095472440891117838, 0.1787899950787401604 ) ) ;
#28255 = AXIS2_PLACEMENT_3D ( 'NONE', #1363, #34699, #1127 ) ;
#28254 = CARTESIAN_POINT ( 'NONE',  ( -9.642888182262618425E-18, -1.572834645669291431, -0.1574803149606299191 ) ) ;
#28257 = ( BOUNDED_CURVE ( )  B_SPLINE_CURVE ( 2, ( #27505, #34430, #9259, #23877, #45423, #38488, #12640, #8778, #45894 ),
 .UNSPECIFIED., .F., .T. ) 
 B_SPLINE_CURVE_WITH_KNOTS ( ( 3, 2, 2, 2, 3 ),
 ( 0.6099999999999999867, 0.6125000000000000444, 0.6149999999999999911, 0.6175000000000000488, 0.6199999999999999956 ),
 .UNSPECIFIED. ) 
 CURVE ( )  GEOMETRIC_REPRESENTATION_ITEM ( )  RATIONAL_B_SPLINE_CURVE ( ( 1.000000000000000000, 0.9238795325112899581, 1.000000000000000000, 0.9238795325112869605, 1.000000000000000000, 0.9238795325112869605, 1.000000000000000000, 0.9238795325112869605, 1.000000000000000000 ) ) 
 REPRESENTATION_ITEM ( '' )  ) ;
#28256 = CARTESIAN_POINT ( 'NONE',  ( 0.9412147342319837628, -0.1574803149606297803, 1.252460629813731741 ) ) ;
#28258 = DIRECTION ( 'NONE',  ( 0.000000000000000000, 0.000000000000000000, 1.000000000000000000 ) ) ;
#28259 = CARTESIAN_POINT ( 'NONE',  ( -0.8759842519685039353, 0.1787899950787401882, 1.926673228292693052 ) ) ;
#28260 = VECTOR ( 'NONE', #14808, 39.37007874015748143 ) ;
#28261 = CARTESIAN_POINT ( 'NONE',  ( 1.002407869896990045, 0.1264236179284866091, 1.961122047190330786 ) ) ;
#28262 = ORIENTED_EDGE ( 'NONE', *, *, #35015, .F. ) ;
#28263 = EDGE_CURVE ( 'NONE', #7400, #37374, #27558, .T. ) ;
#28264 = CYLINDRICAL_SURFACE ( 'NONE', #35830, 0.1574803149606299191 ) ;
#28265 = CARTESIAN_POINT ( 'NONE',  ( -1.054774247047244096, 0.000000000000000000, 1.006397637741511808 ) ) ;
#28266 = EDGE_CURVE ( 'NONE', #34889, #4911, #17405, .T. ) ;
#28267 = CARTESIAN_POINT ( 'NONE',  ( -1.002407869896990045, -0.1264236179284866091, 0.2583661416785200671 ) ) ;
#28268 = EDGE_CURVE ( 'NONE', #34984, #1339, #32832, .T. ) ;
#28269 = CARTESIAN_POINT ( 'NONE',  ( -0.7185039370078739607, 1.928577636452523993E-17, 1.791338582569637738 ) ) ;
#28270 = CARTESIAN_POINT ( 'NONE',  ( -0.8019270111902717657, 0.1787899950787401604, 1.850393700733638624 ) ) ;
#28271 = CARTESIAN_POINT ( 'NONE',  ( -0.8759842519685039353, -0.1787899950787401882, 0.1353346456155279653 ) ) ;
#28272 = CARTESIAN_POINT ( 'NONE',  ( -0.9873396505805591694, 0.1113553986120547346, 1.943897637795275690 ) ) ;
#28273 = CARTESIAN_POINT ( 'NONE',  ( 0.2559054998105182999, 0.08068256135019109820, -0.05400407908655117245 ) ) ;
#28274 = CARTESIAN_POINT ( 'NONE',  ( -1.094772975963752103E-17, -0.2624271178355381817, -0.1787899950787401882 ) ) ;
#28275 = CARTESIAN_POINT ( 'NONE',  ( -0.1299468115398441093, -0.09842519685039370636, 0.1029827665312899737 ) ) ;
#28276 = CARTESIAN_POINT ( 'NONE',  ( -0.8759842519685039353, -0.1574803149606299191, 1.496062992125984259 ) ) ;
#28277 = FACE_OUTER_BOUND ( 'NONE', #4624, .T. ) ;
#28278 = EDGE_CURVE ( 'NONE', #31834, #40149, #14981, .T. ) ;
#28279 = CARTESIAN_POINT ( 'NONE',  ( -0.9500414927467378812, -0.1787899950787401604, 0.09350393695411057804 ) ) ;
#28280 = VECTOR ( 'NONE', #42688, 39.37007874015748143 ) ;
#28281 = ORIENTED_EDGE ( 'NONE', *, *, #33690, .T. ) ;
#28282 = CARTESIAN_POINT ( 'NONE',  ( -0.6971942568897648851, -0.07405724077823297447, 1.230314960576158967 ) ) ;
#28283 = ORIENTED_EDGE ( 'NONE', *, *, #8326, .T. ) ;
#28284 = CARTESIAN_POINT ( 'NONE',  ( 0.1787899950787401882, -1.206200787347811110, -2.189545951927503898E-17 ) ) ;
#28285 = CARTESIAN_POINT ( 'NONE',  ( -0.1264236179284866091, -1.294783464513165283, 0.1264236179284866091 ) ) ;
#28286 = ( CONVERSION_BASED_UNIT ( 'INCH', #24441 ) LENGTH_UNIT ( ) NAMED_UNIT ( #35696 ) ) ;
#28287 = CARTESIAN_POINT ( 'NONE',  ( -0.1270800023317771588, -0.4291776678507621678, 0.1270800023317771588 ) ) ;
#28288 = CARTESIAN_POINT ( 'NONE',  ( 1.033464566929133799, 0.000000000000000000, 0.2460629921259842590 ) ) ;
#28289 = CARTESIAN_POINT ( 'NONE',  ( -0.9873396505805591694, 0.1113553986120547346, 0.9498031494987716483 ) ) ;
#28290 = CARTESIAN_POINT ( 'NONE',  ( -0.7646288533564489232, -0.1113553986120547346, 0.7431102362204724532 ) ) ;
#28291 = CIRCLE ( 'NONE', #40527, 0.1968503937007874405 ) ;
#28292 = CARTESIAN_POINT ( 'NONE',  ( -0.1113553986120547346, -0.1407480314960629919, 0.1113553986120547346 ) ) ;
#28293 = CARTESIAN_POINT ( 'NONE',  ( 0.8759842519685039353, -0.1574803149606299191, 1.840551180994834501 ) ) ;
#28294 = CARTESIAN_POINT ( 'NONE',  ( 0.9873396505805591694, -0.1113553986120547346, 0.7529527559055118058 ) ) ;
#28295 = CARTESIAN_POINT ( 'NONE',  ( -0.9412147342319837628, 0.1574803149606300301, 1.237696850393701586 ) ) ;
#28297 = FILL_AREA_STYLE ('',( #17026 ) ) ;
#28296 = CARTESIAN_POINT ( 'NONE',  ( 1.033464566929133799, 0.000000000000000000, 1.151574803149606474 ) ) ;
#28298 = CARTESIAN_POINT ( 'NONE',  ( 0.9873396505805591694, -0.1113553986120547346, 1.097440944774362270 ) ) ;
#28299 = CARTESIAN_POINT ( 'NONE',  ( 0.9412147342319837628, 0.1574803149606300301, 0.2436023620971974057 ) ) ;
#28300 = DIRECTION ( 'NONE',  ( 0.000000000000000000, 0.000000000000000000, -1.000000000000000000 ) ) ;
#28301 = CARTESIAN_POINT ( 'NONE',  ( 0.07405724077823318263, -0.5442913385289138706, 0.1787899950787401604 ) ) ;
#28302 = CARTESIAN_POINT ( 'NONE',  ( 0.1787899950787401604, -1.395669291284819868, -0.07405724077823318263 ) ) ;
#28303 = CIRCLE ( 'NONE', #33656, 0.09842519685039370636 ) ;
#28304 = CARTESIAN_POINT ( 'NONE',  ( -1.054774247047244540, 0.07405724077823318263, 1.835629921206078485 ) ) ;
#28305 = VERTEX_POINT ( 'NONE', #3703 ) ;
#28306 = CARTESIAN_POINT ( 'NONE',  ( -0.6971942568897637749, 2.189545951927499583E-17, 1.464074803095842370 ) ) ;
#28307 = ADVANCED_FACE ( 'NONE', ( #5344 ), #19261, .T. ) ;
#28308 = CARTESIAN_POINT ( 'NONE',  ( 0.8759842519685039353, 0.1787899950787401882, 1.532972440891118060 ) ) ;
#28309 = CARTESIAN_POINT ( 'NONE',  ( -1.033464566929134687, -0.06523048226347956391, 0.9128937007874010634 ) ) ;
#28310 = CARTESIAN_POINT ( 'NONE',  ( -9.642888182262618425E-18, -1.287401574695621997, -0.1574803149606299191 ) ) ;
#28311 = CARTESIAN_POINT ( 'NONE',  ( 0.7495606340400177148, 0.1264236179284866091, 0.1599409448281264023 ) ) ;
#28312 = CARTESIAN_POINT ( 'NONE',  ( 0.1348365057045624593, -0.09842519898778306908, -0.1174095120931970271 ) ) ;
#28313 = ( NAMED_UNIT ( * ) PLANE_ANGLE_UNIT ( ) SI_UNIT ( $, .RADIAN. ) ) ;
#28314 = CARTESIAN_POINT ( 'NONE',  ( -1.054774247047244540, 0.07405724077823318263, 0.6151574802611965431 ) ) ;
#28315 = AXIS2_PLACEMENT_3D ( 'NONE', #8668, #22345, #37678 ) ;
#28316 = CARTESIAN_POINT ( 'NONE',  ( -0.1574803149606299191, -0.2237541348899642346, -1.272196386806234925 ) ) ;
#28317 = EDGE_CURVE ( 'NONE', #19054, #28080, #30796, .T. ) ;
#28318 = DIRECTION ( 'NONE',  ( -1.000000000000000000, 0.000000000000000000, 0.000000000000000000 ) ) ;
#28319 = ORIENTED_EDGE ( 'NONE', *, *, #27144, .F. ) ;
#28320 = CARTESIAN_POINT ( 'NONE',  ( -0.1574803149606299191, -0.2539370077664885872, 0.000000000000000000 ) ) ;
#28321 = CARTESIAN_POINT ( 'NONE',  ( -0.8019270111902717657, 0.1787899950787401604, 1.456692913332062744 ) ) ;
#28322 = CARTESIAN_POINT ( 'NONE',  ( -0.8759842519685039353, 0.1574803149606299191, 0.5314960629921260393 ) ) ;
#28323 = CARTESIAN_POINT ( 'NONE',  ( 0.8759842519685039353, -0.1787899950787401882, 1.316437007820252081 ) ) ;
#28324 = CARTESIAN_POINT ( 'NONE',  ( 0.2064083604912952674, -0.09851384708312717342, -0.01080128761237854514 ) ) ;
#28325 = EDGE_LOOP ( 'NONE', ( #41750, #44186, #20879, #41519, #40487, #31368 ) ) ;
#28326 = DIRECTION ( 'NONE',  ( 1.000000000000000000, 0.000000000000000000, 0.000000000000000000 ) ) ;
#28327 = CARTESIAN_POINT ( 'NONE',  ( -0.1787899950787401604, -1.746186960355224027, 0.07405724077823318263 ) ) ;
#28328 = ORIENTED_EDGE ( 'NONE', *, *, #43656, .T. ) ;
#28329 = CARTESIAN_POINT ( 'NONE',  ( -0.1264236179284866091, -0.6648622046706456068, 0.1264236179284866091 ) ) ;
#28330 = CARTESIAN_POINT ( 'NONE',  ( 0.8107537697050254399, -0.1574803149606297803, 1.611712598425196319 ) ) ;
#28331 = CARTESIAN_POINT ( 'NONE',  ( 0.9412147342319837628, 0.1574803149606300301, 0.4896653543307082357 ) ) ;
#28332 = ORIENTED_EDGE ( 'NONE', *, *, #25825, .F. ) ;
#28333 = CARTESIAN_POINT ( 'NONE',  ( 0.8759842519685039353, 0.1787899950787401882, 1.449311023568283341 ) ) ;
#28334 = CARTESIAN_POINT ( 'NONE',  ( 0.4620708661417327612, 0.1864803149606299448, -1.186023622047243986 ) ) ;
#28335 = CARTESIAN_POINT ( 'NONE',  ( 0.1787899950787401604, -0.2637795275052916555, 0.07405724077823318263 ) ) ;
#28336 = CARTESIAN_POINT ( 'NONE',  ( 3.284318927891251994E-17, -0.6993110235682834519, 0.1787899950787401882 ) ) ;
#28337 = AXIS2_PLACEMENT_3D ( 'NONE', #11989, #26612, #8368 ) ;
#28338 = DIRECTION ( 'NONE',  ( -1.000000000000000000, 0.000000000000000000, 0.000000000000000000 ) ) ;
#28339 = DIRECTION ( 'NONE',  ( 0.000000000000000000, 0.000000000000000000, 1.000000000000000000 ) ) ;
#28340 = CARTESIAN_POINT ( 'NONE',  ( 0.9500414927467378812, 0.1787899950787401604, 1.683070866087970074 ) ) ;
#28341 = CARTESIAN_POINT ( 'NONE',  ( 1.002407869896990045, -0.1264236179284866091, 0.2928149605761578567 ) ) ;
#28342 = CARTESIAN_POINT ( 'NONE',  ( -0.1264236179284866091, 0.05745477192824158252, -0.1264236179284866091 ) ) ;
#28343 = CARTESIAN_POINT ( 'NONE',  ( 0.1787899950787401604, 0.01181102367581077402, 0.07405724077823318263 ) ) ;
#28344 = ITEM_DEFINED_TRANSFORMATION ( 'NONE', 'NONE', #9470,  #20860 ) ;
#28345 = DIRECTION ( 'NONE',  ( -1.000000000000000000, 0.000000000000000000, 0.000000000000000000 ) ) ;
#28346 = CARTESIAN_POINT ( 'NONE',  ( -0.7185039370078739607, 1.928577636452523993E-17, 1.476377952648377789 ) ) ;
#28347 = CARTESIAN_POINT ( 'NONE',  ( 0.6971942568897626646, 0.07405724077823318263, 0.5905511810485987167 ) ) ;
#28348 = DIMENSIONAL_EXPONENTS ( 1.000000000000000000, 0.000000000000000000, 0.000000000000000000, 0.000000000000000000, 0.000000000000000000, 0.000000000000000000, 0.000000000000000000 ) ;
#28349 = CARTESIAN_POINT ( 'NONE',  ( -0.8019270111902716547, -0.1787899950787401604, 0.8021653542769462408 ) ) ;
#28350 = CARTESIAN_POINT ( 'NONE',  ( 0.1113553986120547346, -0.8395669291338583307, 0.1113553986120547346 ) ) ;
#28352 = CARTESIAN_POINT ( 'NONE',  ( -0.7245660696681988089, -0.07386863617677040528, 1.984694592573497784 ) ) ;
#28351 = CARTESIAN_POINT ( 'NONE',  ( -0.1270800023317771588, -1.728390266275958709, 0.1270800023317771588 ) ) ;
#28353 = CARTESIAN_POINT ( 'NONE',  ( -0.1113553986120547346, -0.4852362203649134287, 0.1113553986120547346 ) ) ;
#28354 = CARTESIAN_POINT ( 'NONE',  ( 0.1787899950787401882, -0.3351377952218271283, -2.189545951927503898E-17 ) ) ;
#28355 = CARTESIAN_POINT ( 'NONE',  ( -1.033464566929133799, 1.928577636452533546E-17, 2.007874015640504162 ) ) ;
#28356 = CARTESIAN_POINT ( 'NONE',  ( 1.054774247047244540, 0.07405724077823318263, 1.643700787347811998 ) ) ;
#28358 = CARTESIAN_POINT ( 'NONE',  ( -0.8759842519685039353, -0.1574803149606299191, 1.811023622047244208 ) ) ;
#28357 = CARTESIAN_POINT ( 'NONE',  ( 0.6971942568897648851, -0.07405724077823297447, 1.973425196796630088 ) ) ;
#28359 = CARTESIAN_POINT ( 'NONE',  ( 0.7495606340400177148, -0.1264236179284866091, 0.3617125983714334359 ) ) ;
#28360 = ORIENTED_EDGE ( 'NONE', *, *, #7906, .F. ) ;
#28361 = ADVANCED_FACE ( 'NONE', ( #26477 ), #19967, .T. ) ;
#28362 = FACE_OUTER_BOUND ( 'NONE', #24261, .T. ) ;
#28364 = CARTESIAN_POINT ( 'NONE',  ( -0.1787899950787401604, -0.04232283459190575720, 0.07405724077823318263 ) ) ;
#28363 = CARTESIAN_POINT ( 'NONE',  ( 0.1574803149606300301, -0.9010826770578276301, -0.06523048226347956391 ) ) ;
#28365 = CARTESIAN_POINT ( 'NONE',  ( 1.002407869896990045, 0.1264236179284866091, 0.5388779527021417826 ) ) ;
#28366 = CARTESIAN_POINT ( 'NONE',  ( 0.1787899950787401604, -0.8838582676627719792, -0.07405724077823318263 ) ) ;
#28367 = CARTESIAN_POINT ( 'NONE',  ( 1.002407869896990045, 0.1264236179284866091, 0.03198818892261445085 ) ) ;
#28368 = DIRECTION ( 'NONE',  ( 1.000000000000000000, -3.469446951953614978E-15, 0.000000000000000000 ) ) ;
#28369 = CARTESIAN_POINT ( 'NONE',  ( 1.002407869896990045, 0.1264236179284866091, 0.5388779527021417826 ) ) ;
#28370 = CARTESIAN_POINT ( 'NONE',  ( -0.7646288533564489232, -0.1113553986120547346, 0.9793307086614173596 ) ) ;
#28371 = CARTESIAN_POINT ( 'NONE',  ( -1.054774247047244096, 0.000000000000000000, 1.400098425143086800 ) ) ;
#28372 = ORIENTED_EDGE ( 'NONE', *, *, #5787, .T. ) ;
#28373 = CARTESIAN_POINT ( 'NONE',  ( -1.054774247047244096, 0.000000000000000000, 1.090059055064346527 ) ) ;
#28374 = CARTESIAN_POINT ( 'NONE',  ( -0.2741503469832766160, -0.1449524958156367394, -0.9602583337237132755 ) ) ;
#28375 = EDGE_CURVE ( 'NONE', #43268, #36366, #41042, .T. ) ;
#28376 = CARTESIAN_POINT ( 'NONE',  ( 0.6971942568897648851, -0.07405724077823297447, 1.151574803095843036 ) ) ;
#28377 = CARTESIAN_POINT ( 'NONE',  ( -0.1574803149606299191, -1.120078740049952781, 0.000000000000000000 ) ) ;
#28378 = CARTESIAN_POINT ( 'NONE',  ( -0.7646288533564489232, 0.1113553986120547346, 0.6446850392625511628 ) ) ;
#28379 = CARTESIAN_POINT ( 'NONE',  ( 0.000000000000000000, 0.4265678656643324129, 0.4783464566929144235 ) ) ;
#28380 = CARTESIAN_POINT ( 'NONE',  ( 0.6971942568897637749, 2.189545951927499583E-17, 1.852854330654897685 ) ) ;
#28381 = CARTESIAN_POINT ( 'NONE',  ( -0.9873396505805591694, 0.1113553986120547346, 1.432086614173228245 ) ) ;
#28382 = CARTESIAN_POINT ( 'NONE',  ( -0.6971942568897626646, 0.07405724077823318263, 0.8661417322297003674 ) ) ;
#28383 = CARTESIAN_POINT ( 'NONE',  ( 1.033464566929134687, -0.06523048226347956391, 1.808562992018457161 ) ) ;
#28384 = CARTESIAN_POINT ( 'NONE',  ( -0.7013252071282976008, 0.02113730517513252166, 0.03937007874015843734 ) ) ;
#28385 = CARTESIAN_POINT ( 'NONE',  ( 0.9500414927467377701, -0.1787899950787401604, 0.09842519679663024046 ) ) ;
#28386 = CARTESIAN_POINT ( 'NONE',  ( 0.7646288533564489232, -0.1113553986120547346, 1.638779527451527551 ) ) ;
#28387 = VERTEX_POINT ( 'NONE', #4872 ) ;
#28388 = VECTOR ( 'NONE', #2904, 39.37007874015748143 ) ;
#28389 = CARTESIAN_POINT ( 'NONE',  ( -0.07405724077823318263, 0.1053149606836847191, -0.1787899950787401604 ) ) ;
#28390 = CARTESIAN_POINT ( 'NONE',  ( 0.2151545284320233176, -0.1712747073548132604, -0.06815351164857932909 ) ) ;
#28391 = CARTESIAN_POINT ( 'NONE',  ( 1.054774247047244096, 0.000000000000000000, 0.8144685038832440993 ) ) ;
#28392 = CARTESIAN_POINT ( 'NONE',  ( -1.054774247047244540, 0.07405724077823318263, 1.717519684985606476 ) ) ;
#28393 = CIRCLE ( 'NONE', #36789, 0.009842519685039378616 ) ;
#28394 = VECTOR ( 'NONE', #15707, 39.37007874015748854 ) ;
#28395 = CARTESIAN_POINT ( 'NONE',  ( -0.2471922904502826812, 0.09336655125506151953, -0.03811874944176997515 ) ) ;
#28396 = CARTESIAN_POINT ( 'NONE',  ( -1.033464566929134687, -0.06523048226347956391, 0.7947834645669290543 ) ) ;
#28397 = CARTESIAN_POINT ( 'NONE',  ( -0.07405724077823318263, -1.362328692638688388, -0.1787899950787401604 ) ) ;
#28398 = ORIENTED_EDGE ( 'NONE', *, *, #17360, .F. ) ;
#28399 = CARTESIAN_POINT ( 'NONE',  ( -0.1787899950787401882, -0.1186023621509610243, 0.000000000000000000 ) ) ;
#28400 = EDGE_LOOP ( 'NONE', ( #19694, #18613, #16505, #11062, #27054 ) ) ;
#28401 = CARTESIAN_POINT ( 'NONE',  ( 0.7495606340400177148, 0.1264236179284866091, 1.099901574749385880 ) ) ;
#28402 = DIRECTION ( 'NONE',  ( 0.8191520442889989040, 1.003171929053533375E-16, -0.5735764363510359454 ) ) ;
#28403 = CARTESIAN_POINT ( 'NONE',  ( -1.033464566929134687, 0.06523048226347956391, 0.9079724408373541777 ) ) ;
#28404 = CARTESIAN_POINT ( 'NONE',  ( 0.7495606340400177148, -0.1264236179284866091, 0.04675196845017354913 ) ) ;
#28405 = ( BOUNDED_CURVE ( )  B_SPLINE_CURVE ( 2, ( #43964, #33694, #14279, #11162, #43724, #10928, #40121, #21936, #3716 ),
 .UNSPECIFIED., .F., .F. ) 
 B_SPLINE_CURVE_WITH_KNOTS ( ( 3, 2, 2, 2, 3 ),
 ( 0.4000000000000000222, 0.4025000000000000244, 0.4050000000000000266, 0.4074999999999999734, 0.4099999999999999756 ),
 .UNSPECIFIED. ) 
 CURVE ( )  GEOMETRIC_REPRESENTATION_ITEM ( )  RATIONAL_B_SPLINE_CURVE ( ( 1.000000000000000000, 0.9238795325112869605, 1.000000000000000000, 0.9238795325112869605, 1.000000000000000000, 0.9238795325112869605, 1.000000000000000000, 0.9238795325112849621, 1.000000000000000000 ) ) 
 REPRESENTATION_ITEM ( '' )  ) ;
#28406 = CARTESIAN_POINT ( 'NONE',  ( -1.094772975963752103E-17, -1.471948818843874074, -0.1787899950787401882 ) ) ;
#28407 = CARTESIAN_POINT ( 'NONE',  ( -0.1787899950787401604, -0.7116141731745821986, 0.07405724077823318263 ) ) ;
#28408 = AXIS2_PLACEMENT_3D ( 'NONE', #16045, #41870, #1634 ) ;
#28409 = CARTESIAN_POINT ( 'NONE',  ( -0.8759842519685039353, -0.1787899950787401882, 0.3321850393163153226 ) ) ;
#28410 = CARTESIAN_POINT ( 'NONE',  ( -0.2001839496640346883, 0.1799179750364343355, -0.05578523004296902232 ) ) ;
#28411 = CARTESIAN_POINT ( 'NONE',  ( 1.002407869896990045, 0.1264236179284866091, 1.173720472387181246 ) ) ;
#28412 = CARTESIAN_POINT ( 'NONE',  ( 0.6971942568897648851, 0.07405724077823318263, 1.496062992072220599 ) ) ;
#28413 = CARTESIAN_POINT ( 'NONE',  ( 0.8759842519685039353, -0.1787899950787401882, 0.1697834645131655606 ) ) ;
#28414 = CIRCLE ( 'NONE', #31461, 0.02899999999999994596 ) ;
#28416 = EDGE_CURVE ( 'NONE', #25910, #33099, #46616, .T. ) ;
#28415 = CARTESIAN_POINT ( 'NONE',  ( -6.728203135043436585E-17, 0.1564960629921311464, -0.4940944881889759444 ) ) ;
#28417 = CARTESIAN_POINT ( 'NONE',  ( 0.8107537697050254399, -0.1574803149606297803, 1.523129921152316379 ) ) ;
#28419 = CARTESIAN_POINT ( 'NONE',  ( 0.1602931993194442739, -0.07955613945526357478, -0.1377952755905511861 ) ) ;
#28418 = CIRCLE ( 'NONE', #25339, 0.09842519685039370636 ) ;
#28420 = CARTESIAN_POINT ( 'NONE',  ( 0.000000000000000000, 0.4003652867858630282, 0.7276473417831955670 ) ) ;
#28421 = CARTESIAN_POINT ( 'NONE',  ( -0.1574803149606299191, -0.7657480313885355327, 0.000000000000000000 ) ) ;
#28422 = CARTESIAN_POINT ( 'NONE',  ( -0.8107537697050253289, -0.1574803149606297803, 1.719980314853102321 ) ) ;
#28423 = CARTESIAN_POINT ( 'NONE',  ( 3.284318927891251994E-17, 0.009350393754550925460, 0.1787899950787401882 ) ) ;
#28424 = CARTESIAN_POINT ( 'NONE',  ( 1.002407869896990045, -0.1264236179284866091, 0.2140748030958428971 ) ) ;
#28425 = EDGE_CURVE ( 'NONE', #22319, #34120, #8713, .T. ) ;
#28426 = CARTESIAN_POINT ( 'NONE',  ( 0.7646288533564489232, -0.1113553986120547346, 1.648622047244094668 ) ) ;
#28428 = CARTESIAN_POINT ( 'NONE',  ( 0.6141732283464567121, 1.098083891755155421E-17, -0.08090551181102362266 ) ) ;
#28427 = CARTESIAN_POINT ( 'NONE',  ( 0.6971942568897648851, -0.07405724077823297447, 1.186023621993481658 ) ) ;
#28429 = DIRECTION ( 'NONE',  ( 0.8191520442889873577, 0.000000000000000000, 0.5735764363510523767 ) ) ;
#28430 = CARTESIAN_POINT ( 'NONE',  ( 0.7185039370078746268, -0.06523048226347956391, 0.5339566928058587791 ) ) ;
#28431 = VERTEX_POINT ( 'NONE', #44637 ) ;
#28432 = SURFACE_STYLE_USAGE ( .BOTH. , #39884 ) ;
#28433 = EDGE_CURVE ( 'NONE', #22098, #24404, #9190, .T. ) ;
#28434 = CARTESIAN_POINT ( 'NONE',  ( -0.06523048226347956391, -1.033956692805859445, 0.1574803149606297803 ) ) ;
#28435 = CARTESIAN_POINT ( 'NONE',  ( -0.7646288533564489232, -0.1113553986120547346, 0.4183070865066456645 ) ) ;
#28436 = ORIENTED_EDGE ( 'NONE', *, *, #19900, .T. ) ;
#28437 = CARTESIAN_POINT ( 'NONE',  ( 0.6971942568897648851, -0.07405724077823297447, 1.382874015694268044 ) ) ;
#28438 = EDGE_CURVE ( 'NONE', #20302, #6854, #12190, .T. ) ;
#28440 = DIRECTION ( 'NONE',  ( 0.000000000000000000, 0.000000000000000000, -1.000000000000000000 ) ) ;
#28439 = DIRECTION ( 'NONE',  ( 0.000000000000000000, 0.000000000000000000, 1.000000000000000000 ) ) ;
#28441 = CARTESIAN_POINT ( 'NONE',  ( -0.6971942568897637749, 2.189545951927499583E-17, 0.04183070860765386589 ) ) ;
#28442 = CARTESIAN_POINT ( 'NONE',  ( -1.094772975963752103E-17, -0.04970472435568527164, -0.1787899950787401882 ) ) ;
#28443 = ORIENTED_EDGE ( 'NONE', *, *, #35185, .T. ) ;
#28444 = CARTESIAN_POINT ( 'NONE',  ( -1.033464566929133799, 0.000000000000000000, 1.771653543199558811 ) ) ;
#28445 = CARTESIAN_POINT ( 'NONE',  ( 0.8759842519685039353, 0.000000000000000000, 4.498031496062992574 ) ) ;
#28446 = CARTESIAN_POINT ( 'NONE',  ( 0.6971942568897637749, 2.189545951927499583E-17, 0.3617125983714334359 ) ) ;
#28447 = ORIENTED_EDGE ( 'NONE', *, *, #12586, .T. ) ;
#28448 = CARTESIAN_POINT ( 'NONE',  ( -0.8759842519685039353, -0.1787899950787401882, 1.429625984198204858 ) ) ;
#28449 = CARTESIAN_POINT ( 'NONE',  ( 0.1787899950787401882, -1.639271653489543290, -2.189545951927503898E-17 ) ) ;
#28450 = CARTESIAN_POINT ( 'NONE',  ( -0.7495606340400177148, -0.1264236179284866091, 1.975885826717889815 ) ) ;
#28451 = ORIENTED_EDGE ( 'NONE', *, *, #25514, .T. ) ;
#28452 = CARTESIAN_POINT ( 'NONE',  ( -0.6971942568897637749, 2.189545951927499583E-17, 1.104822834591905556 ) ) ;
#28453 = CARTESIAN_POINT ( 'NONE',  ( -0.6971942568897626646, -0.07405724077823297447, 0.7578740156942689321 ) ) ;
#28454 = CARTESIAN_POINT ( 'NONE',  ( 0.5839895013123354017, -0.08090551181102362266, 0.000000000000000000 ) ) ;
#28455 = FACE_OUTER_BOUND ( 'NONE', #41015, .T. ) ;
#28456 = CARTESIAN_POINT ( 'NONE',  ( -0.07405724077823318263, -0.7324074327961683784, -0.1787899950787401604 ) ) ;
#28457 = ORIENTED_EDGE ( 'NONE', *, *, #38527, .F. ) ;
#28458 = CARTESIAN_POINT ( 'NONE',  ( 0.3246033735368759610, 0.09842519685039370636, 0.000000000000000000 ) ) ;
#28459 = CARTESIAN_POINT ( 'NONE',  ( -0.8107537697050254399, -0.1574803149606297803, 0.6569881888688504645 ) ) ;
#28460 = VERTEX_POINT ( 'NONE', #30104 ) ;
#28461 = CARTESIAN_POINT ( 'NONE',  ( -0.7185039370078746268, -0.06523048226347956391, 1.724901574803149540 ) ) ;
#28462 = AXIS2_PLACEMENT_3D ( 'NONE', #45405, #23146, #11899 ) ;
#28463 = STYLED_ITEM ( 'NONE', ( #43260 ), #20948 ) ;
#28465 = CARTESIAN_POINT ( 'NONE',  ( -0.8759842519685039353, 0.000000000000000000, 0.000000000000000000 ) ) ;
#28464 = VECTOR ( 'NONE', #22624, 39.37007874015748854 ) ;
#28466 = CARTESIAN_POINT ( 'NONE',  ( -0.6971942568897626646, -0.07405724077823297447, 0.6348425196312760255 ) ) ;
#28467 = CARTESIAN_POINT ( 'NONE',  ( 0.1574803149606299191, -0.007874015748031495954, -1.928577636452523993E-17 ) ) ;
#28468 = VERTEX_POINT ( 'NONE', #45590 ) ;
#28469 = CARTESIAN_POINT ( 'NONE',  ( -0.8759842519685039353, 0.1787899950787401882, 1.611712598371433103 ) ) ;
#28470 = CARTESIAN_POINT ( 'NONE',  ( -0.7185039370078739607, 1.928577636452523993E-17, 1.122047243986960652 ) ) ;
#28471 = CARTESIAN_POINT ( 'NONE',  ( 0.3123359580052492146, -0.08090551181102362266, 0.000000000000000000 ) ) ;
#28472 = FACE_OUTER_BOUND ( 'NONE', #10312, .T. ) ;
#28473 = CARTESIAN_POINT ( 'NONE',  ( -0.07444174185955065859, -0.8745516835987940940, -0.1797182628040039087 ) ) ;
#28474 = DIRECTION ( 'NONE',  ( -1.000000000000000000, -6.679788269418529283E-17, 0.000000000000000000 ) ) ;
#28475 = CARTESIAN_POINT ( 'NONE',  ( -0.9412147342319837628, -0.1574803149606297803, 1.409940944774363825 ) ) ;
#28476 = CARTESIAN_POINT ( 'NONE',  ( 1.002407869896990045, -0.1264236179284866091, 0.6520669290800944484 ) ) ;
#28477 = CARTESIAN_POINT ( 'NONE',  ( 0.1574803149606300301, -0.5565944881889764995, -0.06523048226347956391 ) ) ;
#28478 = DIRECTION ( 'NONE',  ( 1.000000000000000000, 0.000000000000000000, 0.000000000000000000 ) ) ;
#28479 = DIRECTION ( 'NONE',  ( 0.000000000000000000, 0.000000000000000000, 1.000000000000000000 ) ) ;
#28480 = CARTESIAN_POINT ( 'NONE',  ( 0.8759842519685039353, -0.1574803149606299191, 1.220472440944881942 ) ) ;
#28481 = FACE_OUTER_BOUND ( 'NONE', #22214, .T. ) ;
#28483 = CARTESIAN_POINT ( 'NONE',  ( -0.5314960629921260393, 0.000000000000000000, 4.685039370078739829 ) ) ;
#28482 = CARTESIAN_POINT ( 'NONE',  ( 0.7574579170730053601, -0.1223940863669777251, 1.985778636841143641 ) ) ;
#28484 = CARTESIAN_POINT ( 'NONE',  ( 2.892866454678787531E-17, -0.6377952754830236159, 0.1574803149606299191 ) ) ;
#28485 = EDGE_CURVE ( 'NONE', #35290, #26252, #5109, .T. ) ;
#28486 = VECTOR ( 'NONE', #7643, 39.37007874015748854 ) ;
#28488 = FACE_OUTER_BOUND ( 'NONE', #39486, .T. ) ;
#28487 = CARTESIAN_POINT ( 'NONE',  ( 1.054774247047244540, -0.07405724077823318263, 0.7283464566391492090 ) ) ;
#28489 = CARTESIAN_POINT ( 'NONE',  ( -0.8759842519685039353, -0.1574803149606299191, 0.3838582676090082635 ) ) ;
#28490 = PLANE ( 'NONE',  #16875 ) ;
#28491 = ( REPRESENTATION_RELATIONSHIP ('NONE','NONE', #9609, #17291 ) REPRESENTATION_RELATIONSHIP_WITH_TRANSFORMATION ( #45345 )SHAPE_REPRESENTATION_RELATIONSHIP( ) ) ;
#28492 = CARTESIAN_POINT ( 'NONE',  ( 1.033464566929134687, 0.06523048226347956391, 1.744586614173228467 ) ) ;
#28493 = CIRCLE ( 'NONE', #45279, 0.09842519685039310962 ) ;
#28495 = PLANE ( 'NONE',  #19194 ) ;
#28494 = CIRCLE ( 'NONE', #11665, 0.02900000000000070230 ) ;
#28496 = CARTESIAN_POINT ( 'NONE',  ( 0.9500414927467378812, 0.1787899950787401604, 1.053149606245450176 ) ) ;
#28497 = VERTEX_POINT ( 'NONE', #34144 ) ;
#28498 = ADVANCED_FACE ( 'NONE', ( #23104 ), #36681, .T. ) ;
#28499 = CARTESIAN_POINT ( 'NONE',  ( -1.033464566929133799, 0.000000000000000000, 1.820866141732283561 ) ) ;
#28500 = CARTESIAN_POINT ( 'NONE',  ( -0.8107537697050254399, 0.1574803149606300301, 0.5339566929133854334 ) ) ;
#28501 = CARTESIAN_POINT ( 'NONE',  ( -0.1797182628040039365, 0.1170821746689230392, 0.000000000000000000 ) ) ;
#28502 = CARTESIAN_POINT ( 'NONE',  ( 0.1787899950787401882, -1.009350393647023614, -2.189545951927503898E-17 ) ) ;
#28503 = CARTESIAN_POINT ( 'NONE',  ( 0.1113553986120547346, -1.587598425196850460, 0.1113553986120547346 ) ) ;
#28504 = CARTESIAN_POINT ( 'NONE',  ( 0.8107537697050254399, 0.1574803149606300301, 1.242618110236220819 ) ) ;
#28505 = CARTESIAN_POINT ( 'NONE',  ( -1.002407869896990045, -0.1264236179284866091, 0.09596456687537027741 ) ) ;
#28506 = ORIENTED_EDGE ( 'NONE', *, *, #17151, .T. ) ;
#28507 = CARTESIAN_POINT ( 'NONE',  ( -0.8759842519685039353, -0.1574803149606299191, 0.8169291337507401662 ) ) ;
#28508 = ORIENTED_EDGE ( 'NONE', *, *, #25046, .F. ) ;
#28509 = CARTESIAN_POINT ( 'NONE',  ( -0.8019270111902716547, -0.1787899950787401604, 1.983267716481668108 ) ) ;
#28510 = CARTESIAN_POINT ( 'NONE',  ( -0.7495606340400177148, -0.1264236179284866091, 1.070374015694267600 ) ) ;
#28511 = CARTESIAN_POINT ( 'NONE',  ( -0.9500414927467378812, 0.1787899950787401604, 0.2706692912848194243 ) ) ;
#28512 = FACE_OUTER_BOUND ( 'NONE', #10718, .T. ) ;
#28513 = CARTESIAN_POINT ( 'NONE',  ( -0.8759842519685039353, -0.1787899950787401882, 1.906988188922614125 ) ) ;
#28514 = CARTESIAN_POINT ( 'NONE',  ( -0.1377952755905511861, 0.1564960629921283985, -0.7066929133858274037 ) ) ;
#28515 = CARTESIAN_POINT ( 'NONE',  ( -0.9873396505805591694, 0.1113553986120547346, 1.865157480314960647 ) ) ;
#28516 = CARTESIAN_POINT ( 'NONE',  ( 0.2559055118110236116, 0.1477471161312045311, -0.1122047244094488277 ) ) ;
#28517 = CARTESIAN_POINT ( 'NONE',  ( 0.1787899950787401604, -0.1959901099615224129, 0.07405724077823318263 ) ) ;
#28518 = CARTESIAN_POINT ( 'NONE',  ( -0.1699099310998980483, -0.09842519685039370636, 0.02539414388011468349 ) ) ;
#28519 = DIRECTION ( 'NONE',  ( 0.000000000000000000, 0.000000000000000000, 1.000000000000000000 ) ) ;
#28520 = CARTESIAN_POINT ( 'NONE',  ( 0.8107537697050254399, -0.1574803149606297803, 1.050688976270426567 ) ) ;
#28521 = VECTOR ( 'NONE', #31947, 39.37007874015748143 ) ;
#28522 = CARTESIAN_POINT ( 'NONE',  ( -1.054774247047244540, 0.07405724077823318263, 0.2214566928596220785 ) ) ;
#28523 = ( BOUNDED_CURVE ( )  B_SPLINE_CURVE ( 2, ( #28930, #25307, #24588, #24820, #20745, #25058, #17629, #3238, #43492 ),
 .UNSPECIFIED., .F., .T. ) 
 B_SPLINE_CURVE_WITH_KNOTS ( ( 3, 2, 2, 2, 3 ),
 ( 0.2000000000000000111, 0.2025000000000000133, 0.2049999999999999878, 0.2074999999999999900, 0.2099999999999999922 ),
 .UNSPECIFIED. ) 
 CURVE ( )  GEOMETRIC_REPRESENTATION_ITEM ( )  RATIONAL_B_SPLINE_CURVE ( ( 1.000000000000000000, 0.9238795325112849621, 1.000000000000000000, 0.9238795325112869605, 1.000000000000000000, 0.9238795325112869605, 1.000000000000000000, 0.9238795325112869605, 1.000000000000000000 ) ) 
 REPRESENTATION_ITEM ( '' )  ) ;
#28524 = ORIENTED_EDGE ( 'NONE', *, *, #1900, .F. ) ;
#28525 = VERTEX_POINT ( 'NONE', #30333 ) ;
#28526 = AXIS2_PLACEMENT_3D ( 'NONE', #5456, #34718, #26586 ) ;
#28527 = AXIS2_PLACEMENT_3D ( 'NONE', #36956, #37411, #25489 ) ;
#28528 = CARTESIAN_POINT ( 'NONE',  ( 0.1787899950787401882, -1.127460629867496067, -2.189545951927503898E-17 ) ) ;
#28529 = CARTESIAN_POINT ( 'NONE',  ( 0.1787899950787401604, -1.356299212544662014, -0.07405724077823318263 ) ) ;
#28530 = DIRECTION ( 'NONE',  ( -0.000000000000000000, 0.2126700594527843047, -0.9771240687918547607 ) ) ;
#28531 = CARTESIAN_POINT ( 'NONE',  ( 0.07444174185955046430, -0.6038823922602111205, -0.1797182628040039087 ) ) ;
#28532 = DIRECTION ( 'NONE',  ( 0.000000000000000000, 0.000000000000000000, -1.000000000000000000 ) ) ;
#28533 = CARTESIAN_POINT ( 'NONE',  ( -1.033464566929134687, 0.06523048226347956391, 0.9867125983176702197 ) ) ;
#28534 = AXIS2_PLACEMENT_3D ( 'NONE', #40166, #39937, #7125 ) ;
#28535 = CARTESIAN_POINT ( 'NONE',  ( -0.8107537697050253289, -0.1574803149606297803, 0.7455708661417325134 ) ) ;
#28536 = CARTESIAN_POINT ( 'NONE',  ( 0.1574803149606299191, -0.1259842519685039353, -1.928577636452523993E-17 ) ) ;
#28537 = CARTESIAN_POINT ( 'NONE',  ( 0.7646288533564489232, 0.1113553986120547346, 1.747047243986960652 ) ) ;
#28538 = ORIENTED_EDGE ( 'NONE', *, *, #33573, .F. ) ;
#28539 = PLANE ( 'NONE',  #41364 ) ;
#28540 = CARTESIAN_POINT ( 'NONE',  ( 0.9412147342319837628, -0.1574803149606297803, 0.8292322834645677876 ) ) ;
#28541 = CARTESIAN_POINT ( 'NONE',  ( 0.1219373188186398949, -0.2250936884182059838, -0.02739586109245262593 ) ) ;
#28542 = CARTESIAN_POINT ( 'NONE',  ( -1.033464566929134687, -0.06523048226347956391, 1.611712598317669221 ) ) ;
#28543 = ( BOUNDED_CURVE ( )  B_SPLINE_CURVE ( 2, ( #42423, #42884, #2648, #39306, #10340, #31685, #6241, #31445, #6480 ),
 .UNSPECIFIED., .F., .T. ) 
 B_SPLINE_CURVE_WITH_KNOTS ( ( 3, 2, 2, 2, 3 ),
 ( 0.3099999999999999978, 0.3125000000000000000, 0.3150000000000000022, 0.3175000000000000044, 0.3200000000000000067 ),
 .UNSPECIFIED. ) 
 CURVE ( )  GEOMETRIC_REPRESENTATION_ITEM ( )  RATIONAL_B_SPLINE_CURVE ( ( 1.000000000000000000, 0.9238795325112869605, 1.000000000000000000, 0.9238795325112869605, 1.000000000000000000, 0.9238795325112869605, 1.000000000000000000, 0.9238795325112869605, 1.000000000000000000 ) ) 
 REPRESENTATION_ITEM ( '' )  ) ;
#28544 = ADVANCED_FACE ( 'NONE', ( #23576 ), #44879, .T. ) ;
#28546 = SURFACE_SIDE_STYLE ('',( #31663 ) ) ;
#28545 = DIRECTION ( 'NONE',  ( 0.000000000000000000, -0.9771240687918547607, -0.2126700594527842492 ) ) ;
#28547 = CARTESIAN_POINT ( 'NONE',  ( 1.033464566929134687, -0.06523048226347956391, 0.1550196849318430659 ) ) ;
#28548 = EDGE_LOOP ( 'NONE', ( #4792, #43689, #37925, #4423, #3886 ) ) ;
#28549 = EDGE_CURVE ( 'NONE', #27712, #31223, #37412, .T. ) ;
#28550 = FACE_OUTER_BOUND ( 'NONE', #25506, .T. ) ;
#28551 = CARTESIAN_POINT ( 'NONE',  ( -0.06523048226347956391, -1.506397637687749702, 0.1574803149606297803 ) ) ;
#28552 = CARTESIAN_POINT ( 'NONE',  ( 3.284318927891251994E-17, -0.5467519684501732646, 0.1787899950787401882 ) ) ;
#28553 = CARTESIAN_POINT ( 'NONE',  ( 0.8107537697050253289, -0.1574803149606297803, 0.9325787400499522262 ) ) ;
#28554 = FACE_OUTER_BOUND ( 'NONE', #223, .T. ) ;
#28555 = VECTOR ( 'NONE', #24306, 39.37007874015748143 ) ;
#28556 = CARTESIAN_POINT ( 'NONE',  ( -0.6971942568897637749, 2.189545951927499583E-17, 0.4355314960092284138 ) ) ;
#28557 = ORIENTED_EDGE ( 'NONE', *, *, #25988, .F. ) ;
#28558 = CARTESIAN_POINT ( 'NONE',  ( -0.7495606340400177148, 0.1264236179284866091, 1.380413385773007873 ) ) ;
#28559 = CARTESIAN_POINT ( 'NONE',  ( 1.054774247047244540, -0.07405724077823318263, 1.520669291284818758 ) ) ;
#28560 = ORIENTED_EDGE ( 'NONE', *, *, #378, .T. ) ;
#28561 = DIRECTION ( 'NONE',  ( 0.000000000000000000, 0.000000000000000000, -1.000000000000000000 ) ) ;
#28562 = CARTESIAN_POINT ( 'NONE',  ( -1.002407869896990045, 0.1264236179284866091, 0.6619094487651338010 ) ) ;
#28563 = AXIS2_PLACEMENT_3D ( 'NONE', #16972, #2341, #31379 ) ;
#28564 = CARTESIAN_POINT ( 'NONE',  ( 0.6971942568897626646, 0.07405724077823318263, 0.2017716534895435399 ) ) ;
#28565 = CARTESIAN_POINT ( 'NONE',  ( -0.8107537697050254399, -0.1574803149606297803, 1.680610236112946465 ) ) ;
#28566 = CARTESIAN_POINT ( 'NONE',  ( 1.054774247047244096, 0.000000000000000000, 0.7357283464029290565 ) ) ;
#28567 = CARTESIAN_POINT ( 'NONE',  ( -1.002407869896990045, 0.1264236179284866091, 0.6963582676627716461 ) ) ;
#28568 = CARTESIAN_POINT ( 'NONE',  ( 0.1675084398155860799, -0.08956740676346343355, 0.1887210895736453897 ) ) ;
#28569 = CARTESIAN_POINT ( 'NONE',  ( 0.9873396505805591694, 0.1113553986120547346, 1.067913385719243990 ) ) ;
#28570 = CARTESIAN_POINT ( 'NONE',  ( 2.892866454678787531E-17, -0.1653543306011344416, 0.1574803149606299191 ) ) ;
#28571 = CARTESIAN_POINT ( 'NONE',  ( -0.8759842519685039353, -0.1787899950787401882, 1.473917322780881722 ) ) ;
#28572 = CARTESIAN_POINT ( 'NONE',  ( 0.2759478392031617933, -0.5708661417322835607, 1.713085361781125915 ) ) ;
#28573 = CARTESIAN_POINT ( 'NONE',  ( -1.033464566929133799, 0.000000000000000000, 1.466535433070866201 ) ) ;
#28574 = AXIS2_PLACEMENT_3D ( 'NONE', #26174, #16042, #11318 ) ;
#28575 = CARTESIAN_POINT ( 'NONE',  ( -0.8107537697050253289, -0.1574803149606297803, 0.3912401574803148763 ) ) ;
#28576 = CARTESIAN_POINT ( 'NONE',  ( 1.054774247047244096, 0.000000000000000000, 1.365649606245448844 ) ) ;
#28577 = CARTESIAN_POINT ( 'NONE',  ( -0.1674288283605931127, -0.09851383564138858906, -0.05723794432179189068 ) ) ;
#28578 = EDGE_LOOP ( 'NONE', ( #6702, #11746, #18108, #21352 ) ) ;
#28579 = CARTESIAN_POINT ( 'NONE',  ( -0.7185039370078746268, -0.06523048226347956391, 0.6225393700787400508 ) ) ;
#28580 = EDGE_CURVE ( 'NONE', #28431, #32335, #30557, .T. ) ;
#28581 = CARTESIAN_POINT ( 'NONE',  ( -0.1787899950787401604, -1.711738141457585627, -0.07405724077823318263 ) ) ;
#28582 = ORIENTED_EDGE ( 'NONE', *, *, #21973, .F. ) ;
#28583 = CARTESIAN_POINT ( 'NONE',  ( 1.033464566929133799, 0.000000000000000000, 0.4035433070866141780 ) ) ;
#28584 = EDGE_LOOP ( 'NONE', ( #38310, #30833, #13558, #14594 ) ) ;
#28585 = ( GEOMETRIC_REPRESENTATION_CONTEXT ( 3 ) GLOBAL_UNCERTAINTY_ASSIGNED_CONTEXT ( ( #4897 ) ) GLOBAL_UNIT_ASSIGNED_CONTEXT ( ( #37648, #11794, #34311 ) ) REPRESENTATION_CONTEXT ( 'NONE', 'WORKASPACE' ) ) ;
#28586 = CARTESIAN_POINT ( 'NONE',  ( -0.9873396505805591694, -0.1113553986120547346, 1.146653543307086798 ) ) ;
#28587 = CARTESIAN_POINT ( 'NONE',  ( 0.1264236179284866091, -0.2662401574265516047, 0.1264236179284866091 ) ) ;
#28588 = CARTESIAN_POINT ( 'NONE',  ( 0.1787899950787401604, -0.9232283464029299447, -0.07405724077823318263 ) ) ;
#28589 = VECTOR ( 'NONE', #19004, 39.37007874015748143 ) ;
#28590 = CARTESIAN_POINT ( 'NONE',  ( -0.2471902767489406183, -0.09658829859166317977, -0.02317992046427616928 ) ) ;
#28591 = DIRECTION ( 'NONE',  ( 0.000000000000000000, 0.000000000000000000, -1.000000000000000000 ) ) ;
#28592 = LENGTH_MEASURE_WITH_UNIT ( LENGTH_MEASURE( 0.02539999999999999897 ), #29073 ) ;
#28593 = CARTESIAN_POINT ( 'NONE',  ( 0.7495606340400177148, 0.1264236179284866091, 0.2731299212060791515 ) ) ;
#28594 = EDGE_CURVE ( 'NONE', #46609, #43211, #37477, .T. ) ;
#28595 = AXIS2_PLACEMENT_3D ( 'NONE', #3804, #7404, #47429 ) ;
#28596 = CIRCLE ( 'NONE', #36245, 0.3100393700787401619 ) ;
#28597 = CARTESIAN_POINT ( 'NONE',  ( 3.284318927891251994E-17, -0.1640019209851442950, 0.1787899950787401882 ) ) ;
#28598 = CARTESIAN_POINT ( 'NONE',  ( 0.1787899950787401604, 0.09055118115612580121, 0.07405724077823318263 ) ) ;
#28599 = ITEM_DEFINED_TRANSFORMATION ( 'NONE', 'NONE', #20143,  #20860 ) ;
#28600 = CARTESIAN_POINT ( 'NONE',  ( -0.8759842519685039353, 0.000000000000000000, 0.000000000000000000 ) ) ;
#28601 = CARTESIAN_POINT ( 'NONE',  ( -0.7185039370078746268, -0.06523048226347956391, 1.685531496062991019 ) ) ;
#28602 = CARTESIAN_POINT ( 'NONE',  ( 0.6971942568897637749, 2.189545951927499583E-17, 0.5930118109698583329 ) ) ;
#28603 = CARTESIAN_POINT ( 'NONE',  ( -0.6971942568897648851, 0.07405724077823318263, 0.9104330708123777871 ) ) ;
#28604 = EDGE_CURVE ( 'NONE', #30249, #27223, #45818, .T. ) ;
#28605 = LENGTH_MEASURE_WITH_UNIT ( LENGTH_MEASURE( 0.02539999999999999897 ), #3871 ) ;
#28607 = CARTESIAN_POINT ( 'NONE',  ( -0.8844078933030434797, -0.1745978227235963076, 1.988329488380941479 ) ) ;
#28606 = CARTESIAN_POINT ( 'NONE',  ( -0.1797182628040039087, -1.775142234779896411, -0.07444174185955065859 ) ) ;
#28608 = DIRECTION ( 'NONE',  ( -0.8191520442889980158, 0.000000000000000000, -0.5735764363510372776 ) ) ;
#28609 = CARTESIAN_POINT ( 'NONE',  ( 0.6971942568897648851, -0.07405724077823297447, 1.624015747977732849 ) ) ;
#28611 = CARTESIAN_POINT ( 'NONE',  ( 0.2559055118110236116, 0.000000000000000000, -0.3149606299212598381 ) ) ;
#28610 = CARTESIAN_POINT ( 'NONE',  ( 1.002407869896990045, -0.1264236179284866091, 1.946358267662771757 ) ) ;
#28612 = CARTESIAN_POINT ( 'NONE',  ( 0.7495606340400177148, -0.1264236179284866091, 0.5191929133320630774 ) ) ;
#28613 = ORIENTED_EDGE ( 'NONE', *, *, #11714, .T. ) ;
#28614 = CARTESIAN_POINT ( 'NONE',  ( -0.1594432092296970138, -0.09246610911301904323, -0.1933784749626324961 ) ) ;
#28615 = EDGE_CURVE ( 'NONE', #31906, #21602, #23097, .T. ) ;
#28616 = DIRECTION ( 'NONE',  ( 0.000000000000000000, 0.000000000000000000, 1.000000000000000000 ) ) ;
#28617 = CARTESIAN_POINT ( 'NONE',  ( -0.1787899950787401604, -0.1653543306548978520, -0.07405724077823318263 ) ) ;
#28618 = CARTESIAN_POINT ( 'NONE',  ( 1.002407869896990045, 0.1264236179284866091, 0.6569881889226141247 ) ) ;
#28619 = CARTESIAN_POINT ( 'NONE',  ( 0.1787899950787401604, -1.120078740103715997, -0.07405724077823318263 ) ) ;
#28620 = CARTESIAN_POINT ( 'NONE',  ( 1.054774247047244540, -0.07405724077823318263, 0.06397637789899228433 ) ) ;
#28621 = PLANE ( 'NONE',  #1702 ) ;
#28622 = CARTESIAN_POINT ( 'NONE',  ( 1.054774247047244540, -0.07405724077823318263, 0.5708661416785200116 ) ) ;
#28623 = EDGE_CURVE ( 'NONE', #8606, #24988, #38957, .T. ) ;
#28624 = CARTESIAN_POINT ( 'NONE',  ( -0.8759842519685039353, -0.1574803149606299191, 0.9842519685039370358 ) ) ;
#28625 = CARTESIAN_POINT ( 'NONE',  ( -0.8759842519685039353, -0.1787899950787401882, 1.390255905458047447 ) ) ;
#28626 = ORIENTED_EDGE ( 'NONE', *, *, #42258, .T. ) ;
#28627 = CARTESIAN_POINT ( 'NONE',  ( -0.3070839322311867403, -0.04408052624949946457, -1.037775876589189794 ) ) ;
#28628 = CARTESIAN_POINT ( 'NONE',  ( 0.7495606340400177148, 0.1264236179284866091, 1.144192913332062966 ) ) ;
#28629 = CARTESIAN_POINT ( 'NONE',  ( 0.8019270111902717657, 0.1787899950787401604, 1.766732283410803461 ) ) ;
#28630 = CARTESIAN_POINT ( 'NONE',  ( -1.033464566929134687, 0.06523048226347956391, 1.350885826771654363 ) ) ;
#28631 = CARTESIAN_POINT ( 'NONE',  ( -1.002407869896990045, 0.1264236179284866091, 0.9719488188438739629 ) ) ;
#28632 = VECTOR ( 'NONE', #22031, 39.37007874015748854 ) ;
#28633 = CARTESIAN_POINT ( 'NONE',  ( -0.9873396505805591694, 0.1113553986120547346, 0.5167322833570401341 ) ) ;
#28634 = CARTESIAN_POINT ( 'NONE',  ( -0.7067031875023493948, 0.05524205133751965147, 0.03937007874015842346 ) ) ;
#28635 = CARTESIAN_POINT ( 'NONE',  ( 0.9500414927467377701, -0.1787899950787401604, 0.2559055117572600624 ) ) ;
#28636 = CARTESIAN_POINT ( 'NONE',  ( -0.6971942568897626646, 0.07405724077823318263, 0.1574803149068664809 ) ) ;
#28637 = CARTESIAN_POINT ( 'NONE',  ( -0.6971942568897626646, 0.07405724077823318263, 0.5511811023084406402 ) ) ;
#28638 = CARTESIAN_POINT ( 'NONE',  ( 0.7185039370078746268, -0.06523048226347956391, 1.557578740049953225 ) ) ;
#28639 = ORIENTED_EDGE ( 'NONE', *, *, #16994, .F. ) ;
#28640 = CARTESIAN_POINT ( 'NONE',  ( 0.1264236179284866091, 0.01919291343959031448, -0.1264236179284866091 ) ) ;
#28641 = ORIENTED_EDGE ( 'NONE', *, *, #17160, .F. ) ;
#28642 = CARTESIAN_POINT ( 'NONE',  ( 1.054774247047244540, 0.07405724077823318263, 0.8169291338045038264 ) ) ;
#28643 = CARTESIAN_POINT ( 'NONE',  ( -1.054774247047244540, 0.07405724077823318263, 1.796259842465920853 ) ) ;
#28644 = VERTEX_POINT ( 'NONE', #2918 ) ;
#28645 = DIRECTION ( 'NONE',  ( -1.000000000000000000, 0.000000000000000000, 0.000000000000000000 ) ) ;
#28646 = LINE ( 'NONE', #25516, #33639 ) ;
#28647 = CARTESIAN_POINT ( 'NONE',  ( -0.1264236179284866091, -1.320497983977269918, -0.1264236179284866091 ) ) ;
#28648 = EDGE_LOOP ( 'NONE', ( #16418, #24777, #43626, #28524 ) ) ;
#28649 = CARTESIAN_POINT ( 'NONE',  ( 0.1264236179284866091, -0.2613188975840319284, 0.1264236179284866091 ) ) ;
#28650 = CYLINDRICAL_SURFACE ( 'NONE', #33123, 0.02900000000000001882 ) ;
#28651 = ORIENTED_EDGE ( 'NONE', *, *, #1954, .F. ) ;
#28652 = EDGE_CURVE ( 'NONE', #42873, #29582, #22131, .T. ) ;
#28653 = CARTESIAN_POINT ( 'NONE',  ( 0.008396861977716250230, -0.1523390671600990398, -0.01173154688214765075 ) ) ;
#28654 = CARTESIAN_POINT ( 'NONE',  ( -0.2471922931865199735, -0.07794380098772846210, 0.07736948232528978453 ) ) ;
#28655 = ADVANCED_FACE ( 'NONE', ( #2458 ), #46073, .T. ) ;
#28656 = ADVANCED_FACE ( 'NONE', ( #16846 ), #32103, .F. ) ;
#28657 = CARTESIAN_POINT ( 'NONE',  ( -0.1787899950787401604, -1.420275590497418250, 0.07405724077823318263 ) ) ;
#28658 = CARTESIAN_POINT ( 'NONE',  ( -0.1787899950787401604, -0.7903543306548983516, 0.07405724077823318263 ) ) ;
#28659 = CARTESIAN_POINT ( 'NONE',  ( -0.7495606340400177148, 0.1264236179284866091, 0.4749015747493858242 ) ) ;
#28660 = CARTESIAN_POINT ( 'NONE',  ( -0.06699593397071766654, 0.2568141117498029535, -0.04769437235512034856 ) ) ;
#28661 = CARTESIAN_POINT ( 'NONE',  ( 0.8019270111902716547, -0.1787899950787401604, 1.505905511757261062 ) ) ;
#28662 = CONICAL_SURFACE ( 'NONE', #7971, 0.1574803149606299191, 1.047197551196598297 ) ;
#28663 = CARTESIAN_POINT ( 'NONE',  ( -1.033464566929134687, 0.06523048226347956391, 0.5930118109160945616 ) ) ;
#28664 = CARTESIAN_POINT ( 'NONE',  ( 0.9412147342319837628, 0.1574803149606300301, 1.710137795275592065 ) ) ;
#28665 = CARTESIAN_POINT ( 'NONE',  ( -0.01411529459472660869, 0.1299212598425194265, 0.1732737445343259797 ) ) ;
#28667 = CARTESIAN_POINT ( 'NONE',  ( -0.7185039370078746268, -0.06523048226347956391, 1.094980314960629419 ) ) ;
#28666 = CARTESIAN_POINT ( 'NONE',  ( 0.1563802477479413477, 0.02735756446292999730, 0.1403846664728047311 ) ) ;
#28668 = CARTESIAN_POINT ( 'NONE',  ( 0.8759842519685039353, -0.1574803149606299191, 0.7775590550105826448 ) ) ;
#28669 = CARTESIAN_POINT ( 'NONE',  ( -0.8759842519685039353, -0.1574803149606299191, 1.722440944774362270 ) ) ;
#28670 = CARTESIAN_POINT ( 'NONE',  ( 1.054774247047244096, 0.000000000000000000, 0.1008858267178899676 ) ) ;
#28671 = CARTESIAN_POINT ( 'NONE',  ( 0.7073262291835020754, -0.03557810427923590452, 0.03937137958850374375 ) ) ;
#28673 = CARTESIAN_POINT ( 'NONE',  ( 0.7185039370078739607, 1.928577636452523993E-17, 0.2559055117034968463 ) ) ;
#28672 = CARTESIAN_POINT ( 'NONE',  ( 0.8019270111902716547, 0.1787899950787401604, 1.215551181048599272 ) ) ;
#28674 = ADVANCED_FACE ( 'NONE', ( #28362 ), #13966, .T. ) ;
#28675 = CARTESIAN_POINT ( 'NONE',  ( -0.8107537697050254399, -0.1574803149606297803, 1.916830708553890483 ) ) ;
#28676 = CARTESIAN_POINT ( 'NONE',  ( 0.9412147342319837628, -0.1574803149606297803, 0.4650590550105836440 ) ) ;
#28677 = ORIENTED_EDGE ( 'NONE', *, *, #39158, .T. ) ;
#28678 = AXIS2_PLACEMENT_3D ( 'NONE', #9362, #26878, #12737 ) ;
#28679 = ( LENGTH_UNIT ( ) NAMED_UNIT ( * ) SI_UNIT ( $, .METRE. ) ) ;
#28680 = CARTESIAN_POINT ( 'NONE',  ( 0.1574803149606300301, -1.024114173120818982, 0.06523048226347956391 ) ) ;
#28681 = CARTESIAN_POINT ( 'NONE',  ( -0.9412147342319837628, 0.1574803149606300301, 0.3617125983176697201 ) ) ;
#28682 = VERTEX_POINT ( 'NONE', #24989 ) ;
#28683 = CARTESIAN_POINT ( 'NONE',  ( 0.9500414927467378812, 0.1787899950787401604, 1.486220472387181690 ) ) ;
#28685 = DIRECTION ( 'NONE',  ( -1.000000000000000000, 0.000000000000000000, 0.000000000000000000 ) ) ;
#28684 = CARTESIAN_POINT ( 'NONE',  ( -0.9873396505805591694, 0.1113553986120547346, 1.628937007874015963 ) ) ;
#28686 = CARTESIAN_POINT ( 'NONE',  ( -0.07405724077823318263, -0.007874015694267993623, -0.1787899950787401604 ) ) ;
#28687 = ORIENTED_EDGE ( 'NONE', *, *, #26458, .T. ) ;
#28688 = CARTESIAN_POINT ( 'NONE',  ( 0.1587185860253795822, -0.04237460976005667790, -0.1404529029258574369 ) ) ;
#28689 = EDGE_LOOP ( 'NONE', ( #26399, #4546, #40524, #45490 ) ) ;
#28690 = CARTESIAN_POINT ( 'NONE',  ( 1.033464566929134687, -0.06523048226347956391, 1.296751968396409049 ) ) ;
#28691 = CARTESIAN_POINT ( 'NONE',  ( 0.1235961452251413406, -0.09842519685039370636, -0.2140748031496062798 ) ) ;
#28692 = CARTESIAN_POINT ( 'NONE',  ( 0.8759842519685039353, 0.1787899950787401882, 0.5880905511273386566 ) ) ;
#28693 = VERTEX_POINT ( 'NONE', #9675 ) ;
#28694 = CARTESIAN_POINT ( 'NONE',  ( -0.8759842519685039353, 0.1787899950787401882, 1.370570866087968520 ) ) ;
#28695 = CARTESIAN_POINT ( 'NONE',  ( 0.1574803149606299191, 0.1200787402650072971, -1.928577636452523993E-17 ) ) ;
#28696 = CARTESIAN_POINT ( 'NONE',  ( -0.9500414927467378812, -0.1787899950787401604, 1.082677165300567346 ) ) ;
#28697 = CARTESIAN_POINT ( 'NONE',  ( -0.9873396505805591694, 0.1113553986120547346, 0.1722440944881890035 ) ) ;
#28698 = ORIENTED_EDGE ( 'NONE', *, *, #29850, .T. ) ;
#28699 = CARTESIAN_POINT ( 'NONE',  ( -0.9500414927467377701, 0.1787899950787401604, 1.131889763725763887 ) ) ;
#28700 = CARTESIAN_POINT ( 'NONE',  ( -0.6971942568897637749, 2.189545951927499583E-17, 0.7947834645131652831 ) ) ;
#28701 = AXIS2_PLACEMENT_3D ( 'NONE', #33724, #11417, #831 ) ;
#28702 = CARTESIAN_POINT ( 'NONE',  ( -0.1264236179284866091, -0.7693168816150650624, -0.1264236179284866091 ) ) ;
#28703 = ORIENTED_EDGE ( 'NONE', *, *, #47180, .F. ) ;
#28704 = CARTESIAN_POINT ( 'NONE',  ( -0.02028039986305122527, -0.08956190947767678212, 0.1525088234432795398 ) ) ;
#28705 = CARTESIAN_POINT ( 'NONE',  ( -0.1184675242425147629, -0.09842519685039370636, 2.185526306663016616 ) ) ;
#28706 = EDGE_LOOP ( 'NONE', ( #36425, #42843, #22718, #31527 ) ) ;
#28707 = VECTOR ( 'NONE', #30300, 39.37007874015748854 ) ;
#28708 = VERTEX_POINT ( 'NONE', #16624 ) ;
#28709 = DIRECTION ( 'NONE',  ( -0.000000000000000000, -0.2432573283306646017, 0.9699617890481188054 ) ) ;
#28710 = ADVANCED_FACE ( 'NONE', ( #9442 ), #24291, .F. ) ;
#28711 = DIRECTION ( 'NONE',  ( -3.469446951953614583E-15, -1.000000000000000000, -1.751623080406021339E-46 ) ) ;
#28712 = CARTESIAN_POINT ( 'NONE',  ( -1.054774247047244540, 0.07405724077823318263, 0.5757874015210394658 ) ) ;
#28713 = DIRECTION ( 'NONE',  ( 0.000000000000000000, 0.000000000000000000, -1.000000000000000000 ) ) ;
#28714 = EDGE_CURVE ( 'NONE', #3668, #21986, #31723, .T. ) ;
#28715 = ORIENTED_EDGE ( 'NONE', *, *, #12960, .T. ) ;
#28716 = EDGE_CURVE ( 'NONE', #28803, #10456, #39585, .T. ) ;
#28717 = EDGE_CURVE ( 'NONE', #42931, #27211, #28131, .T. ) ;
#28718 = CARTESIAN_POINT ( 'NONE',  ( 0.001099666138475116151, -0.02328811444560369148, -0.1377843663819193765 ) ) ;
#28719 = PLANE ( 'NONE',  #38660 ) ;
#28720 = ORIENTED_EDGE ( 'NONE', *, *, #25526, .T. ) ;
#28721 = CARTESIAN_POINT ( 'NONE',  ( 0.9412147342319837628, 0.1574803149606300301, 0.6471456692913395425 ) ) ;
#28722 = CARTESIAN_POINT ( 'NONE',  ( -0.1797182628040039365, -0.9065398725751713238, 0.000000000000000000 ) ) ;
#28723 = DIRECTION ( 'NONE',  ( -0.000000000000000000, 0.6121968903568509868, 0.7907053606985360306 ) ) ;
#28724 = CARTESIAN_POINT ( 'NONE',  ( -0.8759842519685039353, 0.1574803149606299191, 1.427165354223181248 ) ) ;
#28725 = CARTESIAN_POINT ( 'NONE',  ( 0.8019270111902717657, -0.1787899950787401604, 0.7627952755367881643 ) ) ;
#28726 = CARTESIAN_POINT ( 'NONE',  ( 0.1113553986120547346, -0.5147637795275590289, -0.1113553986120547346 ) ) ;
#28727 = CARTESIAN_POINT ( 'NONE',  ( -0.05777579460957081581, 0.1215522599344571048, -0.1483226373755269778 ) ) ;
#28728 = CARTESIAN_POINT ( 'NONE',  ( 1.033464566929133799, 0.000000000000000000, 0.1574803148531029595 ) ) ;
#28729 = CARTESIAN_POINT ( 'NONE',  ( 0.9873396505805591694, 0.1113553986120547346, 1.235236220472440971 ) ) ;
#28730 = CARTESIAN_POINT ( 'NONE',  ( 0.9050986085126093705, -0.1735205885709931173, 1.988692092061036698 ) ) ;
#28731 = DIRECTION ( 'NONE',  ( -1.000000000000000000, 0.000000000000000000, 0.000000000000000000 ) ) ;
#28733 = DIRECTION ( 'NONE',  ( -1.000000000000000000, 0.000000000000000000, 0.000000000000000000 ) ) ;
#28732 = CARTESIAN_POINT ( 'NONE',  ( 0.6971942568897648851, -0.07405724077823297447, 0.6742125983714336579 ) ) ;
#28734 = CARTESIAN_POINT ( 'NONE',  ( -1.033464566929134687, 0.06523048226347956391, 0.6815944881889761664 ) ) ;
#28735 = AXIS2_PLACEMENT_3D ( 'NONE', #21533, #36170, #3325 ) ;
#28737 = VECTOR ( 'NONE', #11597, 39.37007874015748143 ) ;
#28736 = CARTESIAN_POINT ( 'NONE',  ( -0.07405724077823318263, -0.6624015747493856576, 0.1787899950787401604 ) ) ;
#28738 = CARTESIAN_POINT ( 'NONE',  ( 0.9873396505805591694, 0.1113553986120547346, 1.550196850393700920 ) ) ;
#28739 = EDGE_LOOP ( 'NONE', ( #5672, #12613, #40204, #36450 ) ) ;
#28740 = CARTESIAN_POINT ( 'NONE',  ( -0.7185039370078739607, 1.928577636452523993E-17, 1.171259842519684957 ) ) ;
#28741 = AXIS2_PLACEMENT_3D ( 'NONE', #7673, #26627, #7915 ) ;
#28742 = CARTESIAN_POINT ( 'NONE',  ( 0.0005737749932732162661, 0.1108949133173907642, -0.08352002191776017326 ) ) ;
#28743 = CARTESIAN_POINT ( 'NONE',  ( 0.7495606340400177148, 0.1264236179284866091, 0.9817913385289134265 ) ) ;
#28744 = FACE_OUTER_BOUND ( 'NONE', #16656, .T. ) ;
#28745 = DIRECTION ( 'NONE',  ( 1.000000000000000000, 0.000000000000000000, 0.000000000000000000 ) ) ;
#28746 = CARTESIAN_POINT ( 'NONE',  ( -0.1797182628040039365, 0.07771209592876555938, 0.000000000000000000 ) ) ;
#28747 = CARTESIAN_POINT ( 'NONE',  ( -0.1787899950787401604, -1.149606299158835387, -0.07405724077823318263 ) ) ;
#28748 = CARTESIAN_POINT ( 'NONE',  ( 0.1574803149606299191, -1.503937007874015741, -1.928577636452523993E-17 ) ) ;
#28749 = CARTESIAN_POINT ( 'NONE',  ( -0.7185039370078739607, 0.000000000000000000, -2.869337061179095023E-17 ) ) ;
#28750 = CARTESIAN_POINT ( 'NONE',  ( -1.054774247047244096, 0.000000000000000000, 0.1402559054580474474 ) ) ;
#28751 = CARTESIAN_POINT ( 'NONE',  ( -1.033464566929134687, -0.06523048226347956391, 0.8243110235145210130 ) ) ;
#28752 = ORIENTED_EDGE ( 'NONE', *, *, #35518, .T. ) ;
#28753 = LINE ( 'NONE', #32579, #40176 ) ;
#28754 = CARTESIAN_POINT ( 'NONE',  ( -1.002407869896990045, -0.1264236179284866091, 1.473917322780881722 ) ) ;
#28755 = CARTESIAN_POINT ( 'NONE',  ( 1.002407869896990045, -0.1264236179284866091, 0.8882874015210394658 ) ) ;
#28756 = CARTESIAN_POINT ( 'NONE',  ( -0.8019270111902717657, -0.1787899950787401604, 1.112204724355684959 ) ) ;
#28757 = CARTESIAN_POINT ( 'NONE',  ( -1.054774247047244540, 0.07405724077823318263, 0.3838582676627718127 ) ) ;
#28758 = CARTESIAN_POINT ( 'NONE',  ( -0.1910524284696294706, 0.07767250275969714290, -0.1751288998598694580 ) ) ;
#28759 = CARTESIAN_POINT ( 'NONE',  ( -1.002407869896990045, -0.1264236179284866091, 1.911909448765133801 ) ) ;
#28760 = CARTESIAN_POINT ( 'NONE',  ( -0.7185039370078739607, 1.928577636452523993E-17, 1.958661417322834719 ) ) ;
#28761 = CARTESIAN_POINT ( 'NONE',  ( -0.7646288533564489232, -0.1113553986120547346, 1.884842519685039353 ) ) ;
#28762 = CARTESIAN_POINT ( 'NONE',  ( 0.1787899950787401604, -0.4272893225599475042, -0.07405724077823318263 ) ) ;
#28763 = CARTESIAN_POINT ( 'NONE',  ( -0.1585347235887767658, -0.09842519685039370636, -0.08158260120612992328 ) ) ;
#28764 = CARTESIAN_POINT ( 'NONE',  ( 0.1574803149606299746, -0.4410959923581754816, -0.9673892061308019263 ) ) ;
#28765 = LINE ( 'NONE', #39724, #37942 ) ;
#28766 = CARTESIAN_POINT ( 'NONE',  ( -0.8759842519685039353, 0.1787899950787401882, 0.1894685038832444879 ) ) ;
#28767 = ADVANCED_FACE ( 'NONE', ( #9906 ), #24516, .T. ) ;
#28768 = VERTEX_POINT ( 'NONE', #14215 ) ;
#28769 = EDGE_CURVE ( 'NONE', #30794, #36569, #32447, .T. ) ;
#28770 = CARTESIAN_POINT ( 'NONE',  ( -0.6971942568897648851, -0.07405724077823297447, 1.427165354276944687 ) ) ;
#28771 = ORIENTED_EDGE ( 'NONE', *, *, #9150, .F. ) ;
#28772 = CIRCLE ( 'NONE', #8067, 0.2471922904502826812 ) ;
#28773 = EDGE_CURVE ( 'NONE', #13621, #16635, #36715, .T. ) ;
#28774 = CARTESIAN_POINT ( 'NONE',  ( 0.07405724077823318263, -1.198818897584032150, -0.1787899950787401604 ) ) ;
#28775 = CARTESIAN_POINT ( 'NONE',  ( 0.1787899950787401604, -1.400590551127339323, 0.07405724077823318263 ) ) ;
#28776 = CARTESIAN_POINT ( 'NONE',  ( -0.8107537697050254399, 0.1574803149606300301, 1.547736220364914983 ) ) ;
#28777 = SHAPE_REPRESENTATION_RELATIONSHIP ( 'NONE' , 'NONE' ,  #45408, #24384 ) ;
#28778 = CARTESIAN_POINT ( 'NONE',  ( 0.8107537697050253289, 0.1574803149606300301, 0.3764763779527559029 ) ) ;
#28779 = CARTESIAN_POINT ( 'NONE',  ( 0.000000000000000000, 0.000000000000000000, 1.181102362204724310 ) ) ;
#28780 = CARTESIAN_POINT ( 'NONE',  ( -1.033464566929133799, 0.000000000000000000, 0.9055118109160944506 ) ) ;
#28781 = CARTESIAN_POINT ( 'NONE',  ( -0.7185039370078746268, -0.06523048226347956391, 0.7800196850393692483 ) ) ;
#28782 = ORIENTED_EDGE ( 'NONE', *, *, #27805, .T. ) ;
#28783 = CARTESIAN_POINT ( 'NONE',  ( 0.9412147342319837628, 0.1574803149606300301, 1.857775590443653257 ) ) ;
#28784 = VERTEX_POINT ( 'NONE', #28853 ) ;
#28785 = DIRECTION ( 'NONE',  ( -1.000000000000000000, 0.000000000000000000, 0.000000000000000000 ) ) ;
#28786 = CARTESIAN_POINT ( 'NONE',  ( 0.7185039370078746268, -0.06523048226347956391, 0.7800196850393692483 ) ) ;
#28787 = CARTESIAN_POINT ( 'NONE',  ( 0.1657445988168603501, -0.1998015435187681099, -0.03531881253561163642 ) ) ;
#28788 = CARTESIAN_POINT ( 'NONE',  ( -0.1574803149606297803, -0.06446850393700777337, 0.06523048226347956391 ) ) ;
#28790 = LINE ( 'NONE', #17259, #42222 ) ;
#28789 = CARTESIAN_POINT ( 'NONE',  ( -0.8107537697050254399, -0.1574803149606297803, 0.4699803149606304742 ) ) ;
#28791 = CARTESIAN_POINT ( 'NONE',  ( 0.9873396505805591694, 0.1113553986120547346, 0.2411417321759374011 ) ) ;
#28792 = AXIS2_PLACEMENT_3D ( 'NONE', #30167, #29930, #403 ) ;
#28793 = ORIENTED_EDGE ( 'NONE', *, *, #8159, .F. ) ;
#28794 = DIRECTION ( 'NONE',  ( 0.000000000000000000, 0.000000000000000000, -1.000000000000000000 ) ) ;
#28795 = DIRECTION ( 'NONE',  ( 0.000000000000000000, 0.000000000000000000, -1.000000000000000000 ) ) ;
#28796 = CARTESIAN_POINT ( 'NONE',  ( 0.1113553986120547346, -1.489173228238929170, -0.1113553986120547346 ) ) ;
#28797 = CARTESIAN_POINT ( 'NONE',  ( -0.1787899950787401604, -0.6377952755367874982, -0.07405724077823318263 ) ) ;
#28798 = CARTESIAN_POINT ( 'NONE',  ( -0.1113553986120547346, -1.125000000000000000, 0.1113553986120547346 ) ) ;
#28799 = CARTESIAN_POINT ( 'NONE',  ( 0.7185039370078746268, 0.06523048226347956391, 0.9227362203649142058 ) ) ;
#28800 = DIRECTION ( 'NONE',  ( 0.000000000000000000, 0.000000000000000000, 1.000000000000000000 ) ) ;
#28801 = CARTESIAN_POINT ( 'NONE',  ( -1.054774247047244540, 0.07405724077823318263, 0.3395669290800945039 ) ) ;
#28802 = ORIENTED_EDGE ( 'NONE', *, *, #42032, .T. ) ;
#28803 = VERTEX_POINT ( 'NONE', #29098 ) ;
#28804 = CARTESIAN_POINT ( 'NONE',  ( -1.002407869896990045, -0.1264236179284866091, 1.596948818843874074 ) ) ;
#28805 = ORIENTED_EDGE ( 'NONE', *, *, #42705, .T. ) ;
#28806 = CARTESIAN_POINT ( 'NONE',  ( 0.9500414927467378812, 0.1787899950787401604, 1.530511810969859443 ) ) ;
#28807 = ORIENTED_EDGE ( 'NONE', *, *, #3268, .F. ) ;
#28808 = AXIS2_PLACEMENT_3D ( 'NONE', #5972, #31646, #39263 ) ;
#28809 = CARTESIAN_POINT ( 'NONE',  ( -0.1574803149606300301, -1.280019684931841706, -0.06523048226347956391 ) ) ;
#28810 = CARTESIAN_POINT ( 'NONE',  ( -1.054774247047244096, 0.000000000000000000, 0.7750984251430865779 ) ) ;
#28811 = CYLINDRICAL_SURFACE ( 'NONE', #39613, 0.1574803149606299191 ) ;
#28812 = CARTESIAN_POINT ( 'NONE',  ( 0.8759842519685039353, 0.1787899950787401882, 0.7455708660879684091 ) ) ;
#28813 = CARTESIAN_POINT ( 'NONE',  ( -1.054774247047244540, 0.07405724077823318263, 0.7726377952218266287 ) ) ;
#28814 = CARTESIAN_POINT ( 'NONE',  ( 0.0003553830333942847560, -0.1126092284109665720, 0.08054791328663142569 ) ) ;
#28815 = ( BOUNDED_CURVE ( )  B_SPLINE_CURVE ( 2, ( #19870, #2352, #5490, #8848, #12940, #6182, #41645, #1650, #1891 ),
 .UNSPECIFIED., .F., .F. ) 
 B_SPLINE_CURVE_WITH_KNOTS ( ( 3, 2, 2, 2, 3 ),
 ( 0.9200000000000000400, 0.9224999999999999867, 0.9250000000000000444, 0.9274999999999999911, 0.9300000000000000488 ),
 .UNSPECIFIED. ) 
 CURVE ( )  GEOMETRIC_REPRESENTATION_ITEM ( )  RATIONAL_B_SPLINE_CURVE ( ( 1.000000000000000000, 0.9238795325112869605, 1.000000000000000000, 0.9238795325112869605, 1.000000000000000000, 0.9238795325112869605, 1.000000000000000000, 0.9238795325112829637, 1.000000000000000000 ) ) 
 REPRESENTATION_ITEM ( '' )  ) ;
#28816 = CARTESIAN_POINT ( 'NONE',  ( -0.9873396505805591694, -0.1113553986120547346, 0.8710629921259842590 ) ) ;
#28817 = CARTESIAN_POINT ( 'NONE',  ( 0.06523048226347956391, -0.2810039369003468623, 0.1574803149606297803 ) ) ;
#28818 = CARTESIAN_POINT ( 'NONE',  ( -1.054774247047244540, 0.07405724077823318263, 1.446850393647023614 ) ) ;
#28819 = ORIENTED_EDGE ( 'NONE', *, *, #10584, .F. ) ;
#28820 = CARTESIAN_POINT ( 'NONE',  ( -0.9873396505805591694, -0.1113553986120547346, 0.4379921259842519676 ) ) ;
#28821 = CARTESIAN_POINT ( 'NONE',  ( 0.8019270111902716547, 0.1787899950787401604, 1.535433070812378675 ) ) ;
#28822 = CARTESIAN_POINT ( 'NONE',  ( 0.0007072645643074310616, -0.09851384404544488715, -0.1904345280194874035 ) ) ;
#28823 = CYLINDRICAL_SURFACE ( 'NONE', #5752, 0.7874015748031437667 ) ;
#28824 = ORIENTED_EDGE ( 'NONE', *, *, #34931, .F. ) ;
#28825 = ORIENTED_EDGE ( 'NONE', *, *, #34990, .T. ) ;
#28826 = EDGE_CURVE ( 'NONE', #34618, #40452, #10660, .T. ) ;
#28827 = CARTESIAN_POINT ( 'NONE',  ( -0.07405724077823318263, -1.716659401300104193, -0.1787899950787401604 ) ) ;
#28828 = ORIENTED_EDGE ( 'NONE', *, *, #11546, .T. ) ;
#28829 = CARTESIAN_POINT ( 'NONE',  ( -0.1787899950787401882, -0.6697834645131652831, 0.000000000000000000 ) ) ;
#28830 = ORIENTED_EDGE ( 'NONE', *, *, #2699, .F. ) ;
#28831 = AXIS2_PLACEMENT_3D ( 'NONE', #19753, #42004, #41770 ) ;
#28832 = ADVANCED_FACE ( 'NONE', ( #25937 ), #29059, .T. ) ;
#28833 = CARTESIAN_POINT ( 'NONE',  ( -0.8107537697050254399, -0.1574803149606297803, 1.139271653543306506 ) ) ;
#28834 = ( BOUNDED_CURVE ( )  B_SPLINE_CURVE ( 2, ( #4419, #33950, #19050, #26993, #5147, #16430, #26747, #41306, #34400 ),
 .UNSPECIFIED., .F., .T. ) 
 B_SPLINE_CURVE_WITH_KNOTS ( ( 3, 2, 2, 2, 3 ),
 ( 0.4199999999999999845, 0.4224999999999999867, 0.4249999999999999889, 0.4274999999999999911, 0.4299999999999999933 ),
 .UNSPECIFIED. ) 
 CURVE ( )  GEOMETRIC_REPRESENTATION_ITEM ( )  RATIONAL_B_SPLINE_CURVE ( ( 1.000000000000000000, 0.9238795325112869605, 1.000000000000000000, 0.9238795325112869605, 1.000000000000000000, 0.9238795325112869605, 1.000000000000000000, 0.9238795325112869605, 1.000000000000000000 ) ) 
 REPRESENTATION_ITEM ( '' )  ) ;
#28835 = CARTESIAN_POINT ( 'NONE',  ( -0.1787899950787401604, -0.9478346456155283262, -0.07405724077823318263 ) ) ;
#28836 = CYLINDRICAL_SURFACE ( 'NONE', #31064, 0.1574803149606299191 ) ;
#28837 = CARTESIAN_POINT ( 'NONE',  ( 0.8759842519685039353, 0.1787899950787401882, 1.685531496009228469 ) ) ;
#28838 = CARTESIAN_POINT ( 'NONE',  ( 1.054774247047244540, 0.07405724077823318263, 0.2608267715997796832 ) ) ;
#28839 = CARTESIAN_POINT ( 'NONE',  ( -0.07405724077823318263, -0.1024861729536482163, -0.1787899950787401604 ) ) ;
#28840 = CARTESIAN_POINT ( 'NONE',  ( -0.1787899950787401604, -0.002952755851748290004, 0.07405724077823318263 ) ) ;
#28841 = CARTESIAN_POINT ( 'NONE',  ( 0.2471922466705862576, -0.08138981793850655344, -0.07067796049199921715 ) ) ;
#28842 = CARTESIAN_POINT ( 'NONE',  ( 0.6971942568897626646, 0.07405724077823318263, 0.5511811023084406402 ) ) ;
#28843 = CARTESIAN_POINT ( 'NONE',  ( -1.054774247047244540, 0.07405724077823318263, 0.8956692912848198684 ) ) ;
#28844 = CARTESIAN_POINT ( 'NONE',  ( -0.8547977949112169904, 0.1745539855089116299, 0.03937007874015845815 ) ) ;
#28845 = CARTESIAN_POINT ( 'NONE',  ( 0.1797182628040039087, -1.711165856827140619, -0.07444174185955065859 ) ) ;
#28846 = CARTESIAN_POINT ( 'NONE',  ( 0.000000000000000000, -0.09842519685039370636, 0.000000000000000000 ) ) ;
#28847 = CARTESIAN_POINT ( 'NONE',  ( 0.8759842519685039353, 0.1787899950787401882, 1.611712598371433103 ) ) ;
#28849 = CARTESIAN_POINT ( 'NONE',  ( 0.2559055118110236116, 0.09798266946487620144, -0.3050161490475334358 ) ) ;
#28848 = CARTESIAN_POINT ( 'NONE',  ( -0.1293255151917100387, -0.09842519685039366473, 0.2107669498571209110 ) ) ;
#28850 = ORIENTED_EDGE ( 'NONE', *, *, #14473, .T. ) ;
#28851 = LINE ( 'NONE', #44069, #45169 ) ;
#28852 = CARTESIAN_POINT ( 'NONE',  ( 0.1377952755905509641, 0.000000000000000000, -0.2219368594840610276 ) ) ;
#28853 = CARTESIAN_POINT ( 'NONE',  ( 0.1574803149606299191, 0.3740157480314960647, 0.9783464566929134243 ) ) ;
#28855 = CARTESIAN_POINT ( 'NONE',  ( 0.07405724077823318263, -0.09645669285962235606, -0.1787899950787401604 ) ) ;
#28854 = CARTESIAN_POINT ( 'NONE',  ( -0.1574803149606299191, -0.9232283463491653963, 0.000000000000000000 ) ) ;
#28856 = CARTESIAN_POINT ( 'NONE',  ( -1.054774247047244540, 0.07405724077823318263, 0.4232283464029293896 ) ) ;
#28857 = CARTESIAN_POINT ( 'NONE',  ( 0.9500414927467378812, 0.1787899950787401604, 0.5807086613635594752 ) ) ;
#28858 = ADVANCED_FACE ( 'NONE', ( #3877 ), #39813, .F. ) ;
#28859 = CARTESIAN_POINT ( 'NONE',  ( -0.1787899950787401604, -1.021653543253323138, 0.07405724077823318263 ) ) ;
#28860 = CARTESIAN_POINT ( 'NONE',  ( 0.8759842519685039353, -0.1787899950787401882, 0.1353346456155279653 ) ) ;
#28861 = CARTESIAN_POINT ( 'NONE',  ( -0.8107537697050254399, -0.1574803149606297803, 0.9325787400499523372 ) ) ;
#28862 = CARTESIAN_POINT ( 'NONE',  ( -0.9500414927467378812, -0.1787899950787401604, 1.589566929080094448 ) ) ;
#28863 = VERTEX_POINT ( 'NONE', #44126 ) ;
#28864 = CARTESIAN_POINT ( 'NONE',  ( -0.9500414927467378812, -0.1787899950787401604, 1.122047244040725644 ) ) ;
#28865 = CARTESIAN_POINT ( 'NONE',  ( -0.2984316586355673651, -0.08457185433607496139, -1.020769733662646672 ) ) ;
#28866 = CARTESIAN_POINT ( 'NONE',  ( 0.6971942568897648851, -0.07405724077823297447, 1.190944881836001112 ) ) ;
#28867 = CARTESIAN_POINT ( 'NONE',  ( -0.7185039370078739607, 1.928577636452523993E-17, 0.6889763778452283605 ) ) ;
#28868 = CARTESIAN_POINT ( 'NONE',  ( 1.033464566929134687, -0.06523048226347956391, 1.503444881889764995 ) ) ;
#28869 = CARTESIAN_POINT ( 'NONE',  ( 0.9500414927467378812, 0.1787899950787401604, 1.879921259788756016 ) ) ;
#28870 = CARTESIAN_POINT ( 'NONE',  ( -0.8759842519685039353, 0.1574803149606299191, 0.6102362204724409711 ) ) ;
#28871 = CARTESIAN_POINT ( 'NONE',  ( -0.9500414927467378812, 0.1787899950787401604, 0.8562992125446617919 ) ) ;
#28872 = LINE ( 'NONE', #43430, #38124 ) ;
#28873 = CARTESIAN_POINT ( 'NONE',  ( 0.7185039370078739607, 0.000000000000000000, 4.498031496062992574 ) ) ;
#28874 = CARTESIAN_POINT ( 'NONE',  ( 0.7495606340400177148, -0.1264236179284866091, 0.3272637794737956463 ) ) ;
#28875 = CARTESIAN_POINT ( 'NONE',  ( -0.9500414927467377701, -0.1787899950787401604, 0.2116141731745827814 ) ) ;
#28876 = CARTESIAN_POINT ( 'NONE',  ( -0.6971942568897626646, -0.07405724077823297447, 0.7529527558517473684 ) ) ;
#28877 = CARTESIAN_POINT ( 'NONE',  ( 0.9412147342319837628, -0.1574803149606297803, 1.606791338475149766 ) ) ;
#28878 = ORIENTED_EDGE ( 'NONE', *, *, #34470, .T. ) ;
#28879 = CARTESIAN_POINT ( 'NONE',  ( 0.07405724077823318263, 0.06102362210100767403, -0.1787899950787401604 ) ) ;
#28880 = ORIENTED_EDGE ( 'NONE', *, *, #26538, .T. ) ;
#28881 = CARTESIAN_POINT ( 'NONE',  ( 0.8019270111902717657, -0.1787899950787401604, 0.7234251967966300878 ) ) ;
#28882 = CARTESIAN_POINT ( 'NONE',  ( 0.6971942568897648851, -0.07405724077823297447, 0.9940944881352130613 ) ) ;
#28883 = CARTESIAN_POINT ( 'NONE',  ( -0.9500414927467377701, 0.1787899950787401604, 1.919291338528913649 ) ) ;
#28884 = CARTESIAN_POINT ( 'NONE',  ( 0.7495606340400177148, -0.1264236179284866091, 1.936515747977732405 ) ) ;
#28885 = ORIENTED_EDGE ( 'NONE', *, *, #911, .T. ) ;
#28886 = ADVANCED_FACE ( 'NONE', ( #7249 ), #47263, .F. ) ;
#28887 = DIRECTION ( 'NONE',  ( 0.000000000000000000, 0.000000000000000000, -1.000000000000000000 ) ) ;
#28888 = CARTESIAN_POINT ( 'NONE',  ( 0.9873396505805591694, -0.1113553986120547346, 1.609251968396409493 ) ) ;
#28889 = CARTESIAN_POINT ( 'NONE',  ( -0.07405724077823318263, -1.229454676890656684, 0.1787899950787401604 ) ) ;
#28890 = ORIENTED_EDGE ( 'NONE', *, *, #21603, .T. ) ;
#28891 = CARTESIAN_POINT ( 'NONE',  ( -0.07405724077823318263, -0.3080708660879689087, 0.1787899950787401604 ) ) ;
#28892 = ORIENTED_EDGE ( 'NONE', *, *, #24677, .T. ) ;
#28893 = EDGE_CURVE ( 'NONE', #24436, #46224, #25972, .T. ) ;
#28894 = DIRECTION ( 'NONE',  ( -1.000000000000000000, -0.000000000000000000, 0.000000000000000000 ) ) ;
#28895 = CARTESIAN_POINT ( 'NONE',  ( -0.9873396505805591694, 0.1113553986120547346, 0.9891732282389291697 ) ) ;
#28896 = VECTOR ( 'NONE', #44532, 39.37007874015748143 ) ;
#28897 = CARTESIAN_POINT ( 'NONE',  ( 0.8759842519685039353, 0.1787899950787401882, 0.07135826766277185429 ) ) ;
#28898 = CARTESIAN_POINT ( 'NONE',  ( 3.284318927891251994E-17, -1.609744094434425232, 0.1787899950787401882 ) ) ;
#28899 = CARTESIAN_POINT ( 'NONE',  ( -0.07405724077823318263, -0.7460629920722210429, 0.1787899950787401604 ) ) ;
#28900 = CARTESIAN_POINT ( 'NONE',  ( -1.002407869896990045, 0.1264236179284866091, 0.5437992125446614589 ) ) ;
#28901 = DIRECTION ( 'NONE',  ( 0.000000000000000000, -1.000000000000000000, 0.000000000000000000 ) ) ;
#28902 = CARTESIAN_POINT ( 'NONE',  ( -0.7174213970110099314, -0.05514141941195432883, 1.984310470025690609 ) ) ;
#28903 = DIRECTION ( 'NONE',  ( -3.469446951953614189E-15, -1.000000000000000000, 0.000000000000000000 ) ) ;
#28904 = CARTESIAN_POINT ( 'NONE',  ( 0.6971942568897648851, -0.07405724077823297447, 1.269685039316314601 ) ) ;
#28905 = CARTESIAN_POINT ( 'NONE',  ( 0.6971942568897648851, -0.07405724077823297447, 1.579724409395055318 ) ) ;
#28906 = CARTESIAN_POINT ( 'NONE',  ( -0.8759842519685039353, 0.000000000000000000, 0.000000000000000000 ) ) ;
#28907 = DIRECTION ( 'NONE',  ( 1.822029033848725028E-16, 0.000000000000000000, 1.000000000000000000 ) ) ;
#28908 = CARTESIAN_POINT ( 'NONE',  ( -0.8759842519685039353, 0.1574803149606299191, 1.702755905404283565 ) ) ;
#28909 = CARTESIAN_POINT ( 'NONE',  ( 1.002407869896990045, -0.1264236179284866091, 0.1353346456155277433 ) ) ;
#28910 = CARTESIAN_POINT ( 'NONE',  ( 0.7108038354695511707, 0.06841997037041733232, 0.03937007863263043694 ) ) ;
#28912 = CARTESIAN_POINT ( 'NONE',  ( -0.1476377952755905387, 0.7443365962042343131, -3.523993443072799270 ) ) ;
#28911 = CARTESIAN_POINT ( 'NONE',  ( 1.054774247047244540, 0.07405724077823318263, 1.087598425143086578 ) ) ;
#28913 = CARTESIAN_POINT ( 'NONE',  ( 0.7185039370078739607, 1.928577636452523993E-17, 1.210629921259842590 ) ) ;
#28914 = CARTESIAN_POINT ( 'NONE',  ( -0.8019270111902717657, 0.1787899950787401604, 1.176181102308441417 ) ) ;
#28915 = CARTESIAN_POINT ( 'NONE',  ( 0.9873396505805591694, 0.1113553986120547346, 0.4773622046168818911 ) ) ;
#28916 = ORIENTED_EDGE ( 'NONE', *, *, #41907, .F. ) ;
#28917 = CARTESIAN_POINT ( 'NONE',  ( -0.8107537697050254399, 0.1574803149606300301, 1.124507874015748810 ) ) ;
#28918 = CARTESIAN_POINT ( 'NONE',  ( 0.9494468377376082957, 0.1530141113397992803, 0.03936700763878682452 ) ) ;
#28919 = CARTESIAN_POINT ( 'NONE',  ( 0.9873396505805591694, 0.1113553986120547346, 0.2903543307086614012 ) ) ;
#28920 = CARTESIAN_POINT ( 'NONE',  ( -1.033464566929134687, 0.06523048226347956391, 0.4749015746956221085 ) ) ;
#28921 = VERTEX_POINT ( 'NONE', #11092 ) ;
#28922 = CARTESIAN_POINT ( 'NONE',  ( 0.8759842519685039353, -0.1787899950787401882, 1.468996062938362046 ) ) ;
#28923 = CARTESIAN_POINT ( 'NONE',  ( -0.9873396505805591694, -0.1113553986120547346, 1.146653543307086798 ) ) ;
#28925 = CARTESIAN_POINT ( 'NONE',  ( 0.6195511811023590720, -5.463695987328343027E-16, 1.186023622047243986 ) ) ;
#28924 = PLANE ( 'NONE',  #11198 ) ;
#28926 = CARTESIAN_POINT ( 'NONE',  ( -1.054774247047244096, 0.000000000000000000, 0.06151574797773248782 ) ) ;
#28927 = CARTESIAN_POINT ( 'NONE',  ( 0.1787899950787401604, -0.01771653537930737918, -0.07405724077823318263 ) ) ;
#28928 = VERTEX_POINT ( 'NONE', #33385 ) ;
#28929 = AXIS2_PLACEMENT_3D ( 'NONE', #5721, #35442, #13853 ) ;
#28930 = CARTESIAN_POINT ( 'NONE',  ( 1.033464566929133799, 0.000000000000000000, 0.4330708660342047489 ) ) ;
#28931 = EDGE_LOOP ( 'NONE', ( #12569, #27741, #23133 ) ) ;
#28932 = CARTESIAN_POINT ( 'NONE',  ( 0.2227678560578173761, 0.05525422739377827686, 0.1568179892043651547 ) ) ;
#28933 = CARTESIAN_POINT ( 'NONE',  ( 0.1550311931539155308, -0.09383642490574112260, -0.1959255884474807308 ) ) ;
#28934 = VERTEX_POINT ( 'NONE', #18267 ) ;
#28935 = CARTESIAN_POINT ( 'NONE',  ( 0.6971942568897626646, -0.07405724077823297447, 0.6003937007336389575 ) ) ;
#28936 = ADVANCED_FACE ( 'NONE', ( #4106 ), #12560, .F. ) ;
#28937 = CARTESIAN_POINT ( 'NONE',  ( -0.6971942568897637749, 2.189545951927499583E-17, 1.498523621993480326 ) ) ;
#28938 = CARTESIAN_POINT ( 'NONE',  ( -0.1574803149606297803, 0.1028543308161884856, 0.06523048226347956391 ) ) ;
#28939 = CARTESIAN_POINT ( 'NONE',  ( -0.8759842519685039353, 0.1787899950787401882, 1.178641732229700922 ) ) ;
#28940 = CARTESIAN_POINT ( 'NONE',  ( -0.9412147342319837628, 0.1574803149606300301, 0.2140748031496061687 ) ) ;
#28941 = ORIENTED_EDGE ( 'NONE', *, *, #36131, .F. ) ;
#28942 = CARTESIAN_POINT ( 'NONE',  ( -1.054774247047244540, -0.07405724077823318263, 1.043307086560409269 ) ) ;
#28943 = CARTESIAN_POINT ( 'NONE',  ( -0.7495606340400177148, 0.1264236179284866091, 0.7898622046706456068 ) ) ;
#28944 = ADVANCED_FACE ( 'NONE', ( #19198 ), #8339, .F. ) ;
#28945 = CARTESIAN_POINT ( 'NONE',  ( -0.8019270111902717657, -0.1787899950787401604, 0.1722440944344256208 ) ) ;
#28946 = DIRECTION ( 'NONE',  ( 0.000000000000000000, 0.000000000000000000, 1.000000000000000000 ) ) ;
#28947 = CARTESIAN_POINT ( 'NONE',  ( -0.1787899950787401604, -0.8406751493316020341, 0.07405724077823318263 ) ) ;
#28948 = ORIENTED_EDGE ( 'NONE', *, *, #40209, .T. ) ;
#28949 = CARTESIAN_POINT ( 'NONE',  ( 0.02510167551635381772, -0.08956215230678916950, 0.1488583647765791274 ) ) ;
#28950 = LINE ( 'NONE', #15253, #24163 ) ;
#28951 = ORIENTED_EDGE ( 'NONE', *, *, #39324, .T. ) ;
#28952 = DIRECTION ( 'NONE',  ( 0.000000000000000000, 0.000000000000000000, -1.000000000000000000 ) ) ;
#28953 = CARTESIAN_POINT ( 'NONE',  ( -0.7495606340400177148, -0.1264236179284866091, 0.7947834645131652831 ) ) ;
#28954 = ( BOUNDED_CURVE ( )  B_SPLINE_CURVE ( 2, ( #38923, #46582, #23851, #39384, #31294, #12847, #6085, #9481, #24096 ),
 .UNSPECIFIED., .F., .T. ) 
 B_SPLINE_CURVE_WITH_KNOTS ( ( 3, 2, 2, 2, 3 ),
 ( 0.1900000000000000022, 0.1925000000000000044, 0.1950000000000000067, 0.1975000000000000089, 0.2000000000000000111 ),
 .UNSPECIFIED. ) 
 CURVE ( )  GEOMETRIC_REPRESENTATION_ITEM ( )  RATIONAL_B_SPLINE_CURVE ( ( 1.000000000000000000, 0.9238795325112869605, 1.000000000000000000, 0.9238795325112869605, 1.000000000000000000, 0.9238795325112869605, 1.000000000000000000, 0.9238795325112869605, 1.000000000000000000 ) ) 
 REPRESENTATION_ITEM ( '' )  ) ;
#28955 = FACE_OUTER_BOUND ( 'NONE', #24986, .T. ) ;
#28956 = ORIENTED_EDGE ( 'NONE', *, *, #13752, .T. ) ;
#28957 = EDGE_CURVE ( 'NONE', #10382, #36909, #2958, .T. ) ;
#28958 = VECTOR ( 'NONE', #27676, 39.37007874015748143 ) ;
#28959 = CARTESIAN_POINT ( 'NONE',  ( -0.8019270111902716547, 0.1787899950787401604, 1.850393700733638624 ) ) ;
#28960 = CARTESIAN_POINT ( 'NONE',  ( -1.060626887254335780E-16, 0.000000000000000000, -0.4921259842519680183 ) ) ;
#28961 = AXIS2_PLACEMENT_3D ( 'NONE', #22881, #16180, #12352 ) ;
#28962 = VERTEX_POINT ( 'NONE', #5055 ) ;
#28963 = CARTESIAN_POINT ( 'NONE',  ( 0.8107537697050253289, -0.1574803149606297803, 0.6668307086614162493 ) ) ;
#28964 = CARTESIAN_POINT ( 'NONE',  ( -0.07444174185955065859, -0.7958115261184778300, -0.1797182628040039087 ) ) ;
#28965 = CARTESIAN_POINT ( 'NONE',  ( -0.8759842519685039353, 0.000000000000000000, 0.000000000000000000 ) ) ;
#28966 = CARTESIAN_POINT ( 'NONE',  ( -0.9873396505805591694, -0.1113553986120547346, 1.373031495955464587 ) ) ;
#28967 = CARTESIAN_POINT ( 'NONE',  ( 0.8759842519685039353, 0.1787899950787401882, 0.7062007873478109987 ) ) ;
#28968 = CARTESIAN_POINT ( 'NONE',  ( -0.06523048226347956391, -0.6648622047244090449, -0.1574803149606300301 ) ) ;
#28969 = CARTESIAN_POINT ( 'NONE',  ( -0.1203200820771420931, 0.1234194735009758043, -0.1070349918020434971 ) ) ;
#28970 = VERTEX_POINT ( 'NONE', #4324 ) ;
#28971 = CARTESIAN_POINT ( 'NONE',  ( -4.999628824793424855E-17, -0.2954942322624090623, -0.3149606299212598381 ) ) ;
#28972 = CARTESIAN_POINT ( 'NONE',  ( 0.8107537697050253289, 0.1574803149606300301, 1.281988188976378895 ) ) ;
#28974 = CARTESIAN_POINT ( 'NONE',  ( 0.2471922904502826812, -0.03219022224904102836, -0.1427165354330708902 ) ) ;
#28973 = CARTESIAN_POINT ( 'NONE',  ( 1.002407869896990045, -0.1264236179284866091, 1.990649606245448844 ) ) ;
#28975 = CARTESIAN_POINT ( 'NONE',  ( -0.3161444924769509779, 2.177585298233989164, -3.731703755406937439 ) ) ;
#28976 = CARTESIAN_POINT ( 'NONE',  ( -0.06523048226347956391, -0.6402559054042833431, 0.1574803149606297803 ) ) ;
#28978 = DIRECTION ( 'NONE',  ( 0.000000000000000000, 0.000000000000000000, -1.000000000000000000 ) ) ;
#28977 = CARTESIAN_POINT ( 'NONE',  ( 1.054774247047244540, -0.07405724077823318263, 0.6496062991588353874 ) ) ;
#28979 = CARTESIAN_POINT ( 'NONE',  ( 0.1264236179284866091, -0.6845472440407243120, -0.1264236179284866091 ) ) ;
#28980 = CARTESIAN_POINT ( 'NONE',  ( -0.9873396505805591694, -0.1113553986120547346, 0.3887795274515282729 ) ) ;
#28981 = ORIENTED_EDGE ( 'NONE', *, *, #43046, .F. ) ;
#28982 = CARTESIAN_POINT ( 'NONE',  ( 0.7185039370078746268, -0.06523048226347956391, 0.6126968502861739330 ) ) ;
#28983 = DIRECTION ( 'NONE',  ( 0.000000000000000000, 0.000000000000000000, 1.000000000000000000 ) ) ;
#28984 = CARTESIAN_POINT ( 'NONE',  ( 0.8019270111902717657, -0.1787899950787401604, 0.9547244093950547628 ) ) ;
#28985 = ADVANCED_FACE ( 'NONE', ( #18956 ), #30038, .T. ) ;
#28986 = PLANE ( 'NONE',  #34903 ) ;
#28987 = CARTESIAN_POINT ( 'NONE',  ( 0.1787899950787401604, -1.287401574749386768, 0.07405724077823318263 ) ) ;
#28988 = CARTESIAN_POINT ( 'NONE',  ( 0.1113553986120547346, -1.469488188976377785, 0.1113553986120547346 ) ) ;
#28989 = DIRECTION ( 'NONE',  ( 0.000000000000000000, 0.000000000000000000, 1.000000000000000000 ) ) ;
#28990 = CARTESIAN_POINT ( 'NONE',  ( -0.6971942568897637749, 2.189545951927499583E-17, 0.08120078734781142893 ) ) ;
#28991 = ORIENTED_EDGE ( 'NONE', *, *, #40983, .T. ) ;
#28992 = VERTEX_POINT ( 'NONE', #12752 ) ;
#28993 = EDGE_CURVE ( 'NONE', #43250, #18901, #23039, .T. ) ;
#28994 = CARTESIAN_POINT ( 'NONE',  ( 1.054774247047244096, 0.000000000000000000, 1.956200787347811110 ) ) ;
#28995 = EDGE_LOOP ( 'NONE', ( #16257, #24419, #20932, #18466 ) ) ;
#28996 = CARTESIAN_POINT ( 'NONE',  ( -0.06523048226347956391, -1.427657480207433771, 0.1574803149606297803 ) ) ;
#28997 = CARTESIAN_POINT ( 'NONE',  ( -1.002407869896990045, 0.1264236179284866091, 1.921751968450173376 ) ) ;
#28998 = CARTESIAN_POINT ( 'NONE',  ( -0.7495606340400177148, -0.1264236179284866091, 1.621555118056472455 ) ) ;
#28999 = VECTOR ( 'NONE', #31172, 39.37007874015748854 ) ;
#29000 = CARTESIAN_POINT ( 'NONE',  ( -0.8759842519685039353, 0.1787899950787401882, 0.3912401574265515491 ) ) ;
#29001 = CARTESIAN_POINT ( 'NONE',  ( -1.033464566929134687, -0.06523048226347956391, 1.808562992018457161 ) ) ;
#29002 = CARTESIAN_POINT ( 'NONE',  ( -1.054774247047244096, 0.000000000000000000, 1.956200787347811110 ) ) ;
#29003 = CARTESIAN_POINT ( 'NONE',  ( -0.7185039370078739607, 1.928577636452523993E-17, 1.486220472440944906 ) ) ;
#29004 = CARTESIAN_POINT ( 'NONE',  ( -0.9873396505805591694, -0.1113553986120547346, 1.855314960629921295 ) ) ;
#29005 = CARTESIAN_POINT ( 'NONE',  ( -0.2983856243743982506, 0.08472875797579371149, -1.020674147059416503 ) ) ;
#29006 = CARTESIAN_POINT ( 'NONE',  ( 0.1787899950787401604, -0.4322105824024667364, 0.07405724077823318263 ) ) ;
#29007 = CARTESIAN_POINT ( 'NONE',  ( -0.03606586445802484331, -0.09842519685039370636, 0.1546304134225889859 ) ) ;
#29008 = CONTEXT_DEPENDENT_SHAPE_REPRESENTATION ( #19579, #21444 ) ;
#29009 = CARTESIAN_POINT ( 'NONE',  ( 0.7185039370078739607, 0.000000000000000000, 4.498031496062992574 ) ) ;
#29010 = CARTESIAN_POINT ( 'NONE',  ( 0.2204724409448818867, 0.1591122789105269553, 0.000000000000000000 ) ) ;
#29011 = CARTESIAN_POINT ( 'NONE',  ( -0.6971942568897626646, -0.07405724077823297447, 0.1624015747493861295 ) ) ;
#29012 = EDGE_LOOP ( 'NONE', ( #5807, #32201, #39992, #13245 ) ) ;
#29013 = ORIENTED_EDGE ( 'NONE', *, *, #31842, .T. ) ;
#29014 = CARTESIAN_POINT ( 'NONE',  ( -0.7495606340400177148, 0.1264236179284866091, 1.459153543253322693 ) ) ;
#29015 = VERTEX_POINT ( 'NONE', #40749 ) ;
#29016 = CARTESIAN_POINT ( 'NONE',  ( -0.1787899950787401604, -1.110236220418677533, -0.07405724077823318263 ) ) ;
#29017 = CARTESIAN_POINT ( 'NONE',  ( -0.1264236179284866091, -1.383366141678519678, -0.1264236179284866091 ) ) ;
#29018 = VECTOR ( 'NONE', #38243, 39.37007874015748143 ) ;
#29019 = DIRECTION ( 'NONE',  ( 0.000000000000000000, 0.000000000000000000, -1.000000000000000000 ) ) ;
#29020 = DIRECTION ( 'NONE',  ( -0.000000000000000000, 1.000000000000000000, -0.000000000000000000 ) ) ;
#29021 = CARTESIAN_POINT ( 'NONE',  ( -0.7646288533564489232, 0.1113553986120547346, 0.9990157479239685223 ) ) ;
#29022 = CARTESIAN_POINT ( 'NONE',  ( 0.8019270111902717657, -0.1787899950787401604, 0.4084645668753704717 ) ) ;
#29023 = CARTESIAN_POINT ( 'NONE',  ( -0.1113553986120547346, -0.1505905511811023723, -0.1113553986120547346 ) ) ;
#29024 = CARTESIAN_POINT ( 'NONE',  ( 0.9873396505805591694, 0.1113553986120547346, 1.737204724301921299 ) ) ;
#29025 = ORIENTED_EDGE ( 'NONE', *, *, #11981, .T. ) ;
#29026 = CARTESIAN_POINT ( 'NONE',  ( 0.7185039370078746268, -0.06523048226347956391, 0.2189960628845991353 ) ) ;
#29027 = CARTESIAN_POINT ( 'NONE',  ( 1.033464566929134687, -0.06523048226347956391, 0.7160433070866151217 ) ) ;
#29029 = FACE_OUTER_BOUND ( 'NONE', #11403, .T. ) ;
#29028 = AXIS2_PLACEMENT_3D ( 'NONE', #35858, #32290, #46162 ) ;
#29030 = DIRECTION ( 'NONE',  ( 0.000000000000000000, 0.000000000000000000, 1.000000000000000000 ) ) ;
#29032 = CARTESIAN_POINT ( 'NONE',  ( 0.03901279071809810040, -0.09842519685039370636, 1.224299699984025658 ) ) ;
#29031 = DIRECTION ( 'NONE',  ( -1.144917494144692682E-16, -2.347476851301873745E-33, -1.000000000000000000 ) ) ;
#29033 = CARTESIAN_POINT ( 'NONE',  ( 0.7185039370078739607, 1.928577636452523993E-17, 0.1377952754830242266 ) ) ;
#29034 = CARTESIAN_POINT ( 'NONE',  ( 0.1264236179284866091, -0.02509842514308689362, 0.1264236179284866091 ) ) ;
#29035 = EDGE_CURVE ( 'NONE', #3818, #30831, #16105, .T. ) ;
#29036 = DIRECTION ( 'NONE',  ( -1.144917494144692682E-16, 3.972230510298676574E-31, -1.000000000000000000 ) ) ;
#29037 = CARTESIAN_POINT ( 'NONE',  ( -0.7185039370078739607, 1.928577636452523993E-17, 0.7677165353255432922 ) ) ;
#29038 = CARTESIAN_POINT ( 'NONE',  ( 0.1574803149606300301, -1.457185039262550719, 0.06523048226347956391 ) ) ;
#29039 = CARTESIAN_POINT ( 'NONE',  ( 0.1787899950787401604, -0.6968503936470246130, 0.07405724077823318263 ) ) ;
#29040 = CARTESIAN_POINT ( 'NONE',  ( -1.033464566929134687, 0.06523048226347956391, 0.08120078729404769935 ) ) ;
#29041 = CARTESIAN_POINT ( 'NONE',  ( -0.1574803149606300301, -1.053641732283463917, -0.06523048226347956391 ) ) ;
#29042 = CARTESIAN_POINT ( 'NONE',  ( 0.9412147342319837628, -0.1574803149606297803, 0.9374999998924736788 ) ) ;
#29043 = ADVANCED_FACE ( 'NONE', ( #12517 ), #8171, .T. ) ;
#29044 = DIRECTION ( 'NONE',  ( 7.047314121155781188E-15, 0.000000000000000000, 1.000000000000000000 ) ) ;
#29045 = CARTESIAN_POINT ( 'NONE',  ( -0.9500414927467378812, 0.1787899950787401604, 0.4232283464029293896 ) ) ;
#29046 = EDGE_LOOP ( 'NONE', ( #1787, #21904, #11222, #32772 ) ) ;
#29047 = ORIENTED_EDGE ( 'NONE', *, *, #10122, .T. ) ;
#29048 = CARTESIAN_POINT ( 'NONE',  ( -0.7495606340400177148, 0.1264236179284866091, 1.537893700733637736 ) ) ;
#29049 = ORIENTED_EDGE ( 'NONE', *, *, #34189, .F. ) ;
#29050 = EDGE_CURVE ( 'NONE', #65, #25178, #8411, .T. ) ;
#29051 = ORIENTED_EDGE ( 'NONE', *, *, #20877, .T. ) ;
#29052 = CARTESIAN_POINT ( 'NONE',  ( -0.9500414927467378812, -0.1787899950787401604, 0.8464566928596233275 ) ) ;
#29053 = CARTESIAN_POINT ( 'NONE',  ( 1.054774247047244540, -0.07405724077823318263, 0.1820866141194649179 ) ) ;
#29054 = EDGE_CURVE ( 'NONE', #19538, #5864, #29088, .T. ) ;
#29055 = CARTESIAN_POINT ( 'NONE',  ( 0.000000000000000000, 0.000000000000000000, 2.731847993664263218E-16 ) ) ;
#29056 = CARTESIAN_POINT ( 'NONE',  ( 1.054774247047244096, 0.000000000000000000, 0.6963582676627716461 ) ) ;
#29057 = CARTESIAN_POINT ( 'NONE',  ( -0.6971942568897648851, 0.07405724077823318263, 0.7480314960092282472 ) ) ;
#29058 = CYLINDRICAL_SURFACE ( 'NONE', #44452, 0.1574803149606299191 ) ;
#29059 = CONICAL_SURFACE ( 'NONE', #40483, 0.08090551181102362266, 0.9599310885968742602 ) ;
#29060 = CARTESIAN_POINT ( 'NONE',  ( -0.8759842519685039353, 0.000000000000000000, 0.000000000000000000 ) ) ;
#29061 = CARTESIAN_POINT ( 'NONE',  ( 0.1574803149606300301, -0.2317913384751499328, -0.06523048226347956391 ) ) ;
#29062 = CARTESIAN_POINT ( 'NONE',  ( -0.7185039370078746268, 0.06523048226347956391, 1.946358267609010095 ) ) ;
#29063 = ORIENTED_EDGE ( 'NONE', *, *, #23264, .T. ) ;
#29064 = CARTESIAN_POINT ( 'NONE',  ( -0.7646288533564489232, -0.1113553986120547346, 0.4281496062992125595 ) ) ;
#29065 = CARTESIAN_POINT ( 'NONE',  ( 1.054774247047244096, 0.000000000000000000, 1.523129921206078707 ) ) ;
#29066 = CARTESIAN_POINT ( 'NONE',  ( 0.1352647019381153504, -0.09851384554447126241, -0.1450745768490925292 ) ) ;
#29067 = DIRECTION ( 'NONE',  ( 0.000000000000000000, -1.000000000000000000, 0.000000000000000000 ) ) ;
#29068 = ORIENTED_EDGE ( 'NONE', *, *, #9749, .F. ) ;
#29069 = CIRCLE ( 'NONE', #29852, 0.009842519685039361269 ) ;
#29070 = CARTESIAN_POINT ( 'NONE',  ( 0.1264236179284866091, -1.694513732008765983, 0.1264236179284866091 ) ) ;
#29071 = ORIENTED_EDGE ( 'NONE', *, *, #1262, .F. ) ;
#29072 = VECTOR ( 'NONE', #19801, 39.37007874015748143 ) ;
#29073 = ( LENGTH_UNIT ( ) NAMED_UNIT ( * ) SI_UNIT ( $, .METRE. ) ) ;
#29074 = ORIENTED_EDGE ( 'NONE', *, *, #2699, .T. ) ;
#29075 = DIRECTION ( 'NONE',  ( -1.000000000000000000, 3.469446951953626022E-15, 0.000000000000000000 ) ) ;
#29076 = CARTESIAN_POINT ( 'NONE',  ( -0.07405724077823318263, -0.9773622046706458288, 0.1787899950787401604 ) ) ;
#29077 = CARTESIAN_POINT ( 'NONE',  ( 0.7646288533564489232, 0.1113553986120547346, 1.048228346456692828 ) ) ;
#29078 = CARTESIAN_POINT ( 'NONE',  ( 0.1630380177254369123, -0.1602364199967901970, 6.745834889254991641E-08 ) ) ;
#29079 = CARTESIAN_POINT ( 'NONE',  ( 0.7495606340400177148, -0.1264236179284866091, 1.739665354276945131 ) ) ;
#29080 = CARTESIAN_POINT ( 'NONE',  ( 0.8759842519685039353, 0.1787899950787401882, 0.3075787401037169411 ) ) ;
#29081 = CARTESIAN_POINT ( 'NONE',  ( -0.1270800023317771588, -0.2421697938350141632, -0.1270800023317771588 ) ) ;
#29082 = CARTESIAN_POINT ( 'NONE',  ( 3.284318927891251994E-17, -0.1246318422449868152, 0.1787899950787401882 ) ) ;
#29083 = CARTESIAN_POINT ( 'NONE',  ( 0.1787899950787401882, -0.2957677164816697180, -2.189545951927503898E-17 ) ) ;
#29084 = CARTESIAN_POINT ( 'NONE',  ( 0.1787899950787401882, -0.02509842514308689362, -2.189545951927503898E-17 ) ) ;
#29085 = CARTESIAN_POINT ( 'NONE',  ( 1.033464566929133799, 0.000000000000000000, 0.3641732283464567121 ) ) ;
#29086 = CARTESIAN_POINT ( 'NONE',  ( 0.8019270111902717657, -0.1787899950787401604, 0.6397637794737947026 ) ) ;
#29087 = CARTESIAN_POINT ( 'NONE',  ( -1.054774247047244540, 0.07405724077823318263, 0.9744094487651340231 ) ) ;
#29088 = CIRCLE ( 'NONE', #3797, 0.02900000000000052189 ) ;
#29089 = CARTESIAN_POINT ( 'NONE',  ( 0.7185039370078746268, 0.06523048226347956391, 1.001476377845229804 ) ) ;
#29091 = CARTESIAN_POINT ( 'NONE',  ( -0.8628785951446895641, -0.1737776015968645615, 1.987962957907532635 ) ) ;
#29090 = CARTESIAN_POINT ( 'NONE',  ( 0.1270800023317771588, -1.787445384386197045, -0.1270800023317771588 ) ) ;
#29092 = LINE ( 'NONE', #43170, #32319 ) ;
#29093 = CARTESIAN_POINT ( 'NONE',  ( 0.6971942568897648851, 0.07405724077823318263, 1.697834645615527771 ) ) ;
#29095 = CARTESIAN_POINT ( 'NONE',  ( 0.7185039370078739607, 1.928577636452523993E-17, 0.1377952754830242266 ) ) ;
#29094 = CARTESIAN_POINT ( 'NONE',  ( 0.4330708661417322913, 4.616380251121755931E-17, 0.000000000000000000 ) ) ;
#29096 = ORIENTED_EDGE ( 'NONE', *, *, #39682, .F. ) ;
#29097 = ORIENTED_EDGE ( 'NONE', *, *, #39795, .F. ) ;
#29098 = CARTESIAN_POINT ( 'NONE',  ( -1.284448818897637956, -0.3937007874015748254, -1.181102362204724310 ) ) ;
#29099 = CARTESIAN_POINT ( 'NONE',  ( 3.284318927891251994E-17, -0.3105314960092286913, 0.1787899950787401882 ) ) ;
#29101 = DIRECTION ( 'NONE',  ( 0.000000000000000000, 0.000000000000000000, -1.000000000000000000 ) ) ;
#29100 = CARTESIAN_POINT ( 'NONE',  ( -1.002407869896990045, -0.1264236179284866091, 0.4552165353793071745 ) ) ;
#29102 = AXIS2_PLACEMENT_3D ( 'NONE', #1955, #2185, #41943 ) ;
#29103 = CARTESIAN_POINT ( 'NONE',  ( 0.6971942568897626646, 0.07405724077823318263, 0.6299212597887560161 ) ) ;
#29104 = CARTESIAN_POINT ( 'NONE',  ( 0.07405724077823318263, -1.011811023568284451, 0.1787899950787401604 ) ) ;
#29105 = CARTESIAN_POINT ( 'NONE',  ( 0.8019270111902717657, -0.1787899950787401604, 0.05413385821395302888 ) ) ;
#29106 = ( BOUNDED_CURVE ( )  B_SPLINE_CURVE ( 2, ( #35714, #14147, #13658, #28295, #3349, #43110, #2624, #9841, #41976 ),
 .UNSPECIFIED., .F., .T. ) 
 B_SPLINE_CURVE_WITH_KNOTS ( ( 3, 2, 2, 2, 3 ),
 ( 0.6199999999999999956, 0.6225000000000000533, 0.6250000000000000000, 0.6274999999999999467, 0.6300000000000000044 ),
 .UNSPECIFIED. ) 
 CURVE ( )  GEOMETRIC_REPRESENTATION_ITEM ( )  RATIONAL_B_SPLINE_CURVE ( ( 1.000000000000000000, 0.9238795325112869605, 1.000000000000000000, 0.9238795325112869605, 1.000000000000000000, 0.9238795325112869605, 1.000000000000000000, 0.9238795325112869605, 1.000000000000000000 ) ) 
 REPRESENTATION_ITEM ( '' )  ) ;
#29107 = EDGE_CURVE ( 'NONE', #13283, #21269, #35919, .T. ) ;
#29108 = CARTESIAN_POINT ( 'NONE',  ( -0.4620708661417322616, 0.4133858267716533086, 0.9891732283464566011 ) ) ;
#29109 = CARTESIAN_POINT ( 'NONE',  ( -0.7495606340400177148, 0.1264236179284866091, 1.572342519631275692 ) ) ;
#29110 = EDGE_LOOP ( 'NONE', ( #18451, #41348, #31687, #7599, #21667, #7972, #31266, #24821, #38580, #40584, #18132, #2456, #37205, #42148, #40962, #30689 ) ) ;
#29111 = CARTESIAN_POINT ( 'NONE',  ( -0.6971942568897637749, 2.189545951927499583E-17, 1.149114173174582643 ) ) ;
#29112 = CARTESIAN_POINT ( 'NONE',  ( -0.2802233088437621755, -0.1328339237432896724, -0.7736657976934293579 ) ) ;
#29113 = CARTESIAN_POINT ( 'NONE',  ( 0.8759842519685039353, -0.1787899950787401882, 1.198326771599779628 ) ) ;
#29114 = CARTESIAN_POINT ( 'NONE',  ( 0.8759842519685039353, -0.1787899950787401882, 1.783956692859621995 ) ) ;
#29115 = CARTESIAN_POINT ( 'NONE',  ( -0.7185039370078746268, -0.06523048226347956391, 0.5437992125984247860 ) ) ;
#29116 = CARTESIAN_POINT ( 'NONE',  ( -0.8759842519685039353, -0.1787899950787401882, 0.8784448818360000022 ) ) ;
#29117 = EDGE_CURVE ( 'NONE', #3012, #39709, #1216, .T. ) ;
#29118 = LINE ( 'NONE', #14695, #12865 ) ;
#29119 = CARTESIAN_POINT ( 'NONE',  ( -0.05652825169351902851, -0.2628576309303358172, -0.05517042925146417587 ) ) ;
#29120 = CARTESIAN_POINT ( 'NONE',  ( 0.6971942568897626646, -0.07405724077823297447, 0.3248031495525359746 ) ) ;
#29121 = CARTESIAN_POINT ( 'NONE',  ( -0.8019270111902716547, -0.1787899950787401604, 0.2460629920722207653 ) ) ;
#29122 = CARTESIAN_POINT ( 'NONE',  ( -0.7495606340400177148, -0.1264236179284866091, 0.6766732282926929409 ) ) ;
#29123 = CARTESIAN_POINT ( 'NONE',  ( 0.7185039370078746268, 0.06523048226347956391, 1.552657480207433993 ) ) ;
#29124 = ORIENTED_EDGE ( 'NONE', *, *, #39152, .T. ) ;
#29125 = CARTESIAN_POINT ( 'NONE',  ( 0.1264236179284866091, 0.05856299217974780119, -0.1264236179284866091 ) ) ;
#29126 = CARTESIAN_POINT ( 'NONE',  ( 0.8759842519685039353, 0.1787899950787401882, 0.8636811023084409733 ) ) ;
#29127 = CARTESIAN_POINT ( 'NONE',  ( 0.6971942568897637749, 2.189545951927499583E-17, 1.109744094434425232 ) ) ;
#29128 = CARTESIAN_POINT ( 'NONE',  ( -0.8019270111902716547, -0.1787899950787401604, 1.781496062938362934 ) ) ;
#29129 = CARTESIAN_POINT ( 'NONE',  ( 0.7495606340400177148, -0.1264236179284866091, 1.975885826717889815 ) ) ;
#29130 = ( BOUNDED_CURVE ( )  B_SPLINE_CURVE ( 2, ( #18906, #32199, #28370, #7646, #28624, #25881, #46785, #22263, #40928 ),
 .UNSPECIFIED., .F., .T. ) 
 B_SPLINE_CURVE_WITH_KNOTS ( ( 3, 2, 2, 2, 3 ),
 ( 0.4899999999999999911, 0.4924999999999999933, 0.4949999999999999956, 0.4974999999999999978, 0.5000000000000000000 ),
 .UNSPECIFIED. ) 
 CURVE ( )  GEOMETRIC_REPRESENTATION_ITEM ( )  RATIONAL_B_SPLINE_CURVE ( ( 1.000000000000000000, 0.9238795325112869605, 1.000000000000000000, 0.9238795325112869605, 1.000000000000000000, 0.9238795325112869605, 1.000000000000000000, 0.9238795325112869605, 1.000000000000000000 ) ) 
 REPRESENTATION_ITEM ( '' )  ) ;
#29131 = CIRCLE ( 'NONE', #32166, 0.1003937007874010356 ) ;
#29132 = CYLINDRICAL_SURFACE ( 'NONE', #6803, 0.1574803149606299191 ) ;
#29133 = CARTESIAN_POINT ( 'NONE',  ( -0.1787899950787401604, -1.313116094213492069, 0.07405724077823318263 ) ) ;
#29134 = EDGE_LOOP ( 'NONE', ( #17646, #9992, #27766, #24826, #28991, #32217, #9643, #33538 ) ) ;
#29135 = CARTESIAN_POINT ( 'NONE',  ( 0.07405724077823318263, -0.2637795275052916555, 0.1787899950787401604 ) ) ;
#29136 = CARTESIAN_POINT ( 'NONE',  ( -0.1574803149606299191, 0.02165354341461366364, 0.000000000000000000 ) ) ;
#29137 = ORIENTED_EDGE ( 'NONE', *, *, #9538, .F. ) ;
#29138 = CARTESIAN_POINT ( 'NONE',  ( 0.8019270111902717657, -0.1787899950787401604, 1.151574803095843036 ) ) ;
#29139 = CARTESIAN_POINT ( 'NONE',  ( -1.033464566929133799, 0.000000000000000000, 1.456692913278299084 ) ) ;
#29140 = AXIS2_PLACEMENT_3D ( 'NONE', #5964, #20583, #31404 ) ;
#29141 = CARTESIAN_POINT ( 'NONE',  ( -0.2471922026429036467, -0.09209855619639897850, 0.04265916558023801625 ) ) ;
#29142 = CARTESIAN_POINT ( 'NONE',  ( 0.8019270111902717657, 0.1787899950787401604, 1.491141732229701367 ) ) ;
#29143 = CARTESIAN_POINT ( 'NONE',  ( 1.054774247047244540, 0.07405724077823318263, 0.06397637789899228433 ) ) ;
#29144 = CARTESIAN_POINT ( 'NONE',  ( 0.1264236179284866091, -1.673720472387181024, -0.1264236179284866091 ) ) ;
#29145 = CARTESIAN_POINT ( 'NONE',  ( 0.1264236179284866091, -1.629429133804503937, -0.1264236179284866091 ) ) ;
#29146 = CARTESIAN_POINT ( 'NONE',  ( -1.002407869896990045, 0.1264236179284866091, 0.4650590550643464716 ) ) ;
#29147 = CARTESIAN_POINT ( 'NONE',  ( 0.5538057742782149795, 0.08090551181102362266, 0.000000000000000000 ) ) ;
#29149 = CARTESIAN_POINT ( 'NONE',  ( -0.7117020095487714970, -0.02979564497706602491, 1.983816935281811578 ) ) ;
#29148 = CARTESIAN_POINT ( 'NONE',  ( -0.07444174185955065859, -1.292858770212966135, 0.1797182628040039087 ) ) ;
#29150 = CARTESIAN_POINT ( 'NONE',  ( -1.033464566929134687, 0.06523048226347956391, 1.193405511811024278 ) ) ;
#29151 = CARTESIAN_POINT ( 'NONE',  ( -0.8107537697050253289, -0.1574803149606297803, 1.601870078632630756 ) ) ;
#29152 = CARTESIAN_POINT ( 'NONE',  ( 0.6971942568897637749, 2.189545951927499583E-17, 1.267224409395055096 ) ) ;
#29153 = CARTESIAN_POINT ( 'NONE',  ( 0.8759842519685039353, 0.1787899950787401882, 1.646161417269070837 ) ) ;
#29154 = FACE_OUTER_BOUND ( 'NONE', #12407, .T. ) ;
#29155 = DIRECTION ( 'NONE',  ( -1.000000000000000000, 0.000000000000000000, 0.000000000000000000 ) ) ;
#29156 = CARTESIAN_POINT ( 'NONE',  ( 0.1555687797274980522, 0.05303742630350882087, -0.1377952755905511861 ) ) ;
#29157 = CARTESIAN_POINT ( 'NONE',  ( -0.1113553986120547346, -0.7706692912310552090, -0.1113553986120547346 ) ) ;
#29158 = CARTESIAN_POINT ( 'NONE',  ( -0.9412147342319837628, -0.1574803149606297803, 1.724901574695621553 ) ) ;
#29159 = CARTESIAN_POINT ( 'NONE',  ( 0.8019270111902717657, 0.1787899950787401604, 0.1919291338045042428 ) ) ;
#29160 = CARTESIAN_POINT ( 'NONE',  ( 0.7063448026206018415, -0.03181611069741603626, 0.03937227967794548061 ) ) ;
#29161 = EDGE_CURVE ( 'NONE', #14401, #29926, #15867, .T. ) ;
#29162 = DIRECTION ( 'NONE',  ( -3.532562060772668727E-15, 0.000000000000000000, 1.000000000000000000 ) ) ;
#29163 = VECTOR ( 'NONE', #6282, 39.37007874015748143 ) ;
#29164 = CARTESIAN_POINT ( 'NONE',  ( 0.8759842519685039353, -0.1574803149606299191, 1.220472440944881942 ) ) ;
#29165 = CARTESIAN_POINT ( 'NONE',  ( -1.002407869896990045, -0.1264236179284866091, 1.237696850339937038 ) ) ;
#29166 = CARTESIAN_POINT ( 'NONE',  ( 1.033464566929134687, 0.06523048226347956391, 0.5536417321759372623 ) ) ;
#29167 = ORIENTED_EDGE ( 'NONE', *, *, #40139, .T. ) ;
#29168 = LINE ( 'NONE', #39409, #45206 ) ;
#29169 = CARTESIAN_POINT ( 'NONE',  ( 0.9008793413134227324, 0.1712306536401314860, 0.03937060926507291586 ) ) ;
#29170 = CARTESIAN_POINT ( 'NONE',  ( 1.033464566929133799, 0.000000000000000000, 0.2854330708661417804 ) ) ;
#29171 = DIRECTION ( 'NONE',  ( -0.000000000000000000, 0.6156614753256608452, 0.7880107536067200158 ) ) ;
#29172 = PRODUCT ( 'Handle Arm Right', 'Handle Arm Right', '', ( #16382 ) ) ;
#29173 = CARTESIAN_POINT ( 'NONE',  ( -0.1113553986120547346, -1.036417322727118062, 0.1113553986120547346 ) ) ;
#29174 = CARTESIAN_POINT ( 'NONE',  ( -1.033464566929134687, -0.06523048226347956391, 0.4306102361129448552 ) ) ;
#29175 = AXIS2_PLACEMENT_3D ( 'NONE', #33978, #18848, #37538 ) ;
#29176 = DIRECTION ( 'NONE',  ( 0.000000000000000000, -1.000000000000000000, 0.000000000000000000 ) ) ;
#29177 = CARTESIAN_POINT ( 'NONE',  ( 0.6971942568897648851, 0.07405724077823318263, 1.496062992072220821 ) ) ;
#29178 = CARTESIAN_POINT ( 'NONE',  ( -0.8107537697050253289, -0.1574803149606297803, 1.139271653543306506 ) ) ;
#29179 = EDGE_CURVE ( 'NONE', #6423, #13443, #976, .T. ) ;
#29181 = CARTESIAN_POINT ( 'NONE',  ( -0.9412147342319837628, -0.1574803149606297803, 1.380413385826771533 ) ) ;
#29180 = CARTESIAN_POINT ( 'NONE',  ( -1.033464566929133799, 0.000000000000000000, 1.781496062992125928 ) ) ;
#29182 = CARTESIAN_POINT ( 'NONE',  ( 0.8759842519685039353, -0.1574803149606299191, 1.181102362204724310 ) ) ;
#29183 = CARTESIAN_POINT ( 'NONE',  ( -1.002407869896990045, -0.1264236179284866091, 0.05659448813521283234 ) ) ;
#29185 = CIRCLE ( 'NONE', #19941, 0.1003937007874010356 ) ;
#29184 = CARTESIAN_POINT ( 'NONE',  ( -0.1787899950787401882, -0.07923228341080354453, 0.000000000000000000 ) ) ;
#29186 = VERTEX_POINT ( 'NONE', #34539 ) ;
#29187 = CYLINDRICAL_SURFACE ( 'NONE', #39789, 0.1574803149606299191 ) ;
#29188 = DIRECTION ( 'NONE',  ( -1.000000000000000000, 0.000000000000000000, 0.000000000000000000 ) ) ;
#29189 = CARTESIAN_POINT ( 'NONE',  ( 0.000000000000000000, 0.1299212598425196763, 0.000000000000000000 ) ) ;
#29190 = ORIENTED_EDGE ( 'NONE', *, *, #40334, .F. ) ;
#29191 = CARTESIAN_POINT ( 'NONE',  ( 0.7495606340400177148, 0.1264236179284866091, 0.5930118109698583329 ) ) ;
#29192 = ORIENTED_EDGE ( 'NONE', *, *, #19908, .F. ) ;
#29193 = CARTESIAN_POINT ( 'NONE',  ( 0.1574803149606300301, 0.1176181103437474174, 0.06523048226347956391 ) ) ;
#29194 = CARTESIAN_POINT ( 'NONE',  ( -1.002407869896990045, -0.1264236179284866091, 1.085137795221826629 ) ) ;
#29195 = ORIENTED_EDGE ( 'NONE', *, *, #24035, .T. ) ;
#29196 = CARTESIAN_POINT ( 'NONE',  ( -0.9500414927467377701, 0.1787899950787401604, 1.092519684985606032 ) ) ;
#29197 = CARTESIAN_POINT ( 'NONE',  ( -1.054774247047244540, 0.07405724077823318263, 0.8562992125446617919 ) ) ;
#29198 = CARTESIAN_POINT ( 'NONE',  ( -0.9500414927467378812, -0.1787899950787401604, 0.2165354330171024577 ) ) ;
#29199 = CARTESIAN_POINT ( 'NONE',  ( -1.033464566929133799, 0.000000000000000000, 0.3641732283464567121 ) ) ;
#29200 = CYLINDRICAL_SURFACE ( 'NONE', #19016, 0.1968503937007874405 ) ;
#29201 = CARTESIAN_POINT ( 'NONE',  ( -0.07405724077823318263, -0.7717775115363263438, -0.1787899950787401604 ) ) ;
#29202 = ORIENTED_EDGE ( 'NONE', *, *, #8004, .F. ) ;
#29203 = CARTESIAN_POINT ( 'NONE',  ( -0.9873396505805591694, 0.1113553986120547346, 0.05413385826771653642 ) ) ;
#29204 = CARTESIAN_POINT ( 'NONE',  ( 0.7646288533564489232, -0.1113553986120547346, 1.058070866141732402 ) ) ;
#29205 = EDGE_LOOP ( 'NONE', ( #5679, #1793, #37304, #27792, #28035 ) ) ;
#29206 = CYLINDRICAL_SURFACE ( 'NONE', #34813, 0.1574803149606299191 ) ;
#29207 = EDGE_CURVE ( 'NONE', #12477, #41019, #26418, .T. ) ;
#29208 = CARTESIAN_POINT ( 'NONE',  ( -0.8759842519685039353, -0.1787899950787401882, 0.7209645668753701386 ) ) ;
#29209 = CARTESIAN_POINT ( 'NONE',  ( -1.033464566929134687, -0.06523048226347956391, 0.5880905510735752184 ) ) ;
#29211 = ORIENTED_EDGE ( 'NONE', *, *, #31296, .F. ) ;
#29210 = AXIS2_PLACEMENT_3D ( 'NONE', #31784, #13105, #13329 ) ;
#29212 = CARTESIAN_POINT ( 'NONE',  ( -0.6971942568897648851, 0.07405724077823318263, 1.815944881835999780 ) ) ;
#29213 = AXIS2_PLACEMENT_3D ( 'NONE', #38947, #20267, #2058 ) ;
#29214 = AXIS2_PLACEMENT_3D ( 'NONE', #27626, #38136, #12279 ) ;
#29215 = CARTESIAN_POINT ( 'NONE',  ( -0.8019270111902716547, -0.1787899950787401604, 0.05413385821395302888 ) ) ;
#29216 = CARTESIAN_POINT ( 'NONE',  ( 0.8759842519685039353, -0.1574803149606299191, 0.7086614173228346081 ) ) ;
#29217 = CARTESIAN_POINT ( 'NONE',  ( -0.1270800023317771588, -0.9114611324176910001, -0.1270800023317771588 ) ) ;
#29218 = CARTESIAN_POINT ( 'NONE',  ( 0.1279527559055118058, -0.2216206741968047289, -0.3149606299212598381 ) ) ;
#29219 = CARTESIAN_POINT ( 'NONE',  ( -0.7185039370078739607, 1.928577636452523993E-17, 1.358267716427907779 ) ) ;
#29220 = VECTOR ( 'NONE', #10022, 39.37007874015748143 ) ;
#29221 = EDGE_CURVE ( 'NONE', #12477, #25910, #35179, .T. ) ;
#29222 = CARTESIAN_POINT ( 'NONE',  ( 0.7495606340400177148, 0.1264236179284866091, 0.8292322834108031282 ) ) ;
#29223 = CYLINDRICAL_SURFACE ( 'NONE', #6975, 0.1787899950787401049 ) ;
#29224 = CARTESIAN_POINT ( 'NONE',  ( -0.2559055118110235560, 0.08067097267005921002, -0.05399682104008290962 ) ) ;
#29225 = CARTESIAN_POINT ( 'NONE',  ( 0.9412147342319837628, -0.1574803149606297803, 1.459153543307085688 ) ) ;
#29226 = DIRECTION ( 'NONE',  ( 0.000000000000000000, -0.7880107536067200158, 0.6156614753256608452 ) ) ;
#29228 = CARTESIAN_POINT ( 'NONE',  ( -0.2066929133858267931, 1.174718201258053485, -3.430321324600322352 ) ) ;
#29227 = CARTESIAN_POINT ( 'NONE',  ( 0.7647590343208214847, -0.1296210501886547739, 1.985957554512493006 ) ) ;
#29229 = CARTESIAN_POINT ( 'NONE',  ( -0.5555748031496058337, 0.2597269656108975311, 0.7480314960629921295 ) ) ;
#29230 = EDGE_LOOP ( 'NONE', ( #11101, #15995 ) ) ;
#29231 = EDGE_CURVE ( 'NONE', #6080, #802, #25212, .T. ) ;
#29233 = DIRECTION ( 'NONE',  ( 1.000000000000000000, 0.000000000000000000, 0.000000000000000000 ) ) ;
#29232 = CARTESIAN_POINT ( 'NONE',  ( 0.9500414927467377701, 0.1787899950787401604, 0.7381889763241898939 ) ) ;
#29234 = ORIENTED_EDGE ( 'NONE', *, *, #10299, .F. ) ;
#29235 = CARTESIAN_POINT ( 'NONE',  ( 0.9873396505805591694, -0.1113553986120547346, 0.6249999998924724576 ) ) ;
#29236 = CARTESIAN_POINT ( 'NONE',  ( -0.7185039370078739607, 0.000000000000000000, -2.869337061179095023E-17 ) ) ;
#29237 = CARTESIAN_POINT ( 'NONE',  ( 0.8759842519685039353, 0.1787899950787401882, 1.055610236166708793 ) ) ;
#29238 = EDGE_CURVE ( 'NONE', #38091, #40174, #41248, .T. ) ;
#29239 = DIRECTION ( 'NONE',  ( -1.000000000000000000, 0.000000000000000000, -0.000000000000000000 ) ) ;
#29240 = CARTESIAN_POINT ( 'NONE',  ( 0.1574803149606299191, -1.464566929133858109, -1.928577636452523993E-17 ) ) ;
#29241 = DIRECTION ( 'NONE',  ( -0.7986355100473023771, 5.219913244286809847E-16, -0.6018150231520357218 ) ) ;
#29242 = AXIS2_PLACEMENT_3D ( 'NONE', #8950, #19492, #8464 ) ;
#29243 = UNCERTAINTY_MEASURE_WITH_UNIT (LENGTH_MEASURE( 1.000000000000000082E-05 ), #30026, 'distance_accuracy_value', 'NONE') ;
#29244 = VERTEX_POINT ( 'NONE', #8894 ) ;
#29245 = CARTESIAN_POINT ( 'NONE',  ( -0.9500414927467378812, -0.1787899950787401604, 0.05413385821395302888 ) ) ;
#29246 = ORIENTED_EDGE ( 'NONE', *, *, #42444, .T. ) ;
#29247 = CARTESIAN_POINT ( 'NONE',  ( 0.1574803149606299191, 0.1102362204724409434, -1.928577636452523993E-17 ) ) ;
#29248 = CARTESIAN_POINT ( 'NONE',  ( -0.7646288533564489232, -0.1113553986120547346, 1.845472440944881942 ) ) ;
#29249 = VECTOR ( 'NONE', #30838, 39.37007874015748143 ) ;
#29250 = AXIS2_PLACEMENT_3D ( 'NONE', #10219, #10461, #7329 ) ;
#29251 = CARTESIAN_POINT ( 'NONE',  ( -0.7495606340400177148, 0.1264236179284866091, 1.651082677111590513 ) ) ;
#29252 = CARTESIAN_POINT ( 'NONE',  ( -0.9500414927467377701, 0.1787899950787401604, 0.8169291338045038264 ) ) ;
#29253 = CARTESIAN_POINT ( 'NONE',  ( -0.9500414927467378812, 0.1787899950787401604, 0.3494094487651343006 ) ) ;
#29254 = ( BOUNDED_CURVE ( )  B_SPLINE_CURVE ( 2, ( #14899, #29560, #3, #28833, #7449, #29326, #28586, #24725, #14423 ),
 .UNSPECIFIED., .F., .F. ) 
 B_SPLINE_CURVE_WITH_KNOTS ( ( 3, 2, 2, 2, 3 ),
 ( 0.5699999999999999512, 0.5725000000000000089, 0.5749999999999999556, 0.5775000000000000133, 0.5799999999999999600 ),
 .UNSPECIFIED. ) 
 CURVE ( )  GEOMETRIC_REPRESENTATION_ITEM ( )  RATIONAL_B_SPLINE_CURVE ( ( 1.000000000000000000, 0.9238795325112899581, 1.000000000000000000, 0.9238795325112869605, 1.000000000000000000, 0.9238795325112869605, 1.000000000000000000, 0.9238795325112869605, 1.000000000000000000 ) ) 
 REPRESENTATION_ITEM ( '' )  ) ;
#29255 = CARTESIAN_POINT ( 'NONE',  ( -0.9412147342319837628, -0.1574803149606297803, 1.803641732175937706 ) ) ;
#29256 = CARTESIAN_POINT ( 'NONE',  ( 0.8107537697050254399, 0.1574803149606300301, 0.4060039369003470289 ) ) ;
#29257 = CARTESIAN_POINT ( 'NONE',  ( 0.1006676817877055763, -0.09658349877441900488, -0.2273124399501114945 ) ) ;
#29258 = CARTESIAN_POINT ( 'NONE',  ( 0.08837071341806096436, 0.09266989036297287874, -0.2344122156857449679 ) ) ;
#29259 = CARTESIAN_POINT ( 'NONE',  ( -0.2896382684968236143, 0.1109106728611159998, -1.001724715795912601 ) ) ;
#29260 = CARTESIAN_POINT ( 'NONE',  ( -0.1264236179284866091, -0.3362460154733335482, -0.1264236179284866091 ) ) ;
#29261 = CARTESIAN_POINT ( 'NONE',  ( -0.1127940203827588611, -0.09842519685039370636, -0.1442820423458218704 ) ) ;
#29262 = DIRECTION ( 'NONE',  ( 0.000000000000000000, 0.6156614753256595129, 0.7880107536067211260 ) ) ;
#29263 = CARTESIAN_POINT ( 'NONE',  ( -1.059421526231553215E-16, 0.000000000000000000, -0.4931102362204718426 ) ) ;
#29264 = CARTESIAN_POINT ( 'NONE',  ( -0.7495606340400177148, 0.1264236179284866091, 0.3518700786863940833 ) ) ;
#29265 = ORIENTED_EDGE ( 'NONE', *, *, #47180, .T. ) ;
#29266 = ORIENTED_EDGE ( 'NONE', *, *, #13636, .T. ) ;
#29267 = CARTESIAN_POINT ( 'NONE',  ( -0.7495606340400177148, -0.1264236179284866091, 1.350885826717889815 ) ) ;
#29268 = ORIENTED_EDGE ( 'NONE', *, *, #17171, .T. ) ;
#29269 = ADVANCED_FACE ( 'NONE', ( #23525 ), #19909, .T. ) ;
#29270 = CARTESIAN_POINT ( 'NONE',  ( 0.1264236179284866091, -1.171751968450173154, 0.1264236179284866091 ) ) ;
#29271 = CARTESIAN_POINT ( 'NONE',  ( 3.284318927891251994E-17, -1.329232283410803239, 0.1787899950787401882 ) ) ;
#29272 = CARTESIAN_POINT ( 'NONE',  ( 0.000000000000000000, 0.000000000000000000, 0.09842519685039370636 ) ) ;
#29273 = EDGE_CURVE ( 'NONE', #38634, #31350, #17434, .T. ) ;
#29274 = CARTESIAN_POINT ( 'NONE',  ( 0.8019270111902717657, 0.1787899950787401604, 0.3937007873478115538 ) ) ;
#29275 = CARTESIAN_POINT ( 'NONE',  ( -0.1574803149606300301, -0.1087598425196850405, -0.06523048226347956391 ) ) ;
#29276 = CIRCLE ( 'NONE', #8552, 0.08090551181102362266 ) ;
#29277 = AXIS2_PLACEMENT_3D ( 'NONE', #36066, #3223, #17854 ) ;
#29278 = CARTESIAN_POINT ( 'NONE',  ( 0.7646288533564489232, -0.1113553986120547346, 1.756889763671999782 ) ) ;
#29279 = EDGE_LOOP ( 'NONE', ( #16199, #19620, #35786, #21248 ) ) ;
#29280 = CARTESIAN_POINT ( 'NONE',  ( -0.1787899950787401604, -0.1998031495525358359, 0.07405724077823318263 ) ) ;
#29281 = CARTESIAN_POINT ( 'NONE',  ( 0.9412147342319837628, -0.1574803149606297803, 0.2288385825696384601 ) ) ;
#29282 = CARTESIAN_POINT ( 'NONE',  ( 1.033464566929133799, 0.000000000000000000, 0.7185039370078739607 ) ) ;
#29283 = DIRECTION ( 'NONE',  ( -3.469446951953614978E-15, -1.000000000000000000, 3.995705278811693553E-31 ) ) ;
#29285 = LINE ( 'NONE', #15578, #25439 ) ;
#29284 = DIRECTION ( 'NONE',  ( -0.8660254037844389297, 0.000000000000000000, -0.4999999999999994449 ) ) ;
#29286 = CARTESIAN_POINT ( 'NONE',  ( 0.7185039370078746268, -0.06523048226347956391, 0.7800196850393691372 ) ) ;
#29287 = ORIENTED_EDGE ( 'NONE', *, *, #29563, .F. ) ;
#29288 = ORIENTED_EDGE ( 'NONE', *, *, #3420, .T. ) ;
#29289 = DIRECTION ( 'NONE',  ( 1.000000000000000000, -0.000000000000000000, -0.000000000000000000 ) ) ;
#29290 = CARTESIAN_POINT ( 'NONE',  ( 3.284318927891251994E-17, -1.526082677111590513, 0.1787899950787401882 ) ) ;
#29291 = CARTESIAN_POINT ( 'NONE',  ( -0.06523048226347956391, -1.599901574695621109, -0.1574803149606300301 ) ) ;
#29292 = CARTESIAN_POINT ( 'NONE',  ( 0.1787899950787401882, -0.7731299212060788184, -2.189545951927503898E-17 ) ) ;
#29293 = CARTESIAN_POINT ( 'NONE',  ( -0.8759842519685039353, 0.1574803149606299191, 0.1279527557979848462 ) ) ;
#29294 = CARTESIAN_POINT ( 'NONE',  ( -0.1574803149606299191, -1.011811023622047223, 0.000000000000000000 ) ) ;
#29295 = CARTESIAN_POINT ( 'NONE',  ( 0.8107537697050253289, -0.1574803149606297803, 0.9719488187901104137 ) ) ;
#29296 = CARTESIAN_POINT ( 'NONE',  ( 0.9873396505805591694, 0.1113553986120547346, 0.5265748031496062520 ) ) ;
#29297 = CARTESIAN_POINT ( 'NONE',  ( -0.7495606340400177148, 0.1264236179284866091, 0.3912401574265515491 ) ) ;
#29298 = ORIENTED_EDGE ( 'NONE', *, *, #19719, .F. ) ;
#29299 = ORIENTED_EDGE ( 'NONE', *, *, #17696, .F. ) ;
#29300 = CARTESIAN_POINT ( 'NONE',  ( -1.054774247047244540, -0.07405724077823318263, 1.678149606245448622 ) ) ;
#29301 = VERTEX_POINT ( 'NONE', #46483 ) ;
#29302 = CARTESIAN_POINT ( 'NONE',  ( 0.8019270111902717657, 0.1787899950787401604, 1.692913385773008539 ) ) ;
#29303 = CARTESIAN_POINT ( 'NONE',  ( -1.054774247047244096, 0.000000000000000000, 0.8538385826234016207 ) ) ;
#29304 = CARTESIAN_POINT ( 'NONE',  ( 1.002407869896990045, 0.1264236179284866091, 0.3075787401037169411 ) ) ;
#29305 = CARTESIAN_POINT ( 'NONE',  ( -0.7185039370078739607, 1.928577636452523993E-17, 0.4527559054042842868 ) ) ;
#29306 = CARTESIAN_POINT ( 'NONE',  ( 0.7495606340400177148, -0.1264236179284866091, 0.7603346456155274380 ) ) ;
#29307 = CARTESIAN_POINT ( 'NONE',  ( -1.054774247047244096, 0.000000000000000000, 0.7308070865604093802 ) ) ;
#29308 = CIRCLE ( 'NONE', #26987, 0.09842519685039370636 ) ;
#29309 = CARTESIAN_POINT ( 'NONE',  ( -6.716149524815622026E-17, 0.1574803149606340824, -0.4950787401574787139 ) ) ;
#29310 = VECTOR ( 'NONE', #40459, 39.37007874015748143 ) ;
#29311 = DIRECTION ( 'NONE',  ( 1.000000000000000000, 0.000000000000000000, -1.822029033848725275E-16 ) ) ;
#29312 = CARTESIAN_POINT ( 'NONE',  ( -0.9500414927467378812, 0.1787899950787401604, 1.569881889710015299 ) ) ;
#29313 = CARTESIAN_POINT ( 'NONE',  ( -0.7646288533564489232, -0.1113553986120547346, 1.835629921152314825 ) ) ;
#29314 = ORIENTED_EDGE ( 'NONE', *, *, #26497, .F. ) ;
#29315 = CARTESIAN_POINT ( 'NONE',  ( -0.7185039370078739607, 1.928577636452523993E-17, 1.525590551181102317 ) ) ;
#29316 = CARTESIAN_POINT ( 'NONE',  ( 0.1661702112335584902, -0.4376325038317900873, -0.9700951799340379322 ) ) ;
#29317 = CARTESIAN_POINT ( 'NONE',  ( 1.054774247047244540, -0.07405724077823318263, 1.402559055064346749 ) ) ;
#29318 = CARTESIAN_POINT ( 'NONE',  ( -0.1516630832887128078, -0.09851383746137795661, -0.09563143930829449968 ) ) ;
#29319 = DIRECTION ( 'NONE',  ( 1.000000000000000000, 0.000000000000000000, -1.822029033848725275E-16 ) ) ;
#29320 = AXIS2_PLACEMENT_3D ( 'NONE', #1140, #1374, #34465 ) ;
#29321 = ORIENTED_EDGE ( 'NONE', *, *, #30826, .F. ) ;
#29322 = AXIS2_PLACEMENT_3D ( 'NONE', #40046, #22559, #40282 ) ;
#29323 = EDGE_LOOP ( 'NONE', ( #29211, #40004, #43846, #21744, #20594, #39082, #40842, #11178, #29268, #4728, #31035, #46151, #14948, #39443, #41269, #41187, #28850, #35157, #27339, #4905, #43933, #32284, #28506, #43276, #45548, #35346, #11884, #25776, #45726, #311, #30750, #35838, #38378, #10518, #32262, #44371, #26966, #29556, #14885, #1852, #38662, #46417, #38276, #13179, #33892, #37326, #31498, #1992, #32650, #5012, #22963, #115, #25263, #566, #22640, #41075, #37957, #38914, #166, #9052, #41166, #17407, #31061, #11035, #18210, #20614, #16067, #15738, #5120, #4061, #40795, #16744, #6394, #39355, #39503, #20451, #10956, #37993, #7417, #9116, #10862, #7427, #10329, #43094, #9263, #17296, #24515, #22592, #13473, #34405, #44844, #27686, #38830, #1960, #38727, #17954, #42796, #6836, #32359, #7212, #3246, #9514 ) ) ;
#29324 = ORIENTED_EDGE ( 'NONE', *, *, #2109, .F. ) ;
#29325 = EDGE_CURVE ( 'NONE', #43175, #3655, #47111, .T. ) ;
#29326 = CARTESIAN_POINT ( 'NONE',  ( -0.9412147342319837628, -0.1574803149606297803, 1.144192913385827737 ) ) ;
#29327 = ADVANCED_FACE ( 'NONE', ( #46717 ), #13216, .T. ) ;
#29328 = CARTESIAN_POINT ( 'NONE',  ( 0.07405724077823318263, -0.8395669290800948925, -0.1787899950787401604 ) ) ;
#29329 = DIRECTION ( 'NONE',  ( 0.000000000000000000, 0.7880107536067206819, -0.6156614753256598460 ) ) ;
#29330 = CARTESIAN_POINT ( 'NONE',  ( 0.4755220087074803481, 4.766607801171850497E-17, 0.000000000000000000 ) ) ;
#29331 = CARTESIAN_POINT ( 'NONE',  ( 0.6971942568897648851, 0.07405724077823318263, 1.771653543253322249 ) ) ;
#29332 = CARTESIAN_POINT ( 'NONE',  ( 1.054774247047244540, -0.07405724077823318263, 0.2952755904974176393 ) ) ;
#29333 = CARTESIAN_POINT ( 'NONE',  ( 0.7185039370078739607, 1.928577636452523993E-17, 0.3051181102362204856 ) ) ;
#29334 = CARTESIAN_POINT ( 'NONE',  ( -0.07444174185955065859, -0.1658902662759589863, -0.1797182628040039087 ) ) ;
#29335 = ADVANCED_FACE ( 'NONE', ( #31194 ), #41924, .T. ) ;
#29336 = CARTESIAN_POINT ( 'NONE',  ( -0.07405724077823318263, -0.1270924721662466672, 0.1787899950787401604 ) ) ;
#29337 = CARTESIAN_POINT ( 'NONE',  ( -0.1787899950787401882, -0.3154527558517483676, 0.000000000000000000 ) ) ;
#29338 = CARTESIAN_POINT ( 'NONE',  ( 0.1787899950787401604, -0.1062992125446616531, 0.07405724077823318263 ) ) ;
#29339 = CARTESIAN_POINT ( 'NONE',  ( 0.2471911387363326384, -0.08795568039105847169, -0.05508755932581143461 ) ) ;
#29340 = EDGE_CURVE ( 'NONE', #23379, #40935, #27541, .T. ) ;
#29341 = CARTESIAN_POINT ( 'NONE',  ( 0.9500414927467378812, -0.1787899950787401604, 0.5659448818360001132 ) ) ;
#29343 = DIRECTION ( 'NONE',  ( -1.000000000000000000, 0.000000000000000000, 0.000000000000000000 ) ) ;
#29342 = DIRECTION ( 'NONE',  ( 0.000000000000000000, -1.000000000000000000, 0.000000000000000000 ) ) ;
#29344 = CARTESIAN_POINT ( 'NONE',  ( -0.8759842519685039353, 0.000000000000000000, 2.007874015640504162 ) ) ;
#29345 = CARTESIAN_POINT ( 'NONE',  ( 0.7185039370078739607, 1.928577636452523993E-17, 1.683070866141732402 ) ) ;
#29346 = CARTESIAN_POINT ( 'NONE',  ( 1.002407869896990045, 0.1264236179284866091, 1.646161417269070837 ) ) ;
#29348 = CARTESIAN_POINT ( 'NONE',  ( 0.000000000000000000, 0.000000000000000000, -0.01478361295688420882 ) ) ;
#29347 = CARTESIAN_POINT ( 'NONE',  ( -0.1878058820398608997, -0.07958416565558186495, 0.1770032286857264603 ) ) ;
#29349 = ( GEOMETRIC_REPRESENTATION_CONTEXT ( 3 ) GLOBAL_UNCERTAINTY_ASSIGNED_CONTEXT ( ( #26502 ) ) GLOBAL_UNIT_ASSIGNED_CONTEXT ( ( #15376, #18943, #37393 ) ) REPRESENTATION_CONTEXT ( 'NONE', 'WORKASPACE' ) ) ;
#29350 = AXIS2_PLACEMENT_3D ( 'NONE', #24179, #7766, #36774 ) ;
#29351 = ORIENTED_EDGE ( 'NONE', *, *, #6330, .T. ) ;
#29352 = CARTESIAN_POINT ( 'NONE',  ( 0.7185039370078739607, 1.928577636452523993E-17, 1.830708661309795149 ) ) ;
#29353 = CARTESIAN_POINT ( 'NONE',  ( 0.1564636162838602407, -0.1358284121151820956, 0.04551197418441456366 ) ) ;
#29354 = CARTESIAN_POINT ( 'NONE',  ( 0.1264236179284866091, -0.2268700786863941110, 0.1264236179284866091 ) ) ;
#29355 = CARTESIAN_POINT ( 'NONE',  ( 0.8107537697050254399, 0.1574803149606300301, 0.4847440943806614055 ) ) ;
#29356 = CARTESIAN_POINT ( 'NONE',  ( 0.07405724077823318263, -1.129921259788756682, 0.1787899950787401604 ) ) ;
#29357 = DIRECTION ( 'NONE',  ( 0.000000000000000000, 0.000000000000000000, -1.000000000000000000 ) ) ;
#29358 = CARTESIAN_POINT ( 'NONE',  ( 1.033464566929133799, 0.000000000000000000, 0.04921259842519685318 ) ) ;
#29359 = CARTESIAN_POINT ( 'NONE',  ( -0.8759842519685039353, -0.1787899950787401882, 1.665846456639149764 ) ) ;
#29360 = ORIENTED_EDGE ( 'NONE', *, *, #6873, .F. ) ;
#29361 = CIRCLE ( 'NONE', #9400, 0.1013779527559039162 ) ;
#29362 = CARTESIAN_POINT ( 'NONE',  ( -0.9500414927467378812, 0.1787899950787401604, 1.136811023568283119 ) ) ;
#29363 = DIRECTION ( 'NONE',  ( 1.000000000000000000, 0.000000000000000000, -1.822029033848725275E-16 ) ) ;
#29364 = CARTESIAN_POINT ( 'NONE',  ( 0.6971942568897648851, 0.07405724077823318263, 1.186023621993481658 ) ) ;
#29365 = CARTESIAN_POINT ( 'NONE',  ( 0.1574803149606300301, -1.142224409341292768, 0.06523048226347956391 ) ) ;
#29366 = CARTESIAN_POINT ( 'NONE',  ( 0.7495606340400177148, -0.1264236179284866091, 1.975885826717889815 ) ) ;
#29367 = CARTESIAN_POINT ( 'NONE',  ( -1.033464566929134687, 0.06523048226347956391, 0.6422244094488182009 ) ) ;
#29368 = CARTESIAN_POINT ( 'NONE',  ( -1.054774247047244540, 0.07405724077823318263, 1.008858267662772423 ) ) ;
#29369 = CARTESIAN_POINT ( 'NONE',  ( 0.1587072800413000528, 0.1005018865549645452, -0.1068311739851162540 ) ) ;
#29370 = CARTESIAN_POINT ( 'NONE',  ( 0.1574803149606299746, -5.122214988120488358E-16, -8.878505979408856939E-16 ) ) ;
#29371 = CARTESIAN_POINT ( 'NONE',  ( 0.6971942568897626646, -0.07405724077823297447, 0.2854330708123783977 ) ) ;
#29372 = CARTESIAN_POINT ( 'NONE',  ( -1.054774247047244540, -0.07405724077823318263, 0.1771653542769450751 ) ) ;
#29373 = PRODUCT_DEFINITION_CONTEXT ( 'detailed design', #13765, 'design' ) ;
#29374 = CARTESIAN_POINT ( 'NONE',  ( -0.7495606340400177148, -0.1264236179284866091, 0.7554133857730077617 ) ) ;
#29375 = ORIENTED_EDGE ( 'NONE', *, *, #19965, .T. ) ;
#29376 = CARTESIAN_POINT ( 'NONE',  ( 0.07405724077823318263, -0.01771653537930735142, -0.1787899950787401604 ) ) ;
#29377 = CARTESIAN_POINT ( 'NONE',  ( 0.9500414927467378812, -0.1787899950787401604, 0.7283464566391493200 ) ) ;
#29378 = CARTESIAN_POINT ( 'NONE',  ( 0.8019270111902716547, 0.1787899950787401604, 1.023622047190330342 ) ) ;
#29379 = CARTESIAN_POINT ( 'NONE',  ( -1.054774247047244540, 0.07405724077823318263, 1.874999999946236784 ) ) ;
#29380 = VERTEX_POINT ( 'NONE', #42635 ) ;
#29381 = AXIS2_PLACEMENT_3D ( 'NONE', #10667, #16960, #31830 ) ;
#29382 = CARTESIAN_POINT ( 'NONE',  ( 1.033464566929134687, -0.06523048226347956391, 1.611712598317669221 ) ) ;
#29383 = CARTESIAN_POINT ( 'NONE',  ( -0.1787899950787401604, -1.273746015473333992, 0.07405724077823318263 ) ) ;
#29384 = ORIENTED_EDGE ( 'NONE', *, *, #1444, .T. ) ;
#29385 = CARTESIAN_POINT ( 'NONE',  ( -1.094772975963752103E-17, -0.3252952755367877757, -0.1787899950787401882 ) ) ;
#29386 = ORIENTED_EDGE ( 'NONE', *, *, #41029, .T. ) ;
#29387 = CARTESIAN_POINT ( 'NONE',  ( 1.054774247047244540, -0.07405724077823318263, 1.240157480261197431 ) ) ;
#29388 = CIRCLE ( 'NONE', #38524, 0.09842519685039370636 ) ;
#29389 = CARTESIAN_POINT ( 'NONE',  ( 1.284448818897637956, -0.3937007874015748254, -1.181102362204724310 ) ) ;
#29390 = CARTESIAN_POINT ( 'NONE',  ( -0.2471883443660232993, -0.06218794471711499433, 0.1039611462668204589 ) ) ;
#29391 = EDGE_CURVE ( 'NONE', #9619, #29926, #37301, .T. ) ;
#29392 = CARTESIAN_POINT ( 'NONE',  ( 0.7185039370078739607, 1.928577636452523993E-17, 1.958661417322834719 ) ) ;
#29393 = CARTESIAN_POINT ( 'NONE',  ( 0.1787899950787401604, -1.597440944828127485, -0.07405724077823318263 ) ) ;
#29394 = CARTESIAN_POINT ( 'NONE',  ( -0.07405724077823318263, -1.725393700733637958, 0.1787899950787401604 ) ) ;
#29395 = ADVANCED_FACE ( 'NONE', ( #9377, #42169, #35263 ), #21083, .T. ) ;
#29396 = ( BOUNDED_CURVE ( )  B_SPLINE_CURVE ( 2, ( #30334, #25541, #15455, #44177, #22863, #26479, #18553, #40110, #29865 ),
 .UNSPECIFIED., .F., .F. ) 
 B_SPLINE_CURVE_WITH_KNOTS ( ( 3, 2, 2, 2, 3 ),
 ( 0.5100000000000000089, 0.5124999999999999556, 0.5150000000000000133, 0.5174999999999999600, 0.5200000000000000178 ),
 .UNSPECIFIED. ) 
 CURVE ( )  GEOMETRIC_REPRESENTATION_ITEM ( )  RATIONAL_B_SPLINE_CURVE ( ( 1.000000000000000000, 0.9238795325112869605, 1.000000000000000000, 0.9238795325112869605, 1.000000000000000000, 0.9238795325112869605, 1.000000000000000000, 0.9238795325112869605, 1.000000000000000000 ) ) 
 REPRESENTATION_ITEM ( '' )  ) ;
#29397 = CARTESIAN_POINT ( 'NONE',  ( -0.8019270111902716547, -0.1787899950787401604, 0.5659448818360001132 ) ) ;
#29398 = CARTESIAN_POINT ( 'NONE',  ( -0.08595198851647926908, -0.09842519685039370636, 0.1380468394703990020 ) ) ;
#29399 = CARTESIAN_POINT ( 'NONE',  ( -0.1797182628040039365, -1.457720974937376068, 0.000000000000000000 ) ) ;
#29400 = CARTESIAN_POINT ( 'NONE',  ( 0.1498753904841984286, -0.1193342091828950846, 0.06889763779527559306 ) ) ;
#29401 = CARTESIAN_POINT ( 'NONE',  ( 0.6971942568897648851, -0.07405724077823297447, 1.230314960576156746 ) ) ;
#29402 = CARTESIAN_POINT ( 'NONE',  ( 0.7495606340400177148, -0.1264236179284866091, 1.621555118056472455 ) ) ;
#29403 = DIRECTION ( 'NONE',  ( 0.000000000000000000, 0.000000000000000000, 1.000000000000000000 ) ) ;
#29404 = AXIS2_PLACEMENT_3D ( 'NONE', #39521, #18206, #14384 ) ;
#29405 = DIRECTION ( 'NONE',  ( -1.000000000000000000, -0.000000000000000000, -0.000000000000000000 ) ) ;
#29406 = DIRECTION ( 'NONE',  ( 1.000000000000000000, 0.000000000000000000, -1.822029033848725275E-16 ) ) ;
#29407 = FACE_OUTER_BOUND ( 'NONE', #29497, .T. ) ;
#29408 = CARTESIAN_POINT ( 'NONE',  ( -1.033464566929133799, 1.928577636452524610E-17, 2.869337061179095023E-17 ) ) ;
#29409 = CARTESIAN_POINT ( 'NONE',  ( 1.054774247047244540, -0.07405724077823318263, 0.2559055117572600624 ) ) ;
#29410 = CARTESIAN_POINT ( 'NONE',  ( 0.7027234418073040612, -0.01298421436181104380, 0.03936972784119035368 ) ) ;
#29412 = CARTESIAN_POINT ( 'NONE',  ( 0.000000000000000000, 0.000000000000000000, -0.2357204724409448504 ) ) ;
#29411 = CARTESIAN_POINT ( 'NONE',  ( 1.002407869896990045, -0.1264236179284866091, 1.277066929080094448 ) ) ;
#29413 = CARTESIAN_POINT ( 'NONE',  ( -0.7646288533564489232, -0.1113553986120547346, 1.914370078632629868 ) ) ;
#29414 = LINE ( 'NONE', #11859, #16189 ) ;
#29415 = CARTESIAN_POINT ( 'NONE',  ( 0.7646288533564489232, 0.1113553986120547346, 0.7234251967428662056 ) ) ;
#29416 = ORIENTED_EDGE ( 'NONE', *, *, #28594, .T. ) ;
#29417 = ( NAMED_UNIT ( * ) PLANE_ANGLE_UNIT ( ) SI_UNIT ( $, .RADIAN. ) ) ;
#29418 = CARTESIAN_POINT ( 'NONE',  ( 0.9316794993730774799, 0.1616194352551858504, 0.03936999175310366972 ) ) ;
#29419 = VECTOR ( 'NONE', #18888, 39.37007874015748854 ) ;
#29420 = CARTESIAN_POINT ( 'NONE',  ( -0.9873396505805591694, 0.1113553986120547346, 1.107283464459401623 ) ) ;
#29421 = CARTESIAN_POINT ( 'NONE',  ( 0.8759842519685039353, 0.1787899950787401882, 1.488681102308440751 ) ) ;
#29423 = LINE ( 'NONE', #28925, #40712 ) ;
#29422 = CARTESIAN_POINT ( 'NONE',  ( -0.7646288533564489232, 0.1113553986120547346, 1.835629921259842590 ) ) ;
#29424 = CARTESIAN_POINT ( 'NONE',  ( -0.8019270111902716547, 0.1787899950787401604, 0.07381889758403178958 ) ) ;
#29425 = CARTESIAN_POINT ( 'NONE',  ( 0.1787899950787401604, -0.2194881889226144023, 0.07405724077823318263 ) ) ;
#29426 = ORIENTED_EDGE ( 'NONE', *, *, #39349, .F. ) ;
#29427 = DIRECTION ( 'NONE',  ( 0.000000000000000000, -1.000000000000000000, 0.000000000000000000 ) ) ;
#29428 = ( BOUNDED_CURVE ( )  B_SPLINE_CURVE ( 2, ( #7385, #44023, #8078, #22218, #15534, #33043, #170, #22456, #21994 ),
 .UNSPECIFIED., .F., .T. ) 
 B_SPLINE_CURVE_WITH_KNOTS ( ( 3, 2, 2, 2, 3 ),
 ( 0.3499999999999999778, 0.3524999999999999800, 0.3549999999999999822, 0.3574999999999999845, 0.3599999999999999867 ),
 .UNSPECIFIED. ) 
 CURVE ( )  GEOMETRIC_REPRESENTATION_ITEM ( )  RATIONAL_B_SPLINE_CURVE ( ( 1.000000000000000000, 0.9238795325112879597, 1.000000000000000000, 0.9238795325112869605, 1.000000000000000000, 0.9238795325112869605, 1.000000000000000000, 0.9238795325112869605, 1.000000000000000000 ) ) 
 REPRESENTATION_ITEM ( '' )  ) ;
#29429 = CARTESIAN_POINT ( 'NONE',  ( -9.642888182262618425E-18, 0.08070866141732284393, -0.1574803149606299191 ) ) ;
#29430 = CARTESIAN_POINT ( 'NONE',  ( -0.1235961452251413406, 0.09842519685039370636, 0.2140748031496062798 ) ) ;
#29431 = CARTESIAN_POINT ( 'NONE',  ( 0.7495606340400177148, -0.1264236179284866091, 0.5241141731745827537 ) ) ;
#29432 = ORIENTED_EDGE ( 'NONE', *, *, #29325, .F. ) ;
#29433 = CARTESIAN_POINT ( 'NONE',  ( -1.054774247047244540, -0.07405724077823318263, 1.437007873961985593 ) ) ;
#29434 = CARTESIAN_POINT ( 'NONE',  ( -0.06523048226347956391, 0.05364173239099160467, -0.1574803149606300301 ) ) ;
#29435 = CARTESIAN_POINT ( 'NONE',  ( -1.054774247047244540, -0.07405724077823318263, 1.166338582623402509 ) ) ;
#29436 = ORIENTED_EDGE ( 'NONE', *, *, #8423, .T. ) ;
#29437 = CARTESIAN_POINT ( 'NONE',  ( 0.9412147342319837628, 0.1574803149606300301, 1.306594488081449290 ) ) ;
#29438 = CARTESIAN_POINT ( 'NONE',  ( -1.033464566929133799, 1.928577636452524610E-17, 2.869337061179095023E-17 ) ) ;
#29439 = CARTESIAN_POINT ( 'NONE',  ( -1.094772975963752103E-17, -0.8923483776780569698, -0.1787899950787401882 ) ) ;
#29440 = EDGE_LOOP ( 'NONE', ( #33247, #10575, #24014, #14783 ) ) ;
#29441 = CARTESIAN_POINT ( 'NONE',  ( 0.9412147342319837628, -0.1574803149606297803, 1.065452755905511806 ) ) ;
#29442 = APPLICATION_CONTEXT ( 'automotive_design' ) ;
#29443 = EDGE_LOOP ( 'NONE', ( #1588, #13076 ) ) ;
#29444 = CARTESIAN_POINT ( 'NONE',  ( -1.033464566929134687, 0.06523048226347956391, 0.5536417321759372623 ) ) ;
#29445 = CARTESIAN_POINT ( 'NONE',  ( -1.002407869896990045, 0.1264236179284866091, 0.7357283464029290565 ) ) ;
#29446 = CARTESIAN_POINT ( 'NONE',  ( 0.3849708276051176936, 4.766607801171850497E-17, 0.000000000000000000 ) ) ;
#29447 = EDGE_CURVE ( 'NONE', #2867, #43605, #17543, .T. ) ;
#29448 = CARTESIAN_POINT ( 'NONE',  ( -0.9500414927467377701, -0.1787899950787401604, 1.870078740103715331 ) ) ;
#29449 = EDGE_CURVE ( 'NONE', #22273, #40732, #15645, .T. ) ;
#29450 = CARTESIAN_POINT ( 'NONE',  ( -0.1574803149606299191, 0.09445121742700228473, -0.1242805304366905728 ) ) ;
#29451 = CARTESIAN_POINT ( 'NONE',  ( 0.7185039370078739607, 1.928577636452523993E-17, 0.6594488188976378451 ) ) ;
#29452 = CARTESIAN_POINT ( 'NONE',  ( -0.1797182628040039087, -0.9090005024964308289, -0.07444174185955065859 ) ) ;
#29453 = CARTESIAN_POINT ( 'NONE',  ( -0.9412147342319837628, 0.1574803149606300301, 0.4010826770578274081 ) ) ;
#29454 = CARTESIAN_POINT ( 'NONE',  ( -0.8107537697050253289, 0.1574803149606300301, 1.547736220364914983 ) ) ;
#29455 = CIRCLE ( 'NONE', #4136, 0.1003937007874010356 ) ;
#29456 = CARTESIAN_POINT ( 'NONE',  ( 0.7495606340400177148, -0.1264236179284866091, 0.7603346456155274380 ) ) ;
#29457 = CARTESIAN_POINT ( 'NONE',  ( 1.002407869896990045, 0.1264236179284866091, 1.326279527505291433 ) ) ;
#29458 = DIRECTION ( 'NONE',  ( -2.943801717310650128E-16, 1.000000000000000000, 2.197428715927220134E-15 ) ) ;
#29459 = CARTESIAN_POINT ( 'NONE',  ( 0.7646288533564489232, -0.1113553986120547346, 1.373031496062992352 ) ) ;
#29461 = DIRECTION ( 'NONE',  ( 1.000000000000000000, 0.000000000000000000, 0.000000000000000000 ) ) ;
#29460 = CARTESIAN_POINT ( 'NONE',  ( 0.9893677384800499963, -0.1382549923011644755, 1.990360131067286487 ) ) ;
#29462 = DIRECTION ( 'NONE',  ( 0.000000000000000000, -1.000000000000000000, 0.000000000000000000 ) ) ;
#29463 = CARTESIAN_POINT ( 'NONE',  ( -0.1574803149606300301, -0.6500984250893240279, -0.06523048226347956391 ) ) ;
#29464 = CARTESIAN_POINT ( 'NONE',  ( 1.054774247047244540, -0.07405724077823318263, 0.7677165353793073965 ) ) ;
#29465 = CARTESIAN_POINT ( 'NONE',  ( -0.1264236179284866091, -0.7534448818360000022, -0.1264236179284866091 ) ) ;
#29466 = CARTESIAN_POINT ( 'NONE',  ( 0.2395294000716133853, 0.1968503937007874127, -0.4921259842519684069 ) ) ;
#29467 = ORIENTED_EDGE ( 'NONE', *, *, #23390, .F. ) ;
#29468 = CARTESIAN_POINT ( 'NONE',  ( 0.1629747151064184774, 0.08009231510251769992, 0.1387240349198020917 ) ) ;
#29469 = CARTESIAN_POINT ( 'NONE',  ( -0.1574803149606299191, 0.000000000000000000, -0.1574803149606298636 ) ) ;
#29470 = CARTESIAN_POINT ( 'NONE',  ( 1.054774247047244540, -0.07405724077823318263, 0.9251968503399374821 ) ) ;
#29471 = CARTESIAN_POINT ( 'NONE',  ( 0.7185039370078739607, 1.928577636452523993E-17, 1.643700787401574992 ) ) ;
#29472 = CARTESIAN_POINT ( 'NONE',  ( 0.1574803149606300301, -1.703248031496063408, 0.06523048226347956391 ) ) ;
#29473 = EDGE_CURVE ( 'NONE', #5973, #18563, #15273, .T. ) ;
#29474 = DIRECTION ( 'NONE',  ( -1.000000000000000000, 0.000000000000000000, -6.938893903907220489E-15 ) ) ;
#29475 = ORIENTED_EDGE ( 'NONE', *, *, #4758, .F. ) ;
#29477 = LINE ( 'NONE', #36845, #23698 ) ;
#29476 = VECTOR ( 'NONE', #8211, 39.37007874015748143 ) ;
#29478 = CARTESIAN_POINT ( 'NONE',  ( -0.7495606340400177148, 0.1264236179284866091, 0.1550196849856066983 ) ) ;
#29479 = ORIENTED_EDGE ( 'NONE', *, *, #4304, .F. ) ;
#29480 = CARTESIAN_POINT ( 'NONE',  ( 0.8759842519685039353, 0.1574803149606299191, 1.751968503937007871 ) ) ;
#29481 = AXIS2_PLACEMENT_3D ( 'NONE', #34414, #842, #11903 ) ;
#29482 = VECTOR ( 'NONE', #40921, 39.37007874015748143 ) ;
#29483 = CARTESIAN_POINT ( 'NONE',  ( -0.8019270111902717657, -0.1787899950787401604, 1.624015747977732849 ) ) ;
#29484 = CARTESIAN_POINT ( 'NONE',  ( -0.8019270111902716547, -0.1787899950787401604, 0.8366141731745828647 ) ) ;
#29485 = CARTESIAN_POINT ( 'NONE',  ( -0.6971942568897626646, 0.07405724077823318263, 0.3592519684501735977 ) ) ;
#29486 = DIRECTION ( 'NONE',  ( 0.000000000000000000, 0.000000000000000000, -1.000000000000000000 ) ) ;
#29487 = CARTESIAN_POINT ( 'NONE',  ( 0.7185039370078739607, 1.928577636452523993E-17, 0.4133858266641267654 ) ) ;
#29488 = CARTESIAN_POINT ( 'NONE',  ( -0.7646288533564489232, 0.1113553986120547346, 0.3297244093412917687 ) ) ;
#29489 = CARTESIAN_POINT ( 'NONE',  ( 0.05557684098944757484, 0.07733267719194691914, -0.2533457667601751173 ) ) ;
#29490 = AXIS2_PLACEMENT_3D ( 'NONE', #45848, #13055, #8727 ) ;
#29491 = CARTESIAN_POINT ( 'NONE',  ( -0.2896200801440089734, 0.1109568837733818092, -0.7502863005648467976 ) ) ;
#29492 = CARTESIAN_POINT ( 'NONE',  ( -0.07405724077823318263, -0.3387066453945931643, -0.1787899950787401604 ) ) ;
#29493 = CARTESIAN_POINT ( 'NONE',  ( 0.1110370215561167356, -0.09842519685039370636, 0.09588239823699959419 ) ) ;
#29494 = DIRECTION ( 'NONE',  ( 1.000000000000000000, 0.000000000000000000, 0.000000000000000000 ) ) ;
#29495 = CARTESIAN_POINT ( 'NONE',  ( -1.054774247047244096, 0.000000000000000000, 0.3764763778989925203 ) ) ;
#29496 = EDGE_CURVE ( 'NONE', #15230, #20344, #22044, .T. ) ;
#29497 = EDGE_LOOP ( 'NONE', ( #8827, #12128, #14835, #21820 ) ) ;
#29498 = ORIENTED_EDGE ( 'NONE', *, *, #13085, .F. ) ;
#29499 = CARTESIAN_POINT ( 'NONE',  ( -1.002407869896990045, -0.1264236179284866091, 1.439468503883244210 ) ) ;
#29500 = ORIENTED_EDGE ( 'NONE', *, *, #31084, .F. ) ;
#29501 = EDGE_CURVE ( 'NONE', #31518, #36286, #20619, .T. ) ;
#29502 = CARTESIAN_POINT ( 'NONE',  ( 0.1787899950787401604, -1.400590551127339323, -0.07405724077823318263 ) ) ;
#29503 = CARTESIAN_POINT ( 'NONE',  ( 0.1787899950787401882, -1.437499999946236340, -2.189545951927503898E-17 ) ) ;
#29504 = CYLINDRICAL_SURFACE ( 'NONE', #36328, 0.1574803149606299191 ) ;
#29505 = CARTESIAN_POINT ( 'NONE',  ( -2.859251968503937036, 0.000000000000000000, 0.000000000000000000 ) ) ;
#29506 = CARTESIAN_POINT ( 'NONE',  ( 0.8759842519685039353, 0.1574803149606299191, 0.3740157480314960647 ) ) ;
#29507 = VECTOR ( 'NONE', #44385, 39.37007874015748143 ) ;
#29508 = LINE ( 'NONE', #29272, #39288 ) ;
#29509 = CARTESIAN_POINT ( 'NONE',  ( -0.7185039370078739607, 1.928577636452523993E-17, 1.122047243986960652 ) ) ;
#29510 = CARTESIAN_POINT ( 'NONE',  ( 0.8107537697050254399, 0.1574803149606300301, 0.5634842518609766149 ) ) ;
#29511 = CARTESIAN_POINT ( 'NONE',  ( -0.1574803149606300301, -0.3449803149606298636, -0.06523048226347956391 ) ) ;
#29512 = TOROIDAL_SURFACE ( 'NONE', #33316, 0.03937007874015747977, 0.009842519685039369942 ) ;
#29513 = AXIS2_PLACEMENT_3D ( 'NONE', #42655, #2879, #40017 ) ;
#29514 = CARTESIAN_POINT ( 'NONE',  ( 0.000000000000000000, 0.000000000000000000, 0.000000000000000000 ) ) ;
#29515 = DIRECTION ( 'NONE',  ( -0.8660254037844389297, 0.000000000000000000, 0.4999999999999994449 ) ) ;
#29516 = CARTESIAN_POINT ( 'NONE',  ( 0.8759842519685039353, 0.1574803149606299191, 0.8858267716535432879 ) ) ;
#29517 = CARTESIAN_POINT ( 'NONE',  ( 0.8107537697050254399, 0.1574803149606300301, 1.360728346456693050 ) ) ;
#29519 = DIRECTION ( 'NONE',  ( -1.000000000000000000, 0.000000000000000000, 0.000000000000000000 ) ) ;
#29518 = PLANE ( 'NONE',  #1036 ) ;
#29520 = ORIENTED_EDGE ( 'NONE', *, *, #28067, .T. ) ;
#29521 = CARTESIAN_POINT ( 'NONE',  ( -0.1574803149606300301, 0.09793307097366883707, -0.06523048226347956391 ) ) ;
#29522 = CARTESIAN_POINT ( 'NONE',  ( -1.094772975963752103E-17, -1.585137795221826629, -0.1787899950787401882 ) ) ;
#29523 = CARTESIAN_POINT ( 'NONE',  ( -0.1113553986120547346, -1.469488188868850465, 0.1113553986120547346 ) ) ;
#29524 = CARTESIAN_POINT ( 'NONE',  ( -0.1264236179284866091, -0.7977362204186770889, -0.1264236179284866091 ) ) ;
#29525 = CARTESIAN_POINT ( 'NONE',  ( -0.1574803149606299191, -1.090551181102362266, 0.000000000000000000 ) ) ;
#29526 = CARTESIAN_POINT ( 'NONE',  ( 0.7646288533564489232, -0.1113553986120547346, 1.008858267609007875 ) ) ;
#29527 = ( BOUNDED_CURVE ( )  B_SPLINE_CURVE ( 2, ( #46533, #43168, #13715, #47256, #36253, #10373, #39102, #40041, #6515 ),
 .UNSPECIFIED., .F., .F. ) 
 B_SPLINE_CURVE_WITH_KNOTS ( ( 3, 2, 2, 2, 3 ),
 ( 0.8399999999999999689, 0.8425000000000000266, 0.8449999999999999734, 0.8475000000000000311, 0.8499999999999999778 ),
 .UNSPECIFIED. ) 
 CURVE ( )  GEOMETRIC_REPRESENTATION_ITEM ( )  RATIONAL_B_SPLINE_CURVE ( ( 1.000000000000000000, 0.9238795325112869605, 1.000000000000000000, 0.9238795325112869605, 1.000000000000000000, 0.9238795325112869605, 1.000000000000000000, 0.9238795325112799661, 1.000000000000000000 ) ) 
 REPRESENTATION_ITEM ( '' )  ) ;
#29528 = DIRECTION ( 'NONE',  ( 1.000000000000000000, 0.000000000000000000, 0.000000000000000000 ) ) ;
#29529 = VERTEX_POINT ( 'NONE', #25661 ) ;
#29530 = VERTEX_POINT ( 'NONE', #14395 ) ;
#29531 = ORIENTED_EDGE ( 'NONE', *, *, #4859, .F. ) ;
#29532 = CARTESIAN_POINT ( 'NONE',  ( -0.8759842519685039353, -0.1787899950787401882, 1.552657480261196765 ) ) ;
#29533 = ORIENTED_EDGE ( 'NONE', *, *, #847, .F. ) ;
#29534 = CARTESIAN_POINT ( 'NONE',  ( 1.002407869896990045, 0.1264236179284866091, 1.764271653489543290 ) ) ;
#29535 = CARTESIAN_POINT ( 'NONE',  ( -0.7495606340400177148, -0.1264236179284866091, 0.7603346456155274380 ) ) ;
#29536 = DIRECTION ( 'NONE',  ( -0.8191520442889873577, 1.003171929053519323E-16, 0.5735764363510523767 ) ) ;
#29537 = CARTESIAN_POINT ( 'NONE',  ( 0.8759842519685039353, -0.1787899950787401882, 0.3321850393163153226 ) ) ;
#29538 = DIRECTION ( 'NONE',  ( -0.000000000000000000, 1.000000000000000000, -0.000000000000000000 ) ) ;
#29539 = CARTESIAN_POINT ( 'NONE',  ( -0.9500414927467377701, 0.1787899950787401604, 1.249999999946235896 ) ) ;
#29540 = CARTESIAN_POINT ( 'NONE',  ( -0.8019270111902716547, 0.1787899950787401604, 0.7431102361667091261 ) ) ;
#29541 = CARTESIAN_POINT ( 'NONE',  ( 1.033464566929133799, 0.000000000000000000, 0.9055118109160944506 ) ) ;
#29542 = CARTESIAN_POINT ( 'NONE',  ( -0.7646288533564489232, 0.1113553986120547346, 1.668307086506645609 ) ) ;
#29543 = CARTESIAN_POINT ( 'NONE',  ( -0.7495606340400177148, 0.1264236179284866091, 1.537893700733637736 ) ) ;
#29544 = CARTESIAN_POINT ( 'NONE',  ( -1.033464566929134687, -0.06523048226347956391, 1.887303149498773092 ) ) ;
#29545 = ORIENTED_EDGE ( 'NONE', *, *, #44394, .T. ) ;
#29546 = CIRCLE ( 'NONE', #40951, 0.09940944881889761386 ) ;
#29547 = CARTESIAN_POINT ( 'NONE',  ( -0.7646288533564489232, 0.1113553986120547346, 1.560039370078740273 ) ) ;
#29548 = CARTESIAN_POINT ( 'NONE',  ( 0.8759842519685039353, 0.1574803149606299191, 1.633858267716535639 ) ) ;
#29549 = ADVANCED_FACE ( 'NONE', ( #6949 ), #11046, .T. ) ;
#29550 = CARTESIAN_POINT ( 'NONE',  ( 0.8759842519685039353, 0.1787899950787401882, 1.493602362150960650 ) ) ;
#29551 = CARTESIAN_POINT ( 'NONE',  ( -0.06938717807759606226, -0.09851383877177855020, -0.1728648718439755871 ) ) ;
#29552 = FACE_OUTER_BOUND ( 'NONE', #28578, .T. ) ;
#29553 = AXIS2_PLACEMENT_3D ( 'NONE', #38640, #46049, #38401 ) ;
#29554 = CIRCLE ( 'NONE', #39434, 0.1574803149606299191 ) ;
#29555 = ORIENTED_EDGE ( 'NONE', *, *, #34387, .F. ) ;
#29556 = ORIENTED_EDGE ( 'NONE', *, *, #30909, .T. ) ;
#29557 = SHAPE_REPRESENTATION_RELATIONSHIP ( 'NONE' , 'NONE' ,  #4677, #5636 ) ;
#29558 = ORIENTED_EDGE ( 'NONE', *, *, #2117, .F. ) ;
#29559 = EDGE_CURVE ( 'NONE', #3114, #10926, #42190, .T. ) ;
#29560 = CARTESIAN_POINT ( 'NONE',  ( -0.7185039370078766252, -0.06523048226348168721, 1.134350393700787940 ) ) ;
#29561 = CARTESIAN_POINT ( 'NONE',  ( -0.07405724077823318263, -0.4458661416785199560, -0.1787899950787401604 ) ) ;
#29562 = CARTESIAN_POINT ( 'NONE',  ( -0.07405724077823318263, -0.9379921259304876413, 0.1787899950787401604 ) ) ;
#29563 = EDGE_CURVE ( 'NONE', #23841, #4869, #45861, .T. ) ;
#29564 = CYLINDRICAL_SURFACE ( 'NONE', #1020, 0.09842519685039370636 ) ;
#29565 = ( NAMED_UNIT ( * ) PLANE_ANGLE_UNIT ( ) SI_UNIT ( $, .RADIAN. ) ) ;
#29566 = CARTESIAN_POINT ( 'NONE',  ( 0.8759842519685039353, 0.1787899950787401882, 1.764271653489543290 ) ) ;
#29567 = CARTESIAN_POINT ( 'NONE',  ( -0.1797182628040039087, -0.1166776678507620985, 0.07444174185955065859 ) ) ;
#29568 = PRODUCT_DEFINITION_SHAPE ( 'NONE', 'NONE',  #47465 ) ;
#29569 = DIRECTION ( 'NONE',  ( 7.083454193571959410E-15, 0.000000000000000000, 1.000000000000000000 ) ) ;
#29570 = CIRCLE ( 'NONE', #11953, 0.1864803149606299448 ) ;
#29571 = CARTESIAN_POINT ( 'NONE',  ( 0.9500414927467378812, -0.1787899950787401604, 0.7627952755367881643 ) ) ;
#29573 = DIRECTION ( 'NONE',  ( -1.000000000000000000, 0.000000000000000000, 0.000000000000000000 ) ) ;
#29572 = CARTESIAN_POINT ( 'NONE',  ( 0.1574803149606299746, -0.5708661417322835607, -6.991093932140394160E-17 ) ) ;
#29574 = DIRECTION ( 'NONE',  ( 0.000000000000000000, -0.6156614753256597350, -0.7880107536067207930 ) ) ;
#29575 = DIRECTION ( 'NONE',  ( 0.000000000000000000, -1.000000000000000000, 0.000000000000000000 ) ) ;
#29576 = CARTESIAN_POINT ( 'NONE',  ( 1.054774247047244540, 0.07405724077823318263, 1.879921259788756016 ) ) ;
#29578 = DIRECTION ( 'NONE',  ( 1.000000000000000000, 0.000000000000000000, 0.000000000000000000 ) ) ;
#29577 = DIRECTION ( 'NONE',  ( -0.000000000000000000, -1.000000000000000000, -0.000000000000000000 ) ) ;
#29579 = CARTESIAN_POINT ( 'NONE',  ( 0.6971942568897648851, -0.07405724077823297447, 0.4773622046706456068 ) ) ;
#29580 = AXIS2_PLACEMENT_3D ( 'NONE', #13146, #27782, #42342 ) ;
#29581 = AXIS2_PLACEMENT_3D ( 'NONE', #1077, #15740, #34187 ) ;
#29582 = VERTEX_POINT ( 'NONE', #47213 ) ;
#29583 = CARTESIAN_POINT ( 'NONE',  ( 0.7646288533564489232, 0.1113553986120547346, 0.1033464566929133965 ) ) ;
#29584 = DIRECTION ( 'NONE',  ( 0.000000000000000000, -1.000000000000000000, 0.000000000000000000 ) ) ;
#29586 = CARTESIAN_POINT ( 'NONE',  ( -0.07405724077823318263, -0.2883858267178899260, -0.1787899950787401604 ) ) ;
#29585 = CARTESIAN_POINT ( 'NONE',  ( -0.1113553986120547346, -0.9576771652468032414, 0.1113553986120547346 ) ) ;
#29588 = CARTESIAN_POINT ( 'NONE',  ( 0.8759842519685039353, 0.1574803149606299191, 0.4822834644594015674 ) ) ;
#29587 = CARTESIAN_POINT ( 'NONE',  ( -0.8019270111902717657, -0.1787899950787401604, 0.4872047243556847929 ) ) ;
#29589 = CARTESIAN_POINT ( 'NONE',  ( -0.07405724077823318263, -1.095472440891117838, 0.1787899950787401604 ) ) ;
#29590 = CARTESIAN_POINT ( 'NONE',  ( 0.8759842519685039353, 0.1787899950787401882, 0.3124999999462365619 ) ) ;
#29591 = CARTESIAN_POINT ( 'NONE',  ( 0.7185039370078739607, 1.928577636452523993E-17, 1.122047243986960652 ) ) ;
#29592 = CARTESIAN_POINT ( 'NONE',  ( -1.002407869896990045, 0.1264236179284866091, 1.562499999946236118 ) ) ;
#29593 = ORIENTED_EDGE ( 'NONE', *, *, #7682, .F. ) ;
#29594 = CARTESIAN_POINT ( 'NONE',  ( -0.6971942568897648851, 0.07405724077823318263, 1.225393700733637514 ) ) ;
#29595 = CARTESIAN_POINT ( 'NONE',  ( 0.1574803149606299746, -0.5708661417322837828, 2.134496832518260172E-17 ) ) ;
#29596 = CARTESIAN_POINT ( 'NONE',  ( 1.002407869896990045, 0.1264236179284866091, 1.252460629867496067 ) ) ;
#29597 = CARTESIAN_POINT ( 'NONE',  ( -0.8019270111902717657, 0.1787899950787401604, 0.9793307086076531442 ) ) ;
#29598 = ADVANCED_FACE ( 'NONE', ( #11274 ), #7193, .T. ) ;
#29599 = DIRECTION ( 'NONE',  ( 0.000000000000000000, -1.000000000000000000, 0.000000000000000000 ) ) ;
#29600 = CARTESIAN_POINT ( 'NONE',  ( -0.1339681929923939863, -0.2181476599754015588, -0.02739586109245887441 ) ) ;
#29601 = CARTESIAN_POINT ( 'NONE',  ( 1.054774247047244096, 0.000000000000000000, 0.2632874015210397434 ) ) ;
#29602 = CARTESIAN_POINT ( 'NONE',  ( -0.6971942568897626646, 0.07405724077823318263, 0.2362204723871814682 ) ) ;
#29603 = CARTESIAN_POINT ( 'NONE',  ( -0.8759842519685039353, -0.1787899950787401882, 0.6815944881352126172 ) ) ;
#29604 = CARTESIAN_POINT ( 'NONE',  ( 0.7646288533564489232, 0.1113553986120547346, 1.707677165246803241 ) ) ;
#29605 = EDGE_LOOP ( 'NONE', ( #44369, #16597 ) ) ;
#29606 = EDGE_CURVE ( 'NONE', #3438, #37269, #21088, .T. ) ;
#29607 = CARTESIAN_POINT ( 'NONE',  ( -0.9873396505805591694, 0.1113553986120547346, 1.353346456692913424 ) ) ;
#29608 = VERTEX_POINT ( 'NONE', #17499 ) ;
#29609 = EDGE_CURVE ( 'NONE', #24716, #37198, #40000, .T. ) ;
#29610 = CARTESIAN_POINT ( 'NONE',  ( -0.9500414927467377701, 0.1787899950787401604, 1.801181102308441861 ) ) ;
#29611 = ORIENTED_EDGE ( 'NONE', *, *, #44785, .T. ) ;
#29612 = CARTESIAN_POINT ( 'NONE',  ( 0.7495606340400177148, 0.1264236179284866091, 1.926673228292693052 ) ) ;
#29613 = DIRECTION ( 'NONE',  ( 0.000000000000000000, 0.7907053606985359195, -0.6121968903568508757 ) ) ;
#29614 = CARTESIAN_POINT ( 'NONE',  ( -0.1787899950787401882, -1.433686960355222473, 0.000000000000000000 ) ) ;
#29615 = ORIENTED_EDGE ( 'NONE', *, *, #17590, .T. ) ;
#29616 = CARTESIAN_POINT ( 'NONE',  ( -0.8759842519685039353, 0.000000000000000000, 0.000000000000000000 ) ) ;
#29617 = CARTESIAN_POINT ( 'NONE',  ( 0.1264236179284866091, -0.2514763778989925203, -0.1264236179284866091 ) ) ;
#29618 = CARTESIAN_POINT ( 'NONE',  ( 0.3551574803149606385, 2.613864355459500179E-17, 0.000000000000000000 ) ) ;
#29619 = AXIS2_PLACEMENT_3D ( 'NONE', #7397, #7615, #4018 ) ;
#29620 = EDGE_LOOP ( 'NONE', ( #6725, #10707, #35852, #22298 ) ) ;
#29621 = CARTESIAN_POINT ( 'NONE',  ( 0.9500414927467378812, -0.1787899950787401604, 1.195866141678520345 ) ) ;
#29622 = DIRECTION ( 'NONE',  ( 0.000000000000000000, 0.000000000000000000, -1.000000000000000000 ) ) ;
#29623 = CARTESIAN_POINT ( 'NONE',  ( 0.9873396505805591694, 0.1113553986120547346, 1.382874015640503940 ) ) ;
#29624 = CARTESIAN_POINT ( 'NONE',  ( 0.005686768416281180565, -0.09278660394087787089, -0.1148867573887376176 ) ) ;
#29625 = CARTESIAN_POINT ( 'NONE',  ( 0.9500414927467378812, -0.1787899950787401604, 0.2116141731745827814 ) ) ;
#29626 = CARTESIAN_POINT ( 'NONE',  ( -0.1787899950787401882, -1.658956692859621995, 0.000000000000000000 ) ) ;
#29627 = CARTESIAN_POINT ( 'NONE',  ( -0.1787899950787401882, -1.654035433017102319, 0.000000000000000000 ) ) ;
#29628 = SHAPE_DEFINITION_REPRESENTATION ( #45712, #7769 ) ;
#29629 = CARTESIAN_POINT ( 'NONE',  ( -0.6971942568897648851, 0.07405724077823318263, 0.4379921259304883074 ) ) ;
#29630 = CARTESIAN_POINT ( 'NONE',  ( 3.301370929368692659E-17, -1.408508376512179083, 0.1797182628040039365 ) ) ;
#29631 = PLANE ( 'NONE',  #34072 ) ;
#29632 = CARTESIAN_POINT ( 'NONE',  ( 1.002407869896990045, 0.1264236179284866091, 1.370570866087968520 ) ) ;
#29633 = LINE ( 'NONE', #44173, #3078 ) ;
#29634 = CARTESIAN_POINT ( 'NONE',  ( -0.09686282429646721204, 0.1299212598425196763, 0.1372510960255870494 ) ) ;
#29635 = DIRECTION ( 'NONE',  ( 0.8191520442889996811, 1.003171929053534361E-16, -0.5735764363510347241 ) ) ;
#29636 = DIRECTION ( 'NONE',  ( -1.000000000000000000, 0.000000000000000000, 7.047314121155780399E-15 ) ) ;
#29637 = CARTESIAN_POINT ( 'NONE',  ( 1.033464566929133799, 0.000000000000000000, 0.5511811022546778682 ) ) ;
#29638 = CARTESIAN_POINT ( 'NONE',  ( 0.9500414927467378812, -0.1787899950787401604, 0.3297244093950552069 ) ) ;
#29639 = CARTESIAN_POINT ( 'NONE',  ( 0.7038554687154958689, 0.04168604917028530255, 0.03937107934831506756 ) ) ;
#29640 = CARTESIAN_POINT ( 'NONE',  ( 0.1574803149606299191, 0.000000000000000000, 0.2952755905511810774 ) ) ;
#29641 = DIRECTION ( 'NONE',  ( 1.000000000000000000, 0.000000000000000000, 0.000000000000000000 ) ) ;
#29642 = DIRECTION ( 'NONE',  ( 0.000000000000000000, 0.000000000000000000, -1.000000000000000000 ) ) ;
#29643 = CARTESIAN_POINT ( 'NONE',  ( -0.8759842519685039353, -0.1787899950787401882, 1.272145669237574772 ) ) ;
#29644 = CARTESIAN_POINT ( 'NONE',  ( 0.7185039370078739607, 1.928577636452523993E-17, 0.6889763778452283605 ) ) ;
#29645 = EDGE_LOOP ( 'NONE', ( #10597, #46195 ) ) ;
#29646 = CARTESIAN_POINT ( 'NONE',  ( 0.1126279540338993995, 0.3740157480314960647, 1.206847064312612128 ) ) ;
#29647 = DIRECTION ( 'NONE',  ( 0.000000000000000000, 0.000000000000000000, 1.000000000000000000 ) ) ;
#29648 = ORIENTED_EDGE ( 'NONE', *, *, #20233, .F. ) ;
#29649 = CARTESIAN_POINT ( 'NONE',  ( 0.1797182628040039087, -0.09699262848068328224, -0.07444174185955065859 ) ) ;
#29650 = CARTESIAN_POINT ( 'NONE',  ( -1.033464566929133799, 0.000000000000000000, 0.3149606298137326843 ) ) ;
#29651 = CARTESIAN_POINT ( 'NONE',  ( -0.8759842519685039353, 0.1574803149606299191, 1.594488188976378007 ) ) ;
#29652 = CARTESIAN_POINT ( 'NONE',  ( 1.054774247047244096, 0.000000000000000000, 1.596948818843874074 ) ) ;
#29653 = ADVANCED_FACE ( 'NONE', ( #32130 ), #46967, .F. ) ;
#29654 = CARTESIAN_POINT ( 'NONE',  ( -0.9873396505805591694, -0.1113553986120547346, 1.097440944774362270 ) ) ;
#29656 = CARTESIAN_POINT ( 'NONE',  ( -1.033464566929133799, 0.000000000000000000, 0.1279527559055118058 ) ) ;
#29655 = CARTESIAN_POINT ( 'NONE',  ( 0.1582120475477730714, -0.1402876732178527375, 0.03788922412836724651 ) ) ;
#29657 = CARTESIAN_POINT ( 'NONE',  ( 0.9873396505805591694, -0.1113553986120547346, 1.186023622047243986 ) ) ;
#29658 = CARTESIAN_POINT ( 'NONE',  ( 0.1787899950787401604, -0.1407480314422995815, 0.07405724077823318263 ) ) ;
#29659 = ORIENTED_EDGE ( 'NONE', *, *, #8556, .T. ) ;
#29660 = EDGE_CURVE ( 'NONE', #17962, #4180, #14156, .T. ) ;
#29661 = DIRECTION ( 'NONE',  ( 0.000000000000000000, 0.000000000000000000, 1.000000000000000000 ) ) ;
#29662 = CARTESIAN_POINT ( 'NONE',  ( -0.08837038158045873448, -0.09266989036297303139, 0.2344124146308562417 ) ) ;
#29663 = CARTESIAN_POINT ( 'NONE',  ( 1.002407869896990045, 0.1264236179284866091, 0.5831692912848189803 ) ) ;
#29665 = ADVANCED_FACE ( 'NONE', ( #28554 ), #43123, .F. ) ;
#29664 = ORIENTED_EDGE ( 'NONE', *, *, #5136, .F. ) ;
#29666 = CARTESIAN_POINT ( 'NONE',  ( 1.054774247047244096, 0.000000000000000000, 0.8932086613635591421 ) ) ;
#29667 = CARTESIAN_POINT ( 'NONE',  ( 0.1574803149606299191, 0.04133858278469235842, -1.928577636452523993E-17 ) ) ;
#29668 = CARTESIAN_POINT ( 'NONE',  ( -1.002407869896990045, -0.1264236179284866091, 1.242618110182456714 ) ) ;
#29669 = ORIENTED_EDGE ( 'NONE', *, *, #16196, .T. ) ;
#29670 = EDGE_CURVE ( 'NONE', #3818, #33098, #21372, .T. ) ;
#29671 = CARTESIAN_POINT ( 'NONE',  ( -0.1738065908856299691, 0.1951474930449461631, -0.3118411609179210786 ) ) ;
#29672 = CARTESIAN_POINT ( 'NONE',  ( -1.054774247047244540, -0.07405724077823318263, 0.2608267715997796832 ) ) ;
#29673 = CARTESIAN_POINT ( 'NONE',  ( 1.033464566929133799, 0.000000000000000000, 0.6791338582677166613 ) ) ;
#29674 = FACE_OUTER_BOUND ( 'NONE', #28995, .T. ) ;
#29675 = CARTESIAN_POINT ( 'NONE',  ( 0.1264236179284866091, -0.9071121572056161098, 0.1264236179284866091 ) ) ;
#29676 = EDGE_LOOP ( 'NONE', ( #7944, #20405, #28443, #5107, #8194, #21316 ) ) ;
#29677 = CARTESIAN_POINT ( 'NONE',  ( -0.8107537697050254399, -0.1574803149606297803, 0.8538385825696385156 ) ) ;
#29678 = ORIENTED_EDGE ( 'NONE', *, *, #31141, .F. ) ;
#29679 = CARTESIAN_POINT ( 'NONE',  ( -6.002595689203704805E-19, -0.01343938916650502628, 0.1377952755905511861 ) ) ;
#29680 = CARTESIAN_POINT ( 'NONE',  ( -0.6971942568897637749, 2.189545951927499583E-17, 0.7111220471903307860 ) ) ;
#29681 = DIRECTION ( 'NONE',  ( 7.703719777548939033E-31, -0.6156614753256599570, -0.7880107536067207930 ) ) ;
#29682 = CARTESIAN_POINT ( 'NONE',  ( -0.8759842519685039353, -0.1787899950787401882, 1.749507873961984483 ) ) ;
#29683 = CARTESIAN_POINT ( 'NONE',  ( -0.7646288533564489232, 0.1113553986120547346, 0.8513779527559054427 ) ) ;
#29684 = CARTESIAN_POINT ( 'NONE',  ( 0.1270800023317771588, -1.009886329268084637, 0.1270800023317771588 ) ) ;
#29685 = DIRECTION ( 'NONE',  ( 0.000000000000000000, -0.7880107536067206819, 0.6156614753256598460 ) ) ;
#29686 = CARTESIAN_POINT ( 'NONE',  ( -0.7185039370078746268, 0.06523048226347956391, 1.513287401467275917 ) ) ;
#29687 = CARTESIAN_POINT ( 'NONE',  ( 0.8759842519685039353, -0.1787899950787401882, 0.8833661416785196785 ) ) ;
#29688 = CARTESIAN_POINT ( 'NONE',  ( 1.002407869896990045, -0.1264236179284866091, 1.355807086560409491 ) ) ;
#29689 = LINE ( 'NONE', #40859, #41403 ) ;
#29690 = CARTESIAN_POINT ( 'NONE',  ( 0.7646288533564489232, 0.1113553986120547346, 1.363188976377952999 ) ) ;
#29691 = CARTESIAN_POINT ( 'NONE',  ( 0.7130513932977933234, -0.03761588314558831497, 1.983967136699976486 ) ) ;
#29692 = FACE_OUTER_BOUND ( 'NONE', #47095, .T. ) ;
#29693 = CIRCLE ( 'NONE', #17386, 0.09842519685039370636 ) ;
#29694 = ( BOUNDED_CURVE ( )  B_SPLINE_CURVE ( 2, ( #21231, #39198, #6618, #32764, #14534, #13813, #3009, #21722, #29199 ),
 .UNSPECIFIED., .F., .T. ) 
 B_SPLINE_CURVE_WITH_KNOTS ( ( 3, 2, 2, 2, 3 ),
 ( 0.1700000000000000122, 0.1724999999999999867, 0.1749999999999999889, 0.1774999999999999911, 0.1799999999999999933 ),
 .UNSPECIFIED. ) 
 CURVE ( )  GEOMETRIC_REPRESENTATION_ITEM ( )  RATIONAL_B_SPLINE_CURVE ( ( 1.000000000000000000, 0.9238795325112869605, 1.000000000000000000, 0.9238795325112869605, 1.000000000000000000, 0.9238795325112869605, 1.000000000000000000, 0.9238795325112869605, 1.000000000000000000 ) ) 
 REPRESENTATION_ITEM ( '' )  ) ;
#29696 = CARTESIAN_POINT ( 'NONE',  ( 0.1588150004738740628, 0.09138854459950905562, 0.1173009487050022392 ) ) ;
#29695 = CARTESIAN_POINT ( 'NONE',  ( 0.6971942568897637749, 2.189545951927499583E-17, 0.7504921259304880854 ) ) ;
#29697 = CARTESIAN_POINT ( 'NONE',  ( 0.1264236179284866091, -0.7239173227808818334, -0.1264236179284866091 ) ) ;
#29698 = ORIENTED_EDGE ( 'NONE', *, *, #27109, .F. ) ;
#29699 = CARTESIAN_POINT ( 'NONE',  ( 0.1574803149606299191, 0.000000000000000000, -0.3139606299212599483 ) ) ;
#29700 = CARTESIAN_POINT ( 'NONE',  ( 0.6971942568897648851, 0.07405724077823318263, 1.181102362150960428 ) ) ;
#29701 = CARTESIAN_POINT ( 'NONE',  ( -0.9873396505805591694, 0.1113553986120547346, 1.038385826771653475 ) ) ;
#29702 = CARTESIAN_POINT ( 'NONE',  ( -1.033464566929134687, -0.06523048226347956391, 0.5191929133858269596 ) ) ;
#29703 = ADVANCED_FACE ( 'NONE', ( #30453 ), #37359, .T. ) ;
#29704 = ORIENTED_EDGE ( 'NONE', *, *, #40646, .T. ) ;
#29705 = FACE_OUTER_BOUND ( 'NONE', #33177, .T. ) ;
#29706 = CARTESIAN_POINT ( 'NONE',  ( -0.8759842519685039353, -0.1787899950787401882, 0.2878937007336381804 ) ) ;
#29707 = ORIENTED_EDGE ( 'NONE', *, *, #378, .F. ) ;
#29708 = CARTESIAN_POINT ( 'NONE',  ( -9.642888182262618425E-18, 0.05118110246973173183, -0.1574803149606299191 ) ) ;
#29709 = CARTESIAN_POINT ( 'NONE',  ( -1.054774247047244540, -0.07405724077823318263, 1.633858267662771313 ) ) ;
#29710 = CARTESIAN_POINT ( 'NONE',  ( -0.8759842519685039353, -0.1787899950787401882, 0.9178149605761574126 ) ) ;
#29711 = EDGE_CURVE ( 'NONE', #11324, #42942, #4542, .T. ) ;
#29712 = CARTESIAN_POINT ( 'NONE',  ( -0.7646288533564489232, -0.1113553986120547346, 0.1033464565853864231 ) ) ;
#29713 = CARTESIAN_POINT ( 'NONE',  ( 0.000000000000000000, 0.000000000000000000, -0.02633646578327370619 ) ) ;
#29714 = CARTESIAN_POINT ( 'NONE',  ( -6.728203135043436585E-17, 0.1564960629921311464, -0.4940944881889759444 ) ) ;
#29715 = CARTESIAN_POINT ( 'NONE',  ( 0.8759842519685039353, -0.1787899950787401882, 0.05167322829269314910 ) ) ;
#29716 = DIRECTION ( 'NONE',  ( 0.000000000000000000, 0.000000000000000000, 1.000000000000000000 ) ) ;
#29717 = CARTESIAN_POINT ( 'NONE',  ( -1.094772975963752103E-17, -0.3805373540560102463, -0.1787899950787401882 ) ) ;
#29718 = CARTESIAN_POINT ( 'NONE',  ( -0.2212350913337720881, -0.08955973899257303750, -0.09908300582586200556 ) ) ;
#29719 = CYLINDRICAL_SURFACE ( 'NONE', #33352, 0.09842519685039320676 ) ;
#29720 = DIRECTION ( 'NONE',  ( 0.000000000000000000, -1.000000000000000000, 0.000000000000000000 ) ) ;
#29721 = DIRECTION ( 'NONE',  ( 3.469446951953614583E-15, 1.000000000000000000, 0.000000000000000000 ) ) ;
#29722 = CIRCLE ( 'NONE', #20501, 0.3912448816427545051 ) ;
#29723 = CARTESIAN_POINT ( 'NONE',  ( -1.054774247047244540, 0.07405724077823318263, 0.3789370078202520253 ) ) ;
#29724 = CARTESIAN_POINT ( 'NONE',  ( 0.7646288533564489232, -0.1113553986120547346, 1.609251968503937036 ) ) ;
#29725 = ORIENTED_EDGE ( 'NONE', *, *, #27894, .T. ) ;
#29726 = CARTESIAN_POINT ( 'NONE',  ( -0.6971942568897637749, 2.189545951927499583E-17, 1.385334645615527549 ) ) ;
#29727 = ORIENTED_EDGE ( 'NONE', *, *, #11923, .T. ) ;
#29728 = CARTESIAN_POINT ( 'NONE',  ( -0.1264236179284866091, -1.309547244040724312, -0.1264236179284866091 ) ) ;
#29729 = EDGE_CURVE ( 'NONE', #25910, #18185, #4278, .T. ) ;
#29730 = CARTESIAN_POINT ( 'NONE',  ( -0.07405724077823318263, -1.489173228292693718, 0.1787899950787401604 ) ) ;
#29731 = CARTESIAN_POINT ( 'NONE',  ( 0.8759842519685039353, 0.000000000000000000, 4.498031496062992574 ) ) ;
#29732 = DIRECTION ( 'NONE',  ( -0.9999965023344150605, -0.002644866525197401685, 7.911640093061222956E-15 ) ) ;
#29733 = CARTESIAN_POINT ( 'NONE',  ( 0.7185039370078739607, 1.928577636452523993E-17, 0.4232283464566928832 ) ) ;
#29734 = CARTESIAN_POINT ( 'NONE',  ( -0.6195511811023656223, 0.6529540528279709211, 0.4629603087243971959 ) ) ;
#29735 = CARTESIAN_POINT ( 'NONE',  ( -0.9873396505805591694, -0.1113553986120547346, 1.058070866034204860 ) ) ;
#29736 = CARTESIAN_POINT ( 'NONE',  ( 0.8759842519685039353, -0.1787899950787401882, 0.4502952755367874427 ) ) ;
#29737 = CARTESIAN_POINT ( 'NONE',  ( -1.033464566929133799, 0.000000000000000000, 1.702755905511810885 ) ) ;
#29738 = CARTESIAN_POINT ( 'NONE',  ( 0.1574803149606300301, -0.2465551181102364486, 0.06523048226347956391 ) ) ;
#29739 = CARTESIAN_POINT ( 'NONE',  ( 0.8759842519685039353, -0.1574803149606299191, 1.958661417215307177 ) ) ;
#29740 = VERTEX_POINT ( 'NONE', #26846 ) ;
#29741 = CARTESIAN_POINT ( 'NONE',  ( 1.033464566929134687, -0.06523048226347956391, 0.04675196850393695952 ) ) ;
#29742 = CARTESIAN_POINT ( 'NONE',  ( 1.033464566929134687, -0.06523048226347956391, 0.9522637795275590289 ) ) ;
#29743 = CARTESIAN_POINT ( 'NONE',  ( 0.1377952755905511861, -1.365923996832131609E-16, -0.8070866141732283561 ) ) ;
#29744 = AXIS2_PLACEMENT_3D ( 'NONE', #15097, #47441, #26112 ) ;
#29745 = CARTESIAN_POINT ( 'NONE',  ( 0.9412147342319837628, -0.1574803149606297803, 0.7504921259842517456 ) ) ;
#29746 = CARTESIAN_POINT ( 'NONE',  ( -0.1670491933469263335, -0.08956140236111079234, 0.01966157176086386418 ) ) ;
#29747 = CARTESIAN_POINT ( 'NONE',  ( 0.1588147753335400203, 0.05589013274906071138, -0.1377952755905511861 ) ) ;
#29748 = ORIENTED_EDGE ( 'NONE', *, *, #12905, .F. ) ;
#29749 = DIRECTION ( 'NONE',  ( 1.000000000000000000, 0.000000000000000000, 0.000000000000000000 ) ) ;
#29750 = CARTESIAN_POINT ( 'NONE',  ( -0.3690944881889761109, 0.1864803149606354127, -0.06082000038405668829 ) ) ;
#29751 = CARTESIAN_POINT ( 'NONE',  ( 0.1787899950787401604, -1.592519684985606254, -0.07405724077823318263 ) ) ;
#29752 = CARTESIAN_POINT ( 'NONE',  ( -0.1787899950787401604, -0.7559055117572593963, -0.07405724077823318263 ) ) ;
#29754 = AXIS2_PLACEMENT_3D ( 'NONE', #5960, #5499, #16993 ) ;
#29753 = CARTESIAN_POINT ( 'NONE',  ( -0.1574803149606300301, -1.171751968503937924, -0.06523048226347956391 ) ) ;
#29755 = CARTESIAN_POINT ( 'NONE',  ( 1.033464566929134687, -0.06523048226347956391, 1.178641732175937040 ) ) ;
#29756 = CYLINDRICAL_SURFACE ( 'NONE', #32131, 0.3100393700787401619 ) ;
#29757 = EDGE_CURVE ( 'NONE', #26397, #35281, #9936, .T. ) ;
#29758 = CARTESIAN_POINT ( 'NONE',  ( -0.6971942568897637749, 2.189545951927499583E-17, 0.4749015747493858242 ) ) ;
#29759 = ORIENTED_EDGE ( 'NONE', *, *, #15828, .T. ) ;
#29760 = ORIENTED_EDGE ( 'NONE', *, *, #5952, .F. ) ;
#29761 = CARTESIAN_POINT ( 'NONE',  ( -0.8759842519685039353, 0.1787899950787401882, 1.532972440891118060 ) ) ;
#29762 = CARTESIAN_POINT ( 'NONE',  ( 1.054774247047244096, 0.000000000000000000, 1.641240157426551161 ) ) ;
#29763 = CARTESIAN_POINT ( 'NONE',  ( -1.002407869896990045, 0.1264236179284866091, 0.7406496062454487328 ) ) ;
#29764 = CARTESIAN_POINT ( 'NONE',  ( 0.7185039370078739607, 1.928577636452523993E-17, 1.476377952648377789 ) ) ;
#29765 = CARTESIAN_POINT ( 'NONE',  ( 1.002407869896990045, -0.1264236179284866091, 0.3371062991588349989 ) ) ;
#29766 = CARTESIAN_POINT ( 'NONE',  ( -0.8107537697050254399, 0.1574803149606300301, 1.508366141624757129 ) ) ;
#29767 = CARTESIAN_POINT ( 'NONE',  ( -0.6971942568897648851, -0.07405724077823297447, 1.264763779473795813 ) ) ;
#29768 = EDGE_CURVE ( 'NONE', #28928, #10268, #19880, .T. ) ;
#29769 = DIRECTION ( 'NONE',  ( 0.000000000000000000, -0.6156614753256619554, -0.7880107536067190166 ) ) ;
#29770 = CYLINDRICAL_SURFACE ( 'NONE', #9225, 0.1574803149606299191 ) ;
#29771 = CARTESIAN_POINT ( 'NONE',  ( -1.002407869896990045, -0.1264236179284866091, 1.518208661363559031 ) ) ;
#29772 = CARTESIAN_POINT ( 'NONE',  ( -1.033464566929133799, 0.000000000000000000, 1.889763779420031486 ) ) ;
#29773 = ORIENTED_EDGE ( 'NONE', *, *, #42657, .F. ) ;
#29774 = CARTESIAN_POINT ( 'NONE',  ( -0.8759842519685039353, -0.1574803149606299191, 1.574803149606299302 ) ) ;
#29775 = FACE_OUTER_BOUND ( 'NONE', #43072, .T. ) ;
#29776 = CARTESIAN_POINT ( 'NONE',  ( 0.8019270111902716547, 0.1787899950787401604, 1.496062992072220599 ) ) ;
#29777 = CARTESIAN_POINT ( 'NONE',  ( -0.1028960859539838624, -0.09851383303946475989, 0.1274171143542842388 ) ) ;
#29778 = DIRECTION ( 'NONE',  ( 0.000000000000000000, -0.9699617890481188054, -0.2432573283306646017 ) ) ;
#29779 = EDGE_LOOP ( 'NONE', ( #13851, #32515, #17483, #17975 ) ) ;
#29780 = CIRCLE ( 'NONE', #624, 0.09842519685039370636 ) ;
#29781 = VERTEX_POINT ( 'NONE', #457 ) ;
#29782 = ORIENTED_EDGE ( 'NONE', *, *, #4574, .T. ) ;
#29783 = CARTESIAN_POINT ( 'NONE',  ( -0.1264236179284866091, -0.8272637794737952577, 0.1264236179284866091 ) ) ;
#29784 = AXIS2_PLACEMENT_3D ( 'NONE', #45027, #30942, #12727 ) ;
#29785 = CARTESIAN_POINT ( 'NONE',  ( 0.1264236179284866091, -0.4138779527021417826, -0.1264236179284866091 ) ) ;
#29786 = CARTESIAN_POINT ( 'NONE',  ( -0.1264236179284866091, -1.107775590497417362, -0.1264236179284866091 ) ) ;
#29787 = VERTEX_POINT ( 'NONE', #18674 ) ;
#29788 = DIRECTION ( 'NONE',  ( -1.000000000000000000, 0.000000000000000000, 0.000000000000000000 ) ) ;
#29789 = ( LENGTH_UNIT ( ) NAMED_UNIT ( * ) SI_UNIT ( $, .METRE. ) ) ;
#29790 = CARTESIAN_POINT ( 'NONE',  ( 1.054774247047244540, -0.07405724077823318263, 1.751968503883245765 ) ) ;
#29791 = CARTESIAN_POINT ( 'NONE',  ( 0.07444174185955046430, -0.1708115261184786626, -0.1797182628040039087 ) ) ;
#29792 = CARTESIAN_POINT ( 'NONE',  ( 0.3690944881889770546, 0.1574803149606328057, -0.7480314960629921295 ) ) ;
#29793 = CARTESIAN_POINT ( 'NONE',  ( 1.054774247047244096, 0.000000000000000000, 0.7701771653005669016 ) ) ;
#29794 = ( BOUNDED_CURVE ( )  B_SPLINE_CURVE ( 2, ( #8407, #20322, #26654, #24629, #20553, #38996, #31837, #16508, #35194 ),
 .UNSPECIFIED., .F., .T. ) 
 B_SPLINE_CURVE_WITH_KNOTS ( ( 3, 2, 2, 2, 3 ),
 ( 0.6199999999999999956, 0.6225000000000000533, 0.6250000000000000000, 0.6274999999999999467, 0.6300000000000000044 ),
 .UNSPECIFIED. ) 
 CURVE ( )  GEOMETRIC_REPRESENTATION_ITEM ( )  RATIONAL_B_SPLINE_CURVE ( ( 1.000000000000000000, 0.9238795325112869605, 1.000000000000000000, 0.9238795325112869605, 1.000000000000000000, 0.9238795325112869605, 1.000000000000000000, 0.9238795325112829637, 1.000000000000000000 ) ) 
 REPRESENTATION_ITEM ( '' )  ) ;
#29795 = SURFACE_STYLE_FILL_AREA ( #7464 ) ;
#29797 = CARTESIAN_POINT ( 'NONE',  ( -0.1296641775163207277, 0.9382165298418964072, -1.070508272602716637 ) ) ;
#29796 = CARTESIAN_POINT ( 'NONE',  ( -0.1797182628040039365, -1.812051683598795648, 0.000000000000000000 ) ) ;
#29798 = CARTESIAN_POINT ( 'NONE',  ( -0.7185039370078739607, 1.928577636452523993E-17, 1.328740157480315043 ) ) ;
#29799 = CARTESIAN_POINT ( 'NONE',  ( 0.7495606340400177148, 0.1264236179284866091, 1.774114173174582643 ) ) ;
#29800 = EDGE_CURVE ( 'NONE', #22780, #17392, #28303, .T. ) ;
#29801 = ADVANCED_FACE ( 'NONE', ( #15110 ), #29756, .T. ) ;
#29802 = CARTESIAN_POINT ( 'NONE',  ( 0.8759842519685039353, 0.1574803149606299191, 0.05905511811023622659 ) ) ;
#29803 = CARTESIAN_POINT ( 'NONE',  ( 0.1563805530828635826, -0.1078949188770171180, 0.09388986751132855080 ) ) ;
#29804 = CARTESIAN_POINT ( 'NONE',  ( -0.07405724077823318263, -0.2096456692375751329, -0.1787899950787401604 ) ) ;
#29805 = CARTESIAN_POINT ( 'NONE',  ( 0.1573602050224763571, 0.1080344010929730203, 0.09369282772931890324 ) ) ;
#29806 = CARTESIAN_POINT ( 'NONE',  ( -0.1264236179284866091, -1.176673228292692830, 0.1264236179284866091 ) ) ;
#29807 = CARTESIAN_POINT ( 'NONE',  ( 0.7495606340400177148, -0.1264236179284866091, 0.2091535432533232486 ) ) ;
#29808 = CARTESIAN_POINT ( 'NONE',  ( 0.8107537697050254399, 0.1574803149606300301, 0.06151574803149608556 ) ) ;
#29809 = ADVANCED_FACE ( 'NONE', ( #7895, #40933, #40698 ), #22512, .T. ) ;
#29810 = VECTOR ( 'NONE', #29635, 39.37007874015748854 ) ;
#29811 = CARTESIAN_POINT ( 'NONE',  ( -0.6971942568897648851, 0.07405724077823318263, 1.771653543253322249 ) ) ;
#29812 = ORIENTED_EDGE ( 'NONE', *, *, #43210, .F. ) ;
#29813 = CARTESIAN_POINT ( 'NONE',  ( -0.8759842519685039353, 0.1787899950787401882, 1.178641732229700922 ) ) ;
#29814 = DIRECTION ( 'NONE',  ( -1.000000000000000000, 0.000000000000000000, 0.000000000000000000 ) ) ;
#29815 = CARTESIAN_POINT ( 'NONE',  ( 1.054774247047244096, 0.000000000000000000, 1.247539370024976391 ) ) ;
#29816 = CARTESIAN_POINT ( 'NONE',  ( -9.642888182262618425E-18, -1.169291338475149544, -0.1574803149606299191 ) ) ;
#29817 = CARTESIAN_POINT ( 'NONE',  ( 0.6971942568897626646, -0.07405724077823297447, 0.04921259837143338034 ) ) ;
#29818 = CARTESIAN_POINT ( 'NONE',  ( -1.054774247047244540, -0.07405724077823318263, 1.003937007820251193 ) ) ;
#29819 = LINE ( 'NONE', #28873, #1733 ) ;
#29820 = CARTESIAN_POINT ( 'NONE',  ( 0.6971942568897648851, 0.07405724077823318263, 0.4773622046706456068 ) ) ;
#29821 = CARTESIAN_POINT ( 'NONE',  ( -0.8019270111902716547, 0.1787899950787401604, 0.3494094487651343006 ) ) ;
#29822 = CARTESIAN_POINT ( 'NONE',  ( -1.054774247047244540, -0.07405724077823318263, 0.7677165353793073965 ) ) ;
#29823 = EDGE_LOOP ( 'NONE', ( #22774, #34873, #10175, #35102 ) ) ;
#29824 = AXIS2_PLACEMENT_3D ( 'NONE', #28212, #20987, #36811 ) ;
#29825 = ( BOUNDED_CURVE ( )  B_SPLINE_CURVE ( 2, ( #12692, #16963, #27550, #16277, #23462, #17199, #31835, #28012, #45465 ),
 .UNSPECIFIED., .F., .T. ) 
 B_SPLINE_CURVE_WITH_KNOTS ( ( 3, 2, 2, 2, 3 ),
 ( 0.7800000000000000266, 0.7824999999999999734, 0.7850000000000000311, 0.7874999999999999778, 0.7900000000000000355 ),
 .UNSPECIFIED. ) 
 CURVE ( )  GEOMETRIC_REPRESENTATION_ITEM ( )  RATIONAL_B_SPLINE_CURVE ( ( 1.000000000000000000, 0.9238795325112869605, 1.000000000000000000, 0.9238795325112869605, 1.000000000000000000, 0.9238795325112869605, 1.000000000000000000, 0.9238795325112829637, 1.000000000000000000 ) ) 
 REPRESENTATION_ITEM ( '' )  ) ;
#29826 = PRODUCT_RELATED_PRODUCT_CATEGORY ( 'part', '', ( #14590 ) ) ;
#29827 = CARTESIAN_POINT ( 'NONE',  ( -0.1787899950787401882, -0.08415354325332302654, 0.000000000000000000 ) ) ;
#29828 = CARTESIAN_POINT ( 'NONE',  ( 0.8759842519685039353, 0.1787899950787401882, 0.9030511810485984947 ) ) ;
#29829 = CARTESIAN_POINT ( 'NONE',  ( -0.9873396505805591694, -0.1113553986120547346, 0.1624015748031496231 ) ) ;
#29830 = CARTESIAN_POINT ( 'NONE',  ( 0.6971942568897648851, 0.07405724077823318263, 1.067913385773007651 ) ) ;
#29831 = DIRECTION ( 'NONE',  ( 0.000000000000000000, 1.000000000000000000, 0.000000000000000000 ) ) ;
#29832 = ORIENTED_EDGE ( 'NONE', *, *, #45634, .T. ) ;
#29833 = CARTESIAN_POINT ( 'NONE',  ( 0.8019270111902717657, 0.1787899950787401604, 1.924212598371433325 ) ) ;
#29834 = CARTESIAN_POINT ( 'NONE',  ( -0.7495606340400177148, -0.1264236179284866091, 0.8784448818360000022 ) ) ;
#29835 = CARTESIAN_POINT ( 'NONE',  ( 0.9412147342319837628, -0.1574803149606297803, 0.3174212598425196763 ) ) ;
#29836 = CARTESIAN_POINT ( 'NONE',  ( -0.1264236179284866091, -1.477978298937899559, -0.1264236179284866091 ) ) ;
#29837 = VERTEX_POINT ( 'NONE', #685 ) ;
#29838 = CARTESIAN_POINT ( 'NONE',  ( 0.1787899950787401604, -0.4950787401037172186, 0.07405724077823318263 ) ) ;
#29839 = CARTESIAN_POINT ( 'NONE',  ( -0.3100393700787401619, -0.01129866958151448837, 0.7086614173228350522 ) ) ;
#29840 = ORIENTED_EDGE ( 'NONE', *, *, #2059, .T. ) ;
#29841 = CARTESIAN_POINT ( 'NONE',  ( 0.8019270111902717657, 0.1787899950787401604, 1.176181102308441417 ) ) ;
#29842 = CARTESIAN_POINT ( 'NONE',  ( -1.033464566929134687, 0.06523048226347956391, 0.8292322833570401341 ) ) ;
#29843 = DIRECTION ( 'NONE',  ( -1.000000000000000000, 0.000000000000000000, 0.000000000000000000 ) ) ;
#29844 = VECTOR ( 'NONE', #47455, 39.37007874015748854 ) ;
#29845 = LINE ( 'NONE', #26461, #37110 ) ;
#29846 = CARTESIAN_POINT ( 'NONE',  ( 0.9500414927467378812, 0.1787899950787401604, 0.1082677164816695514 ) ) ;
#29847 = CARTESIAN_POINT ( 'NONE',  ( -0.1787899950787401604, -1.577755905458046115, 0.07405724077823318263 ) ) ;
#29848 = CARTESIAN_POINT ( 'NONE',  ( 0.1787899950787401604, -1.676181102308441639, 0.07405724077823318263 ) ) ;
#29849 = APPLICATION_PROTOCOL_DEFINITION ( 'draft international standard', 'automotive_design', 1998, #46508 ) ;
#29850 = EDGE_CURVE ( 'NONE', #29244, #25968, #43746, .T. ) ;
#29851 = CARTESIAN_POINT ( 'NONE',  ( 0.4330708661417322913, 0.1574803149606299191, 0.9891732283464566011 ) ) ;
#29852 = AXIS2_PLACEMENT_3D ( 'NONE', #37929, #30524, #44378 ) ;
#29853 = CARTESIAN_POINT ( 'NONE',  ( -0.6971942568897637749, 2.189545951927499583E-17, 0.7160433070328504623 ) ) ;
#29855 = FILL_AREA_STYLE ('',( #26706 ) ) ;
#29854 = CARTESIAN_POINT ( 'NONE',  ( -9.642888182262618425E-18, -0.5492125984251968740, -0.1574803149606299191 ) ) ;
#29856 = CARTESIAN_POINT ( 'NONE',  ( 0.1797182628040039365, -1.359295778086982320, -2.200913952912460540E-17 ) ) ;
#29857 = CARTESIAN_POINT ( 'NONE',  ( -0.05734381846710268071, 0.2623867632340645129, -0.05455490385610123338 ) ) ;
#29858 = CARTESIAN_POINT ( 'NONE',  ( 0.8019270111902717657, -0.1787899950787401604, 1.392716535379308285 ) ) ;
#29859 = VECTOR ( 'NONE', #14814, 39.37007874015748143 ) ;
#29860 = CARTESIAN_POINT ( 'NONE',  ( 0.6971942568897637749, 2.189545951927499583E-17, 1.616633858213952779 ) ) ;
#29861 = ADVANCED_FACE ( 'NONE', ( #30226 ), #44774, .T. ) ;
#29862 = LINE ( 'NONE', #7522, #28464 ) ;
#29863 = LINE ( 'NONE', #22861, #47288 ) ;
#29864 = FACE_OUTER_BOUND ( 'NONE', #8481, .T. ) ;
#29865 = CARTESIAN_POINT ( 'NONE',  ( -1.033464566929133799, 0.000000000000000000, 1.033464566929133799 ) ) ;
#29866 = DIRECTION ( 'NONE',  ( 0.000000000000000000, 0.2432573283306645739, -0.9699617890481188054 ) ) ;
#29867 = CARTESIAN_POINT ( 'NONE',  ( 0.1184675242425352465, -0.09842519685039370636, 2.185526306663015728 ) ) ;
#29868 = CARTESIAN_POINT ( 'NONE',  ( -0.4620708661417322616, 0.6102362204724407491, 1.186023622047243986 ) ) ;
#29869 = CARTESIAN_POINT ( 'NONE',  ( 0.8107537697050253289, 0.1574803149606300301, 0.6028543306011346914 ) ) ;
#29870 = ORIENTED_EDGE ( 'NONE', *, *, #5461, .T. ) ;
#29871 = CARTESIAN_POINT ( 'NONE',  ( 0.1184675242425285574, -0.5708661417322835607, 1.214596435718460654 ) ) ;
#29872 = CARTESIAN_POINT ( 'NONE',  ( 0.8241499611671327941, 0.1701252295545555571, 0.03936897362612447326 ) ) ;
#29873 = VERTEX_POINT ( 'NONE', #37606 ) ;
#29874 = CARTESIAN_POINT ( 'NONE',  ( 0.1270800023317771588, -0.02563436076414791348, 0.1270800023317771588 ) ) ;
#29876 = CARTESIAN_POINT ( 'NONE',  ( 0.1787899950787401882, -1.206200787347811110, -2.189545951927503898E-17 ) ) ;
#29875 = CARTESIAN_POINT ( 'NONE',  ( 0.1574803149606300301, -1.058562992018457827, -0.06523048226347956391 ) ) ;
#29877 = CARTESIAN_POINT ( 'NONE',  ( -1.033464566929133799, 0.000000000000000000, 1.102362204616881947 ) ) ;
#29878 = CARTESIAN_POINT ( 'NONE',  ( 0.6971942568897648851, 0.07405724077823318263, 1.653543307032850462 ) ) ;
#29880 = CARTESIAN_POINT ( 'NONE',  ( -0.8107537697050254399, -0.1574803149606297803, 1.375492125984252745 ) ) ;
#29879 = CARTESIAN_POINT ( 'NONE',  ( -0.9873396505805591694, 0.1113553986120547346, 1.825787401574803237 ) ) ;
#29881 = CARTESIAN_POINT ( 'NONE',  ( 1.033464566929133799, 0.000000000000000000, 1.929133858160188897 ) ) ;
#29882 = CARTESIAN_POINT ( 'NONE',  ( -0.1787899950787401882, -0.1186023621509610243, 0.000000000000000000 ) ) ;
#29883 = VERTEX_POINT ( 'NONE', #19393 ) ;
#29884 = EDGE_CURVE ( 'NONE', #43008, #18573, #3024, .T. ) ;
#29885 = VECTOR ( 'NONE', #27512, 39.37007874015748143 ) ;
#29886 = FACE_OUTER_BOUND ( 'NONE', #22217, .T. ) ;
#29887 = CARTESIAN_POINT ( 'NONE',  ( -0.06215339161682907620, -0.08126078924469150311, 0.2495487439735979418 ) ) ;
#29888 = CARTESIAN_POINT ( 'NONE',  ( 1.054774247047244096, 0.000000000000000000, 0.8538385826234016207 ) ) ;
#29889 = CARTESIAN_POINT ( 'NONE',  ( 2.892866454678787531E-17, -0.007874015640504449659, 0.1574803149606299191 ) ) ;
#29890 = CARTESIAN_POINT ( 'NONE',  ( -1.002407869896990045, -0.1264236179284866091, 1.321358267662771757 ) ) ;
#29891 = EDGE_CURVE ( 'NONE', #37245, #43147, #35956, .T. ) ;
#29892 = AXIS2_PLACEMENT_3D ( 'NONE', #29060, #43379, #25186 ) ;
#29893 = CARTESIAN_POINT ( 'NONE',  ( -0.8759842519685039353, 0.1787899950787401882, 0.3912401574265515491 ) ) ;
#29894 = CARTESIAN_POINT ( 'NONE',  ( 0.7185039370078739607, 1.928577636452523993E-17, 0.6594488188976378451 ) ) ;
#29895 = CARTESIAN_POINT ( 'NONE',  ( 0.8107537697050254399, -0.1574803149606297803, 1.641240157372788389 ) ) ;
#29896 = CARTESIAN_POINT ( 'NONE',  ( 0.07405724077823318263, -0.9341790863394755506, -0.1787899950787401604 ) ) ;
#29897 = EDGE_LOOP ( 'NONE', ( #7976, #38835, #46253, #5247, #24887, #38946, #46840, #2085 ) ) ;
#29898 = CARTESIAN_POINT ( 'NONE',  ( 0.7108038354695511707, 0.06841997037041733232, 0.03937007863263043694 ) ) ;
#29899 = EDGE_LOOP ( 'NONE', ( #45507, #42596, #13901, #19115 ) ) ;
#29900 = CARTESIAN_POINT ( 'NONE',  ( 0.7646288533564489232, -0.1113553986120547346, 1.205708661309795371 ) ) ;
#29901 = CARTESIAN_POINT ( 'NONE',  ( 0.000000000000000000, 0.000000000000000000, 0.000000000000000000 ) ) ;
#29902 = LINE ( 'NONE', #33726, #19338 ) ;
#29903 = CARTESIAN_POINT ( 'NONE',  ( 3.284318927891251994E-17, -0.5073818897100158543, 0.1787899950787401882 ) ) ;
#29904 = EDGE_CURVE ( 'NONE', #24840, #40966, #9482, .T. ) ;
#29905 = EDGE_CURVE ( 'NONE', #26896, #14505, #28815, .T. ) ;
#29906 = CARTESIAN_POINT ( 'NONE',  ( 1.033464566929133799, 0.000000000000000000, 0.4724409447743622148 ) ) ;
#29907 = CARTESIAN_POINT ( 'NONE',  ( -0.8759842519685039353, -0.1574803149606299191, 0.8267716535433071723 ) ) ;
#29908 = LINE ( 'NONE', #44686, #4919 ) ;
#29909 = CARTESIAN_POINT ( 'NONE',  ( 0.07444174185955046430, -1.076323337142101266, -0.1797182628040039087 ) ) ;
#29910 = DIRECTION ( 'NONE',  ( 0.000000000000000000, 0.000000000000000000, -1.000000000000000000 ) ) ;
#29911 = CARTESIAN_POINT ( 'NONE',  ( -0.8759842519685039353, 0.1574803149606299191, 1.584645669183810890 ) ) ;
#29912 = CARTESIAN_POINT ( 'NONE',  ( 0.7495606340400177148, 0.1264236179284866091, 0.9867125983714331028 ) ) ;
#29913 = CARTESIAN_POINT ( 'NONE',  ( 0.6971942568897637749, 2.189545951927499583E-17, 1.380413385773007873 ) ) ;
#29914 = ADVANCED_FACE ( 'NONE', ( #23710 ), #38286, .F. ) ;
#29915 = CONICAL_SURFACE ( 'NONE', #20701, 0.1003937007874011050, 0.7853981633973787790 ) ;
#29916 = EDGE_CURVE ( 'NONE', #19636, #15821, #27572, .T. ) ;
#29917 = DIRECTION ( 'NONE',  ( 0.000000000000000000, 1.000000000000000000, 0.000000000000000000 ) ) ;
#29918 = CARTESIAN_POINT ( 'NONE',  ( 0.9412147342319837628, -0.1574803149606297803, 1.419783464566930276 ) ) ;
#29920 = DIRECTION ( 'NONE',  ( 0.000000000000000000, 0.000000000000000000, 1.000000000000000000 ) ) ;
#29919 = CARTESIAN_POINT ( 'NONE',  ( 0.7102656538334291003, 0.005844371759168983001, 1.983162255655229078 ) ) ;
#29921 = VECTOR ( 'NONE', #44259, 39.37007874015748143 ) ;
#29922 = CARTESIAN_POINT ( 'NONE',  ( -0.8759842519685039353, 0.000000000000000000, 0.000000000000000000 ) ) ;
#29924 = DIRECTION ( 'NONE',  ( 0.000000000000000000, 0.000000000000000000, -1.000000000000000000 ) ) ;
#29923 = CARTESIAN_POINT ( 'NONE',  ( 0.6971942568897637749, 2.189545951927499583E-17, 0.8292322834108031282 ) ) ;
#29925 = CARTESIAN_POINT ( 'NONE',  ( 0.07405724077823318263, -0.7214566928596228834, -0.1787899950787401604 ) ) ;
#29926 = VERTEX_POINT ( 'NONE', #38086 ) ;
#29927 = CARTESIAN_POINT ( 'NONE',  ( 0.7185039370078741827, 0.06523048226347841205, 0.9325787401574796576 ) ) ;
#29928 = FACE_OUTER_BOUND ( 'NONE', #25890, .T. ) ;
#29929 = CARTESIAN_POINT ( 'NONE',  ( 1.002407869896990045, -0.1264236179284866091, 1.198326771599779628 ) ) ;
#29930 = DIRECTION ( 'NONE',  ( 1.822029033848725028E-16, 0.000000000000000000, 1.000000000000000000 ) ) ;
#29931 = CARTESIAN_POINT ( 'NONE',  ( 0.1574803149606299191, -1.661417322834645827, -1.928577636452523993E-17 ) ) ;
#29932 = DIRECTION ( 'NONE',  ( -6.938893903907234689E-15, 0.000000000000000000, 1.000000000000000000 ) ) ;
#29933 = ORIENTED_EDGE ( 'NONE', *, *, #19950, .F. ) ;
#29934 = FACE_OUTER_BOUND ( 'NONE', #34545, .T. ) ;
#29935 = CARTESIAN_POINT ( 'NONE',  ( -0.8019270111902717657, 0.1787899950787401604, 0.1919291338045042428 ) ) ;
#29936 = EDGE_LOOP ( 'NONE', ( #30993, #16248, #38087, #38960 ) ) ;
#29937 = CARTESIAN_POINT ( 'NONE',  ( -0.1113553986120547346, 0.05610236231225141507, -0.1113553986120547346 ) ) ;
#29938 = CARTESIAN_POINT ( 'NONE',  ( -0.1113553986120547346, -0.2883858266641263768, 0.1113553986120547346 ) ) ;
#29939 = CARTESIAN_POINT ( 'NONE',  ( -0.8759842519685039353, 0.1787899950787401882, 1.646161417269070837 ) ) ;
#29940 = CARTESIAN_POINT ( 'NONE',  ( -0.8759842519685039353, 0.1787899950787401882, 0.8981299212060788184 ) ) ;
#29941 = CARTESIAN_POINT ( 'NONE',  ( -0.8759842519685039353, -0.1787899950787401882, 0.4896653542769449086 ) ) ;
#29942 = CARTESIAN_POINT ( 'NONE',  ( 0.3980944881889773024, 0.2597269656108940894, 0.5511811023622046335 ) ) ;
#29943 = CARTESIAN_POINT ( 'NONE',  ( 0.1564216623530370331, 8.908831420875236139E-13, 0.1403857474672218497 ) ) ;
#29944 = CARTESIAN_POINT ( 'NONE',  ( -0.8759842519685039353, 0.1574803149606299191, 0.3248031494987720369 ) ) ;
#29945 = CARTESIAN_POINT ( 'NONE',  ( 0.08776479879009585483, 0.09247100924357745666, -0.2347620406593065867 ) ) ;
#29946 = CARTESIAN_POINT ( 'NONE',  ( -0.7185039370078739607, 0.000000000000000000, 2.007874015640504162 ) ) ;
#29947 = CARTESIAN_POINT ( 'NONE',  ( -0.1264236179284866091, -0.4937263304339629677, -0.1264236179284866091 ) ) ;
#29948 = CARTESIAN_POINT ( 'NONE',  ( -0.2086609251499436934, -0.08955986906679389015, 0.1029602451354245940 ) ) ;
#29949 = FACE_OUTER_BOUND ( 'NONE', #18000, .T. ) ;
#29950 = VECTOR ( 'NONE', #2288, 39.37007874015748143 ) ;
#29952 = CARTESIAN_POINT ( 'NONE',  ( -0.9412147342319837628, -0.1574803149606297803, 1.173720472333417586 ) ) ;
#29951 = VECTOR ( 'NONE', #36273, 39.37007874015748143 ) ;
#29953 = CARTESIAN_POINT ( 'NONE',  ( -0.6971942568897626646, 0.07405724077823318263, 0.3543307086076538659 ) ) ;
#29954 = EDGE_LOOP ( 'NONE', ( #1877, #4539, #22299, #24372 ) ) ;
#29955 = CARTESIAN_POINT ( 'NONE',  ( 0.000000000000000000, 0.000000000000000000, -0.0004999999999998990712 ) ) ;
#29956 = ORIENTED_EDGE ( 'NONE', *, *, #25783, .T. ) ;
#29957 = AXIS2_PLACEMENT_3D ( 'NONE', #37285, #4439, #29920 ) ;
#29958 = CARTESIAN_POINT ( 'NONE',  ( -0.6971942568897637749, 2.189545951927499583E-17, 1.542814960576157413 ) ) ;
#29959 = ORIENTED_EDGE ( 'NONE', *, *, #16824, .F. ) ;
#29960 = CARTESIAN_POINT ( 'NONE',  ( -0.1264236179284866091, -1.260334645615527549, 0.1264236179284866091 ) ) ;
#29961 = CARTESIAN_POINT ( 'NONE',  ( -0.1264236179284866091, -1.580216535379306952, -0.1264236179284866091 ) ) ;
#29962 = ( BOUNDED_CURVE ( )  B_SPLINE_CURVE ( 2, ( #4536, #44798, #23263, #12493, #30013, #37629, #40720, #19654, #37879 ),
 .UNSPECIFIED., .F., .F. ) 
 B_SPLINE_CURVE_WITH_KNOTS ( ( 3, 2, 2, 2, 3 ),
 ( 0.08000000000000000167, 0.08250000000000000389, 0.08500000000000000611, 0.08749999999999999445, 0.08999999999999999667 ),
 .UNSPECIFIED. ) 
 CURVE ( )  GEOMETRIC_REPRESENTATION_ITEM ( )  RATIONAL_B_SPLINE_CURVE ( ( 1.000000000000000000, 0.9238795325112869605, 1.000000000000000000, 0.9238795325112869605, 1.000000000000000000, 0.9238795325112869605, 1.000000000000000000, 0.9238795325112869605, 1.000000000000000000 ) ) 
 REPRESENTATION_ITEM ( '' )  ) ;
#29963 = EDGE_CURVE ( 'NONE', #31750, #43509, #5245, .T. ) ;
#29964 = CARTESIAN_POINT ( 'NONE',  ( 0.3690944881889770546, 0.1574803149606328057, -0.7480314960629921295 ) ) ;
#29965 = DIRECTION ( 'NONE',  ( -0.002641082310506000144, 0.9985657301503459982, 0.05347436071179700184 ) ) ;
#29966 = DIRECTION ( 'NONE',  ( -1.000000000000000000, 0.000000000000000000, 0.000000000000000000 ) ) ;
#29967 = CARTESIAN_POINT ( 'NONE',  ( -0.7646288533564489232, -0.1113553986120547346, 1.008858267609007875 ) ) ;
#29968 = CARTESIAN_POINT ( 'NONE',  ( 0.8759842519685039353, -0.1787899950787401882, 0.5290354330171024300 ) ) ;
#29969 = FACE_OUTER_BOUND ( 'NONE', #1835, .T. ) ;
#29970 = CARTESIAN_POINT ( 'NONE',  ( 0.06523048226347956391, -0.2367125984251967630, -0.1574803149606300301 ) ) ;
#29971 = CARTESIAN_POINT ( 'NONE',  ( 0.000000000000000000, 0.1193342091828950846, 0.06889763779527559306 ) ) ;
#29972 = ORIENTED_EDGE ( 'NONE', *, *, #10960, .F. ) ;
#29973 = EDGE_CURVE ( 'NONE', #40417, #35775, #7369, .T. ) ;
#29974 = DIRECTION ( 'NONE',  ( -0.000000000000000000, -0.6156614753256586248, -0.7880107536067217922 ) ) ;
#29975 = CARTESIAN_POINT ( 'NONE',  ( -0.8019270111902716547, 0.1787899950787401604, 0.9055118109698584439 ) ) ;
#29976 = CARTESIAN_POINT ( 'NONE',  ( 0.7646288533564489232, 0.1113553986120547346, 0.9301181102362204856 ) ) ;
#29977 = CARTESIAN_POINT ( 'NONE',  ( 0.4151545546392377273, 4.766607801171850497E-17, 0.000000000000000000 ) ) ;
#29978 = CONICAL_SURFACE ( 'NONE', #42122, 0.09842519685039370636, 0.9599310885968824758 ) ;
#29979 = CARTESIAN_POINT ( 'NONE',  ( -0.9412147342319837628, -0.1574803149606297803, 0.8292322834645677876 ) ) ;
#29980 = CARTESIAN_POINT ( 'NONE',  ( -0.1512883101241234984, -0.08956046692967721545, 0.06580901924223876709 ) ) ;
#29981 = ORIENTED_EDGE ( 'NONE', *, *, #5862, .T. ) ;
#29982 = LINE ( 'NONE', #44998, #34504 ) ;
#29983 = AXIS2_PLACEMENT_3D ( 'NONE', #16951, #43034, #9998 ) ;
#29984 = CARTESIAN_POINT ( 'NONE',  ( -0.2896382684968237808, 0.1109106728611156251, 0.7502437881410954912 ) ) ;
#29985 = ORIENTED_EDGE ( 'NONE', *, *, #20556, .T. ) ;
#29986 = CARTESIAN_POINT ( 'NONE',  ( 0.1574803149606299746, 0.9876813667277571929, 0.7893767492247212303 ) ) ;
#29987 = CARTESIAN_POINT ( 'NONE',  ( 0.8759842519685039353, -0.1574803149606299191, 1.377952755905512028 ) ) ;
#29988 = CARTESIAN_POINT ( 'NONE',  ( -0.1264236179284866091, -1.619586614119464585, -0.1264236179284866091 ) ) ;
#29989 = CARTESIAN_POINT ( 'NONE',  ( 0.07405724077823318263, -0.8051181101824581576, -0.1787899950787401604 ) ) ;
#29990 = AXIS2_PLACEMENT_3D ( 'NONE', #30047, #43904, #23047 ) ;
#29991 = CARTESIAN_POINT ( 'NONE',  ( 0.1574803149606300301, -1.152066929133859219, 0.06523048226347956391 ) ) ;
#29992 = CARTESIAN_POINT ( 'NONE',  ( 1.033464566929134687, 0.06523048226347956391, 1.144192913278300194 ) ) ;
#29993 = CARTESIAN_POINT ( 'NONE',  ( -0.8759842519685039353, -0.1574803149606299191, 1.653543307086614345 ) ) ;
#29994 = VERTEX_POINT ( 'NONE', #9573 ) ;
#29995 = ORIENTED_EDGE ( 'NONE', *, *, #21087, .F. ) ;
#29996 = CARTESIAN_POINT ( 'NONE',  ( -0.8759842519685039353, 0.1787899950787401882, 1.729822834591905556 ) ) ;
#29997 = CARTESIAN_POINT ( 'NONE',  ( 0.7495606340400177148, -0.1264236179284866091, 1.744586614119464807 ) ) ;
#29998 = CARTESIAN_POINT ( 'NONE',  ( 0.1574803149606300301, -1.334153543199559699, -0.06523048226347956391 ) ) ;
#29999 = CARTESIAN_POINT ( 'NONE',  ( -0.8759842519685039353, 0.1787899950787401882, 0.9030511810485984947 ) ) ;
#30000 = CARTESIAN_POINT ( 'NONE',  ( 0.8070866141732283561, 0.000000000000000000, 0.7574803149606299524 ) ) ;
#30001 = CARTESIAN_POINT ( 'NONE',  ( 0.4208034506101054895, 4.466152701071653354E-17, 0.000000000000000000 ) ) ;
#30002 = CARTESIAN_POINT ( 'NONE',  ( -1.054774247047244096, 0.000000000000000000, 1.163877952702141672 ) ) ;
#30003 = CARTESIAN_POINT ( 'NONE',  ( -1.054774247047244096, 0.000000000000000000, 0.9276574802611967652 ) ) ;
#30004 = CARTESIAN_POINT ( 'NONE',  ( -0.8019270111902717657, 0.1787899950787401604, 0.1574803149068664809 ) ) ;
#30005 = FACE_OUTER_BOUND ( 'NONE', #13662, .T. ) ;
#30006 = CARTESIAN_POINT ( 'NONE',  ( -1.054774247047244540, 0.07405724077823318263, 1.525590551127340433 ) ) ;
#30007 = CARTESIAN_POINT ( 'NONE',  ( -0.8759842519685039353, -0.1574803149606299191, 1.958661417215307177 ) ) ;
#30008 = VERTEX_POINT ( 'NONE', #2125 ) ;
#30009 = CARTESIAN_POINT ( 'NONE',  ( -1.033464566929134687, -0.06523048226347956391, 1.660925196850393526 ) ) ;
#30010 = CARTESIAN_POINT ( 'NONE',  ( 0.1595021679387737257, -0.4410959923581755371, -0.9673892061308022594 ) ) ;
#30011 = CARTESIAN_POINT ( 'NONE',  ( 1.054774247047244540, 0.07405724077823318263, 1.604330708607653921 ) ) ;
#30012 = CARTESIAN_POINT ( 'NONE',  ( -0.2245921208055326745, -0.09842519685039370636, -0.1004051365227200815 ) ) ;
#30013 = CARTESIAN_POINT ( 'NONE',  ( 0.8759842519685039353, 0.1574803149606299191, 0.2066929132782996115 ) ) ;
#30014 = CARTESIAN_POINT ( 'NONE',  ( 0.7185039370078739607, 1.928577636452523993E-17, 0.2952755904436539236 ) ) ;
#30015 = ORIENTED_EDGE ( 'NONE', *, *, #22614, .T. ) ;
#30016 = AXIS2_PLACEMENT_3D ( 'NONE', #783, #26944, #1031 ) ;
#30017 = VERTEX_POINT ( 'NONE', #45963 ) ;
#30018 = ORIENTED_EDGE ( 'NONE', *, *, #43437, .F. ) ;
#30019 = VECTOR ( 'NONE', #154, 39.37007874015748143 ) ;
#30020 = CIRCLE ( 'NONE', #23072, 0.009842519685039382085 ) ;
#30021 = CARTESIAN_POINT ( 'NONE',  ( 0.07405724077823318263, -0.8986220471903317852, 0.1787899950787401604 ) ) ;
#30022 = CARTESIAN_POINT ( 'NONE',  ( 0.1787899950787401882, -1.004429133804503937, -2.189545951927503898E-17 ) ) ;
#30023 = EDGE_LOOP ( 'NONE', ( #10646, #13084, #39379, #18641 ) ) ;
#30024 = ADVANCED_FACE ( 'NONE', ( #17682 ), #39757, .F. ) ;
#30025 = ( NAMED_UNIT ( * ) PLANE_ANGLE_UNIT ( ) SI_UNIT ( $, .RADIAN. ) ) ;
#30026 = ( CONVERSION_BASED_UNIT ( 'INCH', #7228 ) LENGTH_UNIT ( ) NAMED_UNIT ( #39334 ) ) ;
#30027 = CARTESIAN_POINT ( 'NONE',  ( 0.07444174185955065859, -0.3036855418665100892, 0.1797182628040039087 ) ) ;
#30028 = CARTESIAN_POINT ( 'NONE',  ( 0.3906197235759846786, 1.205361022782824954E-17, -0.09842519685039370636 ) ) ;
#30029 = ADVANCED_FACE ( 'NONE', ( #2817 ), #41295, .T. ) ;
#30030 = CARTESIAN_POINT ( 'NONE',  ( -0.8107537697050254399, 0.1574803149606300301, 1.075295275483024726 ) ) ;
#30031 = CARTESIAN_POINT ( 'NONE',  ( 0.8759842519685039353, -0.1787899950787401882, 0.7997047243556849594 ) ) ;
#30032 = DIRECTION ( 'NONE',  ( -1.000000000000000000, 0.000000000000000000, 0.000000000000000000 ) ) ;
#30033 = DIRECTION ( 'NONE',  ( -1.000000000000000000, 0.000000000000000000, 0.000000000000000000 ) ) ;
#30034 = CARTESIAN_POINT ( 'NONE',  ( -0.8107537697050234415, -0.1574803149606297803, 0.06643700776648873985 ) ) ;
#30035 = CARTESIAN_POINT ( 'NONE',  ( 0.6971942568897648851, 0.07405724077823318263, 1.776574803095843924 ) ) ;
#30036 = DIRECTION ( 'NONE',  ( 0.000000000000000000, -1.000000000000000000, 0.000000000000000000 ) ) ;
#30037 = CARTESIAN_POINT ( 'NONE',  ( 0.9412147342319837628, -0.1574803149606297803, 0.04183070866141735261 ) ) ;
#30038 = CYLINDRICAL_SURFACE ( 'NONE', #18346, 0.1574803149606299191 ) ;
#30039 = CARTESIAN_POINT ( 'NONE',  ( -0.1787899950787401604, -0.2785433070328505734, 0.07405724077823318263 ) ) ;
#30040 = CARTESIAN_POINT ( 'NONE',  ( 0.000000000000000000, 0.000000000000000000, -0.2219368594840610276 ) ) ;
#30041 = CARTESIAN_POINT ( 'NONE',  ( -0.1264236179284866091, -1.294783464513165283, 0.1264236179284866091 ) ) ;
#30042 = CARTESIAN_POINT ( 'NONE',  ( 0.8019270111902717657, -0.1787899950787401604, 0.2116141731745827814 ) ) ;
#30043 = CARTESIAN_POINT ( 'NONE',  ( -0.7185039370078739607, 1.928577636452523993E-17, 1.633858267609007875 ) ) ;
#30044 = CARTESIAN_POINT ( 'NONE',  ( -1.002407869896990045, -0.1264236179284866091, 1.749507873961984483 ) ) ;
#30045 = VERTEX_POINT ( 'NONE', #43548 ) ;
#30046 = CARTESIAN_POINT ( 'NONE',  ( -1.054774247047244540, -0.07405724077823318263, 1.245078740103716886 ) ) ;
#30047 = CARTESIAN_POINT ( 'NONE',  ( 0.000000000000000000, 0.000000000000000000, -0.1574803149606298636 ) ) ;
#30048 = CARTESIAN_POINT ( 'NONE',  ( 0.9500414927467378812, 0.1787899950787401604, 1.333661417269071059 ) ) ;
#30049 = CARTESIAN_POINT ( 'NONE',  ( 0.1574803149606300301, -1.220964566821607145, 0.06523048226347956391 ) ) ;
#30050 = VECTOR ( 'NONE', #1084, 39.37007874015748143 ) ;
#30051 = AXIS2_PLACEMENT_3D ( 'NONE', #7534, #3710, #8005 ) ;
#30052 = CARTESIAN_POINT ( 'NONE',  ( 1.054774247047244540, 0.07405724077823318263, 1.953740157426552715 ) ) ;
#30053 = CARTESIAN_POINT ( 'NONE',  ( -0.8759842519685039353, -0.1787899950787401882, 0.9965551180564724554 ) ) ;
#30054 = CARTESIAN_POINT ( 'NONE',  ( -0.1076092635444119150, -0.09842303418682271654, -0.1430890476085535934 ) ) ;
#30055 = CARTESIAN_POINT ( 'NONE',  ( -0.6195511811023656223, 0.9842519685039375910, -0.7135826771653542844 ) ) ;
#30056 = CARTESIAN_POINT ( 'NONE',  ( 0.6971942568897648851, 0.07405724077823318263, 0.4379921259304883074 ) ) ;
#30057 = CARTESIAN_POINT ( 'NONE',  ( -0.6971942568897637749, 2.189545951927499583E-17, 0.3961614172690708924 ) ) ;
#30058 = CARTESIAN_POINT ( 'NONE',  ( 1.033464566929134687, 0.06523048226347956391, 1.656003936900346085 ) ) ;
#30059 = ORIENTED_EDGE ( 'NONE', *, *, #4790, .T. ) ;
#30060 = VERTEX_POINT ( 'NONE', #10761 ) ;
#30061 = ADVANCED_FACE ( 'NONE', ( #3774 ), #21275, .F. ) ;
#30062 = CARTESIAN_POINT ( 'NONE',  ( -0.6195511811023656223, 0.4133858267716533086, 1.186023622047243986 ) ) ;
#30063 = PRODUCT_DEFINITION_SHAPE ( 'NONE', 'NONE',  #18369 ) ;
#30064 = ORIENTED_EDGE ( 'NONE', *, *, #30443, .F. ) ;
#30065 = AXIS2_PLACEMENT_3D ( 'NONE', #44933, #8290, #1329 ) ;
#30066 = CARTESIAN_POINT ( 'NONE',  ( -1.033464566929134687, -0.06523048226347956391, 0.08612204724409450174 ) ) ;
#30067 = CARTESIAN_POINT ( 'NONE',  ( -0.2087179188330661184, -0.09851385215208996460, -0.1330443330087964504 ) ) ;
#30068 = ORIENTED_EDGE ( 'NONE', *, *, #32334, .F. ) ;
#30069 = CARTESIAN_POINT ( 'NONE',  ( -1.054774247047244540, -0.07405724077823318263, 0.8907480314422986378 ) ) ;
#30070 = CARTESIAN_POINT ( 'NONE',  ( -0.9873396505805591694, -0.1113553986120547346, 0.3198818897637795700 ) ) ;
#30071 = LINE ( 'NONE', #45084, #14486 ) ;
#30072 = CARTESIAN_POINT ( 'NONE',  ( 0.07405724077823318263, -1.406620031221363476, -0.1787899950787401604 ) ) ;
#30073 = ORIENTED_EDGE ( 'NONE', *, *, #23275, .F. ) ;
#30074 = CARTESIAN_POINT ( 'NONE',  ( -0.1787899950787401604, -0.5098425196312756924, 0.07405724077823318263 ) ) ;
#30075 = EDGE_CURVE ( 'NONE', #47093, #41227, #17448, .T. ) ;
#30076 = CARTESIAN_POINT ( 'NONE',  ( 2.892866454678787531E-17, 0.03149606309965303358, 0.1574803149606299191 ) ) ;
#30077 = VERTEX_POINT ( 'NONE', #3551 ) ;
#30078 = CARTESIAN_POINT ( 'NONE',  ( 0.6971942568897648851, 0.07405724077823318263, 1.181102362150960428 ) ) ;
#30079 = CARTESIAN_POINT ( 'NONE',  ( 0.8107537697050254399, 0.1574803149606300301, 1.596948818897636624 ) ) ;
#30080 = DIRECTION ( 'NONE',  ( 1.000000000000000000, -3.368395098984144529E-15, 0.000000000000000000 ) ) ;
#30081 = ( BOUNDED_CURVE ( )  B_SPLINE_CURVE ( 2, ( #11170, #354, #44424, #19035, #32984, #15005, #47343, #33460, #29656 ),
 .UNSPECIFIED., .F., .F. ) 
 B_SPLINE_CURVE_WITH_KNOTS ( ( 3, 2, 2, 2, 3 ),
 ( 0.05000000000000000278, 0.05249999999999999806, 0.05500000000000000028, 0.05750000000000000250, 0.05999999999999999778 ),
 .UNSPECIFIED. ) 
 CURVE ( )  GEOMETRIC_REPRESENTATION_ITEM ( )  RATIONAL_B_SPLINE_CURVE ( ( 1.000000000000000000, 0.9238795325112859613, 1.000000000000000000, 0.9238795325112869605, 1.000000000000000000, 0.9238795325112869605, 1.000000000000000000, 0.9238795325112869605, 1.000000000000000000 ) ) 
 REPRESENTATION_ITEM ( '' )  ) ;
#30082 = VECTOR ( 'NONE', #23229, 39.37007874015748143 ) ;
#30083 = EDGE_CURVE ( 'NONE', #40254, #6080, #25607, .T. ) ;
#30084 = CARTESIAN_POINT ( 'NONE',  ( 0.004280036809667321987, -0.09642780928087142656, -0.1085877958708996449 ) ) ;
#30085 = CARTESIAN_POINT ( 'NONE',  ( 0.7495606340400177148, -0.1264236179284866091, 1.503444881836000002 ) ) ;
#30086 = ( GEOMETRIC_REPRESENTATION_CONTEXT ( 3 ) GLOBAL_UNCERTAINTY_ASSIGNED_CONTEXT ( ( #17816 ) ) GLOBAL_UNIT_ASSIGNED_CONTEXT ( ( #28286, #26347, #25635 ) ) REPRESENTATION_CONTEXT ( 'NONE', 'WORKASPACE' ) ) ;
#30087 = CIRCLE ( 'NONE', #32361, 0.1968503937007874405 ) ;
#30088 = CARTESIAN_POINT ( 'NONE',  ( -0.1787899950787401604, 0.1042067404321787294, 0.07405724077823318263 ) ) ;
#30089 = CARTESIAN_POINT ( 'NONE',  ( 0.1787899950787401604, -1.636811023568283341, 0.07405724077823318263 ) ) ;
#30090 = ( NAMED_UNIT ( * ) PLANE_ANGLE_UNIT ( ) SI_UNIT ( $, .RADIAN. ) ) ;
#30091 = DIRECTION ( 'NONE',  ( -1.000000000000000000, 0.000000000000000000, 0.000000000000000000 ) ) ;
#30092 = VERTEX_POINT ( 'NONE', #24652 ) ;
#30093 = EDGE_CURVE ( 'NONE', #22445, #7415, #26044, .T. ) ;
#30094 = CARTESIAN_POINT ( 'NONE',  ( -0.8019270111902716547, -0.1787899950787401604, 0.7234251967966300878 ) ) ;
#30096 = ( NAMED_UNIT ( * ) SI_UNIT ( $, .STERADIAN. ) SOLID_ANGLE_UNIT ( ) ) ;
#30095 = CARTESIAN_POINT ( 'NONE',  ( 0.06523048226347956391, -0.7239173228346461597, 0.1574803149606297803 ) ) ;
#30097 = CARTESIAN_POINT ( 'NONE',  ( -0.1797182628040039087, -1.455260345016115231, 0.07444174185955065859 ) ) ;
#30098 = FACE_OUTER_BOUND ( 'NONE', #23586, .T. ) ;
#30099 = CONICAL_SURFACE ( 'NONE', #36187, 0.2471922904502826812, 0.5235987755982992597 ) ;
#30100 = CARTESIAN_POINT ( 'NONE',  ( 0.2471922904502826257, 0.09842519685039370636, -0.01310751975302622621 ) ) ;
#30101 = CARTESIAN_POINT ( 'NONE',  ( 0.7495606340400177148, -0.1264236179284866091, 1.739665354276945131 ) ) ;
#30102 = CARTESIAN_POINT ( 'NONE',  ( -0.9873396505805591694, -0.1113553986120547346, 1.648622047136566904 ) ) ;
#30103 = LINE ( 'NONE', #41041, #15935 ) ;
#30104 = CARTESIAN_POINT ( 'NONE',  ( -0.7185039370078739607, 1.928577636452523993E-17, 0.4625984251968504046 ) ) ;
#30105 = CARTESIAN_POINT ( 'NONE',  ( 0.1787899950787401882, 0.1323818898175431191, -2.189545951927503898E-17 ) ) ;
#30106 = CARTESIAN_POINT ( 'NONE',  ( 0.7185039370078739607, 1.928577636452523993E-17, 0.5314960628845992741 ) ) ;
#30108 = CARTESIAN_POINT ( 'NONE',  ( 1.002407869896990045, 0.1264236179284866091, 0.3026574802611972648 ) ) ;
#30107 = ( BOUNDED_CURVE ( )  B_SPLINE_CURVE ( 2, ( #44814, #12024, #19428, #26649, #41197, #19668, #4799, #34080, #45045 ),
 .UNSPECIFIED., .F., .F. ) 
 B_SPLINE_CURVE_WITH_KNOTS ( ( 3, 2, 2, 2, 3 ),
 ( 0.05999999999999999778, 0.06250000000000000000, 0.06500000000000000222, 0.06750000000000000444, 0.07000000000000000666 ),
 .UNSPECIFIED. ) 
 CURVE ( )  GEOMETRIC_REPRESENTATION_ITEM ( )  RATIONAL_B_SPLINE_CURVE ( ( 1.000000000000000000, 0.9238795325112869605, 1.000000000000000000, 0.9238795325112869605, 1.000000000000000000, 0.9238795325112869605, 1.000000000000000000, 0.9238795325112869605, 1.000000000000000000 ) ) 
 REPRESENTATION_ITEM ( '' )  ) ;
#30109 = CARTESIAN_POINT ( 'NONE',  ( -1.033464566929133799, 0.000000000000000000, 1.732283464459401623 ) ) ;
#30110 = CARTESIAN_POINT ( 'NONE',  ( -0.9873396505805591694, -0.1113553986120547346, 1.333661417215306955 ) ) ;
#30111 = DIRECTION ( 'NONE',  ( -0.8191520442889873577, 1.003171929053519323E-16, 0.5735764363510523767 ) ) ;
#30112 = CARTESIAN_POINT ( 'NONE',  ( -0.8019270111902717657, -0.1787899950787401604, 1.309055118056472899 ) ) ;
#30113 = CARTESIAN_POINT ( 'NONE',  ( 0.7646288533564489232, 0.1113553986120547346, 0.6053149605223937524 ) ) ;
#30114 = ORIENTED_EDGE ( 'NONE', *, *, #23101, .T. ) ;
#30115 = CARTESIAN_POINT ( 'NONE',  ( 0.8070866141732283561, -0.3937007874015746034, 0.7574803149606299524 ) ) ;
#30116 = CARTESIAN_POINT ( 'NONE',  ( -0.1270800023317771588, -0.005949321394069172729, -0.1270800023317771588 ) ) ;
#30117 = CARTESIAN_POINT ( 'NONE',  ( 0.07405724077823318263, -1.213582677111591623, 0.1787899950787401604 ) ) ;
#30118 = CIRCLE ( 'NONE', #9413, 0.09842519685039370636 ) ;
#30119 = CARTESIAN_POINT ( 'NONE',  ( 0.9873396505805591694, 0.1113553986120547346, 0.2411417321759374011 ) ) ;
#30121 = CARTESIAN_POINT ( 'NONE',  ( -1.033464566929134687, -0.06523048226347956391, 0.4404527559055117503 ) ) ;
#30120 = CARTESIAN_POINT ( 'NONE',  ( -0.1113553986120547346, 0.05610236220472441387, 0.1113553986120547346 ) ) ;
#30122 = CARTESIAN_POINT ( 'NONE',  ( 0.9873396505805591694, -0.1113553986120547346, 1.924212598317669221 ) ) ;
#30123 = CARTESIAN_POINT ( 'NONE',  ( 0.1787899950787401604, -0.1801181101824570474, 0.07405724077823318263 ) ) ;
#30124 = B_SPLINE_CURVE_WITH_KNOTS ( 'NONE', 3,
 ( #21114, #3569, #14593, #11009, #25629, #27055, #34009, #4974, #37818, #11721, #37327, #26341, #22717, #23443, #40902, #30892, #19354, #4729, #9053, #38048, #891 ),
 .UNSPECIFIED., .F., .F.,
 ( 4, 2, 1, 1, 2, 2, 2, 1, 1, 1, 2, 2, 4 ),
 ( 0.000000000000000000, 0.1249999999999998890, 0.1874999999999997780, 0.2187499999999997502, 0.2343749999999997780, 0.2499999999999997780, 0.3750000000000000000, 0.4375000000000002220, 0.4687500000000002220, 0.4843750000000002220, 0.4921875000000001665, 0.5000000000000001110, 1.000000000000000000 ),
 .UNSPECIFIED. ) ;
#30125 = CARTESIAN_POINT ( 'NONE',  ( -1.033464566929133799, 0.000000000000000000, 0.3641732283464567121 ) ) ;
#30126 = CARTESIAN_POINT ( 'NONE',  ( 0.06523048226347956391, -0.1087598424121580948, -0.1574803149606300301 ) ) ;
#30127 = CARTESIAN_POINT ( 'NONE',  ( -0.6971942568897648851, -0.07405724077823297447, 1.269685039316314601 ) ) ;
#30128 = AXIS2_PLACEMENT_3D ( 'NONE', #22018, #29732, #37101 ) ;
#30129 = ORIENTED_EDGE ( 'NONE', *, *, #20826, .F. ) ;
#30130 = CARTESIAN_POINT ( 'NONE',  ( -0.8759842519685039353, 0.1787899950787401882, 0.3518700786863940833 ) ) ;
#30131 = CARTESIAN_POINT ( 'NONE',  ( -9.744954730003541136E-18, 0.1260561954212529312, -0.05725481610266102556 ) ) ;
#30132 = LINE ( 'NONE', #8508, #33601 ) ;
#30133 = CARTESIAN_POINT ( 'NONE',  ( 0.07405724077823318263, -1.027683023347349289, 0.1787899950787401604 ) ) ;
#30134 = ORIENTED_EDGE ( 'NONE', *, *, #14679, .F. ) ;
#30135 = CARTESIAN_POINT ( 'NONE',  ( 0.1787899950787401882, 0.05856299217974772486, -2.189545951927503898E-17 ) ) ;
#30136 = EDGE_CURVE ( 'NONE', #43357, #20302, #10274, .T. ) ;
#30137 = ORIENTED_EDGE ( 'NONE', *, *, #14131, .T. ) ;
#30138 = CARTESIAN_POINT ( 'NONE',  ( 0.8019270111902717657, -0.1787899950787401604, 1.033464566875371027 ) ) ;
#30139 = DIRECTION ( 'NONE',  ( 0.000000000000000000, 1.000000000000000000, 0.000000000000000000 ) ) ;
#30140 = CARTESIAN_POINT ( 'NONE',  ( 3.127876812047771422E-16, 0.2954942322624074524, -0.3149606299212598381 ) ) ;
#30141 = CARTESIAN_POINT ( 'NONE',  ( 0.9412147342319837628, 0.1574803149606300301, 1.424704724301921521 ) ) ;
#30142 = CARTESIAN_POINT ( 'NONE',  ( -1.094772975963752103E-17, -0.4876968503399370380, -0.1787899950787401882 ) ) ;
#30143 = ADVANCED_FACE ( 'NONE', ( #32574 ), #25368, .T. ) ;
#30144 = EDGE_CURVE ( 'NONE', #45011, #28038, #43165, .T. ) ;
#30145 = CARTESIAN_POINT ( 'NONE',  ( -0.6971942568897637749, 2.189545951927499583E-17, 0.2436023621509610382 ) ) ;
#30146 = CARTESIAN_POINT ( 'NONE',  ( -0.7646288533564489232, -0.1113553986120547346, 0.9005905511811023167 ) ) ;
#30147 = DIRECTION ( 'NONE',  ( 1.822029033848725028E-16, 0.000000000000000000, 1.000000000000000000 ) ) ;
#30148 = CARTESIAN_POINT ( 'NONE',  ( -0.1797182628040039087, -1.022189478874383495, 0.07444174185955065859 ) ) ;
#30149 = CARTESIAN_POINT ( 'NONE',  ( -0.9412147342319837628, 0.1574803149606300301, 1.936515747923967412 ) ) ;
#30150 = CARTESIAN_POINT ( 'NONE',  ( 0.8019270111902717657, 0.1787899950787401604, 0.9448818897100165204 ) ) ;
#30151 = PRODUCT_DEFINITION_FORMATION_WITH_SPECIFIED_SOURCE ( 'ANY', '', #46114, .NOT_KNOWN. ) ;
#30152 = CONICAL_SURFACE ( 'NONE', #4068, 0.1574803149606299191, 0.9599310885968603824 ) ;
#30153 = DIRECTION ( 'NONE',  ( 0.000000000000000000, 0.7880107536067233465, -0.6156614753256566264 ) ) ;
#30154 = CARTESIAN_POINT ( 'NONE',  ( 0.8107537697050253289, 0.1574803149606300301, 1.400098425196850904 ) ) ;
#30156 = DIRECTION ( 'NONE',  ( 1.000000000000000000, -3.469446951953614189E-15, -1.144917494144692682E-16 ) ) ;
#30155 = CARTESIAN_POINT ( 'NONE',  ( 0.7098837130843900223, -0.004402484902747280486, 1.983343479121606245 ) ) ;
#30157 = CARTESIAN_POINT ( 'NONE',  ( 0.7185039370078778465, -0.06523048226348396317, 1.715059055010583089 ) ) ;
#30158 = DIRECTION ( 'NONE',  ( 0.000000000000000000, 0.000000000000000000, 1.000000000000000000 ) ) ;
#30159 = CARTESIAN_POINT ( 'NONE',  ( 1.054774247047244540, 0.07405724077823318263, 0.8120078739619844832 ) ) ;
#30160 = CARTESIAN_POINT ( 'NONE',  ( -0.07405724077823318263, -0.7559055117572593963, -0.1787899950787401604 ) ) ;
#30161 = CARTESIAN_POINT ( 'NONE',  ( -0.1586641775163213364, 1.025704337919491005, -1.138861239548321524 ) ) ;
#30162 = ORIENTED_EDGE ( 'NONE', *, *, #40238, .T. ) ;
#30163 = CARTESIAN_POINT ( 'NONE',  ( 0.9873396505805591694, -0.1113553986120547346, 0.4281496061916850726 ) ) ;
#30164 = DIRECTION ( 'NONE',  ( -1.000000000000000000, 0.000000000000000000, 0.000000000000000000 ) ) ;
#30165 = CARTESIAN_POINT ( 'NONE',  ( -0.7646288533564489232, 0.1113553986120547346, 0.1722440943806619884 ) ) ;
#30166 = CARTESIAN_POINT ( 'NONE',  ( 0.7495606340400177148, -0.1264236179284866091, 1.109744094434425232 ) ) ;
#30167 = CARTESIAN_POINT ( 'NONE',  ( -0.8759842519685039353, 0.000000000000000000, 0.000000000000000000 ) ) ;
#30168 = DIMENSIONAL_EXPONENTS ( 1.000000000000000000, 0.000000000000000000, 0.000000000000000000, 0.000000000000000000, 0.000000000000000000, 0.000000000000000000, 0.000000000000000000 ) ;
#30169 = CARTESIAN_POINT ( 'NONE',  ( 2.892866454678787531E-17, -1.710629921259842590, 0.1574803149606299191 ) ) ;
#30170 = LINE ( 'NONE', #37300, #8405 ) ;
#30171 = CARTESIAN_POINT ( 'NONE',  ( -0.8019270111902717657, 0.1787899950787401604, 0.5068897637257642197 ) ) ;
#30172 = ORIENTED_EDGE ( 'NONE', *, *, #34186, .F. ) ;
#30173 = DIRECTION ( 'NONE',  ( 0.000000000000000000, -0.7880107536067206819, 0.6156614753256597350 ) ) ;
#30174 = CARTESIAN_POINT ( 'NONE',  ( -0.7495606340400177148, -0.1264236179284866091, 0.2829724408911185041 ) ) ;
#30175 = ORIENTED_EDGE ( 'NONE', *, *, #27906, .T. ) ;
#30176 = ORIENTED_EDGE ( 'NONE', *, *, #10909, .T. ) ;
#30177 = CARTESIAN_POINT ( 'NONE',  ( 0.8107537697050254399, 0.1574803149606300301, 0.3371062992125987146 ) ) ;
#30178 = VERTEX_POINT ( 'NONE', #47159 ) ;
#30179 = CARTESIAN_POINT ( 'NONE',  ( 0.07405724077823318263, -1.489173228292693718, 0.1787899950787401604 ) ) ;
#30180 = CARTESIAN_POINT ( 'NONE',  ( -0.6971942568897637749, 2.189545951927499583E-17, 1.813484251914740053 ) ) ;
#30181 = ADVANCED_FACE ( 'NONE', ( #14572 ), #39949, .T. ) ;
#30182 = CARTESIAN_POINT ( 'NONE',  ( -0.9500414927467378812, -0.1787899950787401604, 0.4527559054580477249 ) ) ;
#30183 = EDGE_CURVE ( 'NONE', #13348, #31518, #35680, .T. ) ;
#30184 = CARTESIAN_POINT ( 'NONE',  ( 0.1574803149606300023, 0.07021257666614932891, -0.1553045758542778432 ) ) ;
#30185 = CARTESIAN_POINT ( 'NONE',  ( -0.1527872282172904050, -0.4068155598699056963, -0.9303617405735025159 ) ) ;
#30186 = CARTESIAN_POINT ( 'NONE',  ( 0.6195511811023604043, 0.4133858267716528090, 1.186023622047243986 ) ) ;
#30187 = CARTESIAN_POINT ( 'NONE',  ( 0.1787899950787401604, -0.6290609761032543990, 0.07405724077823318263 ) ) ;
#30188 = CARTESIAN_POINT ( 'NONE',  ( 0.05257954919166763635, -0.08956008031886615595, 0.2115869642176704812 ) ) ;
#30189 = CARTESIAN_POINT ( 'NONE',  ( 0.1574803149606300301, 0.03887795286343254109, 0.06523048226347956391 ) ) ;
#30190 = DIRECTION ( 'NONE',  ( 5.403967543462346582E-15, -0.6156614753256592909, -0.7880107536067211260 ) ) ;
#30191 = EDGE_CURVE ( 'NONE', #44500, #25965, #10991, .T. ) ;
#30192 = EDGE_CURVE ( 'NONE', #38421, #3331, #36614, .T. ) ;
#30193 = CARTESIAN_POINT ( 'NONE',  ( 0.2559046719760603161, -0.09147515633630175225, -0.06132792317783448272 ) ) ;
#30194 = CARTESIAN_POINT ( 'NONE',  ( -0.8019270111902717657, -0.1787899950787401604, 0.3248031495525355306 ) ) ;
#30195 = CARTESIAN_POINT ( 'NONE',  ( -0.8759842519685039353, 0.000000000000000000, 0.000000000000000000 ) ) ;
#30196 = ORIENTED_EDGE ( 'NONE', *, *, #1308, .F. ) ;
#30197 = CARTESIAN_POINT ( 'NONE',  ( -1.054774247047244540, -0.07405724077823318263, 1.481299212544662902 ) ) ;
#30198 = ORIENTED_EDGE ( 'NONE', *, *, #14016, .T. ) ;
#30199 = CARTESIAN_POINT ( 'NONE',  ( -0.1787899950787401604, -1.385826771599779184, -0.07405724077823318263 ) ) ;
#30200 = CARTESIAN_POINT ( 'NONE',  ( -0.1264236179284866091, -1.491633858213953001, 0.1264236179284866091 ) ) ;
#30201 = FACE_OUTER_BOUND ( 'NONE', #31820, .T. ) ;
#30202 = CARTESIAN_POINT ( 'NONE',  ( 0.2007874015748031815, 2.507150927388283472E-17, -0.2047244094488188948 ) ) ;
#30203 = CARTESIAN_POINT ( 'NONE',  ( 0.9873396505805591694, -0.1113553986120547346, 0.5167322834645668994 ) ) ;
#30204 = DIRECTION ( 'NONE',  ( 0.000000000000000000, 0.000000000000000000, -1.000000000000000000 ) ) ;
#30205 = CARTESIAN_POINT ( 'NONE',  ( -0.9412147342319837628, 0.1574803149606300301, 1.149114173120819427 ) ) ;
#30206 = CARTESIAN_POINT ( 'NONE',  ( 0.6971942568897626646, -0.07405724077823297447, 0.5216535432533228045 ) ) ;
#30207 = CARTESIAN_POINT ( 'NONE',  ( 0.6971942568897626646, -0.07405724077823297447, 0.04429133852891373180 ) ) ;
#30209 = CARTESIAN_POINT ( 'NONE',  ( 0.5538057742782149795, 4.616380251121755931E-17, 0.000000000000000000 ) ) ;
#30208 = CARTESIAN_POINT ( 'NONE',  ( 0.1113553986120547346, -0.3179133858267716994, -0.1113553986120547346 ) ) ;
#30210 = CARTESIAN_POINT ( 'NONE',  ( 0.8107537697050253289, -0.1574803149606297803, 1.916830708553890705 ) ) ;
#30211 = ORIENTED_EDGE ( 'NONE', *, *, #32657, .F. ) ;
#30212 = CARTESIAN_POINT ( 'NONE',  ( 0.01230737760510134012, -0.07955613945526751607, -0.1377952755905511861 ) ) ;
#30213 = CARTESIAN_POINT ( 'NONE',  ( -0.6971942568897648851, -0.07405724077823297447, 0.9153543306548987957 ) ) ;
#30214 = CARTESIAN_POINT ( 'NONE',  ( 1.033464566929133799, 0.000000000000000000, 0.9153543307086614567 ) ) ;
#30215 = FACE_BOUND ( 'NONE', #33927, .T. ) ;
#30216 = LINE ( 'NONE', #22032, #44549 ) ;
#30217 = CARTESIAN_POINT ( 'NONE',  ( -0.1556638648389445378, -0.08956154917608123711, 0.05664513584083256947 ) ) ;
#30218 = ORIENTED_EDGE ( 'NONE', *, *, #39739, .T. ) ;
#30219 = FACE_OUTER_BOUND ( 'NONE', #33412, .T. ) ;
#30220 = CARTESIAN_POINT ( 'NONE',  ( 0.1574803149606299746, -0.2274162997038020051, -0.9219983537151217323 ) ) ;
#30221 = FACE_OUTER_BOUND ( 'NONE', #16855, .T. ) ;
#30222 = CARTESIAN_POINT ( 'NONE',  ( -0.1787899950787401604, -1.612204724355685403, 0.07405724077823318263 ) ) ;
#30223 = CARTESIAN_POINT ( 'NONE',  ( 0.1787899950787401604, -0.8937007873478103326, 0.07405724077823318263 ) ) ;
#30224 = CARTESIAN_POINT ( 'NONE',  ( -0.1574803149606299191, -1.208661417322834719, 0.000000000000000000 ) ) ;
#30225 = CARTESIAN_POINT ( 'NONE',  ( 0.9412147342319837628, 0.1574803149606300301, 1.070374015640503496 ) ) ;
#30226 = FACE_OUTER_BOUND ( 'NONE', #28739, .T. ) ;
#30227 = EDGE_LOOP ( 'NONE', ( #39381, #11630, #8806, #10834 ) ) ;
#30228 = ORIENTED_EDGE ( 'NONE', *, *, #45276, .T. ) ;
#30229 = CARTESIAN_POINT ( 'NONE',  ( -1.054774247047244540, 0.07405724077823318263, 1.722440944828125930 ) ) ;
#30230 = CARTESIAN_POINT ( 'NONE',  ( -0.9873396505805591694, 0.1113553986120547346, 0.6446850393700788162 ) ) ;
#30231 = CARTESIAN_POINT ( 'NONE',  ( 0.6971942568897648851, 0.07405724077823318263, 1.658464566875369472 ) ) ;
#30232 = CARTESIAN_POINT ( 'NONE',  ( -0.02156745609633855046, -0.2830359600832498268, -0.2989494884453736123 ) ) ;
#30233 = CARTESIAN_POINT ( 'NONE',  ( 0.7495606340400177148, -0.1264236179284866091, 0.2878937007336381804 ) ) ;
#30234 = CARTESIAN_POINT ( 'NONE',  ( -0.7495606340400177148, 0.1264236179284866091, 1.375492125930488196 ) ) ;
#30235 = CARTESIAN_POINT ( 'NONE',  ( -0.8759842519685039353, 0.1574803149606299191, 1.505905511703495847 ) ) ;
#30236 = CARTESIAN_POINT ( 'NONE',  ( -1.002407869896990045, 0.1264236179284866091, 1.247539370024976391 ) ) ;
#30237 = CARTESIAN_POINT ( 'NONE',  ( -0.7495606340400177148, 0.1264236179284866091, 0.8636811023084409733 ) ) ;
#30238 = ADVANCED_FACE ( 'NONE', ( #6658 ), #14343, .F. ) ;
#30239 = CARTESIAN_POINT ( 'NONE',  ( -1.033464566929133355, 0.06523048226348168721, 1.656003936900346973 ) ) ;
#30240 = CARTESIAN_POINT ( 'NONE',  ( -1.054774247047244540, -0.07405724077823318263, 1.638779527505292988 ) ) ;
#30241 = CARTESIAN_POINT ( 'NONE',  ( -1.002407869896990045, -0.1264236179284866091, 0.1008858267178899676 ) ) ;
#30242 = LINE ( 'NONE', #37624, #45514 ) ;
#30243 = CARTESIAN_POINT ( 'NONE',  ( -0.7646288533564489232, 0.1113553986120547346, 1.599409448818897683 ) ) ;
#30244 = CARTESIAN_POINT ( 'NONE',  ( 0.1574803149606300023, 0.1005108776172155827, -0.1165245190822938037 ) ) ;
#30245 = CARTESIAN_POINT ( 'NONE',  ( 0.9500414927467377701, -0.1787899950787401604, 1.594488188922615457 ) ) ;
#30246 = CARTESIAN_POINT ( 'NONE',  ( -0.1637653116087653404, -0.09842519685039370636, 0.1653323808283389817 ) ) ;
#30247 = EDGE_CURVE ( 'NONE', #29015, #44955, #18853, .T. ) ;
#30248 = CARTESIAN_POINT ( 'NONE',  ( -0.7185039370078739607, 1.928577636452523993E-17, 0.4133858266641259882 ) ) ;
#30249 = VERTEX_POINT ( 'NONE', #40411 ) ;
#30250 = ADVANCED_FACE ( 'NONE', ( #15282 ), #9170, .F. ) ;
#30251 = ORIENTED_EDGE ( 'NONE', *, *, #15672, .T. ) ;
#30252 = ORIENTED_EDGE ( 'NONE', *, *, #33079, .F. ) ;
#30253 = CARTESIAN_POINT ( 'NONE',  ( -0.8759842519685039353, 0.1787899950787401882, 1.178641732229700922 ) ) ;
#30254 = ORIENTED_EDGE ( 'NONE', *, *, #38107, .F. ) ;
#30255 = CIRCLE ( 'NONE', #24100, 0.08090551181102362266 ) ;
#30256 = CIRCLE ( 'NONE', #42433, 0.1377952755905511861 ) ;
#30257 = CARTESIAN_POINT ( 'NONE',  ( 0.1787899950787401604, -0.9330708660879686311, 0.07405724077823318263 ) ) ;
#30258 = CARTESIAN_POINT ( 'NONE',  ( -0.07405724077823318263, -1.016732283410803905, 0.1787899950787401604 ) ) ;
#30259 = ( NAMED_UNIT ( * ) SI_UNIT ( $, .STERADIAN. ) SOLID_ANGLE_UNIT ( ) ) ;
#30260 = CARTESIAN_POINT ( 'NONE',  ( 0.9500414927467378812, 0.1787899950787401604, 1.840551181048599938 ) ) ;
#30261 = CARTESIAN_POINT ( 'NONE',  ( -0.07444174185955065859, -0.2840005024964313840, -0.1797182628040039087 ) ) ;
#30262 = CYLINDRICAL_SURFACE ( 'NONE', #2735, 0.1003937007874010356 ) ;
#30263 = CARTESIAN_POINT ( 'NONE',  ( 0.1787899950787401604, -0.1456692912848192578, 0.07405724077823318263 ) ) ;
#30264 = CARTESIAN_POINT ( 'NONE',  ( 0.8019270111902717657, 0.1787899950787401604, 0.7431102361667091261 ) ) ;
#30265 = CARTESIAN_POINT ( 'NONE',  ( 0.05614424849856877037, 0.2630793352783085681, -0.05546260682012606191 ) ) ;
#30266 = DIRECTION ( 'NONE',  ( -0.000000000000000000, 1.000000000000000000, -0.000000000000000000 ) ) ;
#30267 = DIRECTION ( 'NONE',  ( 1.000000000000000000, -0.000000000000000000, -1.144917494144692682E-16 ) ) ;
#30268 = CARTESIAN_POINT ( 'NONE',  ( 0.7495606340400177148, 0.1264236179284866091, 1.813484251914740053 ) ) ;
#30269 = ORIENTED_EDGE ( 'NONE', *, *, #42114, .F. ) ;
#30270 = CARTESIAN_POINT ( 'NONE',  ( 0.7646288533564489232, -0.1113553986120547346, 0.1131889763779527630 ) ) ;
#30271 = DIRECTION ( 'NONE',  ( 0.000000000000000000, 0.000000000000000000, 1.000000000000000000 ) ) ;
#30272 = CARTESIAN_POINT ( 'NONE',  ( -0.1787899950787401604, -0.4360236219934807145, 0.07405724077823318263 ) ) ;
#30273 = FACE_OUTER_BOUND ( 'NONE', #34518, .T. ) ;
#30274 = CARTESIAN_POINT ( 'NONE',  ( -0.1787899950787401604, -1.302165354276944242, -0.07405724077823318263 ) ) ;
#30275 = CARTESIAN_POINT ( 'NONE',  ( 0.9500414927467378812, 0.1787899950787401604, 0.2706692912848194243 ) ) ;
#30276 = CARTESIAN_POINT ( 'NONE',  ( -0.7495606340400177148, -0.1264236179284866091, 1.739665354276945131 ) ) ;
#30277 = ORIENTED_EDGE ( 'NONE', *, *, #8336, .T. ) ;
#30278 = AXIS2_PLACEMENT_3D ( 'NONE', #32293, #13577, #13818 ) ;
#30279 = VECTOR ( 'NONE', #11239, 39.37007874015748143 ) ;
#30280 = FACE_OUTER_BOUND ( 'NONE', #22885, .T. ) ;
#30281 = VECTOR ( 'NONE', #45205, 39.37007874015748143 ) ;
#30282 = CARTESIAN_POINT ( 'NONE',  ( -0.1574803149606300301, -1.201279527451527995, -0.06523048226347956391 ) ) ;
#30283 = CARTESIAN_POINT ( 'NONE',  ( -0.9500414927467378812, 0.1787899950787401604, 0.5462598424659214080 ) ) ;
#30284 = CARTESIAN_POINT ( 'NONE',  ( 0.8019270111902717657, -0.1787899950787401604, 1.938976377898990799 ) ) ;
#30285 = CARTESIAN_POINT ( 'NONE',  ( -1.002407869896990045, 0.1264236179284866091, 1.208169291284818980 ) ) ;
#30286 = FACE_OUTER_BOUND ( 'NONE', #28245, .T. ) ;
#30287 = CARTESIAN_POINT ( 'NONE',  ( -0.03626583649048213676, -0.09844386080825558161, -0.1760747600047917194 ) ) ;
#30288 = CARTESIAN_POINT ( 'NONE',  ( -0.8759842519685039353, 0.1574803149606299191, 1.348425196742866206 ) ) ;
#30289 = CARTESIAN_POINT ( 'NONE',  ( 1.054774247047244540, -0.07405724077823318263, 0.4970472440407249226 ) ) ;
#30290 = CARTESIAN_POINT ( 'NONE',  ( -1.002407869896990045, 0.1264236179284866091, 0.3813976377415121966 ) ) ;
#30291 = CARTESIAN_POINT ( 'NONE',  ( -1.054774247047244540, 0.07405724077823318263, 0.8513779527021426707 ) ) ;
#30292 = ORIENTED_EDGE ( 'NONE', *, *, #27985, .T. ) ;
#30293 = ORIENTED_EDGE ( 'NONE', *, *, #20877, .F. ) ;
#30294 = EDGE_CURVE ( 'NONE', #1846, #3412, #19335, .T. ) ;
#30295 = CARTESIAN_POINT ( 'NONE',  ( 0.000000000000000000, 0.000000000000000000, -0.3149606299212598381 ) ) ;
#30296 = CARTESIAN_POINT ( 'NONE',  ( -0.9412147342319837628, 0.1574803149606300301, 0.1353346456692913757 ) ) ;
#30297 = CARTESIAN_POINT ( 'NONE',  ( -0.2341231448849070973, -0.09851385138007755227, -0.07098514503060590619 ) ) ;
#30298 = ORIENTED_EDGE ( 'NONE', *, *, #42244, .T. ) ;
#30299 = EDGE_CURVE ( 'NONE', #26206, #23816, #39025, .T. ) ;
#30300 = DIRECTION ( 'NONE',  ( 0.5735764363510447161, -0.8191520442889925757, 1.003171929053525486E-16 ) ) ;
#30301 = DIRECTION ( 'NONE',  ( 0.000000000000000000, 0.000000000000000000, 1.000000000000000000 ) ) ;
#30302 = CARTESIAN_POINT ( 'NONE',  ( -1.054774247047244096, 0.000000000000000000, 0.06151574797773248782 ) ) ;
#30303 = CARTESIAN_POINT ( 'NONE',  ( -0.1787899950787401604, -1.470596409174119934, 0.07405724077823318263 ) ) ;
#30304 = ORIENTED_EDGE ( 'NONE', *, *, #33152, .T. ) ;
#30305 = CARTESIAN_POINT ( 'NONE',  ( -0.07405724077823318263, -0.4261811023084413064, 0.1787899950787401604 ) ) ;
#30306 = CARTESIAN_POINT ( 'NONE',  ( -0.7185039370078746268, -0.06523048226347956391, 0.07135826771653554224 ) ) ;
#30307 = ORIENTED_EDGE ( 'NONE', *, *, #20386, .T. ) ;
#30308 = LINE ( 'NONE', #44859, #28737 ) ;
#30309 = FACE_OUTER_BOUND ( 'NONE', #38970, .T. ) ;
#30310 = CARTESIAN_POINT ( 'NONE',  ( 0.7108038354695511707, 0.06841997037041733232, 0.03937007863263043694 ) ) ;
#30311 = CARTESIAN_POINT ( 'NONE',  ( 1.054774247047244540, -0.07405724077823318263, 1.555118110182455382 ) ) ;
#30312 = CARTESIAN_POINT ( 'NONE',  ( 0.8019270111902717657, 0.1787899950787401604, 0.1919291338045042428 ) ) ;
#30313 = AXIS2_PLACEMENT_3D ( 'NONE', #27536, #42087, #12669 ) ;
#30314 = VECTOR ( 'NONE', #15729, 39.37007874015748143 ) ;
#30315 = CARTESIAN_POINT ( 'NONE',  ( -0.07405724077823318263, -1.745078740103716886, -0.1787899950787401604 ) ) ;
#30316 = CARTESIAN_POINT ( 'NONE',  ( -0.1787899950787401882, -1.811515747977732405, 0.000000000000000000 ) ) ;
#30317 = ( LENGTH_UNIT ( ) NAMED_UNIT ( * ) SI_UNIT ( $, .METRE. ) ) ;
#30318 = CARTESIAN_POINT ( 'NONE',  ( -1.181102362204724310, -0.3937007874015748254, -0.9842519685039370358 ) ) ;
#30319 = EDGE_CURVE ( 'NONE', #43605, #2855, #30170, .T. ) ;
#30320 = CARTESIAN_POINT ( 'NONE',  ( -0.7495606340400177148, 0.1264236179284866091, 0.6717519684501732646 ) ) ;
#30322 = SURFACE_STYLE_FILL_AREA ( #29855 ) ;
#30321 = CARTESIAN_POINT ( 'NONE',  ( 0.1574803149606300301, -0.7534448818897636624, -0.06523048226347956391 ) ) ;
#30323 = CARTESIAN_POINT ( 'NONE',  ( -0.1797182628040039365, -1.378980817457061026, 0.000000000000000000 ) ) ;
#30324 = DIRECTION ( 'NONE',  ( 0.000000000000000000, 1.000000000000000000, 0.000000000000000000 ) ) ;
#30325 = CYLINDRICAL_SURFACE ( 'NONE', #9316, 0.009842519685039428923 ) ;
#30326 = CARTESIAN_POINT ( 'NONE',  ( 1.054774247047244540, 0.07405724077823318263, 1.328740157426552049 ) ) ;
#30327 = CARTESIAN_POINT ( 'NONE',  ( 0.7495606340400177148, -0.1264236179284866091, 1.818405511757259729 ) ) ;
#30328 = CARTESIAN_POINT ( 'NONE',  ( 0.6971942568897637749, 2.189545951927499583E-17, 0.2780511810485988278 ) ) ;
#30329 = APPLICATION_CONTEXT ( 'automotive_design' ) ;
#30331 = VERTEX_POINT ( 'NONE', #18620 ) ;
#30330 = CARTESIAN_POINT ( 'NONE',  ( -0.8759842519685039353, -0.1574803149606299191, 1.643700787294047228 ) ) ;
#30332 = DIRECTION ( 'NONE',  ( 0.000000000000000000, 1.000000000000000000, 0.000000000000000000 ) ) ;
#30333 = CARTESIAN_POINT ( 'NONE',  ( 4.268512490100409430E-16, 0.2954942322624074524, -0.2921040715117803055 ) ) ;
#30334 = CARTESIAN_POINT ( 'NONE',  ( -0.7185039370078739607, 1.928577636452523993E-17, 1.013779527559055094 ) ) ;
#30335 = CARTESIAN_POINT ( 'NONE',  ( -0.7185039370078714072, 0.06523048226347728795, 1.237696850286174932 ) ) ;
#30336 = CARTESIAN_POINT ( 'NONE',  ( -1.181102362204724310, 0.000000000000000000, 0.9842519685039370358 ) ) ;
#30337 = CARTESIAN_POINT ( 'NONE',  ( -0.8759842519685039353, -0.1574803149606299191, 1.328740157372787278 ) ) ;
#30338 = CARTESIAN_POINT ( 'NONE',  ( 0.2066929133858268486, 0.5419727308409655331, -0.7545416139885203766 ) ) ;
#30339 = CARTESIAN_POINT ( 'NONE',  ( 0.9412147342319837628, 0.1574803149606300301, 0.7160433069790875793 ) ) ;
#30340 = ORIENTED_EDGE ( 'NONE', *, *, #16315, .F. ) ;
#30341 = SURFACE_SIDE_STYLE ('',( #37243 ) ) ;
#30342 = CARTESIAN_POINT ( 'NONE',  ( 0.8163103687857603541, 0.1681809448548153563, 0.03937007863263042307 ) ) ;
#30343 = EDGE_LOOP ( 'NONE', ( #8853, #4832, #41777, #21234 ) ) ;
#30344 = CARTESIAN_POINT ( 'NONE',  ( -1.100456976456230270E-17, -0.01087058123658885857, -0.1797182628040039365 ) ) ;
#30345 = PRODUCT_DEFINITION_SHAPE ( 'NONE', 'NONE',  #14855 ) ;
#30346 = CARTESIAN_POINT ( 'NONE',  ( 3.284318927891251994E-17, -1.137303149552535420, 0.1787899950787401882 ) ) ;
#30347 = CARTESIAN_POINT ( 'NONE',  ( -0.7646288533564489232, 0.1113553986120547346, 0.8120078740157481434 ) ) ;
#30348 = CARTESIAN_POINT ( 'NONE',  ( 0.7495606340400177148, 0.1264236179284866091, 1.611712598371433103 ) ) ;
#30349 = CARTESIAN_POINT ( 'NONE',  ( -0.8107537697050253289, -0.1574803149606297803, 1.178641732283464583 ) ) ;
#30350 = AXIS2_PLACEMENT_3D ( 'NONE', #4223, #19574, #22693 ) ;
#30351 = CARTESIAN_POINT ( 'NONE',  ( 1.033464566929133799, 0.000000000000000000, 0.2362204723334177248 ) ) ;
#30352 = FACE_OUTER_BOUND ( 'NONE', #14631, .T. ) ;
#30353 = DIRECTION ( 'NONE',  ( -1.000000000000000000, 0.000000000000000000, 0.000000000000000000 ) ) ;
#30354 = EDGE_CURVE ( 'NONE', #6659, #30331, #4555, .T. ) ;
#30355 = CARTESIAN_POINT ( 'NONE',  ( 0.7646288533564489232, -0.1113553986120547346, 1.323818897530267602 ) ) ;
#30356 = ORIENTED_EDGE ( 'NONE', *, *, #33845, .F. ) ;
#30357 = ADVANCED_FACE ( 'NONE', ( #19086 ), #622, .F. ) ;
#30358 = CARTESIAN_POINT ( 'NONE',  ( -0.07051875723980910449, -0.08549467455823119011, -0.2447177463901700212 ) ) ;
#30359 = CARTESIAN_POINT ( 'NONE',  ( -0.1113553986120547346, -0.05216535422318158144, 0.1113553986120547346 ) ) ;
#30360 = CARTESIAN_POINT ( 'NONE',  ( -0.8019270111902717657, 0.1787899950787401604, 1.338582677111590069 ) ) ;
#30361 = AXIS2_PLACEMENT_3D ( 'NONE', #13263, #35994, #16612 ) ;
#30362 = ORIENTED_EDGE ( 'NONE', *, *, #19032, .T. ) ;
#30363 = EDGE_CURVE ( 'NONE', #18878, #27285, #11693, .T. ) ;
#30364 = ( BOUNDED_CURVE ( )  B_SPLINE_CURVE ( 2, ( #46193, #28734, #6880, #3290, #13603, #42805, #36135, #13391, #21020 ),
 .UNSPECIFIED., .F., .T. ) 
 B_SPLINE_CURVE_WITH_KNOTS ( ( 3, 2, 2, 2, 3 ),
 ( 0.3400000000000000244, 0.3425000000000000266, 0.3449999999999999734, 0.3474999999999999756, 0.3499999999999999778 ),
 .UNSPECIFIED. ) 
 CURVE ( )  GEOMETRIC_REPRESENTATION_ITEM ( )  RATIONAL_B_SPLINE_CURVE ( ( 1.000000000000000000, 0.9238795325112869605, 1.000000000000000000, 0.9238795325112869605, 1.000000000000000000, 0.9238795325112869605, 1.000000000000000000, 0.9238795325112849621, 1.000000000000000000 ) ) 
 REPRESENTATION_ITEM ( '' )  ) ;
#30365 = FACE_OUTER_BOUND ( 'NONE', #27071, .T. ) ;
#30366 = CARTESIAN_POINT ( 'NONE',  ( -1.054774247047244540, 0.07405724077823318263, 0.3838582676627718127 ) ) ;
#30367 = CARTESIAN_POINT ( 'NONE',  ( 0.004280036809634069940, 0.1422536944055189378, -0.02921503453314187176 ) ) ;
#30368 = DIRECTION ( 'NONE',  ( 0.000000000000000000, 1.000000000000000000, 0.000000000000000000 ) ) ;
#30369 = CARTESIAN_POINT ( 'NONE',  ( -1.094772975963752103E-17, -1.049828692638687055, -0.1787899950787401882 ) ) ;
#30370 = CARTESIAN_POINT ( 'NONE',  ( 0.07405724077823318263, 0.01181102367581074800, 0.1787899950787401604 ) ) ;
#30371 = ORIENTED_EDGE ( 'NONE', *, *, #42449, .F. ) ;
#30372 = ORIENTED_EDGE ( 'NONE', *, *, #32823, .T. ) ;
#30373 = CARTESIAN_POINT ( 'NONE',  ( 0.5555748031496086092, 0.2597269656108935343, 0.7480314960629921295 ) ) ;
#30374 = LINE ( 'NONE', #44921, #29249 ) ;
#30375 = CARTESIAN_POINT ( 'NONE',  ( 0.2642359194686346169, 4.766607801171850497E-17, 0.000000000000000000 ) ) ;
#30376 = AXIS2_PLACEMENT_3D ( 'NONE', #18102, #43253, #32020 ) ;
#30377 = ( BOUNDED_CURVE ( )  B_SPLINE_CURVE ( 2, ( #38194, #45842, #5844, #8722, #5356, #1284, #38436, #16407, #31264 ),
 .UNSPECIFIED., .F., .F. ) 
 B_SPLINE_CURVE_WITH_KNOTS ( ( 3, 2, 2, 2, 3 ),
 ( 0.3800000000000000044, 0.3825000000000000067, 0.3850000000000000089, 0.3875000000000000111, 0.3900000000000000133 ),
 .UNSPECIFIED. ) 
 CURVE ( )  GEOMETRIC_REPRESENTATION_ITEM ( )  RATIONAL_B_SPLINE_CURVE ( ( 1.000000000000000000, 0.9238795325112869605, 1.000000000000000000, 0.9238795325112869605, 1.000000000000000000, 0.9238795325112869605, 1.000000000000000000, 0.9238795325112869605, 1.000000000000000000 ) ) 
 REPRESENTATION_ITEM ( '' )  ) ;
#30378 = CARTESIAN_POINT ( 'NONE',  ( -0.7646288533564489232, -0.1113553986120547346, 0.8218503937007874960 ) ) ;
#30379 = CARTESIAN_POINT ( 'NONE',  ( 0.07444174185955065859, -0.9729768804491867318, 0.1797182628040039087 ) ) ;
#30380 = CARTESIAN_POINT ( 'NONE',  ( -1.033464566929134687, 0.06523048226347956391, 1.931594488081448180 ) ) ;
#30381 = CARTESIAN_POINT ( 'NONE',  ( -0.9873396505805591694, 0.1113553986120547346, 1.461614173120818760 ) ) ;
#30382 = CARTESIAN_POINT ( 'NONE',  ( 0.8759842519685039353, 0.1787899950787401882, 0.9030511810485984947 ) ) ;
#30383 = CARTESIAN_POINT ( 'NONE',  ( 1.054774247047244540, 0.07405724077823318263, 0.1033464566391499029 ) ) ;
#30384 = DIRECTION ( 'NONE',  ( 0.000000000000000000, -1.000000000000000000, 0.000000000000000000 ) ) ;
#30385 = CARTESIAN_POINT ( 'NONE',  ( 0.7646288533564489232, 0.1113553986120547346, 1.638779527559055316 ) ) ;
#30387 = LINE ( 'NONE', #38008, #34651 ) ;
#30386 = CARTESIAN_POINT ( 'NONE',  ( 0.7274018190141648965, -0.07989133380807623974, 1.984821033286637171 ) ) ;
#30388 = DIRECTION ( 'NONE',  ( -0.000000000000000000, -0.2432573283306646017, 0.9699617890481188054 ) ) ;
#30389 = CARTESIAN_POINT ( 'NONE',  ( -0.1787899950787401882, 0.1176181102899840625, 0.000000000000000000 ) ) ;
#30390 = DIRECTION ( 'NONE',  ( -0.000000000000000000, 0.7880107536067207930, -0.6156614753256597350 ) ) ;
#30391 = CARTESIAN_POINT ( 'NONE',  ( 1.054774247047244540, -0.07405724077823318263, 0.8070866141194653620 ) ) ;
#30392 = CARTESIAN_POINT ( 'NONE',  ( 0.9500414927467377701, 0.1787899950787401604, 1.845472440891119392 ) ) ;
#30393 = CARTESIAN_POINT ( 'NONE',  ( -0.1787899950787401882, -0.9060039369541103005, 0.000000000000000000 ) ) ;
#30394 = VERTEX_POINT ( 'NONE', #26553 ) ;
#30395 = EDGE_CURVE ( 'NONE', #30008, #34889, #10463, .T. ) ;
#30396 = CARTESIAN_POINT ( 'NONE',  ( -0.7185039370078739607, 1.928577636452523993E-17, 1.555118110128692832 ) ) ;
#30397 = CARTESIAN_POINT ( 'NONE',  ( -0.06523048226347956391, -1.742618110128693276, 0.1574803149606297803 ) ) ;
#30398 = CARTESIAN_POINT ( 'NONE',  ( -1.033464566929134687, -0.06523048226347956391, 0.07627952745152805081 ) ) ;
#30399 = CARTESIAN_POINT ( 'NONE',  ( 0.6971942568897637749, 2.189545951927499583E-17, 1.144192913332062966 ) ) ;
#30400 = CARTESIAN_POINT ( 'NONE',  ( 0.7185039370078739607, 0.000000000000000000, 4.498031496062992574 ) ) ;
#30401 = CARTESIAN_POINT ( 'NONE',  ( -0.1113553986120547346, -1.676181102362204856, 0.1113553986120547346 ) ) ;
#30402 = DIRECTION ( 'NONE',  ( 0.000000000000000000, 0.000000000000000000, 1.000000000000000000 ) ) ;
#30403 = EDGE_CURVE ( 'NONE', #5296, #41905, #37038, .T. ) ;
#30404 = CARTESIAN_POINT ( 'NONE',  ( 1.033464566929133799, 0.000000000000000000, 0.04921259842519685318 ) ) ;
#30405 = CARTESIAN_POINT ( 'NONE',  ( -0.6971942568897626646, 0.07405724077823318263, 0.3149606298674962890 ) ) ;
#30406 = EDGE_LOOP ( 'NONE', ( #4544, #40134, #32521, #6590 ) ) ;
#30407 = CARTESIAN_POINT ( 'NONE',  ( 3.284318927891251994E-17, -1.491633858213953001, 0.1787899950787401882 ) ) ;
#30408 = CARTESIAN_POINT ( 'NONE',  ( -1.002407869896990045, 0.1264236179284866091, 1.759350393647023614 ) ) ;
#30409 = CARTESIAN_POINT ( 'NONE',  ( -0.9500414927467377701, 0.1787899950787401604, 0.8562992125446617919 ) ) ;
#30410 = EDGE_CURVE ( 'NONE', #42395, #40227, #29131, .T. ) ;
#30411 = CARTESIAN_POINT ( 'NONE',  ( -1.054774247047244540, 0.07405724077823318263, 0.4625984251430869665 ) ) ;
#30412 = CYLINDRICAL_SURFACE ( 'NONE', #25266, 0.009842519685039428923 ) ;
#30413 = DIRECTION ( 'NONE',  ( 0.000000000000000000, -1.000000000000000000, 0.000000000000000000 ) ) ;
#30414 = CARTESIAN_POINT ( 'NONE',  ( -0.7185039370078746268, 0.06523048226347956391, 0.3321850392625518844 ) ) ;
#30415 = DIRECTION ( 'NONE',  ( 0.000000000000000000, -0.7880107536067207930, 0.6156614753256598460 ) ) ;
#30416 = CARTESIAN_POINT ( 'NONE',  ( -1.094772975963752103E-17, -0.4986475902764826995, -0.1787899950787401882 ) ) ;
#30417 = CARTESIAN_POINT ( 'NONE',  ( -0.1613434097111628163, -0.08955965769485689509, 0.1626613769059765680 ) ) ;
#30418 = FACE_OUTER_BOUND ( 'NONE', #9357, .T. ) ;
#30419 = CARTESIAN_POINT ( 'NONE',  ( -0.9873396505805591694, 0.1113553986120547346, 1.973425196742866206 ) ) ;
#30420 = CARTESIAN_POINT ( 'NONE',  ( -0.6971942568897626646, 0.07405724077823318263, 0.5511811023084406402 ) ) ;
#30421 = CARTESIAN_POINT ( 'NONE',  ( 0.9873396505805591694, 0.1113553986120547346, 1.186023621939716666 ) ) ;
#30422 = ORIENTED_EDGE ( 'NONE', *, *, #26458, .F. ) ;
#30423 = CARTESIAN_POINT ( 'NONE',  ( 0.000000000000000000, 0.000000000000000000, -0.07924015748031493223 ) ) ;
#30424 = CARTESIAN_POINT ( 'NONE',  ( 0.1787899950787401604, -1.287401574749386768, 0.07405724077823318263 ) ) ;
#30425 = CARTESIAN_POINT ( 'NONE',  ( 0.1264236179284866091, -1.560531496009228247, 0.1264236179284866091 ) ) ;
#30426 = AXIS2_PLACEMENT_3D ( 'NONE', #29750, #44298, #19387 ) ;
#30427 = CARTESIAN_POINT ( 'NONE',  ( 0.8759842519685039353, 0.1574803149606299191, 0.9645669291338583307 ) ) ;
#30428 = CARTESIAN_POINT ( 'NONE',  ( 0.8107537697050253289, 0.1574803149606300301, 0.4552165354330702240 ) ) ;
#30429 = DIRECTION ( 'NONE',  ( 1.000000000000000000, -3.469446951953614189E-15, -0.000000000000000000 ) ) ;
#30430 = CARTESIAN_POINT ( 'NONE',  ( -0.8107537697050253289, 0.1574803149606300301, 1.035925196742866650 ) ) ;
#30431 = CARTESIAN_POINT ( 'NONE',  ( 0.6971942568897626646, 0.07405724077823318263, 0.5954724408911187261 ) ) ;
#30433 = CARTESIAN_POINT ( 'NONE',  ( 0.7185039370078746268, -0.06523048226347956391, 0.3469488188976379561 ) ) ;
#30432 = CARTESIAN_POINT ( 'NONE',  ( 0.1574803149606300301, -0.2810039370078740162, -0.06523048226347956391 ) ) ;
#30434 = CARTESIAN_POINT ( 'NONE',  ( 0.7185039370078746268, 0.06523048226347956391, 1.985728346349167950 ) ) ;
#30435 = ORIENTED_EDGE ( 'NONE', *, *, #15672, .F. ) ;
#30436 = ADVANCED_FACE ( 'NONE', ( #15527 ), #22451, .T. ) ;
#30437 = CARTESIAN_POINT ( 'NONE',  ( -0.1191479377955081548, -0.09019619403132914104, -0.1333268377994320797 ) ) ;
#30438 = CARTESIAN_POINT ( 'NONE',  ( 0.7646288533564489232, -0.1113553986120547346, 0.9005905511811023167 ) ) ;
#30439 = LINE ( 'NONE', #19376, #44994 ) ;
#30440 = CARTESIAN_POINT ( 'NONE',  ( 0.000000000000000000, 0.09842519685039370636, 0.000000000000000000 ) ) ;
#30441 = CARTESIAN_POINT ( 'NONE',  ( -0.1355115267431857007, -0.08956120344901688513, 0.09056412678083718137 ) ) ;
#30442 = ORIENTED_EDGE ( 'NONE', *, *, #37772, .T. ) ;
#30443 = EDGE_CURVE ( 'NONE', #13083, #36338, #41111, .T. ) ;
#30444 = CARTESIAN_POINT ( 'NONE',  ( 0.1559663611957041174, 0.05603239795798645867, -0.1377952755905511861 ) ) ;
#30445 = CARTESIAN_POINT ( 'NONE',  ( -0.2983856243743983061, 0.08472875797579337842, 0.7312943568775917003 ) ) ;
#30446 = EDGE_LOOP ( 'NONE', ( #30736, #6564, #39020, #3193 ) ) ;
#30447 = CARTESIAN_POINT ( 'NONE',  ( 0.7185039370078746268, 0.06523048226347956391, 1.286909448818897905 ) ) ;
#30448 = DIRECTION ( 'NONE',  ( 1.000000000000000000, 0.000000000000000000, 0.000000000000000000 ) ) ;
#30449 = CARTESIAN_POINT ( 'NONE',  ( 0.1787899950787401604, -1.715551181048599716, 0.07405724077823318263 ) ) ;
#30450 = CARTESIAN_POINT ( 'NONE',  ( 0.1787899950787401604, -0.9330708660879686311, 0.07405724077823318263 ) ) ;
#30451 = CARTESIAN_POINT ( 'NONE',  ( -9.642888182262618425E-18, -1.257874015748031482, -0.1574803149606299191 ) ) ;
#30452 = CARTESIAN_POINT ( 'NONE',  ( 1.033464566929133799, 0.000000000000000000, 1.181102362097196989 ) ) ;
#30453 = FACE_OUTER_BOUND ( 'NONE', #33004, .T. ) ;
#30454 = ORIENTED_EDGE ( 'NONE', *, *, #17254, .F. ) ;
#30455 = VERTEX_POINT ( 'NONE', #41345 ) ;
#30456 = CARTESIAN_POINT ( 'NONE',  ( -0.8019270111902717657, 0.1787899950787401604, 1.811023621993480548 ) ) ;
#30457 = ORIENTED_EDGE ( 'NONE', *, *, #10564, .F. ) ;
#30458 = CARTESIAN_POINT ( 'NONE',  ( 0.1574803149606300301, -1.378444881782237008, 0.06523048226347956391 ) ) ;
#30459 = CARTESIAN_POINT ( 'NONE',  ( -0.07407796729095041111, -0.2527247573021067506, -0.3106979152243043996 ) ) ;
#30460 = CARTESIAN_POINT ( 'NONE',  ( 0.8019270111902717657, -0.1787899950787401604, 0.4872047243556847929 ) ) ;
#30461 = CARTESIAN_POINT ( 'NONE',  ( -0.7495606340400177148, 0.1264236179284866091, 1.414862204670645829 ) ) ;
#30462 = CARTESIAN_POINT ( 'NONE',  ( 0.01090721357323628377, 0.2891969495697860881, -0.2957398093695285390 ) ) ;
#30463 = CARTESIAN_POINT ( 'NONE',  ( -0.8019270111902716547, 0.1787899950787401604, 1.215551181048599272 ) ) ;
#30464 = CARTESIAN_POINT ( 'NONE',  ( -0.6971942568897648851, 0.07405724077823318263, 0.7874015747493863238 ) ) ;
#30465 = CARTESIAN_POINT ( 'NONE',  ( -0.8019270111902717657, -0.1787899950787401604, 0.9547244093950547628 ) ) ;
#30466 = CARTESIAN_POINT ( 'NONE',  ( -0.8759842519685039353, 0.1787899950787401882, 0.1156496062454492185 ) ) ;
#30467 = CARTESIAN_POINT ( 'NONE',  ( 4.801428276353606495E-17, 0.03219022224904102836, 0.2854330708661417804 ) ) ;
#30468 = CARTESIAN_POINT ( 'NONE',  ( -1.002407869896990045, 0.1264236179284866091, 1.803641732229700700 ) ) ;
#30469 = CARTESIAN_POINT ( 'NONE',  ( -0.7495606340400177148, -0.1264236179284866091, 0.1304133857730082613 ) ) ;
#30470 = CARTESIAN_POINT ( 'NONE',  ( -0.9412147342319837628, -0.1574803149606297803, 1.577263779527559917 ) ) ;
#30471 = CARTESIAN_POINT ( 'NONE',  ( 1.033464566929133799, 1.928577636452524610E-17, 4.498031496062992574 ) ) ;
#30472 = CARTESIAN_POINT ( 'NONE',  ( 1.054774247047244540, -0.07405724077823318263, 1.638779527505292766 ) ) ;
#30473 = CARTESIAN_POINT ( 'NONE',  ( -0.1264342353168110278, -0.09851383435030748592, 0.1068074073256397583 ) ) ;
#30474 = CARTESIAN_POINT ( 'NONE',  ( -0.7185039370078739607, 0.000000000000000000, -2.869337061179095023E-17 ) ) ;
#30475 = EDGE_LOOP ( 'NONE', ( #14184, #4656, #44375, #27473 ) ) ;
#30476 = VERTEX_POINT ( 'NONE', #8546 ) ;
#30477 = CARTESIAN_POINT ( 'NONE',  ( 3.284318927891251994E-17, -0.8223425196312754704, 0.1787899950787401882 ) ) ;
#30478 = ( BOUNDED_CURVE ( )  B_SPLINE_CURVE ( 2, ( #20998, #17184, #39208, #21240, #28467, #14064, #35413, #2552, #31819 ),
 .UNSPECIFIED., .F., .T. ) 
 B_SPLINE_CURVE_WITH_KNOTS ( ( 3, 2, 2, 2, 3 ),
 ( 0.08500000000000000611, 0.08749999999999999445, 0.08999999999999999667, 0.09249999999999999889, 0.09500000000000000111 ),
 .UNSPECIFIED. ) 
 CURVE ( )  GEOMETRIC_REPRESENTATION_ITEM ( )  RATIONAL_B_SPLINE_CURVE ( ( 1.000000000000000000, 0.9238795325112869605, 1.000000000000000000, 0.9238795325112869605, 1.000000000000000000, 0.9238795325112869605, 1.000000000000000000, 0.9238795325112869605, 1.000000000000000000 ) ) 
 REPRESENTATION_ITEM ( '' )  ) ;
#30479 = CARTESIAN_POINT ( 'NONE',  ( -0.1787899950787401882, -1.102854330654897685, 0.000000000000000000 ) ) ;
#30480 = VECTOR ( 'NONE', #42739, 39.37007874015748143 ) ;
#30481 = CARTESIAN_POINT ( 'NONE',  ( -0.7185039370078746268, 0.06523048226347956391, 1.286909448818897905 ) ) ;
#30482 = CARTESIAN_POINT ( 'NONE',  ( -0.1270800023317771588, -0.2716973528901322488, 0.1270800023317771588 ) ) ;
#30483 = CARTESIAN_POINT ( 'NONE',  ( 0.2559055118110236116, 0.1477471161312045311, -0.2921040715117803055 ) ) ;
#30484 = ADVANCED_FACE ( 'NONE', ( #33984 ), #22695, .F. ) ;
#30485 = DIRECTION ( 'NONE',  ( -0.000000000000000000, -0.2432573283306819767, 0.9699617890481142535 ) ) ;
#30486 = CARTESIAN_POINT ( 'NONE',  ( 1.054774247047244540, 0.07405724077823318263, 0.8120078739619844832 ) ) ;
#30487 = VECTOR ( 'NONE', #38372, 39.37007874015748143 ) ;
#30488 = EDGE_CURVE ( 'NONE', #2757, #19564, #2170, .T. ) ;
#30489 = SURFACE_STYLE_USAGE ( .BOTH. , #12510 ) ;
#30490 = CARTESIAN_POINT ( 'NONE',  ( -0.8759842519685039353, -0.1574803149606299191, 0.06889763768774861963 ) ) ;
#30491 = CARTESIAN_POINT ( 'NONE',  ( 0.9412147342319837628, -0.1574803149606297803, 0.07135826760900840227 ) ) ;
#30492 = EDGE_CURVE ( 'NONE', #42394, #26601, #37499, .T. ) ;
#30493 = ADVANCED_FACE ( 'NONE', ( #31327 ), #13344, .T. ) ;
#30494 = CARTESIAN_POINT ( 'NONE',  ( 0.8759842519685039353, -0.1574803149606299191, 0.07874015748031495954 ) ) ;
#30495 = DIRECTION ( 'NONE',  ( -0.000000000000000000, 0.7880107536067207930, -0.6156614753256598460 ) ) ;
#30496 = CARTESIAN_POINT ( 'NONE',  ( 0.1787899950787401604, -0.4163385826234020093, -0.07405724077823318263 ) ) ;
#30497 = DIRECTION ( 'NONE',  ( 0.000000000000000000, -1.000000000000000000, 0.000000000000000000 ) ) ;
#30498 = CARTESIAN_POINT ( 'NONE',  ( -1.094772975963752103E-17, -1.309547244040724312, -0.1787899950787401882 ) ) ;
#30499 = CARTESIAN_POINT ( 'NONE',  ( 0.6971942568897626646, -0.07405724077823297447, 0.2854330708123783422 ) ) ;
#30500 = CARTESIAN_POINT ( 'NONE',  ( -1.054774247047244540, -0.07405724077823318263, 1.830708661363559253 ) ) ;
#30501 = VERTEX_POINT ( 'NONE', #9268 ) ;
#30502 = CARTESIAN_POINT ( 'NONE',  ( -0.6971942568897637749, 2.189545951927499583E-17, 1.345964566875370139 ) ) ;
#30503 = CARTESIAN_POINT ( 'NONE',  ( 0.8759842519685039353, 0.000000000000000000, 4.498031496062992574 ) ) ;
#30504 = CARTESIAN_POINT ( 'NONE',  ( -0.6971942568897626646, 0.07405724077823318263, 0.5167322834108034613 ) ) ;
#30505 = CARTESIAN_POINT ( 'NONE',  ( 0.8759842519685039353, -0.1787899950787401882, 0.09596456687537047170 ) ) ;
#30506 = CARTESIAN_POINT ( 'NONE',  ( -1.054774247047244540, 0.07405724077823318263, 1.245078740103716886 ) ) ;
#30507 = DIRECTION ( 'NONE',  ( 0.000000000000000000, 0.000000000000000000, 1.000000000000000000 ) ) ;
#30508 = CARTESIAN_POINT ( 'NONE',  ( 0.05252291220399905175, -0.09842554669817424329, -0.1709337162269513322 ) ) ;
#30509 = DIRECTION ( 'NONE',  ( 0.000000000000000000, -0.6156614753256597350, -0.7880107536067207930 ) ) ;
#30510 = CARTESIAN_POINT ( 'NONE',  ( 0.9500414927467377701, 0.1787899950787401604, 0.4281496062454490659 ) ) ;
#30511 = CARTESIAN_POINT ( 'NONE',  ( -1.054774247047244540, 0.07405724077823318263, 0.4576771653005669016 ) ) ;
#30512 = CARTESIAN_POINT ( 'NONE',  ( -1.002407869896990045, -0.1264236179284866091, 0.8439960629383622681 ) ) ;
#30513 = VERTEX_POINT ( 'NONE', #24134 ) ;
#30514 = FACE_OUTER_BOUND ( 'NONE', #46244, .T. ) ;
#30515 = ORIENTED_EDGE ( 'NONE', *, *, #42303, .T. ) ;
#30516 = ORIENTED_EDGE ( 'NONE', *, *, #30403, .F. ) ;
#30517 = CARTESIAN_POINT ( 'NONE',  ( -0.8759842519685039353, 0.1574803149606299191, 0.2952755905511810774 ) ) ;
#30518 = CARTESIAN_POINT ( 'NONE',  ( -0.9500414927467377701, 0.1787899950787401604, 1.958661417269071947 ) ) ;
#30519 = CARTESIAN_POINT ( 'NONE',  ( -0.2559055118110235560, -0.1362856811059252049, -0.09992972387952742119 ) ) ;
#30520 = ORIENTED_EDGE ( 'NONE', *, *, #28717, .T. ) ;
#30521 = DIRECTION ( 'NONE',  ( 1.000000000000000000, 0.000000000000000000, 0.000000000000000000 ) ) ;
#30522 = VECTOR ( 'NONE', #21052, 39.37007874015748854 ) ;
#30523 = CARTESIAN_POINT ( 'NONE',  ( -0.9412147342319837628, -0.1574803149606297803, 0.3174212598425196763 ) ) ;
#30524 = DIRECTION ( 'NONE',  ( 1.000000000000000000, 0.000000000000000000, -0.000000000000000000 ) ) ;
#30525 = CARTESIAN_POINT ( 'NONE',  ( -0.1787899950787401604, -1.475517669016641165, -0.07405724077823318263 ) ) ;
#30526 = EDGE_LOOP ( 'NONE', ( #21220, #30162, #11050, #32882 ) ) ;
#30527 = DIRECTION ( 'NONE',  ( 1.000000000000000000, -0.000000000000000000, -0.000000000000000000 ) ) ;
#30528 = CARTESIAN_POINT ( 'NONE',  ( 0.1264236179284866091, -0.3794291338045042705, 0.1264236179284866091 ) ) ;
#30529 = LINE ( 'NONE', #45089, #908 ) ;
#30530 = VERTEX_POINT ( 'NONE', #23423 ) ;
#30531 = CARTESIAN_POINT ( 'NONE',  ( -0.02178664995562274928, 0.2829157040457837557, -0.2993662881636575679 ) ) ;
#30532 = LINE ( 'NONE', #1016, #24640 ) ;
#30533 = CARTESIAN_POINT ( 'NONE',  ( 0.1787899950787401604, -0.2194881889226144023, -0.07405724077823318263 ) ) ;
#30534 = CARTESIAN_POINT ( 'NONE',  ( -0.7185039370078746268, 0.06523048226347956391, 1.444389763779527991 ) ) ;
#30535 = CARTESIAN_POINT ( 'NONE',  ( 0.6971942568897648851, 0.07405724077823318263, 1.614173228292692386 ) ) ;
#30536 = CARTESIAN_POINT ( 'NONE',  ( 1.054774247047244540, -0.07405724077823318263, 0.1771653542769450751 ) ) ;
#30537 = CARTESIAN_POINT ( 'NONE',  ( 3.284318927891251994E-17, -1.727854330654897685, 0.1787899950787401882 ) ) ;
#30538 = APPLICATION_PROTOCOL_DEFINITION ( 'draft international standard', 'automotive_design', 1998, #32771 ) ;
#30539 = CARTESIAN_POINT ( 'NONE',  ( -0.9412147342319837628, 0.1574803149606300301, 1.739665354223181470 ) ) ;
#30540 = VERTEX_POINT ( 'NONE', #5423 ) ;
#30541 = EDGE_CURVE ( 'NONE', #3387, #32389, #22057, .T. ) ;
#30542 = CARTESIAN_POINT ( 'NONE',  ( -1.054774247047244540, 0.07405724077823318263, 0.6200787401037166635 ) ) ;
#30543 = CARTESIAN_POINT ( 'NONE',  ( -0.7646288533564489232, -0.1113553986120547346, 1.284448818790110192 ) ) ;
#30545 = CARTESIAN_POINT ( 'NONE',  ( 0.7185039370078739607, 1.928577636452523993E-17, 0.3838582677165354173 ) ) ;
#30544 = CARTESIAN_POINT ( 'NONE',  ( 2.892866454678787531E-17, -0.7657480314960629642, 0.1574803149606299191 ) ) ;
#30546 = CARTESIAN_POINT ( 'NONE',  ( -0.1270800023317771588, -1.580752471000367976, -0.1270800023317771588 ) ) ;
#30547 = DIRECTION ( 'NONE',  ( 0.000000000000000000, 0.000000000000000000, -1.000000000000000000 ) ) ;
#30548 = CARTESIAN_POINT ( 'NONE',  ( 0.06523048226347956391, -0.4384842518609765039, 0.1574803149606297803 ) ) ;
#30549 = CARTESIAN_POINT ( 'NONE',  ( 0.2471922904502826257, 0.09142184925108906568, -0.04493454898960681093 ) ) ;
#30550 = CARTESIAN_POINT ( 'NONE',  ( 0.6971942568897648851, 0.07405724077823318263, 1.771653543253322249 ) ) ;
#30551 = CARTESIAN_POINT ( 'NONE',  ( 1.054774247047244540, 0.07405724077823318263, 0.3001968503399373711 ) ) ;
#30552 = VECTOR ( 'NONE', #44120, 39.37007874015748854 ) ;
#30553 = EDGE_LOOP ( 'NONE', ( #43538, #23185, #6186, #39140 ) ) ;
#30554 = DIRECTION ( 'NONE',  ( 0.8191520442889873577, 0.000000000000000000, 0.5735764363510523767 ) ) ;
#30555 = EDGE_CURVE ( 'NONE', #38458, #14046, #23648, .T. ) ;
#30556 = CARTESIAN_POINT ( 'NONE',  ( -1.033464566929134687, -0.06523048226347956391, 1.454232283357038691 ) ) ;
#30557 = LINE ( 'NONE', #27442, #7591 ) ;
#30558 = CARTESIAN_POINT ( 'NONE',  ( -0.1787899950787401604, 0.1151574803687242243, 0.07405724077823318263 ) ) ;
#30559 = VECTOR ( 'NONE', #124, 39.37007874015748143 ) ;
#30560 = CARTESIAN_POINT ( 'NONE',  ( 0.8759842519685039353, 0.1787899950787401882, 0.5044291338045039375 ) ) ;
#30561 = DIRECTION ( 'NONE',  ( 0.000000000000000000, 0.000000000000000000, 1.000000000000000000 ) ) ;
#30562 = CARTESIAN_POINT ( 'NONE',  ( -0.7185039370078739607, 1.928577636452523993E-17, 1.594488188868850242 ) ) ;
#30563 = CARTESIAN_POINT ( 'NONE',  ( 0.2821522309711287368, -0.08090551181102362266, 0.000000000000000000 ) ) ;
#30564 = CARTESIAN_POINT ( 'NONE',  ( 0.9412147342319837628, 0.1574803149606300301, 0.7554133857192455448 ) ) ;
#30565 = ORIENTED_EDGE ( 'NONE', *, *, #34773, .T. ) ;
#30566 = PLANE ( 'NONE',  #13075 ) ;
#30567 = EDGE_LOOP ( 'NONE', ( #37857, #33337, #22420, #2637 ) ) ;
#30568 = CARTESIAN_POINT ( 'NONE',  ( 0.07444174185955046430, -0.09207136863816363370, -0.1797182628040039087 ) ) ;
#30569 = CARTESIAN_POINT ( 'NONE',  ( 3.284318927891251994E-17, -1.373523621993480326, 0.1787899950787401882 ) ) ;
#30570 = CARTESIAN_POINT ( 'NONE',  ( -0.9873396505805591694, 0.1113553986120547346, 0.5954724408373543998 ) ) ;
#30571 = CYLINDRICAL_SURFACE ( 'NONE', #31649, 0.1574803149606299191 ) ;
#30572 = CARTESIAN_POINT ( 'NONE',  ( 0.8019270111902717657, -0.1787899950787401604, 1.624015747977732849 ) ) ;
#30573 = CARTESIAN_POINT ( 'NONE',  ( -0.8107537697050253289, 0.1574803149606300301, 1.281988188976378895 ) ) ;
#30574 = CARTESIAN_POINT ( 'NONE',  ( 0.8107537697050254399, 0.1574803149606300301, 0.2485236219397169988 ) ) ;
#30575 = DIRECTION ( 'NONE',  ( 0.000000000000000000, -1.000000000000000000, 0.000000000000000000 ) ) ;
#30576 = CARTESIAN_POINT ( 'NONE',  ( 0.7646288533564489232, -0.1113553986120547346, 1.363188976270427455 ) ) ;
#30577 = ORIENTED_EDGE ( 'NONE', *, *, #40660, .T. ) ;
#30578 = EDGE_LOOP ( 'NONE', ( #247, #46461, #11469, #22354 ) ) ;
#30579 = CARTESIAN_POINT ( 'NONE',  ( -0.03313107868980413873, -0.09812580651453278735, 0.1546376223675618999 ) ) ;
#30580 = CARTESIAN_POINT ( 'NONE',  ( -0.7495606340400177148, -0.1264236179284866091, 1.582185039316315045 ) ) ;
#30581 = CARTESIAN_POINT ( 'NONE',  ( 0.06523048226347956391, -0.08415354319955967166, 0.1574803149606297803 ) ) ;
#30582 = CARTESIAN_POINT ( 'NONE',  ( -1.054774247047244540, 0.07405724077823318263, 1.210629921206079818 ) ) ;
#30583 = ORIENTED_EDGE ( 'NONE', *, *, #7103, .T. ) ;
#30584 = EDGE_CURVE ( 'NONE', #28921, #9031, #34683, .T. ) ;
#30585 = DIRECTION ( 'NONE',  ( -1.000000000000000000, 0.000000000000000000, -7.047314121155770932E-15 ) ) ;
#30586 = AXIS2_PLACEMENT_3D ( 'NONE', #15927, #37721, #41271 ) ;
#30587 = CARTESIAN_POINT ( 'NONE',  ( -0.6971942568897637749, 2.189545951927499583E-17, 0.3223425196312759144 ) ) ;
#30588 = CARTESIAN_POINT ( 'NONE',  ( -0.1377952755905510196, 1.687505431895957647E-17, -0.1828167807439035619 ) ) ;
#30589 = CARTESIAN_POINT ( 'NONE',  ( 0.000000000000000000, 0.09842519685039370636, 0.000000000000000000 ) ) ;
#30590 = CARTESIAN_POINT ( 'NONE',  ( 0.1264236179284866091, -0.9464822359457736312, 0.1264236179284866091 ) ) ;
#30591 = ORIENTED_EDGE ( 'NONE', *, *, #21119, .F. ) ;
#30592 = CARTESIAN_POINT ( 'NONE',  ( 0.1264236179284866091, -0.01525590545804753929, -0.1264236179284866091 ) ) ;
#30593 = ORIENTED_EDGE ( 'NONE', *, *, #7370, .T. ) ;
#30594 = CARTESIAN_POINT ( 'NONE',  ( -0.2559077310846238351, -0.04350174606802800076, -0.3128500747680653116 ) ) ;
#30595 = AXIS2_PLACEMENT_3D ( 'NONE', #18756, #46810, #33182 ) ;
#30596 = DIRECTION ( 'NONE',  ( 1.000000000000000000, 0.000000000000000000, 0.000000000000000000 ) ) ;
#30597 = CARTESIAN_POINT ( 'NONE',  ( 0.1787899950787401604, -0.6574803149068665364, 0.07405724077823318263 ) ) ;
#30598 = EDGE_CURVE ( 'NONE', #14105, #27412, #6109, .T. ) ;
#30599 = CARTESIAN_POINT ( 'NONE',  ( -0.8107537697050253289, 0.1574803149606300301, 0.8882874015748027929 ) ) ;
#30600 = CARTESIAN_POINT ( 'NONE',  ( 0.5236220472440944462, 0.08090551181102362266, 9.908067607274841931E-18 ) ) ;
#30601 = CARTESIAN_POINT ( 'NONE',  ( 0.1797182628040039087, -1.046795778086983653, 0.07444174185955046430 ) ) ;
#30602 = CARTESIAN_POINT ( 'NONE',  ( 0.8759842519685039353, -0.1574803149606299191, 1.102362204724409489 ) ) ;
#30603 = CARTESIAN_POINT ( 'NONE',  ( 0.9500414927467378812, 0.1787899950787401604, 0.9005905511273389896 ) ) ;
#30604 = CARTESIAN_POINT ( 'NONE',  ( 0.04485236092672652969, 0.3740157480314960647, 1.206847064312616125 ) ) ;
#30605 = EDGE_CURVE ( 'NONE', #18242, #32474, #1828, .T. ) ;
#30606 = CARTESIAN_POINT ( 'NONE',  ( 0.7185039370078739607, 1.928577636452523993E-17, 1.564960629921259949 ) ) ;
#30608 = CARTESIAN_POINT ( 'NONE',  ( 0.6195511811023606263, 0.4133858267716528090, 0.9891732283464566011 ) ) ;
#30607 = CARTESIAN_POINT ( 'NONE',  ( 0.7162330157071907788, 0.04010186468405893545, 1.982507691646586245 ) ) ;
#30609 = DIRECTION ( 'NONE',  ( 1.000000000000000000, 0.000000000000000000, -1.822029033848725275E-16 ) ) ;
#30610 = CARTESIAN_POINT ( 'NONE',  ( 0.1574803149606299191, -0.7066929132782991951, -1.928577636452523993E-17 ) ) ;
#30611 = CARTESIAN_POINT ( 'NONE',  ( -0.9412147342319837628, 0.1574803149606300301, 1.621555118002709683 ) ) ;
#30612 = CARTESIAN_POINT ( 'NONE',  ( 0.1264236179284866091, 0.1028543307624250058, -0.1264236179284866091 ) ) ;
#30613 = DIRECTION ( 'NONE',  ( 0.8191520442889873577, 0.000000000000000000, 0.5735764363510523767 ) ) ;
#30614 = CARTESIAN_POINT ( 'NONE',  ( 1.054774247047244540, -0.07405724077823318263, 0.9645669290800954476 ) ) ;
#30615 = CARTESIAN_POINT ( 'NONE',  ( 1.002407869896990045, 0.1264236179284866091, 1.882381889710015743 ) ) ;
#30616 = CARTESIAN_POINT ( 'NONE',  ( 0.07405724077823318263, -0.9724409448281265966, 0.1787899950787401604 ) ) ;
#30617 = CARTESIAN_POINT ( 'NONE',  ( 0.7185039370078746268, -0.06523048226347956391, 0.2977362203649139283 ) ) ;
#30618 = ORIENTED_EDGE ( 'NONE', *, *, #19305, .T. ) ;
#30619 = CARTESIAN_POINT ( 'NONE',  ( 0.7185039370078746268, -0.06523048226347956391, 0.4158464565853863260 ) ) ;
#30620 = CARTESIAN_POINT ( 'NONE',  ( 0.7646288533564489232, -0.1113553986120547346, 1.884842519685039353 ) ) ;
#30621 = CARTESIAN_POINT ( 'NONE',  ( 0.1574803149606300301, -1.693405511703496957, 0.06523048226347956391 ) ) ;
#30622 = CARTESIAN_POINT ( 'NONE',  ( -0.9873396505805591694, 0.1113553986120547346, 0.1230314959554651699 ) ) ;
#30623 = CARTESIAN_POINT ( 'NONE',  ( 0.7495606340400177148, 0.1264236179284866091, 1.139271653489543290 ) ) ;
#30624 = LINE ( 'NONE', #22211, #15791 ) ;
#30626 = VECTOR ( 'NONE', #22818, 39.37007874015748854 ) ;
#30625 = CARTESIAN_POINT ( 'NONE',  ( -0.07405724077823318263, 0.1250000000537635492, 0.1787899950787401604 ) ) ;
#30627 = CARTESIAN_POINT ( 'NONE',  ( 0.2066929133858268486, 0.3648440108500932699, -3.619166627704267114 ) ) ;
#30628 = ( BOUNDED_CURVE ( )  B_SPLINE_CURVE ( 2, ( #39048, #10316, #42857, #28788, #18205, #10070, #24686, #46954, #46476 ),
 .UNSPECIFIED., .F., .F. ) 
 B_SPLINE_CURVE_WITH_KNOTS ( ( 3, 2, 2, 2, 3 ),
 ( 0.1150000000000000050, 0.1174999999999999933, 0.1199999999999999956, 0.1224999999999999978, 0.1250000000000000000 ),
 .UNSPECIFIED. ) 
 CURVE ( )  GEOMETRIC_REPRESENTATION_ITEM ( )  RATIONAL_B_SPLINE_CURVE ( ( 1.000000000000000000, 0.9238795325112869605, 1.000000000000000000, 0.9238795325112869605, 1.000000000000000000, 0.9238795325112869605, 1.000000000000000000, 0.9238795325112869605, 1.000000000000000000 ) ) 
 REPRESENTATION_ITEM ( '' )  ) ;
#30629 = CARTESIAN_POINT ( 'NONE',  ( -0.9500414927467378812, 0.1787899950787401604, 0.6594488188438737408 ) ) ;
#30630 = CARTESIAN_POINT ( 'NONE',  ( -0.7185039370078739607, 1.928577636452523993E-17, 0.2657480314960630197 ) ) ;
#30631 = CARTESIAN_POINT ( 'NONE',  ( -0.9500414927467378812, 0.1787899950787401604, 0.2657480314422993595 ) ) ;
#30632 = VERTEX_POINT ( 'NONE', #16924 ) ;
#30633 = CIRCLE ( 'NONE', #4545, 0.08090551181102362266 ) ;
#30634 = ORIENTED_EDGE ( 'NONE', *, *, #44495, .T. ) ;
#30635 = CARTESIAN_POINT ( 'NONE',  ( -0.07405724077823318263, -1.494094488135213394, 0.1787899950787401604 ) ) ;
#30636 = CARTESIAN_POINT ( 'NONE',  ( -0.8019270111902717657, 0.1787899950787401604, 1.884842519631275026 ) ) ;
#30637 = CARTESIAN_POINT ( 'NONE',  ( -1.054774247047244540, 0.07405724077823318263, 1.008858267662772423 ) ) ;
#30638 = CARTESIAN_POINT ( 'NONE',  ( -0.8019270111902717657, -0.1787899950787401604, 0.4872047243556847929 ) ) ;
#30639 = CARTESIAN_POINT ( 'NONE',  ( -0.1476377952755905387, -0.4075443641102559078, -0.9311509272141712534 ) ) ;
#30640 = CARTESIAN_POINT ( 'NONE',  ( -1.033464566929133799, 0.000000000000000000, 1.663385826771653697 ) ) ;
#30641 = CARTESIAN_POINT ( 'NONE',  ( -0.07405724077823318263, -0.5207932595678214094, 0.1787899950787401604 ) ) ;
#30642 = CARTESIAN_POINT ( 'NONE',  ( -0.1639078578912291362, -0.08956131775089744285, -0.05627608123246346378 ) ) ;
#30643 = CARTESIAN_POINT ( 'NONE',  ( 0.7646288533564489232, 0.1113553986120547346, 1.796259842519684957 ) ) ;
#30644 = CARTESIAN_POINT ( 'NONE',  ( 0.5113546317124669782, 4.466152701071653354E-17, 0.000000000000000000 ) ) ;
#30645 = CARTESIAN_POINT ( 'NONE',  ( 0.2559055150599270911, -0.04346181788127674583, -0.03525533988057383966 ) ) ;
#30646 = ( BOUNDED_CURVE ( )  B_SPLINE_CURVE ( 2, ( #33329, #7889, #35784, #26369, #24758, #33091, #17327, #22747, #11748 ),
 .UNSPECIFIED., .F., .T. ) 
 B_SPLINE_CURVE_WITH_KNOTS ( ( 3, 2, 2, 2, 3 ),
 ( 0.5600000000000000533, 0.5625000000000000000, 0.5649999999999999467, 0.5675000000000000044, 0.5699999999999999512 ),
 .UNSPECIFIED. ) 
 CURVE ( )  GEOMETRIC_REPRESENTATION_ITEM ( )  RATIONAL_B_SPLINE_CURVE ( ( 1.000000000000000000, 0.9238795325112869605, 1.000000000000000000, 0.9238795325112869605, 1.000000000000000000, 0.9238795325112869605, 1.000000000000000000, 0.9238795325112829637, 1.000000000000000000 ) ) 
 REPRESENTATION_ITEM ( '' )  ) ;
#30647 = CARTESIAN_POINT ( 'NONE',  ( -0.8019270111902717657, -0.1787899950787401604, 0.4822834645131655606 ) ) ;
#30648 = LINE ( 'NONE', #34707, #33803 ) ;
#30649 = ORIENTED_EDGE ( 'NONE', *, *, #4967, .F. ) ;
#30650 = FACE_OUTER_BOUND ( 'NONE', #32944, .T. ) ;
#30651 = EDGE_CURVE ( 'NONE', #15079, #40074, #34923, .T. ) ;
#30652 = CARTESIAN_POINT ( 'NONE',  ( -0.8019270111902716547, 0.1787899950787401604, 1.535433070812378675 ) ) ;
#30653 = CARTESIAN_POINT ( 'NONE',  ( -0.1787899950787401882, -1.501476377898992354, 0.000000000000000000 ) ) ;
#30654 = AXIS2_PLACEMENT_3D ( 'NONE', #5437, #27526, #38751 ) ;
#30655 = CARTESIAN_POINT ( 'NONE',  ( 0.1264236179284866091, -1.599901574749385880, 0.1264236179284866091 ) ) ;
#30656 = EDGE_CURVE ( 'NONE', #9464, #11301, #31100, .T. ) ;
#30657 = CARTESIAN_POINT ( 'NONE',  ( 0.2944196465027555387, 4.766607801171850497E-17, 0.000000000000000000 ) ) ;
#30658 = CARTESIAN_POINT ( 'NONE',  ( 0.9873396505805591694, 0.1113553986120547346, 0.9596456692913386544 ) ) ;
#30659 = CARTESIAN_POINT ( 'NONE',  ( 0.7185039370078739607, 1.928577636452523993E-17, 0.5019685039370078705 ) ) ;
#30660 = DIRECTION ( 'NONE',  ( 1.000000000000000000, -0.000000000000000000, -0.000000000000000000 ) ) ;
#30661 = CARTESIAN_POINT ( 'NONE',  ( -0.9873396505805591694, -0.1113553986120547346, 1.176181102254677313 ) ) ;
#30662 = CARTESIAN_POINT ( 'NONE',  ( 0.9500414927467378812, 0.1787899950787401604, 0.5856299212060785964 ) ) ;
#30663 = CARTESIAN_POINT ( 'NONE',  ( 0.7495606340400177148, -0.1264236179284866091, 0.08612204719033110523 ) ) ;
#30664 = CARTESIAN_POINT ( 'NONE',  ( -0.06523048226347956391, -0.4680118110236219930, -0.1574803149606300301 ) ) ;
#30665 = CARTESIAN_POINT ( 'NONE',  ( -0.7185039370078746268, 0.06523048226347956391, 0.4207677165354331561 ) ) ;
#30666 = ORIENTED_EDGE ( 'NONE', *, *, #37045, .F. ) ;
#30667 = CARTESIAN_POINT ( 'NONE',  ( 0.7185039370078739607, 1.928577636452523993E-17, 1.722440944881889813 ) ) ;
#30668 = EDGE_CURVE ( 'NONE', #30331, #2867, #35152, .T. ) ;
#30669 = CARTESIAN_POINT ( 'NONE',  ( -1.054774247047244540, -0.07405724077823318263, 1.048228346402928723 ) ) ;
#30670 = CARTESIAN_POINT ( 'NONE',  ( 0.8107537697050253289, -0.1574803149606297803, 1.139271653543306506 ) ) ;
#30671 = CARTESIAN_POINT ( 'NONE',  ( -0.9091039872111508213, -0.1724160430076012163, 1.988772421918897360 ) ) ;
#30672 = LINE ( 'NONE', #19853, #12892 ) ;
#30673 = EDGE_CURVE ( 'NONE', #18878, #1893, #16004, .T. ) ;
#30674 = CYLINDRICAL_SURFACE ( 'NONE', #28408, 0.3937007874015748254 ) ;
#30675 = CARTESIAN_POINT ( 'NONE',  ( -0.7185039370078739607, 1.928577636452523993E-17, 1.250000000000000000 ) ) ;
#30676 = CARTESIAN_POINT ( 'NONE',  ( -0.07117121207836790697, -0.08956324299011318713, 0.1404802767937309016 ) ) ;
#30677 = CARTESIAN_POINT ( 'NONE',  ( 0.07405724077823318263, -0.4852362204186770889, -0.1787899950787401604 ) ) ;
#30678 = ORIENTED_EDGE ( 'NONE', *, *, #25831, .T. ) ;
#30679 = CARTESIAN_POINT ( 'NONE',  ( 0.8107537697050254399, 0.1574803149606300301, 1.163877952755904666 ) ) ;
#30680 = CARTESIAN_POINT ( 'NONE',  ( -0.9873396505805591694, 0.1113553986120547346, 1.117125984251968518 ) ) ;
#30681 = VERTEX_POINT ( 'NONE', #8787 ) ;
#30682 = CARTESIAN_POINT ( 'NONE',  ( -1.033464566929134687, 0.06523048226347956391, 1.774114173120820093 ) ) ;
#30683 = DIRECTION ( 'NONE',  ( 0.000000000000000000, -1.000000000000000000, 0.000000000000000000 ) ) ;
#30684 = CARTESIAN_POINT ( 'NONE',  ( 0.1787899950787401882, -1.752460629867496067, -2.189545951927503898E-17 ) ) ;
#30685 = CARTESIAN_POINT ( 'NONE',  ( -0.1264236179284866091, -0.9552165353793071745, -0.1264236179284866091 ) ) ;
#30686 = CARTESIAN_POINT ( 'NONE',  ( -0.06523048226347956391, -1.280019685039369470, 0.1574803149606297803 ) ) ;
#30687 = CARTESIAN_POINT ( 'NONE',  ( 0.9873396505805591694, 0.1113553986120547346, 1.107283464459401623 ) ) ;
#30688 = CARTESIAN_POINT ( 'NONE',  ( 0.2066929133858268486, -0.5175744617845221551, -0.9076376772307632734 ) ) ;
#30689 = ORIENTED_EDGE ( 'NONE', *, *, #15019, .F. ) ;
#30690 = ORIENTED_EDGE ( 'NONE', *, *, #30651, .F. ) ;
#30691 = CARTESIAN_POINT ( 'NONE',  ( -1.054774247047244096, 0.000000000000000000, 1.719980314906866203 ) ) ;
#30692 = CARTESIAN_POINT ( 'NONE',  ( 0.9500414927467378812, 0.1787899950787401604, 1.884842519631275026 ) ) ;
#30693 = EDGE_LOOP ( 'NONE', ( #26911, #35743, #34046, #27988, #23121, #41368 ) ) ;
#30694 = DIRECTION ( 'NONE',  ( 0.000000000000000000, 0.2432573283306889156, -0.9699617890481125881 ) ) ;
#30695 = CARTESIAN_POINT ( 'NONE',  ( 0.9500414927467378812, -0.1787899950787401604, 0.4133858267178901480 ) ) ;
#30696 = CARTESIAN_POINT ( 'NONE',  ( -1.002407869896990045, -0.1264236179284866091, 1.395177165300567124 ) ) ;
#30697 = CARTESIAN_POINT ( 'NONE',  ( -0.7185039370078739607, 1.928577636452523993E-17, 1.791338582569637738 ) ) ;
#30698 = CARTESIAN_POINT ( 'NONE',  ( -1.054774247047244096, 0.000000000000000000, 0.8882874015210394658 ) ) ;
#30699 = CARTESIAN_POINT ( 'NONE',  ( -0.8019270111902717657, 0.1787899950787401604, 0.07874015742655145200 ) ) ;
#30700 = CARTESIAN_POINT ( 'NONE',  ( -0.2064293380533802347, 0.06762482675900732820, -0.1662510369723865233 ) ) ;
#30701 = CARTESIAN_POINT ( 'NONE',  ( -0.8019270111902717657, -0.1787899950787401604, 1.747047244040724312 ) ) ;
#30702 = CARTESIAN_POINT ( 'NONE',  ( -0.8759842519685039353, 0.1787899950787401882, 0.07627952750529173875 ) ) ;
#30703 = CARTESIAN_POINT ( 'NONE',  ( -1.033464566929134687, -0.06523048226347956391, 1.739665354330709013 ) ) ;
#30704 = CARTESIAN_POINT ( 'NONE',  ( -0.9412147342319837628, -0.1574803149606297803, 0.9473425196850396857 ) ) ;
#30705 = CARTESIAN_POINT ( 'NONE',  ( 1.054774247047244540, 0.07405724077823318263, 1.643700787347811998 ) ) ;
#30706 = CARTESIAN_POINT ( 'NONE',  ( -0.2281650204108027769, -0.09842519685039370636, -0.09074154274604251391 ) ) ;
#30707 = FACE_OUTER_BOUND ( 'NONE', #17451, .T. ) ;
#30708 = ADVANCED_FACE ( 'NONE', ( #38026 ), #5185, .T. ) ;
#30709 = ORIENTED_EDGE ( 'NONE', *, *, #23549, .F. ) ;
#30710 = EDGE_CURVE ( 'NONE', #11484, #43833, #1584, .T. ) ;
#30711 = CARTESIAN_POINT ( 'NONE',  ( -0.6971942568897637749, 2.189545951927499583E-17, 1.188484251914740275 ) ) ;
#30712 = CARTESIAN_POINT ( 'NONE',  ( -0.1787899950787401604, -1.026574803095842370, -0.07405724077823318263 ) ) ;
#30713 = DIRECTION ( 'NONE',  ( 1.822029033848725028E-16, 0.000000000000000000, 1.000000000000000000 ) ) ;
#30714 = CARTESIAN_POINT ( 'NONE',  ( 0.6971942568897648851, -0.07405724077823297447, 1.855314960576157635 ) ) ;
#30715 = CARTESIAN_POINT ( 'NONE',  ( -0.1797182628040039087, -0.3184493213940693401, -0.07444174185955065859 ) ) ;
#30716 = CARTESIAN_POINT ( 'NONE',  ( 0.1574803149606299191, -1.769685039262551163, -1.928577636452523993E-17 ) ) ;
#30717 = CARTESIAN_POINT ( 'NONE',  ( -0.9412147342319837628, 0.1574803149606300301, 0.7554133857192455448 ) ) ;
#30718 = CARTESIAN_POINT ( 'NONE',  ( -0.1574803149606299191, 0.1692913385826771699, 0.000000000000000000 ) ) ;
#30719 = AXIS2_PLACEMENT_3D ( 'NONE', #20737, #35378, #2522 ) ;
#30720 = CARTESIAN_POINT ( 'NONE',  ( 0.07405724077823318263, -0.1899606298674962612, 0.1787899950787401604 ) ) ;
#30721 = CARTESIAN_POINT ( 'NONE',  ( -0.1574803149606299191, 0.000000000000000000, -0.2357204724409448504 ) ) ;
#30722 = CARTESIAN_POINT ( 'NONE',  ( 1.054774247047244540, -0.07405724077823318263, 1.003937007820251193 ) ) ;
#30723 = AXIS2_PLACEMENT_3D ( 'NONE', #21309, #3347, #36651 ) ;
#30725 = CARTESIAN_POINT ( 'NONE',  ( 0.1565984635743035980, -0.01350052470311071708, 0.1403812994535005576 ) ) ;
#30724 = CARTESIAN_POINT ( 'NONE',  ( -0.1534195868007023067, 1.482597719745565312, -0.3467144894627436913 ) ) ;
#30726 = CARTESIAN_POINT ( 'NONE',  ( -0.7646288533564489232, 0.1113553986120547346, 1.313976377845228249 ) ) ;
#30727 = CARTESIAN_POINT ( 'NONE',  ( 1.002407869896990045, -0.1264236179284866091, 1.951279527505291433 ) ) ;
#30728 = ORIENTED_EDGE ( 'NONE', *, *, #6046, .F. ) ;
#30729 = CARTESIAN_POINT ( 'NONE',  ( 0.8759842519685039353, 0.1574803149606299191, 0.1771653543307086520 ) ) ;
#30730 = DIRECTION ( 'NONE',  ( 1.000000000000000000, -0.000000000000000000, 1.224646799147353207E-16 ) ) ;
#30731 = CARTESIAN_POINT ( 'NONE',  ( -0.07405724077823318263, -0.4064960629383624346, -0.1787899950787401604 ) ) ;
#30732 = LINE ( 'NONE', #12519, #23206 ) ;
#30733 = CARTESIAN_POINT ( 'NONE',  ( 0.1264236179284866091, -1.196358267662771757, -0.1264236179284866091 ) ) ;
#30734 = CARTESIAN_POINT ( 'NONE',  ( 0.8759842519685039353, 0.1787899950787401882, 0.3518700786863940833 ) ) ;
#30735 = CARTESIAN_POINT ( 'NONE',  ( -0.6971942568897648851, -0.07405724077823297447, 1.737204724355685848 ) ) ;
#30736 = ORIENTED_EDGE ( 'NONE', *, *, #36302, .F. ) ;
#30737 = CARTESIAN_POINT ( 'NONE',  ( -0.7495606340400177148, -0.1264236179284866091, 1.232775590497417362 ) ) ;
#30738 = CARTESIAN_POINT ( 'NONE',  ( 1.054774247047244540, 0.07405724077823318263, 1.368110236166710125 ) ) ;
#30739 = CARTESIAN_POINT ( 'NONE',  ( -1.002407869896990045, 0.1264236179284866091, 0.5437992125446614589 ) ) ;
#30740 = CARTESIAN_POINT ( 'NONE',  ( -0.6971942568897648851, 0.07405724077823318263, 1.220472440891118504 ) ) ;
#30741 = CARTESIAN_POINT ( 'NONE',  ( 0.8070866141732283561, -0.0009842519685049383633, 0.7574803149606299524 ) ) ;
#30742 = CARTESIAN_POINT ( 'NONE',  ( 0.03732658744263399331, -0.09842026076056133166, -0.1748521113903349911 ) ) ;
#30743 = CARTESIAN_POINT ( 'NONE',  ( 0.8019270111902716547, 0.1787899950787401604, 0.4330708660879683536 ) ) ;
#30744 = CARTESIAN_POINT ( 'NONE',  ( -0.8759842519685039353, 0.1787899950787401882, 0.4256889763241890057 ) ) ;
#30745 = CARTESIAN_POINT ( 'NONE',  ( -0.7495606340400177148, 0.1264236179284866091, 0.8243110235682834519 ) ) ;
#30746 = ORIENTED_EDGE ( 'NONE', *, *, #20407, .T. ) ;
#30747 = SURFACE_STYLE_USAGE ( .BOTH. , #23542 ) ;
#30748 = AXIS2_PLACEMENT_3D ( 'NONE', #7876, #664, #15319 ) ;
#30749 = DIRECTION ( 'NONE',  ( -6.679788269418529283E-17, 1.000000000000000000, 0.000000000000000000 ) ) ;
#30750 = ORIENTED_EDGE ( 'NONE', *, *, #2215, .T. ) ;
#30751 = VERTEX_POINT ( 'NONE', #47094 ) ;
#30752 = CARTESIAN_POINT ( 'NONE',  ( -0.9873396505805591694, -0.1113553986120547346, 0.3198818897637795700 ) ) ;
#30753 = CARTESIAN_POINT ( 'NONE',  ( 1.054774247047244540, 0.07405724077823318263, 1.131889763725763887 ) ) ;
#30754 = CARTESIAN_POINT ( 'NONE',  ( 1.033464566929133799, 0.000000000000000000, 1.929133858160188897 ) ) ;
#30755 = LINE ( 'NONE', #12542, #31765 ) ;
#30756 = VERTEX_POINT ( 'NONE', #42756 ) ;
#30757 = VECTOR ( 'NONE', #38263, 39.37007874015748854 ) ;
#30758 = EDGE_CURVE ( 'NONE', #43422, #183, #18107, .T. ) ;
#30759 = FACE_OUTER_BOUND ( 'NONE', #19117, .T. ) ;
#30760 = CIRCLE ( 'NONE', #26921, 0.2952755905511810774 ) ;
#30761 = CARTESIAN_POINT ( 'NONE',  ( -0.9500414927467378812, -0.1787899950787401604, 0.9251968503399374821 ) ) ;
#30762 = SHAPE_REPRESENTATION ( 'Base Plate', ( #20860 ), #14766 ) ;
#30763 = EDGE_CURVE ( 'NONE', #42760, #5875, #20707, .T. ) ;
#30764 = CARTESIAN_POINT ( 'NONE',  ( 0.1645805237892204731, -0.1627998762483228723, 0.0008383936782243070051 ) ) ;
#30765 = CARTESIAN_POINT ( 'NONE',  ( -1.054774247047244540, 0.07405724077823318263, 0.02460629915883492599 ) ) ;
#30766 = CARTESIAN_POINT ( 'NONE',  ( 0.1264236179284866091, -1.566560976103254177, -0.1264236179284866091 ) ) ;
#30767 = EDGE_LOOP ( 'NONE', ( #2886, #29669, #5466, #43721, #28202, #32234, #22996, #12117 ) ) ;
#30768 = CARTESIAN_POINT ( 'NONE',  ( -1.033464566929133799, 1.928577636452524610E-17, 2.869337061179095023E-17 ) ) ;
#30769 = CARTESIAN_POINT ( 'NONE',  ( 0.07405724077823318263, -0.4064960629383624346, -0.1787899950787401604 ) ) ;
#30770 = ADVANCED_FACE ( 'NONE', ( #17158 ), #21216, .T. ) ;
#30771 = DIRECTION ( 'NONE',  ( -1.000000000000000000, 0.000000000000000000, 0.000000000000000000 ) ) ;
#30772 = CARTESIAN_POINT ( 'NONE',  ( 0.8019270111902717657, 0.1787899950787401604, 1.294291338528912982 ) ) ;
#30773 = EDGE_CURVE ( 'NONE', #25251, #44020, #28523, .T. ) ;
#30774 = CARTESIAN_POINT ( 'NONE',  ( -0.07669050334325228091, 0.2512157378947911801, -0.3110703821945135505 ) ) ;
#30775 = CARTESIAN_POINT ( 'NONE',  ( 0.5358894627757212481, -0.09842519685039370636, 1.205361022782828805E-17 ) ) ;
#30776 = CARTESIAN_POINT ( 'NONE',  ( 1.033464566929133799, 0.000000000000000000, 0.1968503935932602311 ) ) ;
#30777 = CARTESIAN_POINT ( 'NONE',  ( 0.1264236179284866091, -1.801673228292693052, 0.1264236179284866091 ) ) ;
#30778 = APPLICATION_PROTOCOL_DEFINITION ( 'draft international standard', 'automotive_design', 1998, #38264 ) ;
#30779 = DIRECTION ( 'NONE',  ( 0.000000000000000000, 0.000000000000000000, 1.000000000000000000 ) ) ;
#30780 = AXIS2_PLACEMENT_3D ( 'NONE', #3463, #18317, #9781 ) ;
#30781 = CARTESIAN_POINT ( 'NONE',  ( -0.8019270111902716547, 0.1787899950787401604, 0.5905511810485987167 ) ) ;
#30783 = CARTESIAN_POINT ( 'NONE',  ( 0.7185039370078739607, 0.000000000000000000, 4.498031496062992574 ) ) ;
#30782 = CARTESIAN_POINT ( 'NONE',  ( 0.1574803149606300301, -0.7189960629921270385, 0.06523048226347956391 ) ) ;
#30784 = CARTESIAN_POINT ( 'NONE',  ( -0.07444174185955065859, -1.647189478874384605, 0.1797182628040039087 ) ) ;
#30785 = CARTESIAN_POINT ( 'NONE',  ( 3.060083392313581123E-15, 0.5288907983920048128, -0.7507079620615672022 ) ) ;
#30786 = CARTESIAN_POINT ( 'NONE',  ( -0.1113553986120547346, -0.4557086613097952599, -0.1113553986120547346 ) ) ;
#30787 = DIRECTION ( 'NONE',  ( 1.000000000000000000, 0.000000000000000000, 0.000000000000000000 ) ) ;
#30788 = CARTESIAN_POINT ( 'NONE',  ( 0.7495606340400177148, 0.1264236179284866091, 1.498523621993480326 ) ) ;
#30789 = CARTESIAN_POINT ( 'NONE',  ( 0.9500414927467377701, -0.1787899950787401604, 1.904527559001354398 ) ) ;
#30790 = CARTESIAN_POINT ( 'NONE',  ( 0.9500414927467377701, 0.1787899950787401604, 0.3051181101824569919 ) ) ;
#30791 = CIRCLE ( 'NONE', #3208, 0.1377952755905511861 ) ;
#30792 = AXIS2_PLACEMENT_3D ( 'NONE', #29412, #4389, #11857 ) ;
#30794 = VERTEX_POINT ( 'NONE', #10700 ) ;
#30793 = CARTESIAN_POINT ( 'NONE',  ( 0.000000000000000000, 0.1299212598425196763, 0.000000000000000000 ) ) ;
#30795 = CARTESIAN_POINT ( 'NONE',  ( 0.1574803149606299191, 0.1473293504822035527, -0.5595480905233944924 ) ) ;
#30796 = LINE ( 'NONE', #26954, #6038 ) ;
#30797 = CARTESIAN_POINT ( 'NONE',  ( -1.094772975963752103E-17, 0.1028543307624250058, -0.1787899950787401882 ) ) ;
#30798 = CARTESIAN_POINT ( 'NONE',  ( -0.9873396505805591694, 0.1113553986120547346, 0.1722440944881890035 ) ) ;
#30799 = CARTESIAN_POINT ( 'NONE',  ( 0.8759842519685039353, 0.1787899950787401882, 0.3863188975840318173 ) ) ;
#30800 = DIRECTION ( 'NONE',  ( 1.000000000000000000, 0.000000000000000000, 0.000000000000000000 ) ) ;
#30801 = CARTESIAN_POINT ( 'NONE',  ( 1.614954907737318939E-16, 0.1564960629921311464, 0.3937007874015748254 ) ) ;
#30802 = CARTESIAN_POINT ( 'NONE',  ( -0.9500414927467378812, 0.1787899950787401604, 1.328740157426552049 ) ) ;
#30803 = CARTESIAN_POINT ( 'NONE',  ( 1.033464566929134687, -0.06523048226347956391, 0.8243110235145187925 ) ) ;
#30804 = ORIENTED_EDGE ( 'NONE', *, *, #15725, .F. ) ;
#30805 = DIRECTION ( 'NONE',  ( -1.000000000000000000, 0.000000000000000000, 0.000000000000000000 ) ) ;
#30806 = CARTESIAN_POINT ( 'NONE',  ( 0.7495606340400177148, 0.1264236179284866091, 1.026082677111590513 ) ) ;
#30807 = ORIENTED_EDGE ( 'NONE', *, *, #22550, .T. ) ;
#30808 = CARTESIAN_POINT ( 'NONE',  ( -0.7646288533564489232, 0.1113553986120547346, 0.5659448817822370081 ) ) ;
#30809 = CARTESIAN_POINT ( 'NONE',  ( 0.000000000000000000, -0.09842519685039370636, 0.000000000000000000 ) ) ;
#30810 = CARTESIAN_POINT ( 'NONE',  ( -1.033464566929134687, 0.06523048226347956391, 1.311515748031496509 ) ) ;
#30811 = DIRECTION ( 'NONE',  ( 0.000000000000000000, 0.6156614753256598460, 0.7880107536067206819 ) ) ;
#30813 = LINE ( 'NONE', #38444, #20113 ) ;
#30812 = CARTESIAN_POINT ( 'NONE',  ( 0.1832342603884100363, 0.1897030460626166204, -0.3104511204119947965 ) ) ;
#30814 = DIRECTION ( 'NONE',  ( -1.000000000000000000, -0.000000000000000000, -0.000000000000000000 ) ) ;
#30815 = CARTESIAN_POINT ( 'NONE',  ( 0.9873396505805591694, 0.1113553986120547346, 1.382874015640503940 ) ) ;
#30816 = ORIENTED_EDGE ( 'NONE', *, *, #1614, .F. ) ;
#30817 = EDGE_LOOP ( 'NONE', ( #14709, #38447, #46269, #24583 ) ) ;
#30818 = DIRECTION ( 'NONE',  ( 3.385139170096243171E-15, 1.000000000000000000, -0.000000000000000000 ) ) ;
#30819 = EDGE_LOOP ( 'NONE', ( #27983, #9232, #44268, #36933 ) ) ;
#30820 = CARTESIAN_POINT ( 'NONE',  ( -1.002407869896990045, -0.1264236179284866091, 1.592027559001354398 ) ) ;
#30821 = CARTESIAN_POINT ( 'NONE',  ( -0.1113553986120547346, 0.02657480325713335034, 0.1113553986120547346 ) ) ;
#30822 = CARTESIAN_POINT ( 'NONE',  ( -0.6971942568897648851, -0.07405724077823297447, 1.466535433017102763 ) ) ;
#30823 = ORIENTED_EDGE ( 'NONE', *, *, #8764, .T. ) ;
#30824 = AXIS2_PLACEMENT_3D ( 'NONE', #44342, #29573, #15386 ) ;
#30825 = ORIENTED_EDGE ( 'NONE', *, *, #41668, .T. ) ;
#30826 = EDGE_CURVE ( 'NONE', #4180, #31929, #7080, .T. ) ;
#30827 = AXIS2_PLACEMENT_3D ( 'NONE', #20091, #34737, #1876 ) ;
#30828 = CARTESIAN_POINT ( 'NONE',  ( 0.8070866141732283561, 0.000000000000000000, -0.7574803149606299524 ) ) ;
#30829 = CARTESIAN_POINT ( 'NONE',  ( -0.7185039370078739607, 1.928577636452523993E-17, 0.3838582677165354173 ) ) ;
#30830 = CARTESIAN_POINT ( 'NONE',  ( -0.07405724077823318263, -1.047368062717428217, -0.1787899950787401604 ) ) ;
#30831 = VERTEX_POINT ( 'NONE', #32272 ) ;
#30832 = CARTESIAN_POINT ( 'NONE',  ( -1.094772975963752103E-17, 0.1077755906049446960, -0.1787899950787401882 ) ) ;
#30833 = ORIENTED_EDGE ( 'NONE', *, *, #36586, .T. ) ;
#30834 = ORIENTED_EDGE ( 'NONE', *, *, #42538, .T. ) ;
#30835 = AXIS2_PLACEMENT_3D ( 'NONE', #29348, #41627, #43653 ) ;
#30836 = EDGE_CURVE ( 'NONE', #6613, #21958, #26847, .T. ) ;
#30837 = CARTESIAN_POINT ( 'NONE',  ( -0.2558995472165326857, -0.1045113733907631348, -0.3031500423883560225 ) ) ;
#30838 = DIRECTION ( 'NONE',  ( 0.000000000000000000, -0.6220299971367094782, 0.7829934116339072325 ) ) ;
#30839 = CARTESIAN_POINT ( 'NONE',  ( 0.8759842519685039353, 0.1574803149606299191, 1.751968503937007871 ) ) ;
#30840 = AXIS2_PLACEMENT_3D ( 'NONE', #30850, #11913, #27016 ) ;
#30841 = CARTESIAN_POINT ( 'NONE',  ( 3.284318927891251994E-17, -0.6648622046706456068, 0.1787899950787401882 ) ) ;
#30842 = CARTESIAN_POINT ( 'NONE',  ( -0.8019270111902716547, -0.1787899950787401604, 0.2116141731745827814 ) ) ;
#30843 = CARTESIAN_POINT ( 'NONE',  ( -0.9412147342319837628, -0.1574803149606297803, 1.026082677165353729 ) ) ;
#30844 = CARTESIAN_POINT ( 'NONE',  ( 0.1797182628040039087, -1.086165856827139509, 0.07444174185955046430 ) ) ;
#30845 = CARTESIAN_POINT ( 'NONE',  ( 0.1321676148590689159, 0.1299212598425196763, -0.1026092226670043267 ) ) ;
#30846 = CARTESIAN_POINT ( 'NONE',  ( 1.054774247047244540, 0.07405724077823318263, 1.053149606245450176 ) ) ;
#30847 = DIRECTION ( 'NONE',  ( 0.000000000000000000, -1.000000000000000000, 0.000000000000000000 ) ) ;
#30848 = CARTESIAN_POINT ( 'NONE',  ( 0.8759842519685039353, 0.1574803149606299191, 1.555118110236220597 ) ) ;
#30850 = CARTESIAN_POINT ( 'NONE',  ( 0.3649999999999999911, 3.414809992080327174E-17, 0.000000000000000000 ) ) ;
#30849 = CARTESIAN_POINT ( 'NONE',  ( 0.8622796235139646992, 0.1579280213382387443, 1.978604940233764209 ) ) ;
#30851 = CARTESIAN_POINT ( 'NONE',  ( 1.284448818897637956, 0.000000000000000000, 1.181102362204724310 ) ) ;
#30852 = CARTESIAN_POINT ( 'NONE',  ( -0.1574803149606300301, -0.7288385825696378495, -0.06523048226347956391 ) ) ;
#30853 = CARTESIAN_POINT ( 'NONE',  ( 0.07405724077823318263, 0.06594488194352732258, -0.1787899950787401604 ) ) ;
#30854 = AXIS2_PLACEMENT_3D ( 'NONE', #4580, #30975, #11813 ) ;
#30855 = CARTESIAN_POINT ( 'NONE',  ( -0.5555748031496045014, 0.6449983665207589256, -0.7480314960629921295 ) ) ;
#30856 = CARTESIAN_POINT ( 'NONE',  ( 1.002407869896990045, 0.1264236179284866091, 1.050688976324189117 ) ) ;
#30857 = CARTESIAN_POINT ( 'NONE',  ( 0.8759842519685039353, -0.1787899950787401882, 1.788877952702141672 ) ) ;
#30858 = CARTESIAN_POINT ( 'NONE',  ( 0.7185039370078739607, 1.928577636452523993E-17, 0.3346456691838114450 ) ) ;
#30859 = VERTEX_POINT ( 'NONE', #3491 ) ;
#30860 = DIRECTION ( 'NONE',  ( 0.000000000000000000, -1.000000000000000000, -1.224646799147353947E-16 ) ) ;
#30862 = CARTESIAN_POINT ( 'NONE',  ( 0.5538057742782149795, 0.08090551181102362266, 9.908067607274841931E-18 ) ) ;
#30861 = AXIS2_PLACEMENT_3D ( 'NONE', #34481, #38546, #1635 ) ;
#30863 = CARTESIAN_POINT ( 'NONE',  ( -9.642888182262618425E-18, -1.720472440837354400, -0.1574803149606299191 ) ) ;
#30864 = CARTESIAN_POINT ( 'NONE',  ( -0.8759842519685039353, 0.1574803149606299191, 0.2460629920184571051 ) ) ;
#30865 = DIRECTION ( 'NONE',  ( 1.000000000000000000, -3.469446951953613794E-15, -0.000000000000000000 ) ) ;
#30866 = CARTESIAN_POINT ( 'NONE',  ( 1.002407869896990045, 0.1264236179284866091, 1.247539370024976391 ) ) ;
#30867 = CARTESIAN_POINT ( 'NONE',  ( 0.07051875723996789413, -0.08549467455831237517, 0.2447177463900755412 ) ) ;
#30868 = CARTESIAN_POINT ( 'NONE',  ( -0.1264236179284866091, 0.1225393701325037388, 0.1264236179284866091 ) ) ;
#30869 = DIRECTION ( 'NONE',  ( 0.000000000000000000, 0.2432573283306646017, -0.9699617890481188054 ) ) ;
#30870 = CARTESIAN_POINT ( 'NONE',  ( -1.054774247047244540, -0.07405724077823318263, 0.6102362204186774219 ) ) ;
#30871 = CARTESIAN_POINT ( 'NONE',  ( -0.8759842519685039353, 0.000000000000000000, 0.000000000000000000 ) ) ;
#30872 = CARTESIAN_POINT ( 'NONE',  ( 1.033464566929133799, 0.000000000000000000, 1.811023621939716444 ) ) ;
#30873 = AXIS2_PLACEMENT_3D ( 'NONE', #10260, #6404, #21016 ) ;
#30875 = CARTESIAN_POINT ( 'NONE',  ( 0.07405724077823318263, -1.474409448765133801, -0.1787899950787401604 ) ) ;
#30874 = CARTESIAN_POINT ( 'NONE',  ( -0.1574803149606299191, -0.3720472439869610404, 0.000000000000000000 ) ) ;
#30876 = CARTESIAN_POINT ( 'NONE',  ( -0.8019270111902717657, 0.1787899950787401604, 1.806102362150961316 ) ) ;
#30877 = VERTEX_POINT ( 'NONE', #32750 ) ;
#30878 = CARTESIAN_POINT ( 'NONE',  ( -0.8759842519685039353, -0.1787899950787401882, 0.5290354330171024300 ) ) ;
#30879 = ORIENTED_EDGE ( 'NONE', *, *, #20770, .F. ) ;
#30880 = ADVANCED_FACE ( 'NONE', ( #14519 ), #29187, .T. ) ;
#30881 = DIRECTION ( 'NONE',  ( -0.5735764363510518216, 0.8191520442889876907, 1.003171929053519693E-16 ) ) ;
#30882 = DIRECTION ( 'NONE',  ( 0.000000000000000000, -0.7907053606985338101, 0.6121968903568536513 ) ) ;
#30883 = CARTESIAN_POINT ( 'NONE',  ( -0.07405724077823318263, -0.4814231808276640545, 0.1787899950787401604 ) ) ;
#30884 = CARTESIAN_POINT ( 'NONE',  ( 0.2001661423152484298, -0.08956032108766456834, 0.05039172328576543847 ) ) ;
#30885 = CARTESIAN_POINT ( 'NONE',  ( 0.7185039370078739607, 1.928577636452523993E-17, 0.4625984251968504046 ) ) ;
#30886 = CARTESIAN_POINT ( 'NONE',  ( 0.7185039370078739607, 0.000000000000000000, 2.007874015640504162 ) ) ;
#30887 = MECHANICAL_DESIGN_GEOMETRIC_PRESENTATION_REPRESENTATION (  '', ( #43806 ), #28585 ) ;
#30888 = EDGE_CURVE ( 'NONE', #36211, #4000, #45931, .T. ) ;
#30889 = CARTESIAN_POINT ( 'NONE',  ( -0.8019270111902717657, -0.1787899950787401604, 0.5216535432533228045 ) ) ;
#30890 = CARTESIAN_POINT ( 'NONE',  ( -0.1787899950787401882, -1.827387747756799241, 0.000000000000000000 ) ) ;
#30891 = ORIENTED_EDGE ( 'NONE', *, *, #18701, .F. ) ;
#30892 = CARTESIAN_POINT ( 'NONE',  ( 0.2471922732848571835, -0.07885118474260616184, 0.07559718168574836028 ) ) ;
#30893 = CARTESIAN_POINT ( 'NONE',  ( -1.054774247047244540, -0.07405724077823318263, 1.520669291284818758 ) ) ;
#30894 = AXIS2_PLACEMENT_3D ( 'NONE', #11477, #36643, #14840 ) ;
#30895 = AXIS2_PLACEMENT_3D ( 'NONE', #1361, #8558, #23192 ) ;
#30896 = CARTESIAN_POINT ( 'NONE',  ( -0.1787899950787401882, -1.422736220418677311, 0.000000000000000000 ) ) ;
#30897 = CARTESIAN_POINT ( 'NONE',  ( 0.7185039370078739607, 1.928577636452523993E-17, 0.3740157479239689664 ) ) ;
#30898 = CARTESIAN_POINT ( 'NONE',  ( 0.9873396505805591694, 0.1113553986120547346, 1.028543306979086802 ) ) ;
#30899 = LINE ( 'NONE', #41374, #31574 ) ;
#30900 = CARTESIAN_POINT ( 'NONE',  ( -0.1270800023317771588, -0.7539808174570609145, -0.1270800023317771588 ) ) ;
#30901 = CARTESIAN_POINT ( 'NONE',  ( -0.8759842519685039353, 0.1574803149606299191, 1.309055118002708573 ) ) ;
#30902 = CARTESIAN_POINT ( 'NONE',  ( 0.8019270111902717657, 0.1787899950787401604, 0.5905511810485987167 ) ) ;
#30903 = CARTESIAN_POINT ( 'NONE',  ( -0.7185039370078714072, 0.06523048226347728795, 1.631397637687748814 ) ) ;
#30904 = FACE_BOUND ( 'NONE', #46606, .T. ) ;
#30905 = ORIENTED_EDGE ( 'NONE', *, *, #4470, .F. ) ;
#30906 = CARTESIAN_POINT ( 'NONE',  ( 0.8107537697050253289, 0.1574803149606300301, 1.045767716535432879 ) ) ;
#30907 = PLANE ( 'NONE',  #41499 ) ;
#30908 = CARTESIAN_POINT ( 'NONE',  ( 0.3551574803149606385, 2.613864355459500179E-17, 0.000000000000000000 ) ) ;
#30909 = EDGE_CURVE ( 'NONE', #12474, #14401, #15354, .T. ) ;
#30910 = ( BOUNDED_CURVE ( )  B_SPLINE_CURVE ( 2, ( #5112, #45363, #30798, #1999, #12576, #32913, #44352, #33619, #26184 ),
 .UNSPECIFIED., .F., .T. ) 
 B_SPLINE_CURVE_WITH_KNOTS ( ( 3, 2, 2, 2, 3 ),
 ( 0.08000000000000000167, 0.08250000000000000389, 0.08500000000000000611, 0.08749999999999999445, 0.08999999999999999667 ),
 .UNSPECIFIED. ) 
 CURVE ( )  GEOMETRIC_REPRESENTATION_ITEM ( )  RATIONAL_B_SPLINE_CURVE ( ( 1.000000000000000000, 0.9238795325112869605, 1.000000000000000000, 0.9238795325112869605, 1.000000000000000000, 0.9238795325112869605, 1.000000000000000000, 0.9238795325112869605, 1.000000000000000000 ) ) 
 REPRESENTATION_ITEM ( '' )  ) ;
#30912 = CARTESIAN_POINT ( 'NONE',  ( -7.957671378281915615E-17, 0.1564960629921311464, -0.2933070866141737065 ) ) ;
#30911 = CARTESIAN_POINT ( 'NONE',  ( -0.8759842519685039353, 0.000000000000000000, 0.000000000000000000 ) ) ;
#30913 = CARTESIAN_POINT ( 'NONE',  ( 0.9412147342319837628, 0.1574803149606300301, 0.5979330707586145710 ) ) ;
#30914 = CARTESIAN_POINT ( 'NONE',  ( 0.1787899950787401882, -0.5319881889226142357, -2.189545951927503898E-17 ) ) ;
#30915 = ORIENTED_EDGE ( 'NONE', *, *, #45532, .F. ) ;
#30916 = CARTESIAN_POINT ( 'NONE',  ( 1.033464566929134687, 0.06523048226347956391, 1.154035433070866423 ) ) ;
#30917 = ORIENTED_EDGE ( 'NONE', *, *, #30836, .T. ) ;
#30918 = DIRECTION ( 'NONE',  ( 1.000000000000000000, 0.000000000000000000, -1.822029033848725275E-16 ) ) ;
#30919 = CARTESIAN_POINT ( 'NONE',  ( 1.033464566929133799, 0.000000000000000000, 0.9153543307086614567 ) ) ;
#30920 = CARTESIAN_POINT ( 'NONE',  ( -0.07405724077823318263, -1.779527559001355952, -0.1787899950787401604 ) ) ;
#30921 = CARTESIAN_POINT ( 'NONE',  ( 0.1787899950787401604, -0.8887795275052913224, -0.07405724077823318263 ) ) ;
#30922 = CARTESIAN_POINT ( 'NONE',  ( -0.1574803149606299191, -1.405511811023622215, 0.000000000000000000 ) ) ;
#30923 = CARTESIAN_POINT ( 'NONE',  ( 0.1526809758745832635, 0.1055212057016139821, -0.09282246162998031291 ) ) ;
#30924 = ORIENTED_EDGE ( 'NONE', *, *, #8384, .T. ) ;
#30925 = ORIENTED_EDGE ( 'NONE', *, *, #46234, .F. ) ;
#30926 = CARTESIAN_POINT ( 'NONE',  ( -0.7495606340400177148, -0.1264236179284866091, 1.862696850339937038 ) ) ;
#30927 = CARTESIAN_POINT ( 'NONE',  ( 0.6971942568897648851, 0.07405724077823318263, 1.855314960576157635 ) ) ;
#30928 = VERTEX_POINT ( 'NONE', #28444 ) ;
#30930 = DIRECTION ( 'NONE',  ( -1.000000000000000000, -5.411399086424350389E-15, 4.197754538034584604E-15 ) ) ;
#30929 = AXIS2_PLACEMENT_3D ( 'NONE', #38821, #2383, #24443 ) ;
#30931 = CARTESIAN_POINT ( 'NONE',  ( 0.6971942568897637749, 2.189545951927499583E-17, 0.4798228345919055560 ) ) ;
#30932 = CARTESIAN_POINT ( 'NONE',  ( -0.8759842519685039353, -0.1787899950787401882, 1.350885826717889815 ) ) ;
#30933 = FACE_OUTER_BOUND ( 'NONE', #14928, .T. ) ;
#30934 = CARTESIAN_POINT ( 'NONE',  ( -1.054774247047244540, -0.07405724077823318263, 0.9251968503399374821 ) ) ;
#30935 = CARTESIAN_POINT ( 'NONE',  ( -0.7495606340400177148, -0.1264236179284866091, 0.1304133857730082613 ) ) ;
#30936 = ( BOUNDED_CURVE ( )  B_SPLINE_CURVE ( 2, ( #15120, #22522, #23004, #4288, #30235, #29766, #26857, #45020, #18919 ),
 .UNSPECIFIED., .F., .F. ) 
 B_SPLINE_CURVE_WITH_KNOTS ( ( 3, 2, 2, 2, 3 ),
 ( 0.7399999999999999911, 0.7425000000000000488, 0.7449999999999999956, 0.7475000000000000533, 0.7500000000000000000 ),
 .UNSPECIFIED. ) 
 CURVE ( )  GEOMETRIC_REPRESENTATION_ITEM ( )  RATIONAL_B_SPLINE_CURVE ( ( 1.000000000000000000, 0.9238795325112869605, 1.000000000000000000, 0.9238795325112869605, 1.000000000000000000, 0.9238795325112869605, 1.000000000000000000, 0.9238795325112829637, 1.000000000000000000 ) ) 
 REPRESENTATION_ITEM ( '' )  ) ;
#30937 = EDGE_CURVE ( 'NONE', #5631, #2951, #43007, .T. ) ;
#30938 = DIRECTION ( 'NONE',  ( 0.000000000000000000, -1.000000000000000000, 0.000000000000000000 ) ) ;
#30939 = CARTESIAN_POINT ( 'NONE',  ( -1.054774247047244540, 0.07405724077823318263, 1.761811023568284007 ) ) ;
#30940 = CARTESIAN_POINT ( 'NONE',  ( -0.9873396505805591694, 0.1113553986120547346, 1.973425196742866206 ) ) ;
#30941 = CARTESIAN_POINT ( 'NONE',  ( -0.8759842519685039353, 0.1574803149606299191, 1.673228346456693050 ) ) ;
#30942 = DIRECTION ( 'NONE',  ( -1.000000000000000000, -0.000000000000000000, -0.000000000000000000 ) ) ;
#30943 = CARTESIAN_POINT ( 'NONE',  ( 0.6971942568897648851, -0.07405724077823297447, 1.545275590497419138 ) ) ;
#30944 = CARTESIAN_POINT ( 'NONE',  ( -0.02314857569221047059, -0.09842519685039370636, 0.2241248956163086614 ) ) ;
#30945 = CARTESIAN_POINT ( 'NONE',  ( -0.3161444924769509779, 1.209494567139720367, -1.479906699140297599 ) ) ;
#30946 = CARTESIAN_POINT ( 'NONE',  ( -0.9412147342319837628, 0.1574803149606300301, 1.788877952755905554 ) ) ;
#30947 = EDGE_CURVE ( 'NONE', #15464, #10600, #46250, .T. ) ;
#30948 = EDGE_LOOP ( 'NONE', ( #28027, #22111, #2778, #35840 ) ) ;
#30949 = ( REPRESENTATION_RELATIONSHIP ('NONE','NONE', #9609, #5950 ) REPRESENTATION_RELATIONSHIP_WITH_TRANSFORMATION ( #42677 )SHAPE_REPRESENTATION_RELATIONSHIP( ) ) ;
#30950 = CARTESIAN_POINT ( 'NONE',  ( -0.1787899950787401882, -1.029035433017102319, 0.000000000000000000 ) ) ;
#30951 = CARTESIAN_POINT ( 'NONE',  ( 0.07405724077823318263, -1.169291338528914537, 0.1787899950787401604 ) ) ;
#30952 = DIRECTION ( 'NONE',  ( -0.000000000000000000, 1.000000000000000000, -3.995705278811693553E-31 ) ) ;
#30953 = CARTESIAN_POINT ( 'NONE',  ( 3.301370929368692659E-17, -0.3061461717877700939, 0.1797182628040039365 ) ) ;
#30954 = CARTESIAN_POINT ( 'NONE',  ( -0.1113553986120547346, -0.03248031496062991907, -0.1113553986120547346 ) ) ;
#30955 = VECTOR ( 'NONE', #8341, 39.37007874015748143 ) ;
#30956 = CARTESIAN_POINT ( 'NONE',  ( 0.9500414927467378812, -0.1787899950787401604, 0.8809055117572599514 ) ) ;
#30957 = CARTESIAN_POINT ( 'NONE',  ( 0.08080321177261283461, 0.2488424761941021024, -0.03960523631943477924 ) ) ;
#30958 = ( GEOMETRIC_REPRESENTATION_CONTEXT ( 3 ) GLOBAL_UNCERTAINTY_ASSIGNED_CONTEXT ( ( #26376 ) ) GLOBAL_UNIT_ASSIGNED_CONTEXT ( ( #21793, #37100, #44510 ) ) REPRESENTATION_CONTEXT ( 'NONE', 'WORKASPACE' ) ) ;
#30959 = CARTESIAN_POINT ( 'NONE',  ( 0.9873396505805591694, 0.1113553986120547346, 0.04429133847515007855 ) ) ;
#30960 = ORIENTED_EDGE ( 'NONE', *, *, #7200, .F. ) ;
#30961 = DIRECTION ( 'NONE',  ( 0.000000000000000000, -1.000000000000000000, 0.000000000000000000 ) ) ;
#30962 = CARTESIAN_POINT ( 'NONE',  ( 0.1264236179284866091, -0.4926181101824567143, -0.1264236179284866091 ) ) ;
#30963 = FACE_OUTER_BOUND ( 'NONE', #1546, .T. ) ;
#30964 = CARTESIAN_POINT ( 'NONE',  ( 0.1264236179284866091, -1.324311023568283341, 0.1264236179284866091 ) ) ;
#30965 = CARTESIAN_POINT ( 'NONE',  ( -0.8070866141732283561, 0.000000000000000000, -0.8559055118110230342 ) ) ;
#30966 = CARTESIAN_POINT ( 'NONE',  ( -0.7495606340400177148, -0.1264236179284866091, 1.897145669237574772 ) ) ;
#30967 = ORIENTED_EDGE ( 'NONE', *, *, #17917, .T. ) ;
#30968 = CARTESIAN_POINT ( 'NONE',  ( -0.9500414927467378812, 0.1787899950787401604, 1.254921259788757348 ) ) ;
#30969 = PLANE ( 'NONE',  #46754 ) ;
#30970 = ADVANCED_FACE ( 'NONE', ( #8186 ), #45068, .T. ) ;
#30971 = CARTESIAN_POINT ( 'NONE',  ( 1.054774247047244540, -0.07405724077823318263, 1.363188976324188895 ) ) ;
#30972 = CARTESIAN_POINT ( 'NONE',  ( -0.9500414927467378812, 0.1787899950787401604, 0.5068897637257642197 ) ) ;
#30973 = CARTESIAN_POINT ( 'NONE',  ( -1.054774247047244540, 0.07405724077823318263, 1.284448818843874740 ) ) ;
#30974 = DIRECTION ( 'NONE',  ( -1.000000000000000000, -0.000000000000000000, -0.000000000000000000 ) ) ;
#30975 = DIRECTION ( 'NONE',  ( 0.000000000000000000, 0.000000000000000000, 1.000000000000000000 ) ) ;
#30976 = CARTESIAN_POINT ( 'NONE',  ( 0.6971942568897648851, 0.07405724077823318263, 0.6348425196312760255 ) ) ;
#30977 = CARTESIAN_POINT ( 'NONE',  ( -1.002407869896990045, -0.1264236179284866091, 0.5290354330171024300 ) ) ;
#30978 = CARTESIAN_POINT ( 'NONE',  ( -0.08774906724784053980, -0.09246610911299792124, 0.2347711071351809009 ) ) ;
#30979 = CARTESIAN_POINT ( 'NONE',  ( 1.033464566929133799, 0.000000000000000000, 0.03937007863263043694 ) ) ;
#30980 = VERTEX_POINT ( 'NONE', #3724 ) ;
#30981 = AXIS2_PLACEMENT_3D ( 'NONE', #21417, #32713, #9942 ) ;
#30982 = CARTESIAN_POINT ( 'NONE',  ( -1.033464566929134687, 0.06523048226347956391, 0.3666338582677165503 ) ) ;
#30983 = CARTESIAN_POINT ( 'NONE',  ( 0.6971942568897648851, 0.07405724077823318263, 1.146653543253323582 ) ) ;
#30984 = CARTESIAN_POINT ( 'NONE',  ( -0.2415982954816964789, -0.09851385206391319316, -0.02995337850299783361 ) ) ;
#30985 = CARTESIAN_POINT ( 'NONE',  ( 0.7646288533564489232, 0.1113553986120547346, 1.313976377845228249 ) ) ;
#30986 = VECTOR ( 'NONE', #21427, 39.37007874015748854 ) ;
#30987 = EDGE_LOOP ( 'NONE', ( #21471, #10004, #1060, #5751 ) ) ;
#30988 = ADVANCED_FACE ( 'NONE', ( #4578 ), #34102, .T. ) ;
#30989 = CARTESIAN_POINT ( 'NONE',  ( -0.7646288533564489232, -0.1113553986120547346, 1.294291338582677309 ) ) ;
#30990 = CARTESIAN_POINT ( 'NONE',  ( -0.6971942568897648851, -0.07405724077823297447, 0.9940944881352130613 ) ) ;
#30991 = CARTESIAN_POINT ( 'NONE',  ( -1.054774247047244540, 0.07405724077823318263, 0.1820866141194649179 ) ) ;
#30992 = CARTESIAN_POINT ( 'NONE',  ( 0.1787899950787401604, -1.652683023347347957, 0.07405724077823318263 ) ) ;
#30993 = ORIENTED_EDGE ( 'NONE', *, *, #34866, .F. ) ;
#30994 = DIRECTION ( 'NONE',  ( 0.000000000000000000, -0.7880107536067211260, 0.6156614753256591799 ) ) ;
#30995 = CARTESIAN_POINT ( 'NONE',  ( -0.07405724077823318263, -0.5196850393163150450, -0.1787899950787401604 ) ) ;
#30996 = CARTESIAN_POINT ( 'NONE',  ( -0.2664910633248679939, -0.1585270522231945201, 0.9306302837667671524 ) ) ;
#30997 = ORIENTED_EDGE ( 'NONE', *, *, #20407, .F. ) ;
#30998 = CARTESIAN_POINT ( 'NONE',  ( 0.6971942568897637749, 2.189545951927499583E-17, 1.301673228292692830 ) ) ;
#30999 = CARTESIAN_POINT ( 'NONE',  ( -0.06453057165845259291, 0.2582375021999043785, -0.3090319486758607015 ) ) ;
#31000 = DIRECTION ( 'NONE',  ( -0.6018150231520440485, 0.000000000000000000, -0.7986355100472960489 ) ) ;
#31001 = CARTESIAN_POINT ( 'NONE',  ( 0.1787899950787401604, -1.799212598371432659, 0.07405724077823318263 ) ) ;
#31002 = SHAPE_DEFINITION_REPRESENTATION ( #21852, #43589 ) ;
#31003 = DIRECTION ( 'NONE',  ( -3.478357113474434231E-15, -1.000000000000000000, 0.000000000000000000 ) ) ;
#31004 = CARTESIAN_POINT ( 'NONE',  ( 0.8019270111902717657, -0.1787899950787401604, 0.4429133857730075952 ) ) ;
#31005 = CARTESIAN_POINT ( 'NONE',  ( -0.7495606340400177148, 0.1264236179284866091, 0.7898622046706456068 ) ) ;
#31007 = CARTESIAN_POINT ( 'NONE',  ( 0.8759842519685039353, 0.000000000000000000, 4.498031496062992574 ) ) ;
#31006 = CARTESIAN_POINT ( 'NONE',  ( -9.642888182262618425E-18, -0.7460629921259843700, -0.1574803149606299191 ) ) ;
#31009 = CARTESIAN_POINT ( 'NONE',  ( -0.7541062341187345641, -0.1190279680630223907, 1.985685656426464440 ) ) ;
#31008 = CARTESIAN_POINT ( 'NONE',  ( 0.07444174185955065859, -1.524157982811393586, 0.1797182628040039087 ) ) ;
#31010 = CARTESIAN_POINT ( 'NONE',  ( -0.1113553986120547346, -0.06200787390822106587, -0.1113553986120547346 ) ) ;
#31011 = CARTESIAN_POINT ( 'NONE',  ( 2.892866454678787531E-17, -0.4803149605223936969, 0.1574803149606299191 ) ) ;
#31012 = CIRCLE ( 'NONE', #3423, 0.09842519685039370636 ) ;
#31013 = CARTESIAN_POINT ( 'NONE',  ( 0.1264236179284866091, -0.4187992125446614589, 0.1264236179284866091 ) ) ;
#31014 = CARTESIAN_POINT ( 'NONE',  ( 0.2471922904502827090, 0.07573437638785612824, -0.08155181604444516896 ) ) ;
#31015 = CARTESIAN_POINT ( 'NONE',  ( 0.9500414927467378812, 0.1787899950787401604, 1.491141732229701367 ) ) ;
#31016 = CARTESIAN_POINT ( 'NONE',  ( 0.9500414927467377701, -0.1787899950787401604, 1.786417322780882388 ) ) ;
#31017 = CARTESIAN_POINT ( 'NONE',  ( 0.6971942568897648851, 0.07405724077823318263, 0.4330708660879683536 ) ) ;
#31018 = AXIS2_PLACEMENT_3D ( 'NONE', #7102, #17887, #10236 ) ;
#31019 = AXIS2_PLACEMENT_3D ( 'NONE', #9634, #46503, #28093 ) ;
#31022 = ORIENTED_EDGE ( 'NONE', *, *, #31890, .F. ) ;
#31021 = ADVANCED_FACE ( 'NONE', ( #30286 ), #32988, .T. ) ;
#31020 = CARTESIAN_POINT ( 'NONE',  ( 0.2519685039370078705, -0.08090551181102362266, 1.098083891755157578E-17 ) ) ;
#31023 = LINE ( 'NONE', #12810, #38857 ) ;
#31024 = CARTESIAN_POINT ( 'NONE',  ( 1.350095158311321523E-16, -0.0009842519685041700977, 0.2952755905511816326 ) ) ;
#31025 = CARTESIAN_POINT ( 'NONE',  ( -0.1787899950787401604, 0.1102362205262043815, -0.07405724077823318263 ) ) ;
#31026 = CARTESIAN_POINT ( 'NONE',  ( 1.002407869896990045, -0.1264236179284866091, 0.4896653542769449086 ) ) ;
#31027 = EDGE_CURVE ( 'NONE', #1651, #18878, #37520, .T. ) ;
#31029 = DIRECTION ( 'NONE',  ( 0.000000000000000000, 0.000000000000000000, 1.000000000000000000 ) ) ;
#31028 = CARTESIAN_POINT ( 'NONE',  ( 0.8019270111902716547, -0.1787899950787401604, 1.309055118056473122 ) ) ;
#31030 = CARTESIAN_POINT ( 'NONE',  ( 1.033464566929134687, 0.06523048226347956391, 0.2091535433070865757 ) ) ;
#31031 = CARTESIAN_POINT ( 'NONE',  ( 0.8759842519685039353, 0.1574803149606299191, 0.8366141731208189825 ) ) ;
#31032 = VERTEX_POINT ( 'NONE', #37424 ) ;
#31033 = EDGE_CURVE ( 'NONE', #44561, #28497, #21944, .T. ) ;
#31034 = CARTESIAN_POINT ( 'NONE',  ( 0.8759842519685039353, 0.1787899950787401882, 0.9424212597887559051 ) ) ;
#31035 = ORIENTED_EDGE ( 'NONE', *, *, #5081, .T. ) ;
#31036 = CARTESIAN_POINT ( 'NONE',  ( 3.284318927891251994E-17, -1.334153543253322916, 0.1787899950787401882 ) ) ;
#31037 = CARTESIAN_POINT ( 'NONE',  ( -0.7185039370078739607, 1.928577636452523993E-17, 0.5708661416247566844 ) ) ;
#31038 = CARTESIAN_POINT ( 'NONE',  ( 1.033464566929133799, 0.000000000000000000, 0.08858267716535432601 ) ) ;
#31039 = CARTESIAN_POINT ( 'NONE',  ( -0.8759842519685039353, 0.1574803149606299191, 1.318897637795275690 ) ) ;
#31040 = CARTESIAN_POINT ( 'NONE',  ( -0.7185039370078746268, -0.06523048226347956391, 1.045767716427905114 ) ) ;
#31042 = CARTESIAN_POINT ( 'NONE',  ( -0.7185039370078739607, 1.928577636452523993E-17, 0.4232283464566928832 ) ) ;
#31041 = LINE ( 'NONE', #45382, #45607 ) ;
#31043 = CARTESIAN_POINT ( 'NONE',  ( 0.6971942568897626646, 0.07405724077823318263, 0.1230314960092287191 ) ) ;
#31044 = CARTESIAN_POINT ( 'NONE',  ( 0.7185039370078739607, 1.928577636452523993E-17, 1.397637795168062969 ) ) ;
#31045 = ORIENTED_EDGE ( 'NONE', *, *, #14961, .T. ) ;
#31046 = ORIENTED_EDGE ( 'NONE', *, *, #42442, .F. ) ;
#31047 = ( BOUNDED_CURVE ( )  B_SPLINE_CURVE ( 2, ( #3351, #32616, #43112, #25161, #10318, #10561, #13660, #31898, #25416 ),
 .UNSPECIFIED., .F., .T. ) 
 B_SPLINE_CURVE_WITH_KNOTS ( ( 3, 2, 2, 2, 3 ),
 ( 0.7600000000000000089, 0.7624999999999999556, 0.7650000000000000133, 0.7674999999999999600, 0.7700000000000000178 ),
 .UNSPECIFIED. ) 
 CURVE ( )  GEOMETRIC_REPRESENTATION_ITEM ( )  RATIONAL_B_SPLINE_CURVE ( ( 1.000000000000000000, 0.9238795325112869605, 1.000000000000000000, 0.9238795325112869605, 1.000000000000000000, 0.9238795325112869605, 1.000000000000000000, 0.9238795325112869605, 1.000000000000000000 ) ) 
 REPRESENTATION_ITEM ( '' )  ) ;
#31048 = CARTESIAN_POINT ( 'NONE',  ( -0.1264236179284866091, 0.07824803154982658271, 0.1264236179284866091 ) ) ;
#31049 = ORIENTED_EDGE ( 'NONE', *, *, #12485, .T. ) ;
#31050 = CARTESIAN_POINT ( 'NONE',  ( 1.054774247047244096, 0.000000000000000000, 0.6963582676627716461 ) ) ;
#31051 = CARTESIAN_POINT ( 'NONE',  ( 1.054774247047244540, -0.07405724077823318263, 0.9694881889226145688 ) ) ;
#31052 = CARTESIAN_POINT ( 'NONE',  ( -0.9500414927467377701, -0.1787899950787401604, 1.550196850339938148 ) ) ;
#31053 = CARTESIAN_POINT ( 'NONE',  ( 0.1113553986120547346, -0.1505905510735753849, -0.1113553986120547346 ) ) ;
#31054 = ORIENTED_EDGE ( 'NONE', *, *, #26287, .T. ) ;
#31055 = CIRCLE ( 'NONE', #43252, 0.4404574800679669777 ) ;
#31056 = CARTESIAN_POINT ( 'NONE',  ( -0.8107537697050254399, 0.1574803149606300301, 0.2485236219397169988 ) ) ;
#31057 = CARTESIAN_POINT ( 'NONE',  ( 0.7646288533564489232, 0.1113553986120547346, 1.865157480207432883 ) ) ;
#31058 = AXIS2_PLACEMENT_3D ( 'NONE', #46873, #20991, #35640 ) ;
#31059 = CARTESIAN_POINT ( 'NONE',  ( -0.9412147342319837628, -0.1574803149606297803, 1.882381889656251639 ) ) ;
#31060 = CARTESIAN_POINT ( 'NONE',  ( 0.1264236179284866091, -1.094120031221364142, -0.1264236179284866091 ) ) ;
#31061 = ORIENTED_EDGE ( 'NONE', *, *, #10849, .T. ) ;
#31062 = CARTESIAN_POINT ( 'NONE',  ( -0.1787899950787401882, -0.03986220467064590517, 0.000000000000000000 ) ) ;
#31063 = ORIENTED_EDGE ( 'NONE', *, *, #23714, .F. ) ;
#31064 = AXIS2_PLACEMENT_3D ( 'NONE', #13944, #10363, #3392 ) ;
#31065 = ORIENTED_EDGE ( 'NONE', *, *, #35715, .T. ) ;
#31066 = CARTESIAN_POINT ( 'NONE',  ( -0.8759842519685039353, -0.1574803149606299191, 1.407480314853102321 ) ) ;
#31067 = CARTESIAN_POINT ( 'NONE',  ( -0.7185039370078746268, 0.06523048226347956391, 0.9227362203649142058 ) ) ;
#31068 = CARTESIAN_POINT ( 'NONE',  ( 0.9412147342319837628, -0.1574803149606297803, 1.892224409448819644 ) ) ;
#31069 = CARTESIAN_POINT ( 'NONE',  ( -0.07405724077823318263, -0.5639763778989922427, -0.1787899950787401604 ) ) ;
#31070 = ADVANCED_FACE ( 'NONE', ( #1459 ), #41317, .F. ) ;
#31071 = CARTESIAN_POINT ( 'NONE',  ( -0.9500414927467377701, 0.1787899950787401604, 0.3887795275052913224 ) ) ;
#31072 = CARTESIAN_POINT ( 'NONE',  ( -0.7646288533564489232, -0.1113553986120547346, 0.9793307086614173596 ) ) ;
#31073 = CARTESIAN_POINT ( 'NONE',  ( 0.07444174185955065859, -1.209197352890132970, 0.1797182628040039087 ) ) ;
#31074 = CARTESIAN_POINT ( 'NONE',  ( 1.054774247047244540, -0.07405724077823318263, 1.008858267662772423 ) ) ;
#31075 = CARTESIAN_POINT ( 'NONE',  ( 0.9500414927467377701, 0.1787899950787401604, 0.1870078739619845110 ) ) ;
#31076 = CIRCLE ( 'NONE', #13442, 0.4404574800679669777 ) ;
#31078 = ADVANCED_FACE ( 'NONE', ( #12531 ), #34496, .T. ) ;
#31077 = CARTESIAN_POINT ( 'NONE',  ( -0.9873396505805591694, 0.1113553986120547346, 0.6348425195775118102 ) ) ;
#31079 = CARTESIAN_POINT ( 'NONE',  ( 1.033464566929134687, -0.06523048226347956391, 1.621555118110237004 ) ) ;
#31081 = DIRECTION ( 'NONE',  ( 0.000000000000000000, 0.000000000000000000, 1.000000000000000000 ) ) ;
#31080 = CARTESIAN_POINT ( 'NONE',  ( 0.7579794631033002217, 0.1108770549927829419, 1.980899420926319321 ) ) ;
#31082 = DIRECTION ( 'NONE',  ( 1.000000000000000000, 0.000000000000000000, -1.822029033848725275E-16 ) ) ;
#31083 = CARTESIAN_POINT ( 'NONE',  ( -0.1787899950787401604, 0.1200787402112438867, 0.07405724077823318263 ) ) ;
#31084 = EDGE_CURVE ( 'NONE', #5177, #6537, #41903, .T. ) ;
#31085 = DIRECTION ( 'NONE',  ( 1.000000000000000000, -0.000000000000000000, -0.000000000000000000 ) ) ;
#31086 = CARTESIAN_POINT ( 'NONE',  ( 1.002407869896990045, -0.1264236179284866091, 1.040846456639149764 ) ) ;
#31087 = CARTESIAN_POINT ( 'NONE',  ( 0.6971942568897637749, 2.189545951927499583E-17, 1.897145669237574772 ) ) ;
#31088 = CARTESIAN_POINT ( 'NONE',  ( 0.8759842519685039353, 0.1574803149606299191, 0.3248031494987720369 ) ) ;
#31089 = ORIENTED_EDGE ( 'NONE', *, *, #31842, .F. ) ;
#31090 = DIRECTION ( 'NONE',  ( 0.000000000000000000, 0.7880107536067213481, -0.6156614753256589578 ) ) ;
#31091 = ADVANCED_FACE ( 'NONE', ( #37672 ), #19447, .T. ) ;
#31092 = VECTOR ( 'NONE', #37704, 39.37007874015748143 ) ;
#31093 = CIRCLE ( 'NONE', #32525, 0.4404574800679669777 ) ;
#31094 = CARTESIAN_POINT ( 'NONE',  ( 0.06523048226347956391, -1.619586614065700036, 0.1574803149606297803 ) ) ;
#31095 = CARTESIAN_POINT ( 'NONE',  ( -0.7185039370078746268, -0.06523048226347956391, 0.1796259841444415029 ) ) ;
#31096 = CARTESIAN_POINT ( 'NONE',  ( 0.8019270111902717657, -0.1787899950787401604, 1.309055118056472899 ) ) ;
#31097 = EDGE_CURVE ( 'NONE', #16796, #38700, #26104, .T. ) ;
#31098 = CARTESIAN_POINT ( 'NONE',  ( 0.08995663987707425147, -0.09317336072452189755, 0.2334965874938940145 ) ) ;
#31099 = CARTESIAN_POINT ( 'NONE',  ( 0.1264236179284866091, 0.1323818898175431191, 0.1264236179284866091 ) ) ;
#31100 = LINE ( 'NONE', #34221, #42052 ) ;
#31101 = CARTESIAN_POINT ( 'NONE',  ( -0.8759842519685039353, 0.1787899950787401882, 0.5831692912848189803 ) ) ;
#31102 = CARTESIAN_POINT ( 'NONE',  ( 1.033464566929134687, -0.06523048226347956391, 1.375492125876724980 ) ) ;
#31103 = DIRECTION ( 'NONE',  ( 0.000000000000000000, 0.000000000000000000, -1.000000000000000000 ) ) ;
#31104 = CARTESIAN_POINT ( 'NONE',  ( -0.1264236179284866091, -1.496555118056472677, 0.1264236179284866091 ) ) ;
#31105 = CARTESIAN_POINT ( 'NONE',  ( -0.8019270111902717657, 0.1787899950787401604, 0.9448818897100165204 ) ) ;
#31106 = CARTESIAN_POINT ( 'NONE',  ( -1.054774247047244096, 0.000000000000000000, 1.911909448765133801 ) ) ;
#31107 = EDGE_LOOP ( 'NONE', ( #459, #41310, #6735, #21637, #28560, #5556, #30577, #28720, #2652, #14565, #39188 ) ) ;
#31108 = CARTESIAN_POINT ( 'NONE',  ( -0.8759842519685039353, -0.1787899950787401882, 0.6077755904974173617 ) ) ;
#31109 = VERTEX_POINT ( 'NONE', #40912 ) ;
#31110 = DIRECTION ( 'NONE',  ( 0.000000000000000000, 1.000000000000000000, 0.000000000000000000 ) ) ;
#31111 = CARTESIAN_POINT ( 'NONE',  ( 0.1264236179284866091, -0.7397893225599468936, -0.1264236179284866091 ) ) ;
#31112 = VERTEX_POINT ( 'NONE', #43162 ) ;
#31113 = CARTESIAN_POINT ( 'NONE',  ( 0.1731537741114069218, -0.08956052929350570568, -0.09650519479221614239 ) ) ;
#31114 = PLANE ( 'NONE',  #35621 ) ;
#31115 = VERTEX_POINT ( 'NONE', #14846 ) ;
#31116 = FACE_OUTER_BOUND ( 'NONE', #9867, .T. ) ;
#31117 = AXIS2_PLACEMENT_3D ( 'NONE', #5046, #19426, #44338 ) ;
#31118 = LINE ( 'NONE', #5201, #32598 ) ;
#31119 = CARTESIAN_POINT ( 'NONE',  ( -0.6971942568897626646, 0.07405724077823318263, 0.4330708660879683536 ) ) ;
#31120 = CARTESIAN_POINT ( 'NONE',  ( -0.7646288533564489232, -0.1113553986120547346, 0.3887795275590551491 ) ) ;
#31121 = ORIENTED_EDGE ( 'NONE', *, *, #18710, .T. ) ;
#31122 = CARTESIAN_POINT ( 'NONE',  ( -0.6971942568897648851, 0.07405724077823318263, 1.619094488135213838 ) ) ;
#31123 = CARTESIAN_POINT ( 'NONE',  ( -1.094772975963752103E-17, -1.511318897584031484, -0.1787899950787401882 ) ) ;
#31124 = CARTESIAN_POINT ( 'NONE',  ( -0.7185039370078739607, 1.928577636452523993E-17, 1.761811023622047223 ) ) ;
#31125 = DIRECTION ( 'NONE',  ( 0.000000000000000000, 0.000000000000000000, 1.000000000000000000 ) ) ;
#31126 = CYLINDRICAL_SURFACE ( 'NONE', #40722, 0.1574803149606299191 ) ;
#31127 = CARTESIAN_POINT ( 'NONE',  ( -0.1797182628040039365, -0.7096894788743838278, 0.000000000000000000 ) ) ;
#31128 = FACE_OUTER_BOUND ( 'NONE', #44199, .T. ) ;
#31129 = CARTESIAN_POINT ( 'NONE',  ( -0.9873396505805591694, 0.1113553986120547346, 1.304133858160188897 ) ) ;
#31131 = CARTESIAN_POINT ( 'NONE',  ( 0.9412147342319837628, -0.1574803149606297803, 1.764271653435779852 ) ) ;
#31130 = CARTESIAN_POINT ( 'NONE',  ( -0.1113553986120547346, -0.4163385826771653364, 0.1113553986120547346 ) ) ;
#31132 = DIRECTION ( 'NONE',  ( 1.000000000000000000, 0.000000000000000000, 0.000000000000000000 ) ) ;
#31133 = ORIENTED_EDGE ( 'NONE', *, *, #47118, .F. ) ;
#31134 = DIRECTION ( 'NONE',  ( 0.000000000000000000, 0.000000000000000000, 1.000000000000000000 ) ) ;
#31135 = CARTESIAN_POINT ( 'NONE',  ( -0.9500414927467377701, 0.1787899950787401604, 1.097440944828127041 ) ) ;
#31136 = CARTESIAN_POINT ( 'NONE',  ( 0.9412147342319837628, 0.1574803149606300301, 1.119586614173229577 ) ) ;
#31138 = LINE ( 'NONE', #725, #10952 ) ;
#31137 = DIRECTION ( 'NONE',  ( 0.000000000000000000, 0.000000000000000000, -1.000000000000000000 ) ) ;
#31139 = CARTESIAN_POINT ( 'NONE',  ( -0.7185039370078739607, 1.928577636452523993E-17, 0.7283464565853858819 ) ) ;
#31140 = CARTESIAN_POINT ( 'NONE',  ( -0.06523048226347956391, -0.5762795274515275512, -0.1574803149606300301 ) ) ;
#31141 = EDGE_CURVE ( 'NONE', #25222, #18796, #8110, .T. ) ;
#31142 = LINE ( 'NONE', #35435, #22412 ) ;
#31143 = DIRECTION ( 'NONE',  ( -3.469446951953613794E-15, -1.000000000000000000, 0.000000000000000000 ) ) ;
#31144 = CARTESIAN_POINT ( 'NONE',  ( -0.07405724077823318263, -0.5984251967966303098, -0.1787899950787401604 ) ) ;
#31145 = DIRECTION ( 'NONE',  ( 0.000000000000000000, -1.000000000000000000, 0.000000000000000000 ) ) ;
#31146 = CARTESIAN_POINT ( 'NONE',  ( 0.6971942568897626646, 0.07405724077823318263, 0.9055118109698585549 ) ) ;
#31147 = EDGE_CURVE ( 'NONE', #35620, #27211, #13066, .T. ) ;
#31148 = ORIENTED_EDGE ( 'NONE', *, *, #46241, .F. ) ;
#31149 = LINE ( 'NONE', #2579, #37168 ) ;
#31150 = DIRECTION ( 'NONE',  ( 0.000000000000000000, -1.000000000000000000, 0.000000000000000000 ) ) ;
#31151 = CARTESIAN_POINT ( 'NONE',  ( 0.07405724077823318263, -1.784448818843874962, -0.1787899950787401604 ) ) ;
#31152 = CARTESIAN_POINT ( 'NONE',  ( 0.07405724077823318263, -0.8986220471903317852, 0.1787899950787401604 ) ) ;
#31153 = CARTESIAN_POINT ( 'NONE',  ( 0.06523048226347956391, -1.314468503937008093, 0.1574803149606297803 ) ) ;
#31154 = CARTESIAN_POINT ( 'NONE',  ( 0.7646288533564489232, -0.1113553986120547346, 1.245078740049952559 ) ) ;
#31155 = DIRECTION ( 'NONE',  ( 0.000000000000000000, 0.000000000000000000, 1.000000000000000000 ) ) ;
#31156 = ORIENTED_EDGE ( 'NONE', *, *, #37940, .F. ) ;
#31157 = ORIENTED_EDGE ( 'NONE', *, *, #41134, .F. ) ;
#31158 = CARTESIAN_POINT ( 'NONE',  ( -0.7495606340400177148, -0.1264236179284866091, 1.941437007820252081 ) ) ;
#31159 = CARTESIAN_POINT ( 'NONE',  ( 0.8019270111902717657, 0.1787899950787401604, 1.811023621993480548 ) ) ;
#31160 = ORIENTED_EDGE ( 'NONE', *, *, #19593, .F. ) ;
#31161 = CARTESIAN_POINT ( 'NONE',  ( 0.1574803149606299191, -1.375984251860976393, -1.928577636452523993E-17 ) ) ;
#31162 = DIRECTION ( 'NONE',  ( 5.411399086424348811E-15, -1.000000000000000000, 0.000000000000000000 ) ) ;
#31163 = CARTESIAN_POINT ( 'NONE',  ( 0.9500414927467378812, 0.1787899950787401604, 0.5068897637257642197 ) ) ;
#31164 = CARTESIAN_POINT ( 'NONE',  ( -0.9500414927467378812, 0.1787899950787401604, 1.407480314906865981 ) ) ;
#31165 = CARTESIAN_POINT ( 'NONE',  ( 0.07407796729086078835, 0.2527247573021684235, -0.3106979152242848596 ) ) ;
#31166 = CARTESIAN_POINT ( 'NONE',  ( -0.7495606340400177148, -0.1264236179284866091, 0.2878937007336381804 ) ) ;
#31167 = CARTESIAN_POINT ( 'NONE',  ( -0.1184675242425147629, -0.09842519685039369248, 1.555605046820496273 ) ) ;
#31168 = CARTESIAN_POINT ( 'NONE',  ( -1.002407869896990045, -0.1264236179284866091, 1.754429133804503715 ) ) ;
#31169 = CARTESIAN_POINT ( 'NONE',  ( -1.033464566929133799, 0.000000000000000000, 1.968503936900346529 ) ) ;
#31170 = CARTESIAN_POINT ( 'NONE',  ( 0.04509681258129913384, -0.07057211410339600532, -0.2593943580756443157 ) ) ;
#31171 = CARTESIAN_POINT ( 'NONE',  ( -0.7185039370078746268, -0.06523048226347956391, 1.803641732283465693 ) ) ;
#31172 = DIRECTION ( 'NONE',  ( 0.5735764363510447161, 0.8191520442889925757, 0.000000000000000000 ) ) ;
#31173 = CARTESIAN_POINT ( 'NONE',  ( 0.9500414927467377701, 0.1787899950787401604, 1.687992125930489307 ) ) ;
#31174 = CARTESIAN_POINT ( 'NONE',  ( 0.1642845807979765871, -0.09842519685039370636, -0.1153058249971240234 ) ) ;
#31175 = CARTESIAN_POINT ( 'NONE',  ( -1.033464566929134687, -0.06523048226347956391, 1.503444881889764995 ) ) ;
#31176 = CONICAL_SURFACE ( 'NONE', #26583, 0.1574803149606299191, 0.9599310885968713736 ) ;
#31177 = ORIENTED_EDGE ( 'NONE', *, *, #41313, .F. ) ;
#31178 = ORIENTED_EDGE ( 'NONE', *, *, #6931, .T. ) ;
#31179 = CARTESIAN_POINT ( 'NONE',  ( 0.1787899950787401882, -1.088090551127338657, -2.189545951927503898E-17 ) ) ;
#31180 = CARTESIAN_POINT ( 'NONE',  ( 0.1264236179284866091, -1.275098425143086578, -0.1264236179284866091 ) ) ;
#31181 = CARTESIAN_POINT ( 'NONE',  ( 0.1574803149606299746, -0.2274162997038020051, -0.9219983537151217323 ) ) ;
#31182 = CARTESIAN_POINT ( 'NONE',  ( 0.1797182628040039087, -0.4562445969846198879, 0.07444174185955046430 ) ) ;
#31183 = CARTESIAN_POINT ( 'NONE',  ( -0.3161444924769509779, 1.205832402325951680, -1.129708666049261900 ) ) ;
#31184 = CARTESIAN_POINT ( 'NONE',  ( -0.7185039370078746268, 0.06523048226347956391, 0.8046259841444418637 ) ) ;
#31185 = CARTESIAN_POINT ( 'NONE',  ( 0.06523048226347956391, -0.0004921259842519828086, -0.1574803149606300301 ) ) ;
#31186 = CARTESIAN_POINT ( 'NONE',  ( -0.1264236179284866091, -0.1579724408911182820, 0.1264236179284866091 ) ) ;
#31187 = CARTESIAN_POINT ( 'NONE',  ( 0.4330708661417291827, 1.006139616066729676E-16, 1.186023622047243986 ) ) ;
#31189 = EDGE_CURVE ( 'NONE', #16139, #9851, #8618, .T. ) ;
#31188 = CARTESIAN_POINT ( 'NONE',  ( 0.7495606340400177148, 0.1264236179284866091, 0.9030511810485984947 ) ) ;
#31190 = EDGE_CURVE ( 'NONE', #38091, #28106, #18655, .T. ) ;
#31192 = CARTESIAN_POINT ( 'NONE',  ( -0.1377952755905511861, 0.1574803149606320007, -0.7057086614173230243 ) ) ;
#31191 = CARTESIAN_POINT ( 'NONE',  ( -0.7185039370078739607, 1.928577636452523993E-17, 1.131889763779527547 ) ) ;
#31193 = CARTESIAN_POINT ( 'NONE',  ( 0.9500414927467378812, -0.1787899950787401604, 1.948818897584033927 ) ) ;
#31194 = FACE_OUTER_BOUND ( 'NONE', #42896, .T. ) ;
#31195 = CARTESIAN_POINT ( 'NONE',  ( 0.1264236179284866091, -0.5024606298674960669, 0.1264236179284866091 ) ) ;
#31196 = CARTESIAN_POINT ( 'NONE',  ( 0.5236220472440944462, -0.08090551181102362266, 0.000000000000000000 ) ) ;
#31198 = AXIS2_PLACEMENT_3D ( 'NONE', #15718, #30353, #30575 ) ;
#31197 = CARTESIAN_POINT ( 'NONE',  ( -0.07405724077823318263, -1.410433070812377565, 0.1787899950787401604 ) ) ;
#31199 = ( BOUNDED_CURVE ( )  B_SPLINE_CURVE ( 2, ( #17178, #25573, #29203, #31813, #35639, #39666, #2779, #46872, #46400 ),
 .UNSPECIFIED., .F., .T. ) 
 B_SPLINE_CURVE_WITH_KNOTS ( ( 3, 2, 2, 2, 3 ),
 ( 0.02000000000000000042, 0.02249999999999999917, 0.02500000000000000139, 0.02750000000000000014, 0.02999999999999999889 ),
 .UNSPECIFIED. ) 
 CURVE ( )  GEOMETRIC_REPRESENTATION_ITEM ( )  RATIONAL_B_SPLINE_CURVE ( ( 1.000000000000000000, 0.9238795325112869605, 1.000000000000000000, 0.9238795325112869605, 1.000000000000000000, 0.9238795325112869605, 1.000000000000000000, 0.9238795325112869605, 1.000000000000000000 ) ) 
 REPRESENTATION_ITEM ( '' )  ) ;
#31200 = CARTESIAN_POINT ( 'NONE',  ( 1.002407869896990045, -0.1264236179284866091, 0.3764763778989925203 ) ) ;
#31201 = CARTESIAN_POINT ( 'NONE',  ( -0.9500414927467378812, -0.1787899950787401604, 1.943897637741510254 ) ) ;
#31202 = ORIENTED_EDGE ( 'NONE', *, *, #45696, .F. ) ;
#31203 = CARTESIAN_POINT ( 'NONE',  ( -0.8759842519685039353, -0.1787899950787401882, 1.434547244040724534 ) ) ;
#31204 = CARTESIAN_POINT ( 'NONE',  ( -0.7646288533564489232, 0.1113553986120547346, 1.323818897637795367 ) ) ;
#31205 = CARTESIAN_POINT ( 'NONE',  ( 0.6971942568897637749, 2.189545951927499583E-17, 1.385334645615527549 ) ) ;
#31206 = FACE_OUTER_BOUND ( 'NONE', #44471, .T. ) ;
#31207 = CARTESIAN_POINT ( 'NONE',  ( 2.892866454678787531E-17, -1.228346456585385882, 0.1574803149606299191 ) ) ;
#31208 = CARTESIAN_POINT ( 'NONE',  ( 0.8759842519685039353, 0.1787899950787401882, 0.1156496062454492185 ) ) ;
#31209 = CARTESIAN_POINT ( 'NONE',  ( -0.7495606340400177148, 0.1264236179284866091, 1.139271653489543290 ) ) ;
#31210 = CARTESIAN_POINT ( 'NONE',  ( 0.09469176317940933285, -0.09842519655130997636, -0.1516944367183098441 ) ) ;
#31211 = CARTESIAN_POINT ( 'NONE',  ( 0.6971942568897648851, -0.07405724077823297447, 0.6003937007336389575 ) ) ;
#31212 = CARTESIAN_POINT ( 'NONE',  ( -0.6971942568897648851, 0.07405724077823318263, 0.5118110235682844511 ) ) ;
#31213 = CARTESIAN_POINT ( 'NONE',  ( 0.1574803149606299191, -0.08661417322834646937, -1.928577636452523993E-17 ) ) ;
#31214 = ORIENTED_EDGE ( 'NONE', *, *, #14520, .T. ) ;
#31215 = CARTESIAN_POINT ( 'NONE',  ( -0.9412147342319837628, -0.1574803149606297803, 0.3174212598425196763 ) ) ;
#31216 = CARTESIAN_POINT ( 'NONE',  ( 0.6971942568897648851, 0.07405724077823318263, 1.343503936954111966 ) ) ;
#31217 = CARTESIAN_POINT ( 'NONE',  ( 0.1467038341990881956, -0.09851384883411416771, 0.1600693656517706842 ) ) ;
#31218 = ORIENTED_EDGE ( 'NONE', *, *, #41599, .F. ) ;
#31219 = CARTESIAN_POINT ( 'NONE',  ( -0.9412147342319837628, -0.1574803149606297803, 0.6323818897637792924 ) ) ;
#31220 = CARTESIAN_POINT ( 'NONE',  ( -0.6971942568897637749, 2.189545951927499583E-17, 0.9916338582139527791 ) ) ;
#31221 = AXIS2_PLACEMENT_3D ( 'NONE', #4625, #7525, #18784 ) ;
#31222 = CARTESIAN_POINT ( 'NONE',  ( -0.07405724077823318263, -1.544415306811916633, 0.1787899950787401604 ) ) ;
#31223 = VERTEX_POINT ( 'NONE', #31941 ) ;
#31224 = CARTESIAN_POINT ( 'NONE',  ( -0.8107537697050254399, 0.1574803149606300301, 0.1697834644594022058 ) ) ;
#31225 = CARTESIAN_POINT ( 'NONE',  ( -0.1787899950787401604, -0.5541338582139530011, -0.07405724077823318263 ) ) ;
#31226 = CARTESIAN_POINT ( 'NONE',  ( -0.3010365421720465617, -0.07487990393731483452, 1.026013379696918859 ) ) ;
#31227 = CARTESIAN_POINT ( 'NONE',  ( 0.8019270111902717657, 0.1787899950787401604, 1.333661417269071059 ) ) ;
#31228 = LINE ( 'NONE', #45337, #368 ) ;
#31229 = CARTESIAN_POINT ( 'NONE',  ( 0.1787899950787401882, -0.2219488188438744347, -2.189545951927503898E-17 ) ) ;
#31230 = CARTESIAN_POINT ( 'NONE',  ( -0.1787899950787401604, -0.8297244093950564281, -0.07405724077823318263 ) ) ;
#31231 = DIRECTION ( 'NONE',  ( -0.000000000000000000, 1.000000000000000000, -0.000000000000000000 ) ) ;
#31232 = CARTESIAN_POINT ( 'NONE',  ( 1.033464566929134687, 0.06523048226347956391, 1.813484251860976171 ) ) ;
#31233 = CARTESIAN_POINT ( 'NONE',  ( 0.8759842519685039353, -0.1787899950787401882, 1.626476377898992132 ) ) ;
#31234 = ADVANCED_FACE ( 'NONE', ( #7634 ), #21367, .F. ) ;
#31235 = CARTESIAN_POINT ( 'NONE',  ( 0.07405724077823318263, -0.004060976103254483952, 0.1787899950787401604 ) ) ;
#31236 = CARTESIAN_POINT ( 'NONE',  ( 0.1264236179284866091, -1.757381889710015965, 0.1264236179284866091 ) ) ;
#31237 = PRODUCT_CONTEXT ( 'NONE', #8584, 'mechanical' ) ;
#31238 = CARTESIAN_POINT ( 'NONE',  ( -0.4955489724641236604, 0.000000000000000000, 0.3997690233743834698 ) ) ;
#31239 = CARTESIAN_POINT ( 'NONE',  ( 0.8019270111902717657, 0.1787899950787401604, 0.4675196849856070869 ) ) ;
#31240 = CARTESIAN_POINT ( 'NONE',  ( -0.8759842519685039353, -0.1787899950787401882, 0.8046259841982047467 ) ) ;
#31241 = EDGE_CURVE ( 'NONE', #5433, #461, #25438, .T. ) ;
#31243 = DIRECTION ( 'NONE',  ( -1.000000000000000000, 0.000000000000000000, 0.000000000000000000 ) ) ;
#31242 = CARTESIAN_POINT ( 'NONE',  ( 0.1113553986120547346, -0.9576771653543306728, 0.1113553986120547346 ) ) ;
#31245 = CARTESIAN_POINT ( 'NONE',  ( -0.7640572627416960527, -0.1288658717550650867, 1.985929485999813338 ) ) ;
#31244 = CARTESIAN_POINT ( 'NONE',  ( -0.1797182628040039365, -1.615201289898005710, 0.000000000000000000 ) ) ;
#31246 = CARTESIAN_POINT ( 'NONE',  ( -0.06523048226347956391, -0.4434055117034965132, 0.1574803149606297803 ) ) ;
#31247 = CARTESIAN_POINT ( 'NONE',  ( 1.054774247047244540, 0.07405724077823318263, 1.564960629867495845 ) ) ;
#31248 = CARTESIAN_POINT ( 'NONE',  ( 0.8019270111902716547, 0.1787899950787401604, 1.766732283410803239 ) ) ;
#31249 = CARTESIAN_POINT ( 'NONE',  ( 0.7495606340400177148, -0.1264236179284866091, 0.4010826771115905687 ) ) ;
#31250 = ORIENTED_EDGE ( 'NONE', *, *, #40796, .F. ) ;
#31251 = CARTESIAN_POINT ( 'NONE',  ( 0.7185039370078739607, 1.928577636452523993E-17, 0.1377952754830242266 ) ) ;
#31252 = ADVANCED_FACE ( 'NONE', ( #35763 ), #26076, .T. ) ;
#31253 = CARTESIAN_POINT ( 'NONE',  ( 0.7185039370078739607, 1.928577636452523993E-17, 0.8464566928058583350 ) ) ;
#31255 = CARTESIAN_POINT ( 'NONE',  ( -0.1787899950787401604, 0.07578740162856664742, 0.07405724077823318263 ) ) ;
#31254 = CARTESIAN_POINT ( 'NONE',  ( 0.06523048226347956391, -0.8567913384751505435, -0.1574803149606300301 ) ) ;
#31256 = CARTESIAN_POINT ( 'NONE',  ( 1.054774247047244096, 0.000000000000000000, 0.3764763778989925203 ) ) ;
#31257 = CARTESIAN_POINT ( 'NONE',  ( 0.8281979645144629254, -0.1535074065110398345, 0.03937341667646054172 ) ) ;
#31258 = CARTESIAN_POINT ( 'NONE',  ( 0.9873396505805591694, -0.1113553986120547346, 1.963582677057826853 ) ) ;
#31259 = EDGE_CURVE ( 'NONE', #23819, #13130, #38579, .T. ) ;
#31260 = LINE ( 'NONE', #10079, #33994 ) ;
#31261 = CARTESIAN_POINT ( 'NONE',  ( -1.054774247047244096, 0.000000000000000000, 1.518208661363559031 ) ) ;
#31262 = CARTESIAN_POINT ( 'NONE',  ( 0.9873396505805591694, -0.1113553986120547346, 0.8218503935932598425 ) ) ;
#31263 = ORIENTED_EDGE ( 'NONE', *, *, #36987, .T. ) ;
#31264 = CARTESIAN_POINT ( 'NONE',  ( -0.7185039370078739607, 1.928577636452523993E-17, 0.8070866140657008136 ) ) ;
#31265 = CARTESIAN_POINT ( 'NONE',  ( 0.9500414927467378812, -0.1787899950787401604, 1.003937007820251193 ) ) ;
#31266 = ORIENTED_EDGE ( 'NONE', *, *, #9215, .T. ) ;
#31267 = CARTESIAN_POINT ( 'NONE',  ( -0.1264236179284866091, -1.299704724355684959, 0.1264236179284866091 ) ) ;
#31268 = CARTESIAN_POINT ( 'NONE',  ( -0.9873396505805591694, -0.1113553986120547346, 0.5068897636720007815 ) ) ;
#31269 = CARTESIAN_POINT ( 'NONE',  ( -0.9412147342319837628, 0.1574803149606300301, 0.8046259842519695171 ) ) ;
#31270 = CARTESIAN_POINT ( 'NONE',  ( 0.8759842519685039353, -0.1787899950787401882, 1.665846456639149764 ) ) ;
#31271 = CARTESIAN_POINT ( 'NONE',  ( -1.033464566929133799, 0.000000000000000000, 1.387795275590551158 ) ) ;
#31272 = CARTESIAN_POINT ( 'NONE',  ( 0.2066929133858268486, 0.7443365962042343131, -3.523993443072799270 ) ) ;
#31274 = DIRECTION ( 'NONE',  ( -1.000000000000000000, 0.000000000000000000, 0.000000000000000000 ) ) ;
#31273 = FACE_OUTER_BOUND ( 'NONE', #42823, .T. ) ;
#31275 = CARTESIAN_POINT ( 'NONE',  ( 0.8759842519685039353, 0.1787899950787401882, 0.07627952750529173875 ) ) ;
#31276 = CARTESIAN_POINT ( 'NONE',  ( 0.8107537697050253289, 0.1574803149606300301, 1.468996062884598830 ) ) ;
#31277 = EDGE_LOOP ( 'NONE', ( #46675, #45714, #14633, #31160, #36500 ) ) ;
#31278 = VERTEX_POINT ( 'NONE', #11482 ) ;
#31279 = CARTESIAN_POINT ( 'NONE',  ( 0.1822895153388602307, 0.000000000000000000, 0.000000000000000000 ) ) ;
#31280 = CARTESIAN_POINT ( 'NONE',  ( 0.8107537697050254399, -0.1574803149606297803, 0.5880905511811019837 ) ) ;
#31281 = CARTESIAN_POINT ( 'NONE',  ( -0.9500414927467377701, 0.1787899950787401604, 1.683070866087970074 ) ) ;
#31282 = CARTESIAN_POINT ( 'NONE',  ( -9.642888182262618425E-18, -0.2244094487113704739, -0.1574803149606299191 ) ) ;
#31283 = ORIENTED_EDGE ( 'NONE', *, *, #6978, .T. ) ;
#31284 = CARTESIAN_POINT ( 'NONE',  ( 0.3161444924769420961, -1.730062351173306868E-15, 1.351672847932125986E-15 ) ) ;
#31285 = DIRECTION ( 'NONE',  ( 0.000000000000000000, 0.000000000000000000, 1.000000000000000000 ) ) ;
#31286 = CARTESIAN_POINT ( 'NONE',  ( 0.1574803149606299746, 0.5419727308409655331, -0.7545416139885203766 ) ) ;
#31287 = CARTESIAN_POINT ( 'NONE',  ( 0.1264236179284866091, -1.182702708386718538, 0.1264236179284866091 ) ) ;
#31288 = ORIENTED_EDGE ( 'NONE', *, *, #31492, .F. ) ;
#31289 = CARTESIAN_POINT ( 'NONE',  ( -0.1787899950787401882, -0.07923228341080354453, 0.000000000000000000 ) ) ;
#31290 = ORIENTED_EDGE ( 'NONE', *, *, #14666, .T. ) ;
#31291 = VERTEX_POINT ( 'NONE', #15315 ) ;
#31292 = ADVANCED_FACE ( 'NONE', ( #29969 ), #44516, .F. ) ;
#31293 = DIRECTION ( 'NONE',  ( 0.000000000000000000, -1.000000000000000000, 0.000000000000000000 ) ) ;
#31294 = CARTESIAN_POINT ( 'NONE',  ( -0.8759842519685039353, -0.1574803149606299191, 0.4232283463491653963 ) ) ;
#31295 = CARTESIAN_POINT ( 'NONE',  ( 0.9412147342319837628, 0.1574803149606300301, 1.749507874015747699 ) ) ;
#31296 = EDGE_CURVE ( 'NONE', #42583, #24091, #26694, .T. ) ;
#31297 = CARTESIAN_POINT ( 'NONE',  ( 0.1787899950787401604, -0.6525590550643474153, -0.07405724077823318263 ) ) ;
#31298 = VECTOR ( 'NONE', #9759, 39.37007874015748143 ) ;
#31299 = CARTESIAN_POINT ( 'NONE',  ( -0.7495606340400177148, -0.1264236179284866091, 0.3666338582139531677 ) ) ;
#31300 = CARTESIAN_POINT ( 'NONE',  ( -0.7646288533564489232, 0.1113553986120547346, 1.048228346456692828 ) ) ;
#31302 = CARTESIAN_POINT ( 'NONE',  ( -0.7124115563218176295, 0.02371305101100566748, 1.982827744692199801 ) ) ;
#31301 = CARTESIAN_POINT ( 'NONE',  ( 0.07444174185955046430, -1.194433573362573497, -0.1797182628040039087 ) ) ;
#31303 = CARTESIAN_POINT ( 'NONE',  ( 0.000000000000000000, 0.000000000000000000, -0.3149606299212598381 ) ) ;
#31304 = CARTESIAN_POINT ( 'NONE',  ( 1.054774247047244540, 0.07405724077823318263, 1.013779527505291878 ) ) ;
#31305 = CARTESIAN_POINT ( 'NONE',  ( 0.9500414927467377701, -0.1787899950787401604, 1.392716535379308285 ) ) ;
#31306 = CARTESIAN_POINT ( 'NONE',  ( 0.7495606340400177148, -0.1264236179284866091, 0.2436023621509610382 ) ) ;
#31307 = CARTESIAN_POINT ( 'NONE',  ( 0.06801279071811515420, -0.5708661417322834497, 1.224299699984019663 ) ) ;
#31308 = CARTESIAN_POINT ( 'NONE',  ( 0.9412147342319837628, -0.1574803149606297803, 1.577263779527559917 ) ) ;
#31310 = CARTESIAN_POINT ( 'NONE',  ( -0.8639857840511040443, 0.1575694914283039538, 1.978574434837644835 ) ) ;
#31309 = CARTESIAN_POINT ( 'NONE',  ( 1.033464566929133799, 0.000000000000000000, 1.427165354330708569 ) ) ;
#31311 = CARTESIAN_POINT ( 'NONE',  ( 0.2944196465027555387, 1.205361022782824954E-17, -0.09842519685039370636 ) ) ;
#31312 = CARTESIAN_POINT ( 'NONE',  ( 0.06523048226347956391, -0.7534448817822362310, 0.1574803149606297803 ) ) ;
#31313 = CARTESIAN_POINT ( 'NONE',  ( 0.06841996760812382727, 0.1299212598425196763, 0.1651804176431311000 ) ) ;
#31314 = ( BOUNDED_CURVE ( )  B_SPLINE_CURVE ( 2, ( #2550, #15078, #13696, #42664, #11243, #6497, #22238, #4022, #9880 ),
 .UNSPECIFIED., .F., .T. ) 
 B_SPLINE_CURVE_WITH_KNOTS ( ( 3, 2, 2, 2, 3 ),
 ( 0.4000000000000000222, 0.4025000000000000244, 0.4050000000000000266, 0.4074999999999999734, 0.4099999999999999756 ),
 .UNSPECIFIED. ) 
 CURVE ( )  GEOMETRIC_REPRESENTATION_ITEM ( )  RATIONAL_B_SPLINE_CURVE ( ( 1.000000000000000000, 0.9238795325112869605, 1.000000000000000000, 0.9238795325112869605, 1.000000000000000000, 0.9238795325112869605, 1.000000000000000000, 0.9238795325112849621, 1.000000000000000000 ) ) 
 REPRESENTATION_ITEM ( '' )  ) ;
#31315 = DIRECTION ( 'NONE',  ( 1.000000000000000000, 0.000000000000000000, 2.048823632034775047E-14 ) ) ;
#31316 = CARTESIAN_POINT ( 'NONE',  ( 0.9500414927467377701, -0.1787899950787401604, 0.9990157479777320715 ) ) ;
#31317 = CARTESIAN_POINT ( 'NONE',  ( 1.033464566929134687, -0.06523048226347956391, 0.3912401573727880555 ) ) ;
#31318 = EDGE_LOOP ( 'NONE', ( #7184, #44614, #9829, #26752 ) ) ;
#31319 = DIRECTION ( 'NONE',  ( 0.000000000000000000, 0.000000000000000000, 1.000000000000000000 ) ) ;
#31320 = CARTESIAN_POINT ( 'NONE',  ( 0.9976899381744536166, 0.1122945889148146276, 0.03936994490810627467 ) ) ;
#31321 = CARTESIAN_POINT ( 'NONE',  ( 2.892866454678787531E-17, -1.700787401467275473, 0.1574803149606299191 ) ) ;
#31322 = CARTESIAN_POINT ( 'NONE',  ( -0.8759842519685039353, -0.1574803149606299191, 0.3051181101286932762 ) ) ;
#31323 = DIRECTION ( 'NONE',  ( 1.000000000000000000, 0.000000000000000000, 0.000000000000000000 ) ) ;
#31324 = CARTESIAN_POINT ( 'NONE',  ( 0.8019270111902717657, 0.1787899950787401604, 1.333661417269071059 ) ) ;
#31325 = DIRECTION ( 'NONE',  ( 0.000000000000000000, -0.000000000000000000, -1.000000000000000000 ) ) ;
#31326 = CARTESIAN_POINT ( 'NONE',  ( 0.1264236179284866091, 0.06348425202226751218, -0.1264236179284866091 ) ) ;
#31327 = FACE_OUTER_BOUND ( 'NONE', #46471, .T. ) ;
#31328 = CARTESIAN_POINT ( 'NONE',  ( -0.8759842519685039353, 0.1787899950787401882, 0.6619094487651338010 ) ) ;
#31329 = CARTESIAN_POINT ( 'NONE',  ( 0.9412147342319837628, -0.1574803149606297803, 1.370570866034205748 ) ) ;
#31330 = CARTESIAN_POINT ( 'NONE',  ( -0.07034821948466075947, 0.08559642391438677944, 0.2448175074096620163 ) ) ;
#31331 = CARTESIAN_POINT ( 'NONE',  ( -1.094772975963752103E-17, -1.708169291284818980, -0.1787899950787401882 ) ) ;
#31332 = CARTESIAN_POINT ( 'NONE',  ( -1.054774247047244096, 0.000000000000000000, 1.990649606245448844 ) ) ;
#31333 = ORIENTED_EDGE ( 'NONE', *, *, #24908, .F. ) ;
#31334 = AXIS2_PLACEMENT_3D ( 'NONE', #31286, #12840, #27471 ) ;
#31335 = ORIENTED_EDGE ( 'NONE', *, *, #38696, .F. ) ;
#31336 = CARTESIAN_POINT ( 'NONE',  ( 0.5555748031496086092, 0.2597269656108935343, 0.5511811023622046335 ) ) ;
#31337 = CARTESIAN_POINT ( 'NONE',  ( 0.002317772416624286781, 0.03366109551137453498, -0.1377956189922244779 ) ) ;
#31338 = CARTESIAN_POINT ( 'NONE',  ( -1.094772975963752103E-17, -0.6954979839772696959, -0.1787899950787401882 ) ) ;
#31339 = ORIENTED_EDGE ( 'NONE', *, *, #17744, .T. ) ;
#31340 = CARTESIAN_POINT ( 'NONE',  ( 0.1797904941528189193, -0.08956025049567893637, 0.1078749962962417402 ) ) ;
#31341 = AXIS2_PLACEMENT_3D ( 'NONE', #45778, #17039, #24699 ) ;
#31342 = CARTESIAN_POINT ( 'NONE',  ( -0.9873396505805591694, -0.1113553986120547346, 0.6643700786326299790 ) ) ;
#31343 = ORIENTED_EDGE ( 'NONE', *, *, #45389, .T. ) ;
#31344 = CYLINDRICAL_SURFACE ( 'NONE', #4952, 0.3912448816427701037 ) ;
#31345 = ADVANCED_FACE ( 'NONE', ( #10377 ), #2914, .T. ) ;
#31346 = CYLINDRICAL_SURFACE ( 'NONE', #38617, 0.1377952755905511306 ) ;
#31347 = CARTESIAN_POINT ( 'NONE',  ( -0.8019270111902717657, 0.1787899950787401604, 0.5068897637257642197 ) ) ;
#31348 = CARTESIAN_POINT ( 'NONE',  ( 0.000000000000000000, 0.000000000000000000, -0.06545654452343109553 ) ) ;
#31349 = EDGE_CURVE ( 'NONE', #26985, #39269, #2369, .T. ) ;
#31350 = VERTEX_POINT ( 'NONE', #24984 ) ;
#31351 = ADVANCED_FACE ( 'NONE', ( #39579 ), #35256, .F. ) ;
#31352 = CARTESIAN_POINT ( 'NONE',  ( -1.002407869896990045, -0.1264236179284866091, 1.715059055064346527 ) ) ;
#31353 = EDGE_CURVE ( 'NONE', #18699, #873, #46067, .T. ) ;
#31354 = ORIENTED_EDGE ( 'NONE', *, *, #44041, .T. ) ;
#31355 = CARTESIAN_POINT ( 'NONE',  ( 0.7185039370078739607, 0.000000000000000000, 4.498031496062992574 ) ) ;
#31356 = AXIS2_PLACEMENT_3D ( 'NONE', #1691, #16340, #17266 ) ;
#31357 = CARTESIAN_POINT ( 'NONE',  ( -0.7185039370078739607, 1.928577636452523993E-17, 0.1377952754830242266 ) ) ;
#31358 = DIRECTION ( 'NONE',  ( 0.000000000000000000, 0.000000000000000000, -1.000000000000000000 ) ) ;
#31359 = ORIENTED_EDGE ( 'NONE', *, *, #46612, .F. ) ;
#31360 = CARTESIAN_POINT ( 'NONE',  ( 0.7185039370078746268, -0.06523048226347956391, 0.5831692913385827515 ) ) ;
#31361 = CARTESIAN_POINT ( 'NONE',  ( -0.07444174185955065859, -0.6629375103704481242, 0.1797182628040039087 ) ) ;
#31362 = CARTESIAN_POINT ( 'NONE',  ( 0.2471922904502827090, 0.09773636000336977103, 0.01649811039745145355 ) ) ;
#31363 = CARTESIAN_POINT ( 'NONE',  ( -0.7646288533564489232, -0.1113553986120547346, 1.205708661309795371 ) ) ;
#31364 = CARTESIAN_POINT ( 'NONE',  ( 0.9500414927467378812, 0.1787899950787401604, 0.6643700786863929730 ) ) ;
#31366 = CARTESIAN_POINT ( 'NONE',  ( -0.03598878106637547203, -0.09842522444525984848, 0.1542999736886214723 ) ) ;
#31365 = CARTESIAN_POINT ( 'NONE',  ( -0.1574803149606297803, -0.4187992125984250080, 0.06523048226347956391 ) ) ;
#31367 = DIRECTION ( 'NONE',  ( 1.822029033848725028E-16, 0.000000000000000000, 1.000000000000000000 ) ) ;
#31368 = ORIENTED_EDGE ( 'NONE', *, *, #25015, .F. ) ;
#31369 = DIRECTION ( 'NONE',  ( 1.000000000000000000, 0.000000000000000000, 0.000000000000000000 ) ) ;
#31370 = CARTESIAN_POINT ( 'NONE',  ( -1.002407869896990045, 0.1264236179284866091, 1.055610236166708793 ) ) ;
#31371 = CARTESIAN_POINT ( 'NONE',  ( 0.8107537697050253289, 0.1574803149606300301, 1.085137795275590955 ) ) ;
#31372 = CARTESIAN_POINT ( 'NONE',  ( 0.1113553986120547346, 0.08562992136736949367, -0.1113553986120547346 ) ) ;
#31374 = FACE_OUTER_BOUND ( 'NONE', #34679, .T. ) ;
#31373 = CYLINDRICAL_SURFACE ( 'NONE', #38180, 0.1574803149606299191 ) ;
#31375 = AXIS2_PLACEMENT_3D ( 'NONE', #43317, #32087, #25372 ) ;
#31376 = LINE ( 'NONE', #34253, #43460 ) ;
#31377 = CARTESIAN_POINT ( 'NONE',  ( -0.06523048226347956391, -0.6008858266641260437, 0.1574803149606297803 ) ) ;
#31379 = DIRECTION ( 'NONE',  ( 0.000000000000000000, 0.6156614753256578476, 0.7880107536067223473 ) ) ;
#31378 = CARTESIAN_POINT ( 'NONE',  ( 0.9873396505805591694, 0.1113553986120547346, 0.1722440944881890035 ) ) ;
#31380 = CARTESIAN_POINT ( 'NONE',  ( -0.8107537697050254399, -0.1574803149606297803, 1.257381889763780736 ) ) ;
#31381 = CARTESIAN_POINT ( 'NONE',  ( -0.1659561666016914627, -0.08956010649363622955, -0.04686757988705942540 ) ) ;
#31382 = CARTESIAN_POINT ( 'NONE',  ( 0.1264236179284866091, -0.4876968503399370380, -0.1264236179284866091 ) ) ;
#31383 = ORIENTED_EDGE ( 'NONE', *, *, #10237, .T. ) ;
#31384 = AXIS2_PLACEMENT_3D ( 'NONE', #22405, #15478, #32990 ) ;
#31385 = CARTESIAN_POINT ( 'NONE',  ( 0.06841996760812382727, 0.1299212598425196763, 0.1651804176431311000 ) ) ;
#31386 = CARTESIAN_POINT ( 'NONE',  ( 0.7185039370078739607, 1.928577636452523993E-17, 1.171259842519684957 ) ) ;
#31387 = CARTESIAN_POINT ( 'NONE',  ( 1.002407869896990045, -0.1264236179284866091, 0.8439960629383622681 ) ) ;
#31388 = ORIENTED_EDGE ( 'NONE', *, *, #45584, .T. ) ;
#31389 = CYLINDRICAL_SURFACE ( 'NONE', #35648, 0.2362204724409449064 ) ;
#31390 = CARTESIAN_POINT ( 'NONE',  ( 0.000000000000000000, 0.000000000000000000, 0.000000000000000000 ) ) ;
#31391 = CARTESIAN_POINT ( 'NONE',  ( 0.1787899950787401604, -1.710629921206078041, -0.07405724077823318263 ) ) ;
#31392 = CARTESIAN_POINT ( 'NONE',  ( 0.1787899950787401882, -1.048720472387181024, -2.189545951927503898E-17 ) ) ;
#31393 = CARTESIAN_POINT ( 'NONE',  ( -0.06523048226347956391, -1.373523622047243320, -0.1574803149606300301 ) ) ;
#31394 = CARTESIAN_POINT ( 'NONE',  ( 1.033464566929133799, 0.000000000000000000, 1.181102362097196989 ) ) ;
#31395 = ORIENTED_EDGE ( 'NONE', *, *, #26978, .T. ) ;
#31396 = CARTESIAN_POINT ( 'NONE',  ( -0.8759842519685039353, -0.1787899950787401882, 1.867618110182456714 ) ) ;
#31397 = CARTESIAN_POINT ( 'NONE',  ( 0.8759842519685039353, -0.1787899950787401882, 1.867618110182456714 ) ) ;
#31398 = ORIENTED_EDGE ( 'NONE', *, *, #7736, .T. ) ;
#31399 = CARTESIAN_POINT ( 'NONE',  ( 0.8759842519685039353, -0.1574803149606299191, 1.771653543307086576 ) ) ;
#31400 = CARTESIAN_POINT ( 'NONE',  ( -0.6971942568897648851, -0.07405724077823297447, 1.461614173174583753 ) ) ;
#31401 = DIRECTION ( 'NONE',  ( 0.000000000000000000, 0.000000000000000000, -1.000000000000000000 ) ) ;
#31402 = CARTESIAN_POINT ( 'NONE',  ( -0.9500414927467378812, 0.1787899950787401604, 0.3100393700249766682 ) ) ;
#31403 = AXIS2_PLACEMENT_3D ( 'NONE', #7598, #8304, #44018 ) ;
#31404 = DIRECTION ( 'NONE',  ( -0.7986355100472968260, 0.000000000000000000, 0.6018150231520429383 ) ) ;
#31405 = CARTESIAN_POINT ( 'NONE',  ( -1.054774247047244540, -0.07405724077823318263, 1.796259842465923073 ) ) ;
#31406 = CARTESIAN_POINT ( 'NONE',  ( 0.04858533447342753414, -0.07294156354243669371, -0.2573812140284293393 ) ) ;
#31407 = CARTESIAN_POINT ( 'NONE',  ( -0.7185039370078739607, 1.928577636452523993E-17, 1.722440944881889813 ) ) ;
#31408 = CARTESIAN_POINT ( 'NONE',  ( 0.5057057357416000487, -0.09842519685039370636, 1.205361022782828805E-17 ) ) ;
#31409 = CARTESIAN_POINT ( 'NONE',  ( 0.1787899950787401604, -0.2747302674418372059, 0.07405724077823318263 ) ) ;
#31410 = CARTESIAN_POINT ( 'NONE',  ( 0.8759842519685039353, 0.1787899950787401882, 1.690452755851748146 ) ) ;
#31411 = CARTESIAN_POINT ( 'NONE',  ( -0.04012737397972362258, -0.09842519685039370636, -0.1835268552075023374 ) ) ;
#31412 = CYLINDRICAL_SURFACE ( 'NONE', #46304, 0.1574803149606292529 ) ;
#31413 = DIMENSIONAL_EXPONENTS ( 1.000000000000000000, 0.000000000000000000, 0.000000000000000000, 0.000000000000000000, 0.000000000000000000, 0.000000000000000000, 0.000000000000000000 ) ;
#31414 = EDGE_CURVE ( 'NONE', #41019, #45599, #5830, .T. ) ;
#31415 = EDGE_LOOP ( 'NONE', ( #43006, #9913, #20296, #37593 ) ) ;
#31416 = CARTESIAN_POINT ( 'NONE',  ( -0.7495606340400177148, 0.1264236179284866091, 1.301673228292692830 ) ) ;
#31417 = ADVANCED_FACE ( 'NONE', ( #27902 ), #43634, .T. ) ;
#31418 = CARTESIAN_POINT ( 'NONE',  ( -0.07405724077823318263, -0.9822834645131651721, 0.1787899950787401604 ) ) ;
#31419 = CARTESIAN_POINT ( 'NONE',  ( 0.07405724077823318263, -1.208661417269070393, 0.1787899950787401604 ) ) ;
#31420 = LINE ( 'NONE', #35475, #14872 ) ;
#31421 = CARTESIAN_POINT ( 'NONE',  ( -0.07444174185955065859, -0.4660871166696600731, 0.1797182628040039087 ) ) ;
#31422 = CARTESIAN_POINT ( 'NONE',  ( 0.1476377952755906220, -0.4812165006432430059, -0.8611016091043821596 ) ) ;
#31423 = CARTESIAN_POINT ( 'NONE',  ( -0.8107537697050253289, -0.1574803149606297803, 0.7750984250893222516 ) ) ;
#31424 = CARTESIAN_POINT ( 'NONE',  ( -0.8107537697050253289, -0.1574803149606297803, 0.6668307086614162493 ) ) ;
#31425 = CARTESIAN_POINT ( 'NONE',  ( 0.06523048226347956391, -0.01525590551181101734, 0.1574803149606297803 ) ) ;
#31426 = CARTESIAN_POINT ( 'NONE',  ( 0.7495606340400177148, -0.1264236179284866091, 0.9916338582139527791 ) ) ;
#31427 = CARTESIAN_POINT ( 'NONE',  ( 1.054774247047244096, 0.000000000000000000, 1.995570866087968520 ) ) ;
#31428 = VECTOR ( 'NONE', #11215, 39.37007874015748143 ) ;
#31429 = EDGE_LOOP ( 'NONE', ( #11839, #41213, #15955, #35481, #35890, #23371 ) ) ;
#31430 = CARTESIAN_POINT ( 'NONE',  ( 0.8107537697050254399, -0.1574803149606297803, 0.3813976376877488139 ) ) ;
#31431 = CARTESIAN_POINT ( 'NONE',  ( -1.094772975963752103E-17, -0.6451771653005667906, -0.1787899950787401882 ) ) ;
#31432 = CONICAL_SURFACE ( 'NONE', #18, 0.1574803149606299191, 0.9599310885968735940 ) ;
#31433 = CARTESIAN_POINT ( 'NONE',  ( 0.1264236179284866091, -1.314468503883243988, -0.1264236179284866091 ) ) ;
#31434 = CARTESIAN_POINT ( 'NONE',  ( -0.6971942568897648851, 0.07405724077823318263, 1.929133858213952335 ) ) ;
#31435 = VERTEX_POINT ( 'NONE', #40045 ) ;
#31436 = CARTESIAN_POINT ( 'NONE',  ( -1.054774247047244540, 0.07405724077823318263, 1.486220472387181690 ) ) ;
#31437 = CARTESIAN_POINT ( 'NONE',  ( 1.002407869896990045, -0.1264236179284866091, 1.400098425143086800 ) ) ;
#31438 = LINE ( 'NONE', #35501, #2968 ) ;
#31439 = CARTESIAN_POINT ( 'NONE',  ( -0.8759842519685039353, -0.1787899950787401882, 0.6077755904974173617 ) ) ;
#31440 = CARTESIAN_POINT ( 'NONE',  ( 1.002407869896990045, -0.1264236179284866091, 0.1008858267178899676 ) ) ;
#31441 = CARTESIAN_POINT ( 'NONE',  ( 0.1697303854094444342, -0.09842519689050829856, -0.05760433632937374260 ) ) ;
#31442 = ( CONVERSION_BASED_UNIT ( 'INCH', #35505 ) LENGTH_UNIT ( ) NAMED_UNIT ( #6272 ) ) ;
#31443 = CARTESIAN_POINT ( 'NONE',  ( 0.6971942568897637749, 2.189545951927499583E-17, 0.6373031495525354195 ) ) ;
#31444 = CARTESIAN_POINT ( 'NONE',  ( -1.054774247047244540, 0.07405724077823318263, 0.5757874015210393548 ) ) ;
#31445 = CARTESIAN_POINT ( 'NONE',  ( 1.033464566929134687, -0.06523048226347956391, 0.6373031496062994128 ) ) ;
#31446 = CARTESIAN_POINT ( 'NONE',  ( 0.06523048226347956391, -0.07923228346456692717, -0.1574803149606300301 ) ) ;
#31447 = EDGE_LOOP ( 'NONE', ( #15854, #42712 ) ) ;
#31448 = CARTESIAN_POINT ( 'NONE',  ( -0.9412147342319837628, 0.1574803149606300301, 0.2928149606299214613 ) ) ;
#31449 = CARTESIAN_POINT ( 'NONE',  ( 0.8019270111902716547, 0.1787899950787401604, 1.338582677111590069 ) ) ;
#31450 = CARTESIAN_POINT ( 'NONE',  ( 0.2014638753618972489, -0.09851384545634704615, 0.06137933528758169471 ) ) ;
#31451 = DIRECTION ( 'NONE',  ( -1.000000000000000000, 0.000000000000000000, 0.000000000000000000 ) ) ;
#31452 = VERTEX_POINT ( 'NONE', #14208 ) ;
#31453 = CARTESIAN_POINT ( 'NONE',  ( -0.8019270111902717657, -0.1787899950787401604, 0.9202755904974182499 ) ) ;
#31454 = ADVANCED_FACE ( 'NONE', ( #10860 ), #6, .T. ) ;
#31455 = CIRCLE ( 'NONE', #39080, 0.7775590551181102983 ) ;
#31456 = CARTESIAN_POINT ( 'NONE',  ( -0.1264236179284866091, -1.546875936733175250, 0.1264236179284866091 ) ) ;
#31457 = ORIENTED_EDGE ( 'NONE', *, *, #43557, .T. ) ;
#31458 = CARTESIAN_POINT ( 'NONE',  ( 0.8759842519685039353, 0.1574803149606299191, 1.003937007874015741 ) ) ;
#31459 = CARTESIAN_POINT ( 'NONE',  ( -0.07405724077823318263, -0.6230314960092281362, 0.1787899950787401604 ) ) ;
#31460 = DIRECTION ( 'NONE',  ( 0.8191520442889949072, -0.4519843998600416302, 0.3531289150159167556 ) ) ;
#31461 = AXIS2_PLACEMENT_3D ( 'NONE', #20032, #1820, #31090 ) ;
#31462 = EDGE_CURVE ( 'NONE', #1966, #3336, #32219, .T. ) ;
#31463 = AXIS2_PLACEMENT_3D ( 'NONE', #30503, #45776, #34799 ) ;
#31464 = LINE ( 'NONE', #23787, #16976 ) ;
#31465 = CARTESIAN_POINT ( 'NONE',  ( -1.094772975963752103E-17, -0.2908464566391499861, -0.1787899950787401882 ) ) ;
#31466 = CARTESIAN_POINT ( 'NONE',  ( -0.07405724077823318263, -0.7805118109698575557, 0.1787899950787401604 ) ) ;
#31467 = CARTESIAN_POINT ( 'NONE',  ( 0.8107537697050234415, -0.1574803149606297803, 0.1845472439869611792 ) ) ;
#31468 = CARTESIAN_POINT ( 'NONE',  ( -0.4620708661417322616, 0.6102362204724407491, 0.9891732283464566011 ) ) ;
#31469 = CARTESIAN_POINT ( 'NONE',  ( -0.07405724077823318263, 0.06975792153454075939, 0.1787899950787401604 ) ) ;
#31470 = CONTEXT_DEPENDENT_SHAPE_REPRESENTATION ( #24485, #36788 ) ;
#31471 = CARTESIAN_POINT ( 'NONE',  ( 0.2559055118110236116, -0.07734300567387089598, -0.3083604012389705717 ) ) ;
#31472 = CARTESIAN_POINT ( 'NONE',  ( 0.8759842519685039353, 0.1787899950787401882, 0.4256889763241890057 ) ) ;
#31473 = ( BOUNDED_CURVE ( )  B_SPLINE_CURVE ( 2, ( #33830, #16317, #22534, #19413, #7919, #34063, #18933, #34516, #33592 ),
 .UNSPECIFIED., .F., .F. ) 
 B_SPLINE_CURVE_WITH_KNOTS ( ( 3, 2, 2, 2, 3 ),
 ( 0.4899999999999999911, 0.4924999999999999933, 0.4949999999999999956, 0.4974999999999999978, 0.5000000000000000000 ),
 .UNSPECIFIED. ) 
 CURVE ( )  GEOMETRIC_REPRESENTATION_ITEM ( )  RATIONAL_B_SPLINE_CURVE ( ( 1.000000000000000000, 0.9238795325112869605, 1.000000000000000000, 0.9238795325112869605, 1.000000000000000000, 0.9238795325112869605, 1.000000000000000000, 0.9238795325112869605, 1.000000000000000000 ) ) 
 REPRESENTATION_ITEM ( '' )  ) ;
#31474 = CARTESIAN_POINT ( 'NONE',  ( -0.7495606340400177148, -0.1264236179284866091, 0.7603346456155274380 ) ) ;
#31476 = CARTESIAN_POINT ( 'NONE',  ( 0.9412147342319837628, 0.1574803149606300301, 0.08612204713656733401 ) ) ;
#31475 = CARTESIAN_POINT ( 'NONE',  ( 0.1113553986120547346, -0.9084645669291337988, -0.1113553986120547346 ) ) ;
#31477 = CARTESIAN_POINT ( 'NONE',  ( -0.1797182628040039087, -1.538921762338951060, -0.07444174185955065859 ) ) ;
#31478 = CARTESIAN_POINT ( 'NONE',  ( 0.4509871776442260227, 0.09842519685039370636, 1.205361022782828805E-17 ) ) ;
#31479 = CARTESIAN_POINT ( 'NONE',  ( 0.8759842519685039353, -0.1787899950787401882, 1.592027559001354398 ) ) ;
#31481 = CARTESIAN_POINT ( 'NONE',  ( 0.1617601974887943606, 0.1594115816221988724, 3.519129779734452560E-06 ) ) ;
#31480 = CARTESIAN_POINT ( 'NONE',  ( 0.000000000000000000, 0.000000000000000000, -0.04012007874015743186 ) ) ;
#31482 = CARTESIAN_POINT ( 'NONE',  ( 1.002407869896990045, -0.1264236179284866091, 0.4109251967966299213 ) ) ;
#31483 = ORIENTED_EDGE ( 'NONE', *, *, #22725, .F. ) ;
#31485 = ORIENTED_EDGE ( 'NONE', *, *, #15833, .T. ) ;
#31484 = FACE_OUTER_BOUND ( 'NONE', #44322, .T. ) ;
#31486 = FACE_OUTER_BOUND ( 'NONE', #7620, .T. ) ;
#31487 = DIRECTION ( 'NONE',  ( -3.662381193211854913E-16, 1.000000000000000000, 2.355041373848520102E-15 ) ) ;
#31488 = CARTESIAN_POINT ( 'NONE',  ( -0.07405724077823318263, 0.08070866147108628208, 0.1787899950787401604 ) ) ;
#31489 = LINE ( 'NONE', #23107, #188 ) ;
#31490 = CARTESIAN_POINT ( 'NONE',  ( 0.1787899950787401604, -0.05708661411946481384, -0.07405724077823318263 ) ) ;
#31491 = CARTESIAN_POINT ( 'NONE',  ( 0.6971942568897637749, 2.189545951927499583E-17, 0.3961614172690708924 ) ) ;
#31492 = EDGE_CURVE ( 'NONE', #22330, #33536, #44122, .T. ) ;
#31493 = CARTESIAN_POINT ( 'NONE',  ( -0.1264236179284866091, -0.9404527558517480346, 0.1264236179284866091 ) ) ;
#31494 = FACE_OUTER_BOUND ( 'NONE', #6174, .T. ) ;
#31495 = CARTESIAN_POINT ( 'NONE',  ( 0.7185039370078739607, 0.000000000000000000, 2.007874015640504162 ) ) ;
#31496 = CIRCLE ( 'NONE', #30016, 0.08090551181102362266 ) ;
#31497 = CARTESIAN_POINT ( 'NONE',  ( -0.8019270111902717657, 0.1787899950787401604, 1.412401574749386990 ) ) ;
#31498 = ORIENTED_EDGE ( 'NONE', *, *, #10077, .T. ) ;
#31499 = DIRECTION ( 'NONE',  ( -0.000000000000000000, -1.000000000000000000, -0.000000000000000000 ) ) ;
#31500 = CARTESIAN_POINT ( 'NONE',  ( 0.8019270111902717657, 0.1787899950787401604, 0.9448818897100165204 ) ) ;
#31501 = CARTESIAN_POINT ( 'NONE',  ( -0.7185039370078739607, 1.928577636452523993E-17, 0.4921259841444416971 ) ) ;
#31502 = VECTOR ( 'NONE', #28713, 39.37007874015748143 ) ;
#31503 = CARTESIAN_POINT ( 'NONE',  ( 0.7495606340400177148, -0.1264236179284866091, 1.739665354276945131 ) ) ;
#31504 = CARTESIAN_POINT ( 'NONE',  ( -0.9873396505805591694, -0.1113553986120547346, 1.382874015748031704 ) ) ;
#31505 = CARTESIAN_POINT ( 'NONE',  ( 0.000000000000000000, -5.122214988120488358E-16, -8.878505979408856939E-16 ) ) ;
#31507 = CARTESIAN_POINT ( 'NONE',  ( -0.02440571223931113296, -0.2814035877312771605, -0.08364281214758069460 ) ) ;
#31506 = CARTESIAN_POINT ( 'NONE',  ( 0.1279527559055118058, 0.2216206741968047289, -0.3149606299212598381 ) ) ;
#31508 = CARTESIAN_POINT ( 'NONE',  ( 1.002407869896990045, -0.1264236179284866091, 0.2189960629383626012 ) ) ;
#31509 = CARTESIAN_POINT ( 'NONE',  ( -1.002407869896990045, 0.1264236179284866091, 0.1058070865604098382 ) ) ;
#31510 = AXIS2_PLACEMENT_3D ( 'NONE', #42575, #1626, #38299 ) ;
#31511 = CARTESIAN_POINT ( 'NONE',  ( 1.033464566929134687, -0.06523048226347956391, 1.414862204616882835 ) ) ;
#31512 = VERTEX_POINT ( 'NONE', #3409 ) ;
#31513 = VERTEX_POINT ( 'NONE', #32671 ) ;
#31514 = CARTESIAN_POINT ( 'NONE',  ( -0.07405724077823318263, 0.08070866147108628208, 0.1787899950787401604 ) ) ;
#31515 = ORIENTED_EDGE ( 'NONE', *, *, #9639, .T. ) ;
#31516 = EDGE_CURVE ( 'NONE', #18913, #38550, #14440, .T. ) ;
#31517 = CARTESIAN_POINT ( 'NONE',  ( -0.8019270111902716547, -0.1787899950787401604, 1.624015747977732849 ) ) ;
#31518 = VERTEX_POINT ( 'NONE', #36257 ) ;
#31519 = EDGE_CURVE ( 'NONE', #40492, #40417, #43652, .T. ) ;
#31520 = CARTESIAN_POINT ( 'NONE',  ( 0.1377952755905511861, 0.000000000000000000, -0.01478361295688420882 ) ) ;
#31521 = CARTESIAN_POINT ( 'NONE',  ( 0.8759842519685039353, 0.000000000000000000, 4.498031496062992574 ) ) ;
#31522 = DIRECTION ( 'NONE',  ( 1.822029033848725028E-16, 0.000000000000000000, 1.000000000000000000 ) ) ;
#31523 = CARTESIAN_POINT ( 'NONE',  ( -0.1787899950787401604, -1.121186960355223139, -0.07405724077823318263 ) ) ;
#31524 = VERTEX_POINT ( 'NONE', #18025 ) ;
#31525 = CARTESIAN_POINT ( 'NONE',  ( 0.1787899950787401882, -0.1382874015210395768, -2.189545951927503898E-17 ) ) ;
#31526 = VERTEX_POINT ( 'NONE', #6997 ) ;
#31527 = ORIENTED_EDGE ( 'NONE', *, *, #9766, .T. ) ;
#31528 = CARTESIAN_POINT ( 'NONE',  ( 0.8019270111902717657, -0.1787899950787401604, 1.112204724355684959 ) ) ;
#31529 = ADVANCED_FACE ( 'NONE', ( #47013 ), #11321, .T. ) ;
#31530 = CARTESIAN_POINT ( 'NONE',  ( -0.2559027535725037494, -0.08943520109415376007, -0.3062076317311127061 ) ) ;
#31531 = DIRECTION ( 'NONE',  ( 1.000000000000000000, 0.000000000000000000, 0.000000000000000000 ) ) ;
#31532 = EDGE_CURVE ( 'NONE', #27412, #34797, #5267, .T. ) ;
#31533 = CARTESIAN_POINT ( 'NONE',  ( 0.9873396505805591694, 0.1113553986120547346, 1.904527559055118280 ) ) ;
#31534 = AXIS2_PLACEMENT_3D ( 'NONE', #8689, #15908, #29843 ) ;
#31535 = CIRCLE ( 'NONE', #30792, 0.1574803149606299191 ) ;
#31536 = CARTESIAN_POINT ( 'NONE',  ( -0.1264236179284866091, -0.6796259841982046357, -0.1264236179284866091 ) ) ;
#31537 = CARTESIAN_POINT ( 'NONE',  ( -0.7495606340400177148, 0.1264236179284866091, 0.3567913385289137596 ) ) ;
#31538 = CARTESIAN_POINT ( 'NONE',  ( -0.7646288533564489232, 0.1113553986120547346, 0.9694881889763780070 ) ) ;
#31540 = CARTESIAN_POINT ( 'NONE',  ( -0.7111459129584819516, 0.01515968786127315504, 1.982990166292141643 ) ) ;
#31539 = CARTESIAN_POINT ( 'NONE',  ( 0.1797182628040039365, -1.083705226905880004, -2.200913952912460540E-17 ) ) ;
#31541 = CARTESIAN_POINT ( 'NONE',  ( -0.1660477163176994342, 0.1996265385480609222, -0.03544556188504487115 ) ) ;
#31542 = CARTESIAN_POINT ( 'NONE',  ( 1.054774247047244096, 0.000000000000000000, 1.090059055064346527 ) ) ;
#31543 = CARTESIAN_POINT ( 'NONE',  ( 1.002407869896990045, 0.1264236179284866091, 1.601870078686393750 ) ) ;
#31544 = CARTESIAN_POINT ( 'NONE',  ( 1.002407869896990045, 0.1264236179284866091, 0.2239173227808822775 ) ) ;
#31545 = DIRECTION ( 'NONE',  ( 1.822029033848725028E-16, 0.000000000000000000, 1.000000000000000000 ) ) ;
#31546 = CARTESIAN_POINT ( 'NONE',  ( 0.7646288533564489232, 0.1113553986120547346, 1.678149606299212726 ) ) ;
#31548 = CARTESIAN_POINT ( 'NONE',  ( -0.8370031021572473806, 0.1539506378960530386, 1.979113158066270639 ) ) ;
#31547 = CARTESIAN_POINT ( 'NONE',  ( -0.1184675242425147906, -0.09842519685039369248, 1.555605046820496273 ) ) ;
#31549 = FACE_OUTER_BOUND ( 'NONE', #25889, .T. ) ;
#31550 = CARTESIAN_POINT ( 'NONE',  ( -0.06523048226347956391, -0.7189960628845993851, 0.1574803149606297803 ) ) ;
#31551 = CARTESIAN_POINT ( 'NONE',  ( -0.1787899950787401604, 0.04133858273092887170, 0.07405724077823318263 ) ) ;
#31552 = FACE_OUTER_BOUND ( 'NONE', #4454, .T. ) ;
#31553 = CARTESIAN_POINT ( 'NONE',  ( 0.8759842519685039353, -0.1787899950787401882, 0.9178149605761574126 ) ) ;
#31554 = CARTESIAN_POINT ( 'NONE',  ( 0.8759842519685039353, 0.1787899950787401882, 1.966043307032850462 ) ) ;
#31555 = CARTESIAN_POINT ( 'NONE',  ( 0.8107537697050253289, 0.1574803149606300301, 0.3272637794200322636 ) ) ;
#31556 = ORIENTED_EDGE ( 'NONE', *, *, #24615, .T. ) ;
#31557 = FACE_OUTER_BOUND ( 'NONE', #44081, .T. ) ;
#31558 = CARTESIAN_POINT ( 'NONE',  ( 1.031069757465331804, 0.04013614735736921457, 0.03937007433850867738 ) ) ;
#31559 = CARTESIAN_POINT ( 'NONE',  ( -0.8759842519685039353, -0.1574803149606299191, 0.2263779526483783444 ) ) ;
#31560 = CARTESIAN_POINT ( 'NONE',  ( 0.9500414927467378812, -0.1787899950787401604, 1.313976377898992132 ) ) ;
#31561 = PRESENTATION_LAYER_ASSIGNMENT (  '', '', ( #25436 ) ) ;
#31562 = ORIENTED_EDGE ( 'NONE', *, *, #29904, .T. ) ;
#31564 = CARTESIAN_POINT ( 'NONE',  ( 0.8759842519685039353, -0.1574803149606299191, 0.06889763768774861963 ) ) ;
#31563 = DIRECTION ( 'NONE',  ( -4.336808689942014285E-16, 0.000000000000000000, -1.000000000000000000 ) ) ;
#31565 = CARTESIAN_POINT ( 'NONE',  ( 0.1264236179284866091, 0.1422244095025824717, -0.1264236179284866091 ) ) ;
#31566 = CARTESIAN_POINT ( 'NONE',  ( -0.7185039370078739607, 1.928577636452523993E-17, 1.003937007766488199 ) ) ;
#31567 = VECTOR ( 'NONE', #13844, 39.37007874015748143 ) ;
#31568 = DIRECTION ( 'NONE',  ( 0.000000000000000000, -0.000000000000000000, 1.000000000000000000 ) ) ;
#31569 = LINE ( 'NONE', #20280, #20722 ) ;
#31570 = ORIENTED_EDGE ( 'NONE', *, *, #40721, .F. ) ;
#31571 = ADVANCED_FACE ( 'NONE', ( #23228 ), #271, .T. ) ;
#31572 = VERTEX_POINT ( 'NONE', #34030 ) ;
#31573 = CARTESIAN_POINT ( 'NONE',  ( 0.1787899950787401604, -1.715551181048599716, -0.07405724077823318263 ) ) ;
#31574 = VECTOR ( 'NONE', #44746, 39.37007874015748143 ) ;
#31575 = VECTOR ( 'NONE', #42685, 39.37007874015748854 ) ;
#31576 = CARTESIAN_POINT ( 'NONE',  ( -1.002407869896990045, 0.1264236179284866091, 1.916830708607653477 ) ) ;
#31577 = ORIENTED_EDGE ( 'NONE', *, *, #25450, .F. ) ;
#31578 = CARTESIAN_POINT ( 'NONE',  ( -0.7495606340400177148, -0.1264236179284866091, 0.6815944881352126172 ) ) ;
#31579 = CARTESIAN_POINT ( 'NONE',  ( 0.5555748031496086092, 0.2597269656108935343, 0.7480314960629921295 ) ) ;
#31580 = CARTESIAN_POINT ( 'NONE',  ( 3.284318927891251994E-17, -0.6758129446071911017, 0.1787899950787401882 ) ) ;
#31581 = ORIENTED_EDGE ( 'NONE', *, *, #36215, .F. ) ;
#31582 = CARTESIAN_POINT ( 'NONE',  ( 0.1289854442636478304, -0.08956037640241240605, -0.1454962696668769817 ) ) ;
#31583 = DIRECTION ( 'NONE',  ( 0.000000000000000000, 0.000000000000000000, -1.000000000000000000 ) ) ;
#31584 = ORIENTED_EDGE ( 'NONE', *, *, #34875, .F. ) ;
#31585 = DIRECTION ( 'NONE',  ( 2.787771407953479926E-15, 0.7829934116339072325, 0.6220299971367093672 ) ) ;
#31586 = EDGE_CURVE ( 'NONE', #40074, #12155, #8475, .T. ) ;
#31587 = CARTESIAN_POINT ( 'NONE',  ( -1.054774247047244096, 0.000000000000000000, 0.5733267715997795166 ) ) ;
#31588 = DIRECTION ( 'NONE',  ( -1.000000000000000000, 0.000000000000000000, 0.000000000000000000 ) ) ;
#31589 = EDGE_LOOP ( 'NONE', ( #9753, #38616, #29386, #8669 ) ) ;
#31590 = CARTESIAN_POINT ( 'NONE',  ( -0.7495606340400177148, -0.1264236179284866091, 1.587106299158834721 ) ) ;
#31591 = DIRECTION ( 'NONE',  ( -0.8191520442890534159, 0.000000000000000000, -0.5735764363509581187 ) ) ;
#31592 = ( BOUNDED_CURVE ( )  B_SPLINE_CURVE ( 2, ( #23459, #30433, #34726, #1379, #9304, #23219, #41862, #19368, #34023 ),
 .UNSPECIFIED., .F., .T. ) 
 B_SPLINE_CURVE_WITH_KNOTS ( ( 3, 2, 2, 2, 3 ),
 ( 0.1700000000000000122, 0.1724999999999999867, 0.1749999999999999889, 0.1774999999999999911, 0.1799999999999999933 ),
 .UNSPECIFIED. ) 
 CURVE ( )  GEOMETRIC_REPRESENTATION_ITEM ( )  RATIONAL_B_SPLINE_CURVE ( ( 1.000000000000000000, 0.9238795325112869605, 1.000000000000000000, 0.9238795325112869605, 1.000000000000000000, 0.9238795325112869605, 1.000000000000000000, 0.9238795325112869605, 1.000000000000000000 ) ) 
 REPRESENTATION_ITEM ( '' )  ) ;
#31593 = CARTESIAN_POINT ( 'NONE',  ( -0.1574803149606299191, 0.1005108776172155410, -0.1165245190822937899 ) ) ;
#31594 = CARTESIAN_POINT ( 'NONE',  ( 0.7646288533564489232, 0.1113553986120547346, 0.6545275590551181688 ) ) ;
#31595 = EDGE_LOOP ( 'NONE', ( #46489, #33187, #44214, #33688 ) ) ;
#31596 = CARTESIAN_POINT ( 'NONE',  ( 1.033464566929134687, -0.06523048226347956391, 0.5979330708661413363 ) ) ;
#31597 = CARTESIAN_POINT ( 'NONE',  ( 0.9873396505805591694, 0.1113553986120547346, 0.6348425195775118102 ) ) ;
#31598 = CARTESIAN_POINT ( 'NONE',  ( -0.7646288533564489232, 0.1113553986120547346, 1.235236220364913207 ) ) ;
#31600 = LINE ( 'NONE', #11140, #45387 ) ;
#31599 = CARTESIAN_POINT ( 'NONE',  ( -0.1574803149606297803, -0.4975393700787406059, 0.06523048226347956391 ) ) ;
#31601 = ( GEOMETRIC_REPRESENTATION_CONTEXT ( 3 ) GLOBAL_UNCERTAINTY_ASSIGNED_CONTEXT ( ( #44658 ) ) GLOBAL_UNIT_ASSIGNED_CONTEXT ( ( #39792, #6742, #17773 ) ) REPRESENTATION_CONTEXT ( 'NONE', 'WORKASPACE' ) ) ;
#31602 = CARTESIAN_POINT ( 'NONE',  ( 0.3690944881889778317, 3.409318977613033647E-15, -0.7480314960629921295 ) ) ;
#31603 = ORIENTED_EDGE ( 'NONE', *, *, #9816, .T. ) ;
#31604 = LINE ( 'NONE', #27316, #17694 ) ;
#31605 = CARTESIAN_POINT ( 'NONE',  ( 0.9873396505805591694, 0.1113553986120547346, 1.156496062992125928 ) ) ;
#31607 = CYLINDRICAL_SURFACE ( 'NONE', #30873, 0.5708661417322835607 ) ;
#31606 = CARTESIAN_POINT ( 'NONE',  ( 0.4453382816733590377, 4.766607801171850497E-17, 0.000000000000000000 ) ) ;
#31608 = CYLINDRICAL_SURFACE ( 'NONE', #22066, 0.1574803149606299191 ) ;
#31609 = LINE ( 'NONE', #41871, #39225 ) ;
#31610 = LINE ( 'NONE', #32321, #33112 ) ;
#31611 = LINE ( 'NONE', #16973, #24579 ) ;
#31612 = PRODUCT_DEFINITION_SHAPE ( 'NONE', 'NONE',  #7809 ) ;
#31613 = CARTESIAN_POINT ( 'NONE',  ( 0.1787899950787401604, -0.5688976377415115859, -0.07405724077823318263 ) ) ;
#31614 = ORIENTED_EDGE ( 'NONE', *, *, #9595, .F. ) ;
#31615 = CONICAL_SURFACE ( 'NONE', #14007, 0.2471922904502826812, 0.5235987755982992597 ) ;
#31616 = LINE ( 'NONE', #2345, #12363 ) ;
#31617 = CARTESIAN_POINT ( 'NONE',  ( 0.9500414927467378812, -0.1787899950787401604, 0.8809055117572599514 ) ) ;
#31618 = ADVANCED_FACE ( 'NONE', ( #41389 ), #23025, .F. ) ;
#31619 = CARTESIAN_POINT ( 'NONE',  ( -0.05837987205261271212, 0.07899857248962625922, -0.2517274360213099804 ) ) ;
#31620 = CYLINDRICAL_SURFACE ( 'NONE', #19713, 0.1574803149606299191 ) ;
#31621 = CARTESIAN_POINT ( 'NONE',  ( -0.07444174185955065859, 0.1097002849051434414, -0.1797182628040039087 ) ) ;
#31622 = CARTESIAN_POINT ( 'NONE',  ( -1.094772975963752103E-17, -1.078248031442299304, -0.1787899950787401882 ) ) ;
#31623 = CARTESIAN_POINT ( 'NONE',  ( 0.1113553986120547346, -1.351377952755905554, 0.1113553986120547346 ) ) ;
#31625 = ( BOUNDED_CURVE ( )  B_SPLINE_CURVE ( 2, ( #36058, #18080, #39870, #25538, #21189, #2736, #6578, #43711, #24564 ),
 .UNSPECIFIED., .F., .T. ) 
 B_SPLINE_CURVE_WITH_KNOTS ( ( 3, 2, 2, 2, 3 ),
 ( 0.9599999999999999645, 0.9625000000000000222, 0.9649999999999999689, 0.9675000000000000266, 0.9699999999999999734 ),
 .UNSPECIFIED. ) 
 CURVE ( )  GEOMETRIC_REPRESENTATION_ITEM ( )  RATIONAL_B_SPLINE_CURVE ( ( 1.000000000000000000, 0.9238795325112869605, 1.000000000000000000, 0.9238795325112869605, 1.000000000000000000, 0.9238795325112869605, 1.000000000000000000, 0.9238795325112869605, 1.000000000000000000 ) ) 
 REPRESENTATION_ITEM ( '' )  ) ;
#31624 = CARTESIAN_POINT ( 'NONE',  ( 0.7185039370078746268, 0.06523048226347956391, 1.277066929026331898 ) ) ;
#31626 = EDGE_CURVE ( 'NONE', #7863, #6761, #33715, .T. ) ;
#31627 = DIRECTION ( 'NONE',  ( -1.000000000000000000, -3.552713678800500140E-15, 0.000000000000000000 ) ) ;
#31628 = ORIENTED_EDGE ( 'NONE', *, *, #45281, .F. ) ;
#31629 = CARTESIAN_POINT ( 'NONE',  ( -1.054774247047244540, -0.07405724077823318263, 1.993110236166711013 ) ) ;
#31630 = EDGE_CURVE ( 'NONE', #9851, #11117, #20232, .T. ) ;
#31631 = ORIENTED_EDGE ( 'NONE', *, *, #424, .T. ) ;
#31632 = CARTESIAN_POINT ( 'NONE',  ( -0.1113553986120547346, -1.430118110128692832, 0.1113553986120547346 ) ) ;
#31633 = CARTESIAN_POINT ( 'NONE',  ( 1.350095158311321523E-16, 0.000000000000000000, 0.2952755905511816326 ) ) ;
#31634 = CARTESIAN_POINT ( 'NONE',  ( -0.9500414927467378812, -0.1787899950787401604, 1.550196850339937926 ) ) ;
#31635 = CARTESIAN_POINT ( 'NONE',  ( -0.7495606340400177148, 0.1264236179284866091, 1.021161417269070837 ) ) ;
#31636 = CARTESIAN_POINT ( 'NONE',  ( -1.002407869896990045, 0.1264236179284866091, 0.1894685038832444879 ) ) ;
#31637 = ( GEOMETRIC_REPRESENTATION_CONTEXT ( 3 ) GLOBAL_UNCERTAINTY_ASSIGNED_CONTEXT ( ( #11990 ) ) GLOBAL_UNIT_ASSIGNED_CONTEXT ( ( #45107, #11611, #30096 ) ) REPRESENTATION_CONTEXT ( 'NONE', 'WORKASPACE' ) ) ;
#31638 = DIRECTION ( 'NONE',  ( 0.000000000000000000, 0.000000000000000000, 1.000000000000000000 ) ) ;
#31639 = CARTESIAN_POINT ( 'NONE',  ( -0.6971942568897648851, 0.07405724077823318263, 1.934055118056471567 ) ) ;
#31640 = CARTESIAN_POINT ( 'NONE',  ( -0.1378230750848668529, 0.09774221684002683264, 0.2058608813653518832 ) ) ;
#31641 = CARTESIAN_POINT ( 'NONE',  ( -0.7185039370078746268, 0.06523048226347956391, 1.877460629921260393 ) ) ;
#31642 = CARTESIAN_POINT ( 'NONE',  ( 0.2559054633625183484, 0.04128200529817901976, -0.03449252736539545894 ) ) ;
#31643 = CARTESIAN_POINT ( 'NONE',  ( -0.1787899950787401604, -0.2894940469693961238, 0.07405724077823318263 ) ) ;
#31644 = CARTESIAN_POINT ( 'NONE',  ( 0.1954512992741562760, -0.09842519685039370636, 0.08123841634054980443 ) ) ;
#31645 = CARTESIAN_POINT ( 'NONE',  ( -0.1574803149606299191, 0.01181102362204724393, 0.000000000000000000 ) ) ;
#31646 = DIRECTION ( 'NONE',  ( -1.000000000000000000, 0.000000000000000000, 0.000000000000000000 ) ) ;
#31647 = AXIS2_PLACEMENT_3D ( 'NONE', #32834, #22484, #10789 ) ;
#31648 = AXIS2_PLACEMENT_3D ( 'NONE', #25658, #47210, #22040 ) ;
#31649 = AXIS2_PLACEMENT_3D ( 'NONE', #30809, #2012, #27693 ) ;
#31650 = ORIENTED_EDGE ( 'NONE', *, *, #6862, .F. ) ;
#31651 = VERTEX_POINT ( 'NONE', #45709 ) ;
#31652 = CARTESIAN_POINT ( 'NONE',  ( -0.07405724077823318263, -1.061023621993481214, 0.1787899950787401604 ) ) ;
#31653 = CARTESIAN_POINT ( 'NONE',  ( 0.1787899950787401882, -1.201279527505291433, -2.189545951927503898E-17 ) ) ;
#31654 = CARTESIAN_POINT ( 'NONE',  ( 0.5555748031496077211, 2.762335417273526192E-15, -0.7480314960629921295 ) ) ;
#31655 = CARTESIAN_POINT ( 'NONE',  ( 0.07444174185955065859, -0.5399060143074553286, 0.1797182628040039087 ) ) ;
#31656 = LINE ( 'NONE', #10306, #38567 ) ;
#31657 = CARTESIAN_POINT ( 'NONE',  ( -0.8107537697050253289, -0.1574803149606297803, 0.8144685038294804391 ) ) ;
#31658 = CARTESIAN_POINT ( 'NONE',  ( -1.033464566929134687, -0.06523048226347956391, 0.7554133858267707557 ) ) ;
#31659 = CARTESIAN_POINT ( 'NONE',  ( 2.892866454678787531E-17, 0.02165354330708661734, 0.1574803149606299191 ) ) ;
#31660 = CARTESIAN_POINT ( 'NONE',  ( 1.054774247047244540, 0.07405724077823318263, 0.9301181101824563813 ) ) ;
#31661 = DIRECTION ( 'NONE',  ( 1.000000000000000000, -3.469446951953614189E-15, -1.144917494144692682E-16 ) ) ;
#31663 = SURFACE_STYLE_FILL_AREA ( #28297 ) ;
#31662 = DIRECTION ( 'NONE',  ( 0.6018150231520356108, -0.000000000000000000, -0.7986355100473022661 ) ) ;
#31664 = CARTESIAN_POINT ( 'NONE',  ( 0.7185039370078746268, 0.06523048226347956391, 0.2140748030420794590 ) ) ;
#31665 = ORIENTED_EDGE ( 'NONE', *, *, #42772, .T. ) ;
#31666 = ORIENTED_EDGE ( 'NONE', *, *, #14771, .T. ) ;
#31667 = CARTESIAN_POINT ( 'NONE',  ( 1.033464566929133799, 0.000000000000000000, 0.2066929133858267931 ) ) ;
#31668 = CARTESIAN_POINT ( 'NONE',  ( 0.9412147342319837628, -0.1574803149606297803, 0.3863188975302684347 ) ) ;
#31669 = CARTESIAN_POINT ( 'NONE',  ( -0.1787899950787401604, -0.5541338582139530011, 0.07405724077823318263 ) ) ;
#31670 = CARTESIAN_POINT ( 'NONE',  ( -0.1787899950787401604, -1.341535433017102541, -0.07405724077823318263 ) ) ;
#31671 = EDGE_CURVE ( 'NONE', #32150, #712, #19616, .T. ) ;
#31672 = CARTESIAN_POINT ( 'NONE',  ( -0.6971942568897648851, -0.07405724077823297447, 1.973425196796630088 ) ) ;
#31673 = ORIENTED_EDGE ( 'NONE', *, *, #17171, .F. ) ;
#31674 = ORIENTED_EDGE ( 'NONE', *, *, #17151, .F. ) ;
#31675 = CARTESIAN_POINT ( 'NONE',  ( -0.9500414927467378812, -0.1787899950787401604, 1.437007873961985371 ) ) ;
#31676 = ADVANCED_FACE ( 'NONE', ( #42108 ), #30674, .F. ) ;
#31677 = CARTESIAN_POINT ( 'NONE',  ( 0.6971942568897648851, 0.07405724077823318263, 1.422244094434426120 ) ) ;
#31678 = CARTESIAN_POINT ( 'NONE',  ( -7.957671378281915615E-17, 0.1564960629921311464, -0.2933070866141737065 ) ) ;
#31679 = CARTESIAN_POINT ( 'NONE',  ( -1.054774247047244096, 0.000000000000000000, 0.5782480314422993040 ) ) ;
#31680 = CARTESIAN_POINT ( 'NONE',  ( 0.8759842519685039353, 0.1787899950787401882, 0.1550196849856066983 ) ) ;
#31681 = ADVANCED_FACE ( 'NONE', ( #46191 ), #13090, .T. ) ;
#31682 = CARTESIAN_POINT ( 'NONE',  ( 0.1781957201322358353, -0.09842519685039370636, -0.01456528979491370120 ) ) ;
#31683 = CARTESIAN_POINT ( 'NONE',  ( 1.054774247047244540, -0.07405724077823318263, 0.6545275590013546196 ) ) ;
#31684 = CARTESIAN_POINT ( 'NONE',  ( -0.6971942568897637749, 2.189545951927499583E-17, 0.4749015747493858242 ) ) ;
#31685 = CARTESIAN_POINT ( 'NONE',  ( 0.9412147342319837628, -0.1574803149606297803, 0.6323818897637792924 ) ) ;
#31686 = CYLINDRICAL_SURFACE ( 'NONE', #6084, 0.1574803149606299191 ) ;
#31687 = ORIENTED_EDGE ( 'NONE', *, *, #3121, .T. ) ;
#31688 = CARTESIAN_POINT ( 'NONE',  ( -0.7495606340400177148, 0.1264236179284866091, 1.498523621993480326 ) ) ;
#31689 = EDGE_LOOP ( 'NONE', ( #25394, #37431, #44012, #3346 ) ) ;
#31690 = DIRECTION ( 'NONE',  ( -1.000000000000000000, 0.000000000000000000, 0.000000000000000000 ) ) ;
#31691 = CARTESIAN_POINT ( 'NONE',  ( -0.8759842519685039353, 0.1574803149606299191, 0.4921259842519685179 ) ) ;
#31692 = CARTESIAN_POINT ( 'NONE',  ( 0.6971942568897637749, 2.189545951927499583E-17, 1.345964566875370139 ) ) ;
#31693 = CARTESIAN_POINT ( 'NONE',  ( 0.03861100025345957226, -0.09851384863655454627, 0.2192374635482165490 ) ) ;
#31694 = ORIENTED_EDGE ( 'NONE', *, *, #25596, .F. ) ;
#31695 = DIRECTION ( 'NONE',  ( -1.000000000000000000, 0.000000000000000000, 0.000000000000000000 ) ) ;
#31696 = CARTESIAN_POINT ( 'NONE',  ( -1.054774247047244540, -0.07405724077823318263, 0.9301181101824563813 ) ) ;
#31697 = ORIENTED_EDGE ( 'NONE', *, *, #17308, .T. ) ;
#31698 = CARTESIAN_POINT ( 'NONE',  ( -0.1787899950787401604, -0.5885826771115909573, 0.07405724077823318263 ) ) ;
#31699 = LENGTH_MEASURE_WITH_UNIT ( LENGTH_MEASURE( 0.02539999999999999897 ), #46044 ) ;
#31700 = ORIENTED_EDGE ( 'NONE', *, *, #8336, .F. ) ;
#31701 = AXIS2_PLACEMENT_3D ( 'NONE', #21488, #17421, #21251 ) ;
#31702 = CARTESIAN_POINT ( 'NONE',  ( -0.1787899950787401604, -0.7903543306548983516, -0.07405724077823318263 ) ) ;
#31703 = CARTESIAN_POINT ( 'NONE',  ( 0.8759842519685039353, -0.1574803149606299191, 0.1870078739082208508 ) ) ;
#31704 = CARTESIAN_POINT ( 'NONE',  ( 0.3161444924769515885, 0.4457451269443646336, -1.671447902550338815 ) ) ;
#31705 = CONICAL_SURFACE ( 'NONE', #19431, 0.09842519685039370636, 0.9599310885968824758 ) ;
#31706 = CARTESIAN_POINT ( 'NONE',  ( -0.1787899950787401604, -0.01390349578829383655, 0.07405724077823318263 ) ) ;
#31707 = CARTESIAN_POINT ( 'NONE',  ( -1.094772975963752103E-17, 0.02411417328210995956, -0.1787899950787401882 ) ) ;
#31708 = CONTEXT_DEPENDENT_SHAPE_REPRESENTATION ( #45585, #40972 ) ;
#31709 = CARTESIAN_POINT ( 'NONE',  ( 0.08053768427153103204, -0.09842519685039369248, 0.1460475935136278658 ) ) ;
#31710 = CARTESIAN_POINT ( 'NONE',  ( 0.6971942568897626646, -0.07405724077823297447, 0.4379921259304882519 ) ) ;
#31711 = DIMENSIONAL_EXPONENTS ( 1.000000000000000000, 0.000000000000000000, 0.000000000000000000, 0.000000000000000000, 0.000000000000000000, 0.000000000000000000, 0.000000000000000000 ) ;
#31712 = CARTESIAN_POINT ( 'NONE',  ( -0.9500414927467377701, -0.1787899950787401604, 0.7677165353793073965 ) ) ;
#31714 = FACE_OUTER_BOUND ( 'NONE', #22659, .T. ) ;
#31713 = CARTESIAN_POINT ( 'NONE',  ( 0.06523048226347956391, -0.9453740157480327033, -0.1574803149606300301 ) ) ;
#31715 = CARTESIAN_POINT ( 'NONE',  ( 0.07444174185955065859, -1.799748533992495014, 0.1797182628040039087 ) ) ;
#31716 = CARTESIAN_POINT ( 'NONE',  ( 0.8759842519685039353, -0.1787899950787401882, 1.552657480261196765 ) ) ;
#31718 = CARTESIAN_POINT ( 'NONE',  ( 0.1644020957507539848, 0.1623118080249112138, 1.367956046207553540E-19 ) ) ;
#31717 = CARTESIAN_POINT ( 'NONE',  ( 0.7495606340400177148, 0.1264236179284866091, 1.966043307032850462 ) ) ;
#31719 = CARTESIAN_POINT ( 'NONE',  ( 0.8019270111902716547, 0.1787899950787401604, 0.3494094487651343006 ) ) ;
#31720 = EDGE_LOOP ( 'NONE', ( #33251, #37119 ) ) ;
#31721 = CARTESIAN_POINT ( 'NONE',  ( -0.4620708661417322616, 0.9842519685039370358, -0.7135826771653542844 ) ) ;
#31722 = CARTESIAN_POINT ( 'NONE',  ( 0.8759842519685039353, 0.000000000000000000, 1.978346456692913646 ) ) ;
#31723 = LINE ( 'NONE', #46315, #43535 ) ;
#31724 = CARTESIAN_POINT ( 'NONE',  ( -0.1787899950787401604, -0.1210629920722208208, 0.07405724077823318263 ) ) ;
#31725 = CARTESIAN_POINT ( 'NONE',  ( 0.6971942568897637749, 2.189545951927499583E-17, 0.5536417322297008115 ) ) ;
#31726 = CARTESIAN_POINT ( 'NONE',  ( 0.1787899950787401882, -0.9256889763241890057, -2.189545951927503898E-17 ) ) ;
#31727 = ADVANCED_FACE ( 'NONE', ( #42362 ), #38070, .T. ) ;
#31728 = DIRECTION ( 'NONE',  ( -6.944548107256197364E-15, -0.7880107536067206819, 0.6156614753256598460 ) ) ;
#31729 = CARTESIAN_POINT ( 'NONE',  ( -0.7495606340400177148, -0.1264236179284866091, 1.464074803095842370 ) ) ;
#31730 = ORIENTED_EDGE ( 'NONE', *, *, #28240, .F. ) ;
#31731 = CARTESIAN_POINT ( 'NONE',  ( -0.1574803149606299191, 1.928577636452524610E-17, -0.1183602362204724257 ) ) ;
#31732 = CARTESIAN_POINT ( 'NONE',  ( 0.6971942568897648851, -0.07405724077823297447, 0.9940944881352130613 ) ) ;
#31733 = ORIENTED_EDGE ( 'NONE', *, *, #32553, .T. ) ;
#31734 = AXIS2_PLACEMENT_3D ( 'NONE', #33488, #26526, #44458 ) ;
#31735 = CIRCLE ( 'NONE', #37848, 0.02900000000000056352 ) ;
#31736 = CARTESIAN_POINT ( 'NONE',  ( -9.642888182262618425E-18, -1.090551180994834723, -0.1574803149606299191 ) ) ;
#31737 = CARTESIAN_POINT ( 'NONE',  ( -0.7646288533564489232, -0.1113553986120547346, 0.6545275589475906264 ) ) ;
#31738 = CARTESIAN_POINT ( 'NONE',  ( 0.7185039370078739607, 1.928577636452523993E-17, 1.486220472440944906 ) ) ;
#31739 = CARTESIAN_POINT ( 'NONE',  ( 1.002407869896990045, 0.1264236179284866091, 1.719980314906866203 ) ) ;
#31740 = CARTESIAN_POINT ( 'NONE',  ( -0.7646288533564489232, 0.1113553986120547346, 1.441929133858267598 ) ) ;
#31741 = CARTESIAN_POINT ( 'NONE',  ( -1.054774247047244540, -0.07405724077823318263, 0.8464566928596233275 ) ) ;
#31742 = EDGE_CURVE ( 'NONE', #36338, #41049, #6935, .T. ) ;
#31743 = DIRECTION ( 'NONE',  ( 0.000000000000000000, 0.000000000000000000, 1.000000000000000000 ) ) ;
#31744 = CARTESIAN_POINT ( 'NONE',  ( 0.3000685424736224127, 4.466152701071653354E-17, 0.000000000000000000 ) ) ;
#31745 = CARTESIAN_POINT ( 'NONE',  ( 1.002407869896990045, 0.1264236179284866091, 0.1107283464029293202 ) ) ;
#31746 = CARTESIAN_POINT ( 'NONE',  ( 1.033464566929133799, 0.000000000000000000, 1.496062992018456494 ) ) ;
#31747 = ORIENTED_EDGE ( 'NONE', *, *, #47184, .T. ) ;
#31748 = CARTESIAN_POINT ( 'NONE',  ( -0.1787899950787401604, 0.1102362205262043815, -0.07405724077823318263 ) ) ;
#31749 = CARTESIAN_POINT ( 'NONE',  ( 1.033464566929134687, 0.06523048226347956391, 1.774114173120820093 ) ) ;
#31751 = CLOSED_SHELL ( 'NONE', ( #47293, #4972, #18448, #29549, #1903, #16780, #28674, #6920, #17527, #15873, #30970, #19195, #36087, #14533, #9916, #32141, #8016, #6326, #27315, #5748, #33139, #41636, #3575, #15636, #39601, #14254, #39921, #9485, #27480, #44828, #28886, #7321, #36532, #3919, #37331, #25520, #5570, #32601, #33189, #730, #38632, #23444, #16646, #24617, #45380, #41241, #43922, #21719, #27041, #9864, #8039, #29598, #9323, #38538, #30357 ) ) ;
#31750 = VERTEX_POINT ( 'NONE', #38303 ) ;
#31752 = CARTESIAN_POINT ( 'NONE',  ( -1.054774247047244096, 0.000000000000000000, 1.754429133804503715 ) ) ;
#31753 = EDGE_LOOP ( 'NONE', ( #15969, #509, #6647, #43304 ) ) ;
#31754 = CARTESIAN_POINT ( 'NONE',  ( -0.7185039370078746268, 0.06523048226347956391, 0.6569881889763780070 ) ) ;
#31755 = CARTESIAN_POINT ( 'NONE',  ( 1.530041696156790562E-15, 0.4667239666988196034, -0.7023826619074857724 ) ) ;
#31756 = CARTESIAN_POINT ( 'NONE',  ( -1.094772975963752103E-17, -1.128568850119001876, -0.1787899950787401882 ) ) ;
#31757 = ORIENTED_EDGE ( 'NONE', *, *, #35766, .F. ) ;
#31758 = CARTESIAN_POINT ( 'NONE',  ( 3.284318927891251994E-17, -0.1874999999462366451, 0.1787899950787401882 ) ) ;
#31759 = ORIENTED_EDGE ( 'NONE', *, *, #22725, .T. ) ;
#31760 = VERTEX_POINT ( 'NONE', #38545 ) ;
#31761 = CARTESIAN_POINT ( 'NONE',  ( 0.3547871005709968273, 4.766607801171850497E-17, 0.000000000000000000 ) ) ;
#31762 = ADVANCED_FACE ( 'NONE', ( #8834 ), #23468, .T. ) ;
#31763 = CARTESIAN_POINT ( 'NONE',  ( -0.7185039370078739607, 1.928577636452523993E-17, 0.8169291338582678197 ) ) ;
#31764 = CARTESIAN_POINT ( 'NONE',  ( 1.033464566929134687, -0.06523048226347956391, 1.779035433070867089 ) ) ;
#31765 = VECTOR ( 'NONE', #38383, 39.37007874015748143 ) ;
#31767 = CARTESIAN_POINT ( 'NONE',  ( -0.1797182628040039365, -0.1585083765121793331, 0.000000000000000000 ) ) ;
#31766 = AXIS2_PLACEMENT_3D ( 'NONE', #31925, #28326, #5800 ) ;
#31768 = CARTESIAN_POINT ( 'NONE',  ( -0.1264236179284866091, -0.7189960629383621571, -0.1264236179284866091 ) ) ;
#31769 = ORIENTED_EDGE ( 'NONE', *, *, #39100, .T. ) ;
#31770 = CARTESIAN_POINT ( 'NONE',  ( -0.8759842519685039353, -0.1787899950787401882, 0.4109251967966299213 ) ) ;
#31771 = CARTESIAN_POINT ( 'NONE',  ( -1.033464566929134687, -0.06523048226347956391, 0.9916338582677171054 ) ) ;
#31772 = CARTESIAN_POINT ( 'NONE',  ( -0.07444174185955065859, -1.174748533992494126, 0.1797182628040039087 ) ) ;
#31773 = CARTESIAN_POINT ( 'NONE',  ( -0.2031507276427601261, 0.1782051049717913449, -0.05809220732314908375 ) ) ;
#31774 = B_SPLINE_CURVE_WITH_KNOTS ( 'NONE', 3,
 ( #31506, #23367, #12827, #5854, #27459, #2243, #2016, #37975, #34388, #34868, #30812, #37396, #7692, #34079, #4798, #26167, #30483 ),
 .UNSPECIFIED., .F., .F.,
 ( 4, 2, 2, 2, 2, 1, 2, 2, 4 ),
 ( 0.000000000000000000, 0.1250000000000009714, 0.1875000000000012768, 0.2500000000000012768, 0.3750000000000014433, 0.4375000000000018874, 0.4687500000000020539, 0.5000000000000021094, 1.000000000000000000 ),
 .UNSPECIFIED. ) ;
#31775 = CARTESIAN_POINT ( 'NONE',  ( 1.002407869896990045, 0.1264236179284866091, 1.094980314906866203 ) ) ;
#31776 = CARTESIAN_POINT ( 'NONE',  ( 1.054774247047244096, 0.000000000000000000, 1.478838582623401399 ) ) ;
#31777 = CARTESIAN_POINT ( 'NONE',  ( 0.6971942568897626646, 0.07405724077823318263, 0.1574803149068664809 ) ) ;
#31778 = CARTESIAN_POINT ( 'NONE',  ( 0.1574803149606299746, 0.3171096708378827178, -3.631137952917390166 ) ) ;
#31779 = EDGE_CURVE ( 'NONE', #6124, #7028, #42898, .T. ) ;
#31780 = LINE ( 'NONE', #46363, #30480 ) ;
#31781 = CARTESIAN_POINT ( 'NONE',  ( 0.1631287777903855374, -0.08016275093080070524, -0.1388449280286157550 ) ) ;
#31782 = CARTESIAN_POINT ( 'NONE',  ( 0.8107537697050254399, 0.1574803149606300301, 0.6815944880814486240 ) ) ;
#31783 = CARTESIAN_POINT ( 'NONE',  ( -0.7646288533564489232, 0.1113553986120547346, 1.707677165246803241 ) ) ;
#31784 = CARTESIAN_POINT ( 'NONE',  ( 0.3980944881889805775, 1.194414586609139795, -0.06082000038405787484 ) ) ;
#31785 = EDGE_CURVE ( 'NONE', #6423, #3799, #34480, .T. ) ;
#31787 = LINE ( 'NONE', #14027, #15450 ) ;
#31786 = CARTESIAN_POINT ( 'NONE',  ( 0.6971942568897648851, 0.07405724077823318263, 1.141732283410804349 ) ) ;
#31788 = DIRECTION ( 'NONE',  ( 0.000000000000000000, -0.6220299971367094782, 0.7829934116339072325 ) ) ;
#31789 = CARTESIAN_POINT ( 'NONE',  ( -0.9500414927467378812, -0.1787899950787401604, 1.156496062938362046 ) ) ;
#31790 = CARTESIAN_POINT ( 'NONE',  ( 1.033464566929134687, -0.06523048226347956391, 0.5093503935932609528 ) ) ;
#31791 = ORIENTED_EDGE ( 'NONE', *, *, #26986, .F. ) ;
#31792 = DIRECTION ( 'NONE',  ( 3.469446951953614978E-15, 1.000000000000000000, -3.995705278811693553E-31 ) ) ;
#31793 = CARTESIAN_POINT ( 'NONE',  ( -1.033464566929133799, 0.000000000000000000, 0.3149606298137326843 ) ) ;
#31794 = ORIENTED_EDGE ( 'NONE', *, *, #22614, .F. ) ;
#31795 = CARTESIAN_POINT ( 'NONE',  ( 0.9500414927467378812, -0.1787899950787401604, 1.235236220418678199 ) ) ;
#31796 = ADVANCED_FACE ( 'NONE', ( #20326 ), #34965, .F. ) ;
#31798 = CARTESIAN_POINT ( 'NONE',  ( 0.7185039370078739607, 1.928577636452523993E-17, 0.05905511800270921846 ) ) ;
#31797 = CARTESIAN_POINT ( 'NONE',  ( -0.2431102362204724532, 0.000000000000000000, 0.000000000000000000 ) ) ;
#31799 = CARTESIAN_POINT ( 'NONE',  ( 3.284318927891251994E-17, 0.04872047249470835839, 0.1787899950787401882 ) ) ;
#31800 = CARTESIAN_POINT ( 'NONE',  ( 0.7185039370078746268, 0.06523048226347956391, 0.7357283464566919395 ) ) ;
#31801 = ORIENTED_EDGE ( 'NONE', *, *, #27123, .F. ) ;
#31802 = AXIS2_PLACEMENT_3D ( 'NONE', #34453, #9288, #41360 ) ;
#31803 = LINE ( 'NONE', #13564, #33672 ) ;
#31804 = ORIENTED_EDGE ( 'NONE', *, *, #22561, .T. ) ;
#31805 = CARTESIAN_POINT ( 'NONE',  ( -0.6971942568897637749, 2.189545951927499583E-17, 1.380413385773007873 ) ) ;
#31806 = CARTESIAN_POINT ( 'NONE',  ( 0.1264236179284866091, -1.673720472387181024, -0.1264236179284866091 ) ) ;
#31807 = CARTESIAN_POINT ( 'NONE',  ( -1.002407869896990045, -0.1264236179284866091, 0.9670275590013542866 ) ) ;
#31808 = CARTESIAN_POINT ( 'NONE',  ( -0.9412147342319837628, -0.1574803149606297803, 0.04183070866141735261 ) ) ;
#31809 = VERTEX_POINT ( 'NONE', #13389 ) ;
#31810 = CARTESIAN_POINT ( 'NONE',  ( -0.6971942568897637749, 2.189545951927499583E-17, 0.6373031495525354195 ) ) ;
#31811 = CYLINDRICAL_SURFACE ( 'NONE', #46587, 0.1377952755905510751 ) ;
#31812 = ORIENTED_EDGE ( 'NONE', *, *, #16805, .T. ) ;
#31813 = CARTESIAN_POINT ( 'NONE',  ( -0.9412147342319837628, 0.1574803149606300301, 0.05659448818897643008 ) ) ;
#31814 = CARTESIAN_POINT ( 'NONE',  ( 0.000000000000000000, 1.205361022782826802E-17, -0.09842519685039370636 ) ) ;
#31815 = ORIENTED_EDGE ( 'NONE', *, *, #47080, .T. ) ;
#31816 = DIRECTION ( 'NONE',  ( 1.000000000000000000, -3.368395098984090098E-15, 0.000000000000000000 ) ) ;
#31817 = DIRECTION ( 'NONE',  ( -1.000000000000000000, 0.000000000000000000, 0.000000000000000000 ) ) ;
#31818 = CARTESIAN_POINT ( 'NONE',  ( -0.9500414927467378812, -0.1787899950787401604, 0.6053149605761579677 ) ) ;
#31819 = CARTESIAN_POINT ( 'NONE',  ( 2.892866454678787531E-17, -0.01771653543307086590, 0.1574803149606299191 ) ) ;
#31820 = EDGE_LOOP ( 'NONE', ( #13345, #11391, #32537, #36299, #26726 ) ) ;
#31821 = CARTESIAN_POINT ( 'NONE',  ( -0.7495606340400177148, -0.1264236179284866091, 1.665846456639149764 ) ) ;
#31822 = CARTESIAN_POINT ( 'NONE',  ( 1.033464566929133799, 1.928577636452524610E-17, 4.498031496062992574 ) ) ;
#31823 = LINE ( 'NONE', #28471, #37882 ) ;
#31824 = CARTESIAN_POINT ( 'NONE',  ( 0.1797182628040039365, -0.6900044395043051226, -2.200913952912460540E-17 ) ) ;
#31825 = CARTESIAN_POINT ( 'NONE',  ( 0.2471922904502826812, 0.09442133267706716293, 0.03395025085954773980 ) ) ;
#31826 = CARTESIAN_POINT ( 'NONE',  ( -0.7185039370078739607, 1.928577636452523993E-17, 1.397637795168062969 ) ) ;
#31827 = EDGE_CURVE ( 'NONE', #18734, #28693, #28018, .T. ) ;
#31828 = CARTESIAN_POINT ( 'NONE',  ( 0.6971942568897637749, 2.189545951927499583E-17, 0.6373031495525354195 ) ) ;
#31830 = DIRECTION ( 'NONE',  ( -3.478357113474434231E-15, -1.000000000000000000, 0.000000000000000000 ) ) ;
#31829 = CARTESIAN_POINT ( 'NONE',  ( 0.06523048226347956391, -0.6304133858267716439, -0.1574803149606300301 ) ) ;
#31831 = AXIS2_PLACEMENT_3D ( 'NONE', #2608, #46455, #3075 ) ;
#31832 = VECTOR ( 'NONE', #45151, 39.37007874015748143 ) ;
#31833 = CARTESIAN_POINT ( 'NONE',  ( 1.033464566929133799, 0.000000000000000000, 1.614173228238929170 ) ) ;
#31834 = VERTEX_POINT ( 'NONE', #23164 ) ;
#31835 = CARTESIAN_POINT ( 'NONE',  ( 0.7646288533564489232, 0.1113553986120547346, 1.589566929026330566 ) ) ;
#31836 = CARTESIAN_POINT ( 'NONE',  ( 1.033464566929133799, 0.000000000000000000, 1.309055118110236338 ) ) ;
#31838 = CARTESIAN_POINT ( 'NONE',  ( -0.9412147342319837628, -0.1574803149606297803, 1.341043307086613456 ) ) ;
#31837 = CARTESIAN_POINT ( 'NONE',  ( -0.7646288533564489232, 0.1113553986120547346, 1.274606299105070839 ) ) ;
#31839 = CARTESIAN_POINT ( 'NONE',  ( 0.8107537697050254399, -0.1574803149606297803, 1.966043307086614567 ) ) ;
#31840 = CARTESIAN_POINT ( 'NONE',  ( 0.1574803149606299191, -0.5885826770578268530, -1.928577636452523993E-17 ) ) ;
#31842 = EDGE_CURVE ( 'NONE', #4000, #36211, #41355, .T. ) ;
#31841 = EDGE_LOOP ( 'NONE', ( #6144, #32025, #16426, #15830, #39308, #4601, #45400 ) ) ;
#31844 = CARTESIAN_POINT ( 'NONE',  ( 0.6141732283464567121, 0.000000000000000000, 0.000000000000000000 ) ) ;
#31843 = CARTESIAN_POINT ( 'NONE',  ( 0.8019270111902716547, 0.1787899950787401604, 0.7431102361667091261 ) ) ;
#31845 = DIRECTION ( 'NONE',  ( 7.542275982507857147E-17, -0.6156614753256598460, -0.7880107536067206819 ) ) ;
#31846 = CARTESIAN_POINT ( 'NONE',  ( -0.1158283541424031532, -0.08956345598586890056, -0.1361971163587911426 ) ) ;
#31847 = VERTEX_POINT ( 'NONE', #1334 ) ;
#31848 = CARTESIAN_POINT ( 'NONE',  ( -0.9873396505805591694, -0.1113553986120547346, 1.067913385826771755 ) ) ;
#31849 = CARTESIAN_POINT ( 'NONE',  ( 0.7185039370078746268, -0.06523048226347956391, 1.724901574803149762 ) ) ;
#31850 = CARTESIAN_POINT ( 'NONE',  ( 0.005401850751909476230, 0.09279043093865825542, -0.1148724510413045297 ) ) ;
#31851 = CARTESIAN_POINT ( 'NONE',  ( 0.9500414927467378812, -0.1787899950787401604, 0.8021653542769460188 ) ) ;
#31852 = DIRECTION ( 'NONE',  ( -0.5735764363510518216, -0.8191520442889876907, 0.000000000000000000 ) ) ;
#31853 = CARTESIAN_POINT ( 'NONE',  ( 0.8759842519685039353, -0.1574803149606299191, 0.6988188975302678241 ) ) ;
#31854 = CARTESIAN_POINT ( 'NONE',  ( -0.1264236179284866091, -1.806594488135212728, 0.1264236179284866091 ) ) ;
#31855 = CARTESIAN_POINT ( 'NONE',  ( 0.1787899950787401604, -1.051181102308440529, 0.07405724077823318263 ) ) ;
#31856 = CARTESIAN_POINT ( 'NONE',  ( 0.1574803149606300301, -1.462106299212597493, -0.06523048226347956391 ) ) ;
#31857 = CARTESIAN_POINT ( 'NONE',  ( 0.1377952755905511861, -1.365923996832131609E-16, -0.8070866141732283561 ) ) ;
#31858 = EDGE_CURVE ( 'NONE', #36803, #27280, #15989, .T. ) ;
#31859 = PRODUCT_RELATED_PRODUCT_CATEGORY ( 'part', '', ( #19185 ) ) ;
#31860 = CARTESIAN_POINT ( 'NONE',  ( -0.6971942568897648851, -0.07405724077823297447, 1.899606299158834943 ) ) ;
#31861 = FACE_OUTER_BOUND ( 'NONE', #31595, .T. ) ;
#31862 = EDGE_LOOP ( 'NONE', ( #28023, #8438, #5272, #36797, #40058, #42862, #17995, #13002, #2006, #41052 ) ) ;
#31863 = CARTESIAN_POINT ( 'NONE',  ( -0.8759842519685039353, -0.1574803149606299191, 1.850393700787401619 ) ) ;
#31864 = CARTESIAN_POINT ( 'NONE',  ( -0.7495606340400177148, 0.1264236179284866091, 1.572342519631275692 ) ) ;
#31865 = DIRECTION ( 'NONE',  ( 0.000000000000000000, 1.000000000000000000, 0.000000000000000000 ) ) ;
#31866 = CARTESIAN_POINT ( 'NONE',  ( -1.002407869896990045, 0.1264236179284866091, 1.011318897584031484 ) ) ;
#31867 = CARTESIAN_POINT ( 'NONE',  ( -0.6971942568897626646, -0.07405724077823297447, 0.2066929133320631329 ) ) ;
#31868 = CARTESIAN_POINT ( 'NONE',  ( -0.1235961452251413406, 0.09842519685039370636, -0.2140748031496062798 ) ) ;
#31869 = CARTESIAN_POINT ( 'NONE',  ( -0.6971942568897648851, -0.07405724077823297447, 1.899606299158834943 ) ) ;
#31870 = CARTESIAN_POINT ( 'NONE',  ( 0.4736248074375574713, 1.975221432870720495, -0.9622519263226653186 ) ) ;
#31871 = CARTESIAN_POINT ( 'NONE',  ( -0.9873396505805591694, -0.1113553986120547346, 1.934055118110236338 ) ) ;
#31872 = CARTESIAN_POINT ( 'NONE',  ( 0.2559030184365650995, 0.02510022111087184885, -0.02997901531815388293 ) ) ;
#31873 = CARTESIAN_POINT ( 'NONE',  ( 0.1264236179284866091, -0.1984507398827823066, 0.1264236179284866091 ) ) ;
#31874 = CARTESIAN_POINT ( 'NONE',  ( 0.1267115641817155580, -0.09842519685039370636, 0.1767117842128110017 ) ) ;
#31875 = CARTESIAN_POINT ( 'NONE',  ( -0.7185039370078746268, -0.06523048226347956391, 1.488681102362205300 ) ) ;
#31876 = CARTESIAN_POINT ( 'NONE',  ( -0.7185039370078739607, 0.000000000000000000, -2.869337061179095023E-17 ) ) ;
#31877 = VECTOR ( 'NONE', #4469, 39.37007874015748143 ) ;
#31878 = CARTESIAN_POINT ( 'NONE',  ( -1.054774247047244096, 0.000000000000000000, 0.2189960629383626012 ) ) ;
#31879 = ( BOUNDED_CURVE ( )  B_SPLINE_CURVE ( 2, ( #24452, #13212, #41921, #46480, #20375, #35259, #28298, #10074, #2627 ),
 .UNSPECIFIED., .F., .F. ) 
 B_SPLINE_CURVE_WITH_KNOTS ( ( 3, 2, 2, 2, 3 ),
 ( 0.5300000000000000266, 0.5324999999999999734, 0.5350000000000000311, 0.5374999999999999778, 0.5400000000000000355 ),
 .UNSPECIFIED. ) 
 CURVE ( )  GEOMETRIC_REPRESENTATION_ITEM ( )  RATIONAL_B_SPLINE_CURVE ( ( 1.000000000000000000, 0.9238795325112869605, 1.000000000000000000, 0.9238795325112869605, 1.000000000000000000, 0.9238795325112869605, 1.000000000000000000, 0.9238795325112869605, 1.000000000000000000 ) ) 
 REPRESENTATION_ITEM ( '' )  ) ;
#31880 = ADVANCED_BREP_SHAPE_REPRESENTATION ( 'Side Bracket', ( #37046, #20860 ), #46110 ) ;
#31881 = ORIENTED_EDGE ( 'NONE', *, *, #32823, .F. ) ;
#31882 = CARTESIAN_POINT ( 'NONE',  ( -0.9500414927467377701, 0.1787899950787401604, 1.254921259788757348 ) ) ;
#31883 = ORIENTED_EDGE ( 'NONE', *, *, #1809, .T. ) ;
#31884 = EDGE_CURVE ( 'NONE', #2356, #5354, #9012, .T. ) ;
#31885 = CARTESIAN_POINT ( 'NONE',  ( -0.1264236179284866091, -1.191437007820251859, -0.1264236179284866091 ) ) ;
#31886 = CARTESIAN_POINT ( 'NONE',  ( -0.07405724077823318263, -1.292322834591905778, 0.1787899950787401604 ) ) ;
#31887 = CARTESIAN_POINT ( 'NONE',  ( -0.1270800023317771588, -0.5571304237562740846, -0.1270800023317771588 ) ) ;
#31888 = CARTESIAN_POINT ( 'NONE',  ( 0.000000000000000000, 0.000000000000000000, 0.09842519685039370636 ) ) ;
#31889 = CARTESIAN_POINT ( 'NONE',  ( -1.033464566929133799, 0.000000000000000000, 0.7972440944881890035 ) ) ;
#31890 = EDGE_CURVE ( 'NONE', #8749, #7162, #13859, .T. ) ;
#31891 = CARTESIAN_POINT ( 'NONE',  ( 0.1113553986120547346, -0.1309055118110236116, 0.1113553986120547346 ) ) ;
#31892 = CARTESIAN_POINT ( 'NONE',  ( 0.8759842519685039353, 0.1574803149606299191, 1.820866141624755796 ) ) ;
#31893 = CARTESIAN_POINT ( 'NONE',  ( 0.7646288533564489232, 0.1113553986120547346, 0.8513779527559054427 ) ) ;
#31894 = CARTESIAN_POINT ( 'NONE',  ( 0.05734381846710276398, -0.2623867632340661782, -0.05455490385610432119 ) ) ;
#31895 = CYLINDRICAL_SURFACE ( 'NONE', #35562, 0.6872114956789353579 ) ;
#31896 = ( BOUNDED_CURVE ( )  B_SPLINE_CURVE ( 2, ( #18715, #8638, #37397, #16098, #37891, #4313, #491, #37646, #11791 ),
 .UNSPECIFIED., .F., .T. ) 
 B_SPLINE_CURVE_WITH_KNOTS ( ( 3, 2, 2, 2, 3 ),
 ( 0.4299999999999999933, 0.4324999999999999956, 0.4349999999999999978, 0.4375000000000000000, 0.4400000000000000022 ),
 .UNSPECIFIED. ) 
 CURVE ( )  GEOMETRIC_REPRESENTATION_ITEM ( )  RATIONAL_B_SPLINE_CURVE ( ( 1.000000000000000000, 0.9238795325112869605, 1.000000000000000000, 0.9238795325112869605, 1.000000000000000000, 0.9238795325112869605, 1.000000000000000000, 0.9238795325112869605, 1.000000000000000000 ) ) 
 REPRESENTATION_ITEM ( '' )  ) ;
#31898 = CARTESIAN_POINT ( 'NONE',  ( 0.7185039370078746268, 0.06523048226347956391, 1.523129921259841923 ) ) ;
#31897 = CARTESIAN_POINT ( 'NONE',  ( 0.1623289600446794489, 0.2017735634833385805, -0.03395687952545685395 ) ) ;
#31899 = CARTESIAN_POINT ( 'NONE',  ( 0.7185039370078746268, -0.06523048226347956391, 0.2189960628845991353 ) ) ;
#31900 = ORIENTED_EDGE ( 'NONE', *, *, #47297, .F. ) ;
#31901 = ORIENTED_EDGE ( 'NONE', *, *, #1954, .T. ) ;
#31902 = CARTESIAN_POINT ( 'NONE',  ( -1.033464566929133799, 0.000000000000000000, 1.190944881889763884 ) ) ;
#31903 = CARTESIAN_POINT ( 'NONE',  ( 0.07405724077823318263, -0.6082677164816695514, -0.1787899950787401604 ) ) ;
#31904 = CARTESIAN_POINT ( 'NONE',  ( -0.1787899950787401604, -1.415354330654897019, 0.07405724077823318263 ) ) ;
#31905 = CARTESIAN_POINT ( 'NONE',  ( -0.9500414927467378812, -0.1787899950787401604, 1.904527559001354398 ) ) ;
#31906 = VERTEX_POINT ( 'NONE', #19323 ) ;
#31907 = CARTESIAN_POINT ( 'NONE',  ( -1.002407869896990045, 0.1264236179284866091, 1.449311023568283341 ) ) ;
#31908 = CARTESIAN_POINT ( 'NONE',  ( 0.6971942568897637749, 2.189545951927499583E-17, 1.542814960576157413 ) ) ;
#31909 = EDGE_LOOP ( 'NONE', ( #28319, #44766, #25175, #14308 ) ) ;
#31910 = CARTESIAN_POINT ( 'NONE',  ( -0.8759842519685039353, -0.1574803149606299191, 0.9055118110236221041 ) ) ;
#31911 = CARTESIAN_POINT ( 'NONE',  ( -1.054774247047244540, -0.07405724077823318263, 0.6545275590013545086 ) ) ;
#31912 = CARTESIAN_POINT ( 'NONE',  ( 1.054774247047244540, 0.07405724077823318263, 0.1870078739619845387 ) ) ;
#31913 = CARTESIAN_POINT ( 'NONE',  ( -1.033464566929133799, 1.928577636452524610E-17, 2.869337061179095023E-17 ) ) ;
#31914 = ( NAMED_UNIT ( * ) SI_UNIT ( $, .STERADIAN. ) SOLID_ANGLE_UNIT ( ) ) ;
#31915 = CARTESIAN_POINT ( 'NONE',  ( 0.7495606340400177148, 0.1264236179284866091, 0.7504921259304880854 ) ) ;
#31916 = CARTESIAN_POINT ( 'NONE',  ( -0.6971942568897648851, 0.07405724077823318263, 0.5905511810485987167 ) ) ;
#31917 = DIRECTION ( 'NONE',  ( 0.000000000000000000, 0.000000000000000000, -1.000000000000000000 ) ) ;
#31918 = CARTESIAN_POINT ( 'NONE',  ( 0.7646288533564489232, -0.1113553986120547346, 1.136811023622047223 ) ) ;
#31919 = ORIENTED_EDGE ( 'NONE', *, *, #2899, .T. ) ;
#31920 = CARTESIAN_POINT ( 'NONE',  ( -1.033464566929133799, 1.928577636452524610E-17, 2.869337061179095023E-17 ) ) ;
#31921 = CARTESIAN_POINT ( 'NONE',  ( -0.8107537697050253289, -0.1574803149606297803, 0.5093503937007877180 ) ) ;
#31922 = CARTESIAN_POINT ( 'NONE',  ( 0.7495606340400177148, 0.1264236179284866091, 1.301673228292692830 ) ) ;
#31923 = CARTESIAN_POINT ( 'NONE',  ( 0.08749754606363346898, -0.09851384719155904801, 0.2018685754223755735 ) ) ;
#31924 = ORIENTED_EDGE ( 'NONE', *, *, #20244, .F. ) ;
#31925 = CARTESIAN_POINT ( 'NONE',  ( 0.000000000000000000, 0.000000000000000000, 0.000000000000000000 ) ) ;
#31926 = ORIENTED_EDGE ( 'NONE', *, *, #6259, .F. ) ;
#31927 = CARTESIAN_POINT ( 'NONE',  ( -0.07405724077823318263, -0.5984251967966303098, -0.1787899950787401604 ) ) ;
#31928 = DIRECTION ( 'NONE',  ( 1.000000000000000000, 0.000000000000000000, -0.000000000000000000 ) ) ;
#31929 = VERTEX_POINT ( 'NONE', #14614 ) ;
#31930 = CARTESIAN_POINT ( 'NONE',  ( 1.054774247047244540, -0.07405724077823318263, 1.437007873961985371 ) ) ;
#31931 = EDGE_CURVE ( 'NONE', #23841, #19150, #27259, .T. ) ;
#31932 = CARTESIAN_POINT ( 'NONE',  ( 1.033464566929133799, 1.928577636452524610E-17, 4.498031496062992574 ) ) ;
#31933 = ADVANCED_FACE ( 'NONE', ( #1571, #33972 ), #23634, .T. ) ;
#31934 = DIRECTION ( 'NONE',  ( -1.144917494144692682E-16, 3.972230510298674823E-31, -1.000000000000000000 ) ) ;
#31935 = CARTESIAN_POINT ( 'NONE',  ( 0.6195511811023624027, 0.9842519685039370358, -0.7135826771653542844 ) ) ;
#31936 = CARTESIAN_POINT ( 'NONE',  ( 1.054774247047244540, -0.07405724077823318263, 0.3740157479777325711 ) ) ;
#31937 = EDGE_CURVE ( 'NONE', #43630, #14529, #33427, .T. ) ;
#31938 = CARTESIAN_POINT ( 'NONE',  ( -1.094772975963752103E-17, 0.01316343334556440911, -0.1787899950787401882 ) ) ;
#31939 = CONTEXT_DEPENDENT_SHAPE_REPRESENTATION ( #33396, #6508 ) ;
#31940 = CYLINDRICAL_SURFACE ( 'NONE', #22658, 0.1574803149606299191 ) ;
#31941 = CARTESIAN_POINT ( 'NONE',  ( 0.000000000000000000, -0.1193342091828949042, 0.06889763779527559306 ) ) ;
#31942 = EDGE_CURVE ( 'NONE', #29301, #28190, #5173, .T. ) ;
#31943 = CARTESIAN_POINT ( 'NONE',  ( 0.6971942568897637749, 2.189545951927499583E-17, 0.6323818897100157432 ) ) ;
#31944 = CIRCLE ( 'NONE', #5141, 0.09842519685039310962 ) ;
#31945 = CARTESIAN_POINT ( 'NONE',  ( -0.8019270111902716547, -0.1787899950787401604, 0.8415354330171020969 ) ) ;
#31947 = DIRECTION ( 'NONE',  ( 0.000000000000000000, 1.000000000000000000, 8.673617379884034486E-16 ) ) ;
#31946 = CARTESIAN_POINT ( 'NONE',  ( 0.1574803149606300301, -0.8371062992125989366, 0.06523048226347956391 ) ) ;
#31949 = CARTESIAN_POINT ( 'NONE',  ( -0.8361142526885965154, -0.1686726915505806779, 1.987473384380551877 ) ) ;
#31948 = CARTESIAN_POINT ( 'NONE',  ( -0.07444174185955065859, -1.686559557614542459, 0.1797182628040039087 ) ) ;
#31950 = CARTESIAN_POINT ( 'NONE',  ( 0.1574803149606300301, -0.5073818896562523051, -0.06523048226347956391 ) ) ;
#31951 = CARTESIAN_POINT ( 'NONE',  ( -0.1787899950787401882, -0.3941929133320630219, 0.000000000000000000 ) ) ;
#31952 = CARTESIAN_POINT ( 'NONE',  ( 0.8759842519685039353, -0.1787899950787401882, 1.749507873961984483 ) ) ;
#31954 = CARTESIAN_POINT ( 'NONE',  ( -0.1476377952755905387, -0.4933358210236689634, -0.8766136318131756422 ) ) ;
#31953 = CARTESIAN_POINT ( 'NONE',  ( 1.054774247047244540, 0.07405724077823318263, 1.953740157426552715 ) ) ;
#31955 = CARTESIAN_POINT ( 'NONE',  ( 0.9500414927467377701, -0.1787899950787401604, 0.4478346456155276045 ) ) ;
#31956 = VERTEX_POINT ( 'NONE', #11916 ) ;
#31957 = CARTESIAN_POINT ( 'NONE',  ( -0.1916485431826253083, -0.07731288306168948576, -0.1747847109491778572 ) ) ;
#31958 = CARTESIAN_POINT ( 'NONE',  ( 0.1495543973312418728, -0.2091518620004978180, -0.3144333452974441556 ) ) ;
#31959 = CARTESIAN_POINT ( 'NONE',  ( 0.1787899950787401882, -0.1038385826234017734, -2.189545951927503898E-17 ) ) ;
#31960 = CARTESIAN_POINT ( 'NONE',  ( 0.1787899950787401604, -0.9232283464029299447, -0.07405724077823318263 ) ) ;
#31961 = CARTESIAN_POINT ( 'NONE',  ( 0.8019270111902717657, 0.1787899950787401604, 0.03937007868639399305 ) ) ;
#31962 = CARTESIAN_POINT ( 'NONE',  ( -0.7646288533564489232, -0.1113553986120547346, 1.520669291231054876 ) ) ;
#31963 = CYLINDRICAL_SURFACE ( 'NONE', #19677, 0.4724409448818896462 ) ;
#31964 = CARTESIAN_POINT ( 'NONE',  ( -0.6971942568897648851, -0.07405724077823297447, 1.461614173174583753 ) ) ;
#31965 = VERTEX_POINT ( 'NONE', #18434 ) ;
#31966 = CARTESIAN_POINT ( 'NONE',  ( -0.2624241468390501320, -0.1651049555683126169, -0.8482729357033111928 ) ) ;
#31967 = CARTESIAN_POINT ( 'NONE',  ( 1.002407869896990045, 0.1264236179284866091, 1.213090551127338435 ) ) ;
#31968 = CARTESIAN_POINT ( 'NONE',  ( -1.033464566929134687, -0.06523048226347956391, 0.7062007872940467834 ) ) ;
#31969 = CARTESIAN_POINT ( 'NONE',  ( -0.1377952755905509641, 1.687505431895957030E-17, -0.2219368594840610276 ) ) ;
#31970 = CARTESIAN_POINT ( 'NONE',  ( 0.7495606340400177148, 0.1264236179284866091, 1.769192913332062966 ) ) ;
#31971 = CARTESIAN_POINT ( 'NONE',  ( -0.8107537697050253289, -0.1574803149606297803, 1.336122047244094446 ) ) ;
#31972 = CARTESIAN_POINT ( 'NONE',  ( -1.002407869896990045, -0.1264236179284866091, 0.9227362204186770889 ) ) ;
#31973 = DIRECTION ( 'NONE',  ( -1.000000000000000000, -0.000000000000000000, 0.000000000000000000 ) ) ;
#31974 = CARTESIAN_POINT ( 'NONE',  ( 0.000000000000000000, 0.1102362204724409434, 0.000000000000000000 ) ) ;
#31975 = CARTESIAN_POINT ( 'NONE',  ( 0.8019270111902716547, -0.1787899950787401604, 0.1328740156942679884 ) ) ;
#31976 = CARTESIAN_POINT ( 'NONE',  ( 1.033464566929134687, 0.06523048226347956391, 1.616633858160190229 ) ) ;
#31977 = CARTESIAN_POINT ( 'NONE',  ( 0.07405724077823318263, 0.1250000000537635492, 0.1787899950787401604 ) ) ;
#31978 = CARTESIAN_POINT ( 'NONE',  ( 0.7185039370078739607, 1.928577636452523993E-17, 1.791338582569637738 ) ) ;
#31979 = CARTESIAN_POINT ( 'NONE',  ( 0.8759842519685039353, -0.1787899950787401882, 0.7258858267178898149 ) ) ;
#31980 = CARTESIAN_POINT ( 'NONE',  ( -0.8759842519685039353, -0.1787899950787401882, 1.705216535379307174 ) ) ;
#31981 = AXIS2_PLACEMENT_3D ( 'NONE', #40353, #11168, #44196 ) ;
#31982 = DIRECTION ( 'NONE',  ( 1.000000000000000000, 0.000000000000000000, -4.710082747697005495E-15 ) ) ;
#31983 = CYLINDRICAL_SURFACE ( 'NONE', #24170, 0.1968503937007874405 ) ;
#31984 = CARTESIAN_POINT ( 'NONE',  ( 0.000000000000000000, -0.09842519685039370636, 0.2471922904502826812 ) ) ;
#31985 = CARTESIAN_POINT ( 'NONE',  ( 3.284318927891251994E-17, -1.069513732008765761, 0.1787899950787401882 ) ) ;
#31986 = EDGE_LOOP ( 'NONE', ( #37514, #19519, #25491, #44542 ) ) ;
#31987 = CARTESIAN_POINT ( 'NONE',  ( 0.1264236179284866091, -0.06446850388324429360, 0.1264236179284866091 ) ) ;
#31988 = VERTEX_POINT ( 'NONE', #32850 ) ;
#31989 = CARTESIAN_POINT ( 'NONE',  ( 1.002407869896990045, 0.1264236179284866091, 1.050688976324189117 ) ) ;
#31990 = DIRECTION ( 'NONE',  ( 0.000000000000000000, 0.000000000000000000, 1.000000000000000000 ) ) ;
#31991 = CARTESIAN_POINT ( 'NONE',  ( -0.7185039370078746268, -0.06523048226347956391, 1.449311023622047445 ) ) ;
#31992 = EDGE_CURVE ( 'NONE', #36366, #1004, #45418, .T. ) ;
#31993 = CARTESIAN_POINT ( 'NONE',  ( 0.9412147342319837628, 0.1574803149606300301, 1.906988188976377563 ) ) ;
#31994 = CARTESIAN_POINT ( 'NONE',  ( 0.07405724077823318263, -1.474409448765133801, -0.1787899950787401604 ) ) ;
#31995 = EDGE_CURVE ( 'NONE', #46176, #4886, #36052, .T. ) ;
#31996 = CARTESIAN_POINT ( 'NONE',  ( -0.7495606340400177148, -0.1264236179284866091, 0.2878937007336381804 ) ) ;
#31997 = LINE ( 'NONE', #20950, #7999 ) ;
#31998 = CARTESIAN_POINT ( 'NONE',  ( 0.8759842519685039353, 0.1787899950787401882, 1.178641732229700922 ) ) ;
#31999 = CARTESIAN_POINT ( 'NONE',  ( 0.9500414927467377701, 0.1787899950787401604, 1.564960629867495845 ) ) ;
#32000 = CARTESIAN_POINT ( 'NONE',  ( 0.7495606340400177148, 0.1264236179284866091, 0.1550196849856066983 ) ) ;
#32002 = CARTESIAN_POINT ( 'NONE',  ( -0.1574803149606299191, 1.928577636452524610E-17, -0.3139606299212599483 ) ) ;
#32001 = CARTESIAN_POINT ( 'NONE',  ( 0.7185039370078746268, -0.06523048226347956391, 0.8882874014672752505 ) ) ;
#32003 = DIRECTION ( 'NONE',  ( 0.000000000000000000, -1.000000000000000000, 0.000000000000000000 ) ) ;
#32004 = CARTESIAN_POINT ( 'NONE',  ( 0.1113553986120547346, -0.7903543306011338032, 0.1113553986120547346 ) ) ;
#32005 = CARTESIAN_POINT ( 'NONE',  ( -0.8107537697050253289, 0.1574803149606300301, 1.705216535325545069 ) ) ;
#32006 = VECTOR ( 'NONE', #2015, 39.37007874015748143 ) ;
#32007 = CARTESIAN_POINT ( 'NONE',  ( 0.1787899950787401604, 0.01673228351833044164, 0.07405724077823318263 ) ) ;
#32008 = CARTESIAN_POINT ( 'NONE',  ( 0.7495606340400177148, 0.1264236179284866091, 0.1156496062454492185 ) ) ;
#32009 = DIRECTION ( 'NONE',  ( 0.000000000000000000, 0.7880107536067200158, -0.6156614753256608452 ) ) ;
#32011 = PLANE ( 'NONE',  #29277 ) ;
#32010 = CARTESIAN_POINT ( 'NONE',  ( 0.6971942568897637749, 2.189545951927499583E-17, 1.065452755851747924 ) ) ;
#32012 = LINE ( 'NONE', #46604, #4365 ) ;
#32013 = CARTESIAN_POINT ( 'NONE',  ( 0.7646288533564489232, -0.1113553986120547346, 0.5364173227271189504 ) ) ;
#32014 = VERTEX_POINT ( 'NONE', #209 ) ;
#32015 = CARTESIAN_POINT ( 'NONE',  ( -1.033464566929133799, 0.000000000000000000, 0.4724409447743622148 ) ) ;
#32016 = CARTESIAN_POINT ( 'NONE',  ( 1.023384524333779799, 0.06767030011490859920, 0.03937429509552410611 ) ) ;
#32017 = CARTESIAN_POINT ( 'NONE',  ( -0.8107537697050253289, 0.1574803149606300301, 0.3666338581601894520 ) ) ;
#32018 = ORIENTED_EDGE ( 'NONE', *, *, #24367, .T. ) ;
#32019 = CARTESIAN_POINT ( 'NONE',  ( 0.9500414927467378812, -0.1787899950787401604, 1.471456692859622217 ) ) ;
#32021 = CARTESIAN_POINT ( 'NONE',  ( -0.8759842519685039353, -0.1574803149606299191, 0.2263779526483783444 ) ) ;
#32020 = DIRECTION ( 'NONE',  ( 0.000000000000000000, 0.000000000000000000, -1.000000000000000000 ) ) ;
#32022 = DIMENSIONAL_EXPONENTS ( 1.000000000000000000, 0.000000000000000000, 0.000000000000000000, 0.000000000000000000, 0.000000000000000000, 0.000000000000000000, 0.000000000000000000 ) ;
#32023 = CARTESIAN_POINT ( 'NONE',  ( 3.284318927891251994E-17, 0.009350393754550925460, 0.1787899950787401882 ) ) ;
#32025 = ORIENTED_EDGE ( 'NONE', *, *, #30584, .T. ) ;
#32024 = EDGE_CURVE ( 'NONE', #28708, #24192, #26773, .T. ) ;
#32026 = CARTESIAN_POINT ( 'NONE',  ( 0.000000000000000000, 0.3740157480314960647, 0.9783464566929134243 ) ) ;
#32027 = ORIENTED_EDGE ( 'NONE', *, *, #2578, .F. ) ;
#32028 = CARTESIAN_POINT ( 'NONE',  ( 0.1588215770322271292, 0.09266989036297287874, 0.1937373906134645662 ) ) ;
#32029 = CARTESIAN_POINT ( 'NONE',  ( 0.8759842519685039353, -0.1787899950787401882, 0.4502952755367874427 ) ) ;
#32030 = ORIENTED_EDGE ( 'NONE', *, *, #1873, .T. ) ;
#32031 = CARTESIAN_POINT ( 'NONE',  ( -1.002407869896990045, 0.1264236179284866091, 1.365649606245448844 ) ) ;
#32033 = CARTESIAN_POINT ( 'NONE',  ( 0.1264236179284866091, -1.683562992072220599, 0.1264236179284866091 ) ) ;
#32032 = CARTESIAN_POINT ( 'NONE',  ( 0.1574803149606299191, -0.3917322833570398011, -1.928577636452523993E-17 ) ) ;
#32034 = CARTESIAN_POINT ( 'NONE',  ( -0.8759842519685039353, -0.1787899950787401882, 0.9621062991588346103 ) ) ;
#32035 = CARTESIAN_POINT ( 'NONE',  ( -0.9500414927467378812, 0.1787899950787401604, 1.958661417269071947 ) ) ;
#32036 = CARTESIAN_POINT ( 'NONE',  ( -0.8019270111902716547, 0.1787899950787401604, 1.097440944828127041 ) ) ;
#32037 = CARTESIAN_POINT ( 'NONE',  ( -0.9500414927467378812, 0.1787899950787401604, 0.7037401574265510495 ) ) ;
#32038 = AXIS2_PLACEMENT_3D ( 'NONE', #41096, #4690, #19788 ) ;
#32039 = FACE_OUTER_BOUND ( 'NONE', #19136, .T. ) ;
#32040 = CARTESIAN_POINT ( 'NONE',  ( -0.1787899950787401604, -0.7225649131111276935, 0.07405724077823318263 ) ) ;
#32041 = ORIENTED_EDGE ( 'NONE', *, *, #35453, .F. ) ;
#32042 = CARTESIAN_POINT ( 'NONE',  ( -0.1113553986120547346, -0.02263779516806350284, -0.1113553986120547346 ) ) ;
#32043 = DIRECTION ( 'NONE',  ( -1.000000000000000000, 0.000000000000000000, 0.000000000000000000 ) ) ;
#32044 = ORIENTED_EDGE ( 'NONE', *, *, #29107, .T. ) ;
#32045 = CARTESIAN_POINT ( 'NONE',  ( -0.8107537697050254399, -0.1574803149606297803, 1.729822834645670548 ) ) ;
#32046 = CYLINDRICAL_SURFACE ( 'NONE', #17275, 0.1574803149606299191 ) ;
#32047 = VECTOR ( 'NONE', #31401, 39.37007874015748143 ) ;
#32048 = CARTESIAN_POINT ( 'NONE',  ( -0.8019270111902717657, -0.1787899950787401604, 0.6791338582139527791 ) ) ;
#32049 = CARTESIAN_POINT ( 'NONE',  ( -9.642888182262618425E-18, 0.08070866141732284393, -0.1574803149606299191 ) ) ;
#32050 = ADVANCED_FACE ( 'NONE', ( #41333 ), #22033, .T. ) ;
#32051 = ORIENTED_EDGE ( 'NONE', *, *, #966, .F. ) ;
#32052 = DIRECTION ( 'NONE',  ( 0.000000000000000000, 0.000000000000000000, 1.000000000000000000 ) ) ;
#32053 = CARTESIAN_POINT ( 'NONE',  ( -0.6971942568897648851, -0.07405724077823297447, 1.624015747977732849 ) ) ;
#32054 = DIRECTION ( 'NONE',  ( 1.000000000000000000, 0.000000000000000000, 0.000000000000000000 ) ) ;
#32055 = CARTESIAN_POINT ( 'NONE',  ( 0.7185039370078739607, 1.928577636452523993E-17, 1.043307086506645831 ) ) ;
#32056 = ORIENTED_EDGE ( 'NONE', *, *, #18271, .T. ) ;
#32057 = CARTESIAN_POINT ( 'NONE',  ( 0.1797182628040039365, -0.8081146757247775758, -2.200913952912460540E-17 ) ) ;
#32058 = CARTESIAN_POINT ( 'NONE',  ( 0.2471922904502827090, 0.08082342248660308315, 0.07163232281567669113 ) ) ;
#32059 = CARTESIAN_POINT ( 'NONE',  ( -0.7185039370078746268, -0.06523048226347956391, 1.360728346349165285 ) ) ;
#32060 = CARTESIAN_POINT ( 'NONE',  ( 0.8019270111902717657, -0.1787899950787401604, 0.6840551180564720113 ) ) ;
#32061 = CARTESIAN_POINT ( 'NONE',  ( 0.1574803149606299191, -0.5196850393700787052, -1.928577636452523993E-17 ) ) ;
#32062 = CARTESIAN_POINT ( 'NONE',  ( 0.8759842519685039353, 0.000000000000000000, 4.498031496062992574 ) ) ;
#32063 = ORIENTED_EDGE ( 'NONE', *, *, #39799, .T. ) ;
#32064 = CARTESIAN_POINT ( 'NONE',  ( -0.2559055118110235560, 0.07633542835890737288, -0.05125767443128528833 ) ) ;
#32065 = CARTESIAN_POINT ( 'NONE',  ( 0.8759842519685039353, -0.1574803149606299191, 1.299212598425196985 ) ) ;
#32066 = CARTESIAN_POINT ( 'NONE',  ( 0.000000000000000000, 0.000000000000000000, 0.000000000000000000 ) ) ;
#32067 = CYLINDRICAL_SURFACE ( 'NONE', #7515, 0.02900000000000001882 ) ;
#32069 = LINE ( 'NONE', #7130, #15418 ) ;
#32068 = CARTESIAN_POINT ( 'NONE',  ( 0.8759842519685039353, 0.1787899950787401882, 0.6225393700249762796 ) ) ;
#32070 = AXIS2_PLACEMENT_3D ( 'NONE', #8291, #45646, #27257 ) ;
#32071 = CARTESIAN_POINT ( 'NONE',  ( 0.07405724077823318263, -0.6427165353793066194, -0.1787899950787401604 ) ) ;
#32072 = CARTESIAN_POINT ( 'NONE',  ( 0.7185039370078739607, 1.928577636452523993E-17, 1.673228346349165285 ) ) ;
#32073 = ORIENTED_EDGE ( 'NONE', *, *, #18705, .T. ) ;
#32074 = DIRECTION ( 'NONE',  ( 0.000000000000000000, 0.000000000000000000, -1.000000000000000000 ) ) ;
#32075 = DIRECTION ( 'NONE',  ( 0.000000000000000000, 1.000000000000000000, 0.000000000000000000 ) ) ;
#32076 = CARTESIAN_POINT ( 'NONE',  ( 0.8019270111902717657, -0.1787899950787401604, 0.8759842519147408302 ) ) ;
#32077 = CARTESIAN_POINT ( 'NONE',  ( -0.1476377952755905387, -0.4812165006432425063, -0.8611016091043822707 ) ) ;
#32078 = DIRECTION ( 'NONE',  ( -1.000000000000000000, 0.000000000000000000, 0.000000000000000000 ) ) ;
#32079 = CARTESIAN_POINT ( 'NONE',  ( -0.1797182628040039087, 0.08017272585002534202, 0.07444174185955065859 ) ) ;
#32080 = CARTESIAN_POINT ( 'NONE',  ( 0.1787899950787401604, -1.006889763725763220, -0.07405724077823318263 ) ) ;
#32082 = VECTOR ( 'NONE', #16939, 39.37007874015748854 ) ;
#32081 = CARTESIAN_POINT ( 'NONE',  ( -0.1113553986120547346, -1.558070866141732180, 0.1113553986120547346 ) ) ;
#32083 = CARTESIAN_POINT ( 'NONE',  ( 0.2944196465027555387, 4.766607801171850497E-17, 0.000000000000000000 ) ) ;
#32084 = CARTESIAN_POINT ( 'NONE',  ( -0.8759842519685039353, 0.1787899950787401882, 0.03198818892261445085 ) ) ;
#32085 = EDGE_LOOP ( 'NONE', ( #32030, #3854, #21037, #30634, #23638, #22755, #44775, #8193 ) ) ;
#32086 = VECTOR ( 'NONE', #45424, 39.37007874015748143 ) ;
#32087 = DIRECTION ( 'NONE',  ( 1.000000000000000000, 0.000000000000000000, 0.000000000000000000 ) ) ;
#32088 = ORIENTED_EDGE ( 'NONE', *, *, #15366, .T. ) ;
#32089 = CARTESIAN_POINT ( 'NONE',  ( -0.6971942568897648851, -0.07405724077823297447, 1.978346456639149098 ) ) ;
#32090 = CARTESIAN_POINT ( 'NONE',  ( -0.6971942568897648851, -0.07405724077823297447, 1.067913385773007651 ) ) ;
#32091 = CARTESIAN_POINT ( 'NONE',  ( -1.054774247047244540, -0.07405724077823318263, 0.2608267715997796832 ) ) ;
#32092 = CARTESIAN_POINT ( 'NONE',  ( -0.1465299180647509913, 0.09658349877441911591, -0.2008339832271239522 ) ) ;
#32093 = CARTESIAN_POINT ( 'NONE',  ( -0.8759842519685039353, 0.1787899950787401882, 1.966043307032850462 ) ) ;
#32094 = CARTESIAN_POINT ( 'NONE',  ( 0.1120715992852186343, -0.09842519685039369248, -0.2207285028503088720 ) ) ;
#32095 = CARTESIAN_POINT ( 'NONE',  ( -0.8107537697050253289, -0.1574803149606297803, 1.926673228346456490 ) ) ;
#32096 = DIRECTION ( 'NONE',  ( -1.000000000000000000, 0.000000000000000000, 0.000000000000000000 ) ) ;
#32097 = EDGE_CURVE ( 'NONE', #42397, #30513, #31455, .T. ) ;
#32098 = CARTESIAN_POINT ( 'NONE',  ( -0.1730231402413970609, -0.09842519685039370636, 0.004655736871993992367 ) ) ;
#32099 = CARTESIAN_POINT ( 'NONE',  ( -1.033464566929133799, 1.928577636452524610E-17, 2.869337061179095023E-17 ) ) ;
#32100 = CARTESIAN_POINT ( 'NONE',  ( 2.892866454678787531E-17, -0.09645669291338582196, 0.1574803149606299191 ) ) ;
#32101 = CARTESIAN_POINT ( 'NONE',  ( -0.9500414927467378812, -0.1787899950787401604, 0.1722440944344254266 ) ) ;
#32102 = EDGE_CURVE ( 'NONE', #42555, #35982, #23604, .T. ) ;
#32103 = CONICAL_SURFACE ( 'NONE', #4481, 0.09842519685039310962, 0.7853981633972314524 ) ;
#32104 = ORIENTED_EDGE ( 'NONE', *, *, #35122, .F. ) ;
#32105 = ORIENTED_EDGE ( 'NONE', *, *, #1798, .F. ) ;
#32106 = EDGE_CURVE ( 'NONE', #18241, #17345, #43455, .T. ) ;
#32107 = CARTESIAN_POINT ( 'NONE',  ( 0.07405724077823318263, -1.252952755851747924, 0.1787899950787401604 ) ) ;
#32108 = VECTOR ( 'NONE', #37510, 39.37007874015748143 ) ;
#32109 = CARTESIAN_POINT ( 'NONE',  ( 0.1264236179284866091, -1.324311023568283341, 0.1264236179284866091 ) ) ;
#32110 = ADVANCED_FACE ( 'NONE', ( #5405, #38245, #20027 ), #35372, .F. ) ;
#32111 = DIRECTION ( 'NONE',  ( 0.000000000000000000, 0.000000000000000000, 1.000000000000000000 ) ) ;
#32112 = CARTESIAN_POINT ( 'NONE',  ( -0.1797182628040039087, -0.5940398725751709907, -0.07444174185955065859 ) ) ;
#32113 = DIRECTION ( 'NONE',  ( 1.000000000000000000, 0.000000000000000000, 0.000000000000000000 ) ) ;
#32114 = CARTESIAN_POINT ( 'NONE',  ( -0.7185039370078746268, -0.06523048226347956391, 0.7406496062992133922 ) ) ;
#32115 = CARTESIAN_POINT ( 'NONE',  ( 0.06523048226347956391, -0.1973425196850395746, -0.1574803149606300301 ) ) ;
#32116 = CARTESIAN_POINT ( 'NONE',  ( 0.8759842519685039353, -0.1574803149606299191, 1.801181102254677091 ) ) ;
#32117 = ORIENTED_EDGE ( 'NONE', *, *, #41719, .T. ) ;
#32118 = CARTESIAN_POINT ( 'NONE',  ( -0.8759842519685039353, 0.1574803149606299191, 1.427165354223181248 ) ) ;
#32119 = CARTESIAN_POINT ( 'NONE',  ( 1.033464566929133799, 0.000000000000000000, 0.7972440944881890035 ) ) ;
#32120 = DIRECTION ( 'NONE',  ( -3.469446951953613794E-15, -1.000000000000000000, 0.000000000000000000 ) ) ;
#32122 = DIRECTION ( 'NONE',  ( -0.000000000000000000, 1.000000000000000000, 0.000000000000000000 ) ) ;
#32121 = CARTESIAN_POINT ( 'NONE',  ( -1.033464566929133799, 0.000000000000000000, 0.4822834645669291653 ) ) ;
#32123 = CARTESIAN_POINT ( 'NONE',  ( 0.8107537697050234415, -0.1574803149606297803, 0.1058070865066461225 ) ) ;
#32124 = EDGE_LOOP ( 'NONE', ( #31156, #32759, #25334, #34775 ) ) ;
#32125 = DIRECTION ( 'NONE',  ( 0.000000000000000000, -1.000000000000000000, 0.000000000000000000 ) ) ;
#32126 = CARTESIAN_POINT ( 'NONE',  ( -0.7646288533564489232, -0.1113553986120547346, 1.176181102362204633 ) ) ;
#32127 = CARTESIAN_POINT ( 'NONE',  ( 0.1264236179284866091, -0.5319881889226142357, -0.1264236179284866091 ) ) ;
#32128 = CARTESIAN_POINT ( 'NONE',  ( 0.06523048226347956391, -1.117618110236220152, 0.1574803149606297803 ) ) ;
#32129 = CARTESIAN_POINT ( 'NONE',  ( 0.7185039370078739607, 1.928577636452523993E-17, 0.8858267715460158565 ) ) ;
#32130 = FACE_OUTER_BOUND ( 'NONE', #10177, .T. ) ;
#32131 = AXIS2_PLACEMENT_3D ( 'NONE', #44303, #26129, #1402 ) ;
#32132 = CARTESIAN_POINT ( 'NONE',  ( -0.8759842519685039353, -0.1787899950787401882, 0.4060039369541102450 ) ) ;
#32133 = VERTEX_POINT ( 'NONE', #42991 ) ;
#32134 = CARTESIAN_POINT ( 'NONE',  ( -1.002407869896990045, -0.1264236179284866091, 1.478838582623401399 ) ) ;
#32135 = CARTESIAN_POINT ( 'NONE',  ( 0.6971942568897648851, 0.07405724077823318263, 1.579724409395055318 ) ) ;
#32136 = ORIENTED_EDGE ( 'NONE', *, *, #3197, .F. ) ;
#32137 = CARTESIAN_POINT ( 'NONE',  ( 0.8759842519685039353, -0.1574803149606299191, 0.9350393699712126194 ) ) ;
#32138 = CARTESIAN_POINT ( 'NONE',  ( -0.7495606340400177148, -0.1264236179284866091, 0.6422244093950550958 ) ) ;
#32139 = CARTESIAN_POINT ( 'NONE',  ( 1.002407869896990045, -0.1264236179284866091, 0.1796259841982051075 ) ) ;
#32140 = CARTESIAN_POINT ( 'NONE',  ( -0.6971942568897648851, 0.07405724077823318263, 1.299212598371432215 ) ) ;
#32141 = ADVANCED_FACE ( 'NONE', ( #31552 ), #24345, .T. ) ;
#32142 = CARTESIAN_POINT ( 'NONE',  ( 0.000000000000000000, 0.1299212598425196763, 0.2007874015748031815 ) ) ;
#32143 = CARTESIAN_POINT ( 'NONE',  ( 0.9500414927467377701, 0.1787899950787401604, 0.7431102361667091261 ) ) ;
#32144 = CARTESIAN_POINT ( 'NONE',  ( -0.7495606340400177148, 0.1264236179284866091, 0.6668307086076534773 ) ) ;
#32145 = DIRECTION ( 'NONE',  ( 0.000000000000000000, -0.9699617890481186944, -0.2432573283306648515 ) ) ;
#32146 = ( BOUNDED_CURVE ( )  B_SPLINE_CURVE ( 2, ( #37175, #15864, #45050, #30034, #30490, #23036, #12263, #12512, #4559 ),
 .UNSPECIFIED., .F., .T. ) 
 B_SPLINE_CURVE_WITH_KNOTS ( ( 3, 2, 2, 2, 3 ),
 ( 0.01000000000000000021, 0.01250000000000000069, 0.01499999999999999944, 0.01750000000000000167, 0.02000000000000000042 ),
 .UNSPECIFIED. ) 
 CURVE ( )  GEOMETRIC_REPRESENTATION_ITEM ( )  RATIONAL_B_SPLINE_CURVE ( ( 1.000000000000000000, 0.9238795325112869605, 1.000000000000000000, 0.9238795325112869605, 1.000000000000000000, 0.9238795325112869605, 1.000000000000000000, 0.9238795325112869605, 1.000000000000000000 ) ) 
 REPRESENTATION_ITEM ( '' )  ) ;
#32147 = CARTESIAN_POINT ( 'NONE',  ( -0.9412147342319837628, -0.1574803149606297803, 0.8686023622047237547 ) ) ;
#32148 = CARTESIAN_POINT ( 'NONE',  ( -0.1574803149606297803, -0.1727362203649139838, 0.06523048226347956391 ) ) ;
#32149 = CARTESIAN_POINT ( 'NONE',  ( -0.7495606340400177148, 0.1264236179284866091, 1.380413385773007873 ) ) ;
#32150 = VERTEX_POINT ( 'NONE', #2515 ) ;
#32151 = CARTESIAN_POINT ( 'NONE',  ( -0.7185039370078739607, 1.928577636452523993E-17, 0.5019685039370078705 ) ) ;
#32152 = VECTOR ( 'NONE', #35940, 39.37007874015748143 ) ;
#32153 = ADVANCED_FACE ( 'NONE', ( #2745 ), #16452, .T. ) ;
#32154 = CARTESIAN_POINT ( 'NONE',  ( 0.9500414927467377701, 0.1787899950787401604, 1.254921259788757348 ) ) ;
#32155 = CARTESIAN_POINT ( 'NONE',  ( -0.1643945842212350683, -0.09851383576920552665, -0.06716829673107893584 ) ) ;
#32156 = ORIENTED_EDGE ( 'NONE', *, *, #17489, .F. ) ;
#32157 = CARTESIAN_POINT ( 'NONE',  ( -1.033464566929135131, 1.928577636452536319E-17, 0.03937007874015843040 ) ) ;
#32158 = EDGE_LOOP ( 'NONE', ( #21728, #6704, #10097, #3369 ) ) ;
#32159 = CARTESIAN_POINT ( 'NONE',  ( -0.3115983495410063475, 0.1719309546946380107, -0.1343271836544986386 ) ) ;
#32160 = ORIENTED_EDGE ( 'NONE', *, *, #34116, .F. ) ;
#32161 = CARTESIAN_POINT ( 'NONE',  ( 0.9500414927467378812, -0.1787899950787401604, 1.392716535379308285 ) ) ;
#32162 = CARTESIAN_POINT ( 'NONE',  ( 0.000000000000000000, 0.000000000000000000, -0.2748405511811023438 ) ) ;
#32163 = ( BOUNDED_CURVE ( )  B_SPLINE_CURVE ( 2, ( #12581, #4877, #27209, #41757, #30337, #23111, #30110, #22633, #8243 ),
 .UNSPECIFIED., .F., .F. ) 
 B_SPLINE_CURVE_WITH_KNOTS ( ( 3, 2, 2, 2, 3 ),
 ( 0.6500000000000000222, 0.6524999999999999689, 0.6550000000000000266, 0.6574999999999999734, 0.6600000000000000311 ),
 .UNSPECIFIED. ) 
 CURVE ( )  GEOMETRIC_REPRESENTATION_ITEM ( )  RATIONAL_B_SPLINE_CURVE ( ( 1.000000000000000000, 0.9238795325112899581, 1.000000000000000000, 0.9238795325112869605, 1.000000000000000000, 0.9238795325112869605, 1.000000000000000000, 0.9238795325112869605, 1.000000000000000000 ) ) 
 REPRESENTATION_ITEM ( '' )  ) ;
#32164 = CARTESIAN_POINT ( 'NONE',  ( -0.1264236179284866091, -0.2859251967966303098, -0.1264236179284866091 ) ) ;
#32165 = CARTESIAN_POINT ( 'NONE',  ( 0.1787899950787401604, -0.8100393700249772788, 0.07405724077823318263 ) ) ;
#32166 = AXIS2_PLACEMENT_3D ( 'NONE', #4705, #26067, #40636 ) ;
#32167 = EDGE_CURVE ( 'NONE', #23773, #18452, #25333, .T. ) ;
#32168 = FACE_OUTER_BOUND ( 'NONE', #14288, .T. ) ;
#32169 = CARTESIAN_POINT ( 'NONE',  ( 0.6971942568897637749, 2.189545951927499583E-17, 1.695374015694267822 ) ) ;
#32170 = CARTESIAN_POINT ( 'NONE',  ( 0.6971942568897637749, 2.189545951927499583E-17, 0.3174212597887562382 ) ) ;
#32171 = PRODUCT_DEFINITION_SHAPE ( 'NONE', 'NONE',  #47474 ) ;
#32172 = CARTESIAN_POINT ( 'NONE',  ( -0.1264236179284866091, -0.1393956217725458580, -0.1264236179284866091 ) ) ;
#32173 = CARTESIAN_POINT ( 'NONE',  ( 0.1264236179284866091, -0.2613188975840319284, 0.1264236179284866091 ) ) ;
#32174 = CARTESIAN_POINT ( 'NONE',  ( -1.094772975963752103E-17, 0.1028543307624250058, -0.1787899950787401882 ) ) ;
#32175 = ITEM_DEFINED_TRANSFORMATION ( 'NONE', 'NONE', #30128,  #20860 ) ;
#32176 = CARTESIAN_POINT ( 'NONE',  ( -0.7185039370078739607, 1.928577636452523993E-17, 0.6102362203649134287 ) ) ;
#32177 = CARTESIAN_POINT ( 'NONE',  ( 0.1574803149606299191, 0.000000000000000000, -0.0009999999999999347518 ) ) ;
#32178 = CARTESIAN_POINT ( 'NONE',  ( 0.7495606340400177148, 0.1264236179284866091, 0.5487204723871811352 ) ) ;
#32179 = TOROIDAL_SURFACE ( 'NONE', #42093, 0.03937007874015747977, 0.009842519685039369942 ) ;
#32180 = CARTESIAN_POINT ( 'NONE',  ( -1.002407869896990045, 0.1264236179284866091, 0.9374999999462362288 ) ) ;
#32182 = FACE_OUTER_BOUND ( 'NONE', #43793, .T. ) ;
#32181 = CARTESIAN_POINT ( 'NONE',  ( 0.06523048226347956391, -0.8813976377952761343, 0.1574803149606297803 ) ) ;
#32183 = CARTESIAN_POINT ( 'NONE',  ( 0.1270800023317771588, -1.757917825331076767, 0.1270800023317771588 ) ) ;
#32184 = CARTESIAN_POINT ( 'NONE',  ( 0.1574803149606300301, -0.5123031494987715373, 0.06523048226347956391 ) ) ;
#32185 = CARTESIAN_POINT ( 'NONE',  ( -0.1787899950787401882, -0.4335629920722205433, 0.000000000000000000 ) ) ;
#32186 = CARTESIAN_POINT ( 'NONE',  ( 0.8019270111902717657, 0.1787899950787401604, 1.653543307032850462 ) ) ;
#32188 = CARTESIAN_POINT ( 'NONE',  ( 0.1633669211802766530, 0.1605769902838746210, 5.116904466765171429E-07 ) ) ;
#32187 = CARTESIAN_POINT ( 'NONE',  ( 0.1877875577363964654, 0.07959431159475735540, -0.1770138738565708303 ) ) ;
#32189 = CARTESIAN_POINT ( 'NONE',  ( 0.9500414927467377701, -0.1787899950787401604, 0.4872047243556847929 ) ) ;
#32190 = ORIENTED_EDGE ( 'NONE', *, *, #44616, .F. ) ;
#32191 = CARTESIAN_POINT ( 'NONE',  ( -2.680625843783058887E-15, -0.2954942322624074524, -0.2921040715117803055 ) ) ;
#32192 = DIRECTION ( 'NONE',  ( -1.000000000000000000, 0.000000000000000000, 0.000000000000000000 ) ) ;
#32193 = CARTESIAN_POINT ( 'NONE',  ( -1.094772975963752103E-17, -0.1727362204186775607, -0.1787899950787401882 ) ) ;
#32194 = CARTESIAN_POINT ( 'NONE',  ( 0.8759842519685039353, 0.1787899950787401882, 0.5437992125446614589 ) ) ;
#32195 = CARTESIAN_POINT ( 'NONE',  ( 0.1264236179284866091, -1.088090551127338657, 0.1264236179284866091 ) ) ;
#32196 = CARTESIAN_POINT ( 'NONE',  ( 1.054774247047244540, -0.07405724077823318263, 0.1033464566391498751 ) ) ;
#32197 = FACE_OUTER_BOUND ( 'NONE', #39652, .T. ) ;
#32198 = CARTESIAN_POINT ( 'NONE',  ( 0.6971942568897648851, -0.07405724077823297447, 0.5561023621509617598 ) ) ;
#32199 = CARTESIAN_POINT ( 'NONE',  ( -0.7185039370078746268, -0.06523048226347956391, 0.9768700787401572994 ) ) ;
#32200 = CARTESIAN_POINT ( 'NONE',  ( -0.6971942568897648851, -0.07405724077823297447, 1.500984251914741607 ) ) ;
#32201 = ORIENTED_EDGE ( 'NONE', *, *, #28425, .T. ) ;
#32202 = CARTESIAN_POINT ( 'NONE',  ( -0.3100393700787401063, -0.01129866958151416051, -1.043307086614172485 ) ) ;
#32203 = CARTESIAN_POINT ( 'NONE',  ( 0.6971942568897648851, -0.07405724077823297447, 1.230314960576156746 ) ) ;
#32204 = CARTESIAN_POINT ( 'NONE',  ( -0.8107537697050253289, -0.1574803149606297803, 0.6963582676090082080 ) ) ;
#32205 = CARTESIAN_POINT ( 'NONE',  ( -1.033464566929133799, 0.000000000000000000, 1.102362204616881947 ) ) ;
#32206 = CARTESIAN_POINT ( 'NONE',  ( 0.8019270111902717657, 0.1787899950787401604, 1.845472440891119392 ) ) ;
#32207 = CARTESIAN_POINT ( 'NONE',  ( -1.033464566929134687, -0.06523048226347956391, 1.424704724409449064 ) ) ;
#32208 = CARTESIAN_POINT ( 'NONE',  ( -1.002407869896990045, -0.1264236179284866091, 0.9621062991588346103 ) ) ;
#32209 = EDGE_CURVE ( 'NONE', #33762, #46575, #15374, .T. ) ;
#32210 = DIRECTION ( 'NONE',  ( 0.8191520442889991260, 1.003171929053533745E-16, -0.5735764363510356123 ) ) ;
#32211 = CARTESIAN_POINT ( 'NONE',  ( -0.7085582780037171791, 0.06187450949840840597, 0.03937007874015843734 ) ) ;
#32212 = CARTESIAN_POINT ( 'NONE',  ( 1.054774247047244096, 0.000000000000000000, 0.3420275590013546751 ) ) ;
#32213 = CARTESIAN_POINT ( 'NONE',  ( -1.054774247047244540, -0.07405724077823318263, 0.1377952755367876370 ) ) ;
#32214 = UNCERTAINTY_MEASURE_WITH_UNIT (LENGTH_MEASURE( 1.000000000000000082E-05 ), #35928, 'distance_accuracy_value', 'NONE') ;
#32215 = CARTESIAN_POINT ( 'NONE',  ( -0.7495606340400177148, -0.1264236179284866091, 0.6373031495525354195 ) ) ;
#32216 = CARTESIAN_POINT ( 'NONE',  ( 0.9873396505805591694, 0.1113553986120547346, 1.540354330601133803 ) ) ;
#32217 = ORIENTED_EDGE ( 'NONE', *, *, #20513, .T. ) ;
#32218 = ADVANCED_FACE ( 'NONE', ( #45649 ), #17372, .F. ) ;
#32219 = CIRCLE ( 'NONE', #12299, 0.1968503937007874127 ) ;
#32220 = CARTESIAN_POINT ( 'NONE',  ( 0.1787899950787401882, 0.05364173233722811102, -2.189545951927503898E-17 ) ) ;
#32221 = CARTESIAN_POINT ( 'NONE',  ( 0.7185039370078714072, 0.06523048226347728795, 1.788877952648379122 ) ) ;
#32222 = CARTESIAN_POINT ( 'NONE',  ( 0.8019270111902717657, 0.1787899950787401604, 0.8267716534895444003 ) ) ;
#32223 = EDGE_CURVE ( 'NONE', #38458, #34404, #34948, .T. ) ;
#32224 = CARTESIAN_POINT ( 'NONE',  ( -0.8019270111902716547, -0.1787899950787401604, 1.742125984198204858 ) ) ;
#32225 = CIRCLE ( 'NONE', #3866, 0.1864803149606298061 ) ;
#32226 = ADVANCED_FACE ( 'NONE', ( #23871 ), #35140, .F. ) ;
#32227 = VECTOR ( 'NONE', #45600, 39.37007874015748143 ) ;
#32228 = CARTESIAN_POINT ( 'NONE',  ( -0.3100393700787401619, 0.000000000000000000, -1.181102362204724310 ) ) ;
#32229 = DIRECTION ( 'NONE',  ( 0.000000000000000000, 0.000000000000000000, 1.000000000000000000 ) ) ;
#32230 = CARTESIAN_POINT ( 'NONE',  ( 0.1787899950787401882, -1.335261763504828947, -2.189545951927503898E-17 ) ) ;
#32231 = ORIENTED_EDGE ( 'NONE', *, *, #33256, .F. ) ;
#32232 = AXIS2_PLACEMENT_3D ( 'NONE', #28248, #17675, #25109 ) ;
#32233 = CARTESIAN_POINT ( 'NONE',  ( -1.094772975963752103E-17, -0.1678149605761578844, -0.1787899950787401882 ) ) ;
#32234 = ORIENTED_EDGE ( 'NONE', *, *, #35872, .T. ) ;
#32235 = CARTESIAN_POINT ( 'NONE',  ( 0.6971942568897637749, 2.189545951927499583E-17, 1.104822834591905556 ) ) ;
#32236 = CARTESIAN_POINT ( 'NONE',  ( 0.005401850751748405420, -0.1458776762657084669, -0.02292264490068926519 ) ) ;
#32237 = CARTESIAN_POINT ( 'NONE',  ( -1.033464566929134687, 0.06523048226347956391, 0.9867125983176703308 ) ) ;
#32238 = CARTESIAN_POINT ( 'NONE',  ( 0.8019270111902717657, 0.1787899950787401604, 0.07381889758403178958 ) ) ;
#32239 = CARTESIAN_POINT ( 'NONE',  ( 0.1264236179284866091, -1.526082677111590513, 0.1264236179284866091 ) ) ;
#32240 = CARTESIAN_POINT ( 'NONE',  ( -0.1264236179284866091, -0.7485236219934803259, 0.1264236179284866091 ) ) ;
#32241 = CARTESIAN_POINT ( 'NONE',  ( -1.054774247047244540, -0.07405724077823318263, 0.4183070865604096578 ) ) ;
#32243 = CARTESIAN_POINT ( 'NONE',  ( -0.7163004791323965836, -0.05128305946486693551, 1.984233574417522350 ) ) ;
#32242 = CARTESIAN_POINT ( 'NONE',  ( 0.1797182628040039365, -1.241185541866509645, -2.200913952912460540E-17 ) ) ;
#32244 = CARTESIAN_POINT ( 'NONE',  ( -0.09118578515492140046, 0.2428480946569460674, -0.03489849683095607585 ) ) ;
#32245 = CARTESIAN_POINT ( 'NONE',  ( 1.054774247047244540, -0.07405724077823318263, 1.245078740103716886 ) ) ;
#32246 = CARTESIAN_POINT ( 'NONE',  ( 0.6971942568897637749, 2.189545951927499583E-17, 1.537893700733637736 ) ) ;
#32247 = VECTOR ( 'NONE', #46878, 39.37007874015748143 ) ;
#32248 = VECTOR ( 'NONE', #44413, 39.37007874015748143 ) ;
#32249 = CARTESIAN_POINT ( 'NONE',  ( 0.9412147342319837628, -0.1574803149606297803, 1.656003937007873406 ) ) ;
#32250 = FACE_OUTER_BOUND ( 'NONE', #29323, .T. ) ;
#32252 = CARTESIAN_POINT ( 'NONE',  ( -0.8759842519685039353, -0.1574803149606299191, 1.102362204724409489 ) ) ;
#32251 = CARTESIAN_POINT ( 'NONE',  ( 0.1608809531673208726, 0.08280530883162598443, 0.1377952755905511861 ) ) ;
#32253 = CIRCLE ( 'NONE', #8494, 0.01968503937007874335 ) ;
#32254 = DIRECTION ( 'NONE',  ( 1.822029033848725028E-16, 0.000000000000000000, 1.000000000000000000 ) ) ;
#32255 = CARTESIAN_POINT ( 'NONE',  ( -0.9412147342319837628, 0.1574803149606300301, 1.779035432963339991 ) ) ;
#32256 = CARTESIAN_POINT ( 'NONE',  ( 0.1787899950787401604, -0.02263779522182702425, 0.07405724077823318263 ) ) ;
#32257 = CARTESIAN_POINT ( 'NONE',  ( 1.002407869896990045, -0.1264236179284866091, 0.09596456687537027741 ) ) ;
#32259 = CARTESIAN_POINT ( 'NONE',  ( -0.8759842519685039353, -0.1574803149606299191, 0.5413385825696385156 ) ) ;
#32258 = CARTESIAN_POINT ( 'NONE',  ( 1.002407869896990045, 0.1264236179284866091, 1.208169291284818980 ) ) ;
#32260 = CARTESIAN_POINT ( 'NONE',  ( 0.6971942568897637749, 2.189545951927499583E-17, 1.936515747977732405 ) ) ;
#32261 = CARTESIAN_POINT ( 'NONE',  ( 0.9873396505805591694, -0.1113553986120547346, 0.5068897636720007815 ) ) ;
#32262 = ORIENTED_EDGE ( 'NONE', *, *, #6307, .T. ) ;
#32263 = DIRECTION ( 'NONE',  ( 0.000000000000000000, 0.000000000000000000, -1.000000000000000000 ) ) ;
#32264 = CARTESIAN_POINT ( 'NONE',  ( 0.8716041552374669266, 0.1747403318699642938, 0.03936765223768743521 ) ) ;
#32265 = CARTESIAN_POINT ( 'NONE',  ( -0.8759842519685039353, -0.1574803149606299191, 0.4625984250893235838 ) ) ;
#32266 = VERTEX_POINT ( 'NONE', #2053 ) ;
#32267 = CARTESIAN_POINT ( 'NONE',  ( 0.8019270111902717657, -0.1787899950787401604, 1.387795275536786610 ) ) ;
#32269 = CARTESIAN_POINT ( 'NONE',  ( -1.033464566929134687, -0.06523048226347956391, 0.2337598424121580809 ) ) ;
#32268 = CARTESIAN_POINT ( 'NONE',  ( 0.7185039370078739607, 1.928577636452523993E-17, 1.564960629921259949 ) ) ;
#32270 = CARTESIAN_POINT ( 'NONE',  ( 0.1264236179284866091, -0.06446850388324429360, 0.1264236179284866091 ) ) ;
#32271 = EDGE_LOOP ( 'NONE', ( #45331, #23613, #6485, #44419 ) ) ;
#32272 = CARTESIAN_POINT ( 'NONE',  ( 0.4453382816733590377, -3.032960542342102697E-32, 0.09842519685039370636 ) ) ;
#32273 = EDGE_CURVE ( 'NONE', #44530, #12585, #27736, .T. ) ;
#32274 = ORIENTED_EDGE ( 'NONE', *, *, #36261, .T. ) ;
#32275 = CARTESIAN_POINT ( 'NONE',  ( 0.9412147342319837628, -0.1574803149606297803, 1.291830708553889595 ) ) ;
#32276 = SURFACE_STYLE_FILL_AREA ( #14523 ) ;
#32277 = CARTESIAN_POINT ( 'NONE',  ( 1.054774247047244096, 0.000000000000000000, 0.6569881889226141247 ) ) ;
#32279 = EDGE_CURVE ( 'NONE', #42583, #1531, #20120, .T. ) ;
#32278 = VERTEX_POINT ( 'NONE', #36064 ) ;
#32280 = CARTESIAN_POINT ( 'NONE',  ( -0.7495606340400177148, 0.1264236179284866091, 1.336122047190330786 ) ) ;
#32282 = CARTESIAN_POINT ( 'NONE',  ( 0.1787899950787401604, -1.754921259788755128, -0.07405724077823318263 ) ) ;
#32281 = CARTESIAN_POINT ( 'NONE',  ( 0.1574803149606300301, -0.4286417321759371513, -0.06523048226347956391 ) ) ;
#32283 = CARTESIAN_POINT ( 'NONE',  ( -0.7185039370078746268, 0.06523048226347956391, 0.1845472440944883052 ) ) ;
#32284 = ORIENTED_EDGE ( 'NONE', *, *, #25936, .T. ) ;
#32285 = CARTESIAN_POINT ( 'NONE',  ( -1.054774247047244540, -0.07405724077823318263, 1.122047244040725422 ) ) ;
#32286 = ADVANCED_FACE ( 'NONE', ( #16402 ), #26113, .T. ) ;
#32287 = CARTESIAN_POINT ( 'NONE',  ( -1.054774247047244540, -0.07405724077823318263, 0.7726377952218265177 ) ) ;
#32288 = CARTESIAN_POINT ( 'NONE',  ( -0.8759842519685039353, 0.1787899950787401882, 0.1943897637257641919 ) ) ;
#32289 = CARTESIAN_POINT ( 'NONE',  ( -4.999628824793424855E-17, -0.2954942322624090623, -0.3149606299212598381 ) ) ;
#32290 = DIRECTION ( 'NONE',  ( 1.000000000000000000, 0.000000000000000000, 0.000000000000000000 ) ) ;
#32291 = CARTESIAN_POINT ( 'NONE',  ( 0.07405724077823318263, -0.8702027083867192037, 0.1787899950787401604 ) ) ;
#32292 = ORIENTED_EDGE ( 'NONE', *, *, #40028, .F. ) ;
#32293 = CARTESIAN_POINT ( 'NONE',  ( -0.1184675242425147629, -0.09842519685039370636, 1.713085361781126803 ) ) ;
#32294 = ORIENTED_EDGE ( 'NONE', *, *, #44681, .T. ) ;
#32295 = CARTESIAN_POINT ( 'NONE',  ( -0.7185039370078739607, 1.928577636452523993E-17, 1.712598425089322918 ) ) ;
#32296 = CIRCLE ( 'NONE', #24607, 0.3912448816427701037 ) ;
#32297 = VECTOR ( 'NONE', #24012, 39.37007874015748143 ) ;
#32299 = DIRECTION ( 'NONE',  ( 0.000000000000000000, -1.000000000000000000, 0.000000000000000000 ) ) ;
#32298 = AXIS2_PLACEMENT_3D ( 'NONE', #9308, #1868, #12452 ) ;
#32300 = CARTESIAN_POINT ( 'NONE',  ( -0.7495606340400177148, 0.1264236179284866091, 0.6274606298674959559 ) ) ;
#32301 = ( BOUNDED_SURFACE ( )  B_SPLINE_SURFACE ( 1, 2, ( 
 ( #40145, #4194, #18822, #7100, #14778, #22179, #25804, #7804, #21726, #596, #39667, #36814, #47365, #6853, #43989, #3970, #18588, #33246, #36358, #14539, #30832, #37513, #27236, #15492, #37990, #44917, #15968, #1313, #22665, #828, #37268, #33721, #26750, #8747, #20003, #34403, #26515, #19296, #40843, #19534, #30135, #12612, #41309, #8036, #45626, #1548, #8989, #33952, #12129, #23387, #4422, #8511, #16197, #26284, #41790, #44676, #4669, #41076, #8273, #30370, #23611, #1073, #15734, #45401, #23141, #37757, #26996, #4912, #16433, #34184, #30592, #45155, #12372, #41544, #5150, #19772, #38223, #5383, #34642, #1794, #31062, #24546, #34888, #6565, #20941, #6318, #39148, #20706, #42723, #24782, #31987, #17589, #13307, #46107, #27936, #2952, #31289, #24092, #9940, #35580, #16661, #46576, #13759, #2722, #42502, #2031, #42025, #38701, #12843, #10176, #20478, #17353, #28399, #20239, #16883, #27474, #2492, #9708, #42966, #39380, #31525, #5630, #24321, #38919, #45867, #6081, #21174, #35808, #13082, #35347, #28162, #46341, #32233, #27713, #9231, #23846, #38459, #5873, #42276, #17119, #31758, #2260, #13526, #9477, #35115, #3910, #10654, #309, #36043, #11129, #18062, #36524, #21901, #43206, #21414, #10420, #6795, #7504, #43930, #32708, #3202, #33185, #14478, #14000, #18760, #22123, #29617, #39851, #47301, #25749, #28649, #29135, #36751, #46813, #14955, #17830, #43451, #25020, #32475, #3450, #44158, #39618, #47054, #18531, #25262, #14249, #66, #43690, #36981, #28891, #10896, #25519, #32945, #40087, #40319, #7040, #29385, #11358, #21666, #25966, #3679, #40549, #36298, #7742, #22356, #4139, #7284, #18303, #14710, #45333, #5086, #38157, #33890, #19234, #1011, #23553, #4356, #44612, #30528, #15904, #37212, #19708, #34349, #8684, #15668, #22599, #15190, #11829, #33420, #30769, #41017, #45088, #37933, #40783, #37449, #534, #23077, #30305, #12305, #23320, #4600, #26216, #44855, #12065, #18992, #26689, #16137, #12550, #33651, #41240, #1250, #19470, #1480, #765, #27172, #41725, #26927, #26452, #8929, #8445, #37691, #22834, #4844, #34122, #41478, #29838, #8207, #44381, #15426, #11591, #7977, #30074, #42439, #16371, #41958, #30995, #27414, #28103, #17057, #38631, #20415, #2431, #13694, #42663, #5564, #13008, #34573, #13250, #42901, #31225, #9165, #24720, #13472, #6025, #20646, #45801, #23780, #2199, #5805, #27651, #9879, #38394, #10111, #31698, #16819, #39320, #17294, #31927, #9645, #39083, #24263, #24489, #42207, #16599, #19937, #1726, #35050, #31459, #46043, #45558, #6255, #12778, #20881, #35291, #20174, #9409, #38859, #46282, #24027, #35523, #27879, #2663, #46515, #34825, #28329, #1968, #28829, #11300, #11070, #17525, #40261, #13938, #17999, #32651, #10356, #17298, #35530, #9416, #28336, #24268, #16823, #13255, #9652, #38639, #21122, #38865, #10116, #34830, #2895, #13015, #41964, #6028, #5812, #20421, #42671, #42214, #24036, #46521, #20650, #27658, #24726, #27884, #2205, #35296, #28110, #35055, #39327, #2435, #46757, #42445, #42908, #31466, #46048, #24496, #17060, #31702, #46287, #39090, #13943, #23788, #6503, #6262, #35755, #32165, #20888, #38400, #2668, #5571, #20182, #1974, #16604, #31230, #10362, #46995, #21358, #29328, #40266, #43873, #6739, #255, #7451, #35985, #36471, #25203, #24968, #3146, #33367, #22072, #14657, #11076, #6983, #17770, #10843, #47242, #39788, #18480, #32418, #18706, #25695, #25458, #485, #25917, #40499, #18247, #14901, #32889, #33130, #21606, #36241, #28588, #43152, #14424, #43633, #40030, #39563, #29562, #14188, #44112, #36700, #28835, #3391, #3626, #5, #18003, #3859, #7225, #11305, #7685, #43392, #22304, #32656, #29076, #36936, #4086, #10605, #21848, #22544, #715, #41192, #11536, #37884, #8634, #30022, #34302, #44806, #37390, #33841, #30258, #11785, #41674, #12018, #30712, #7926, #23513, #33602, #15140, #26642, #26403, #40965, #15857, #15372, #44569, #19660, #8397, #18940, #45283, #959, #22782, #23024, #34075, #8156, #12500, #37639, #19892, #15617, #5040, #4548, #19180, #45039, #4794, #19420, #1202, #30479, #34522, #29786, #1429, #12255, #27124, #16091, #26874, #44334, #41437, #23268, #8879, #38115, #26162, #5278, #40731, #37162, #4308, #2378, #13431, #17016, #27366, #20834, #28061, #41909, #9599, #45752, #30951, #9120, #24676, #12963, #23737, #45516, #38341, #39273, #27603, #5518, #6448, #42621, #35244, #31653, #42152, #20133, #31419, #20367, #9361, #39039, #34778, #21064, #46226, #45995, #1679, #46463, #13647, #38818, #35474, #5978, #6204, #23983, #38584, #16325, #12736, #35005, #16779, #13205, #1918, #2612, #16552, #17249, #9831, #31180, #5758, #24219, #20599, #2152, #24438, #27838, #31886, #28285, #42399, #42849, #10058, #10544, #36641, #39975, #3802, #22015, #43098, #21299, #14371, #32109, #11015, #29271, #3088, #7402, #17942, #25141, #6919, #3339, #32364, #14837, #32600, #18419, #28529, #44050, #6681, #35702, #47189, #46941, #14130, #36417, #35925, #17710, #40210, #29017, #39507, #33067, #21543, #43343, #43574, #7167, #28775, #191, #10787, #40440, #36181, #25634, #39733, #25396, #18192, #21792, #3574, #32831, #47427, #7628, #2839, #29503, #14598, #11249, #25859, #43816, #17473, #46696, #13886, #10304, #24917, #4028, #26098, #18647, #40669, #15083, #22965, #34014, #37573, #431, #41372, #1139, #29730, #30200, #18883, #8338, #8572, #7866, #23208, #34243, #4733, #15309, #12188, #37333, #15561, #11726, #897, #41138, #11963, #26815, #33540, #37822, #11474, #15799, #40905, #26582, #44744, #33304, #44272, #22483, #37099, #30425, #19358, #8103, #22723, #44975, #16029, #4979, #4248, #29961, #36873, #19601, #654, #1372, #4480, #44508, #41609, #30655, #45216, #26345, #19121, #12436, #27059, #22243, #37223, #19242, #15435, #36534, #43940, #29145, #18314, #3918, #30089, #43699, #40097, #22610, #25757, #25532, #543, #29627, #37460, #14722, #18542, #25976, #33430, #33197, #44391, #3690, #29848, #11605, #11138, #26227, #36992, #40792, #21911, #41026, #7986, #4369, #19000, #7751, #33661, #11837, #775, #4610, #318, #14971, #40560, #47311, #29394, #40327, #26466, #8221, #7513, #22846, #14485, #7292, #22368, #36762, #4147, #18774, #15199, #31236, #41489, #45570, #38404, #41253, #37945, #1022, #5327, #45344, #16381, #9173, #5094, #26699, #27181, #41736, #37702, #8938, #16609, #13021, #1258, #19947, #12790, #30316 ),
 ( #23793, #34585, #27425, #23330, #41968, #5577, #34834, #1979, #45101, #45813, #23084, #27662, #42219, #9424, #24042, #44865, #8455, #12074, #12319, #5818, #32174, #39096, #20896, #2902, #14195, #28598, #6032, #13484, #35059, #13707, #42451, #21365, #2673, #2210, #39797, #43160, #3152, #28113, #6267, #46763, #16829, #17304, #24974, #27891, #35993, #9657, #17067, #24273, #38869, #46527, #32425, #35301, #31707, #39569, #46292, #42676, #21127, #28343, #10609, #9888, #24733, #35761, #47002, #28840, #43399, #10852, #36939, #18712, #3633, #4090, #44115, #33372, #29084, #720, #15146, #490, #11545, #14907, #26168, #33607, #40737, #26408, #22080, #40273, #3867, #44572, #25465, #18255, #7932, #15380, #7234, #6989, #21614, #36248, #18486, #43642, #3399, #32897, #18010, #47250, #14664, #21854, #36480, #15, #11082, #29338, #11310, #43881, #33134, #25702, #262, #25924, #40506, #7695, #22309, #19899, #45521, #12743, #965, #27374, #5524, #30263, #1437, #37645, #22789, #44812, #31186, #23274, #41196, #12970, #20138, #27131, #1925, #37889, #8402, #5047, #19667, #16097, #40973, #30720, #8161, #11259, #11026, #29280, #25643, #441, #15094, #45565, #1487, #16376, #15910, #30533, #31229, #11834, #8690, #23324, #45339, #4606, #12784, #41730, #27420, #8934, #26460, #23559, #38162, #34579, #20649, #13701, #13478, #28335, #28587, #3144, #21121, #42443, #35295, #46756, #42907, #43151, #32164, #5811, #31465, #24495, #42213, #2893, #39326, #27883, #17532, #28109, #2434, #46286, #42670, #9651, #24967, #9882, #10361, #38638, #21356, #46047, #45807, #39089, #24267, #6261, #10115, #20887, #6501, #39562, #17769, #2204, #13014, #27657, #9415, #24034, #20420, #25457, #15139, #25694, #4307, #18246, #22303, #47240, #43632, #14900, #40029, #21847, #40265, #18002, #32417, #25202, #36935, #4, #29785, #4085, #7450, #36240, #21605, #36699, #3858, #33129, #44111, #253, #18479, #18704, #11304, #29561, #25916, #40497, #7684, #33366, #7925, #11535, #26161, #40730, #22543, #27365, #26291, #379, #11199, #22425, #11423, #15033, #30142, #135, #3749, #22671, #4200, #18371, #37519, #19304, #29903, #41082, #44453, #8280, #44222, #26042, #25812, #40616, #7811, #18829, #33485, #8042, #22907, #33727, #33959, #836, #1081, #15742, #1802, #16441, #34411, #45632, #41798, #31069, #42285, #16891, #2037, #23393, #1553, #27721, #12852, #9484, #13089, #34191, #12381, #5390, #23148, #16667, #20250, #41549, #45877, #8997, #16208, #45407, #23620, #37997, #5879, #38232, #24102, #19543, #35121, #45160, #26759, #20010, #5157, #19778, #27483, #27002, #8754, #31297, #42035, #30597, #38709, #12621, #30841, #9237, #23856, #27242, #20486, #38467, #31536, #5638, #2270, #34896, #46117, #41316, #8519, #37763, #4921, #1318, #15975, #18072, #32483, #28407, #10664, #47066, #31768, #42511, #17598, #39159, #21183, #36051, #9716, #3460, #25271, #39859, #2962, #28899, #32240, #43458, #6329, #9946, #32719, #13314, #10185, #24791, #35814, #24329, #7051, #38928, #21675, #14009, #6090, #35591, #46822, #28658, #43221, #10428, #36306, #35358, #2503, #17126, #46351, #24551, #28170, #45036, #958, #12254, #30477, #4084, #29783, #22781, #40496, #19419, #37638, #11534, #15856, #26402, #18939, #15370, #11784, #40729, #23267, #40964, #26873, #36934, #5039, #15138, #44110, #8154, #7924, #22542, #44805, #44333, #26160, #1201, #37388, #484, #41436, #30021, #4306, #4547, #15616, #37159, #8631, #19178, #1427, #44568, #34074, #33600, #714, #26640, #33840, #30257, #12016, #41190, #16089, #11302, #37883, #8396, #19659, #34301, #23023, #25915, #4793, #7683, #22302, #18702, #33365, #34520, #12499, #1678, #23512, #31418, #9598, #45994, #8878, #2377, #24218, #38114, #38583, #27364, #27122, #5275, #6203, #41908, #19891, #35473, #38817, #13204, #5976, #9118, #30950, #12961, #1917, #23736, #20597, #45515, #20833, #35243, #27602, #42151, #12735, #45282, #41673, #31652, #16550, #28060, #13430, #38340, #5517, #35004, #20132, #9360, #42620, #34777, #31179, #45751, #23982, #5757, #24437, #39038, #2151, #42847, #36416, #29016, #24675, #25140, #13884, #46462, #39272, #40208, #28528, #6447, #22014, #10786, #3337, #17941, #43097, #21063, #46940, #35924, #10303, #7166, #35701, #7401, #47188, #14129, #36640, #14597, #29270, #6918, #3573, #21542, #21790, #24916, #39506, #17248, #31885, #3087, #32362, #28774, #13646, #18191, #28284, #32830, #32599, #2838, #21298, #39732, #36180, #17709, #14370, #43342, #43572, #47425, #17472, #39974, #10543, #25395, #43815, #11014, #25633, #32107, #46695, #36872, #29960, #190, #26581, #44743, #18646, #22964, #33539, #26097, #22482, #18882, #430, #30424, #652, #19357, #44049, #12187, #22242, #3800, #15307, #15082, #29728, #4479, #4027, #33303, #8337, #44507, #7626, #34013, #37098, #11472, #11725, #22722, #44271, #1138, #26344, #8570, #4247, #41137, #40668, #7865, #896, #40904, #8102, #41371, #15560, #37332, #23207, #15798, #44974, #19119, #37571, #30199, #4732, #11962, #26813, #33066, #14836, #29502, #11247, #25858, #40439, #42975, #19600, #10184, #38525, #28657, #30896, #12908, #27539, #45452, #9297, #5453, #42092, #6571, #43220, #13766, #34462, #12674, #39388, #23917, #21181, #24790, #45215, #23448, #16490, #34242, #28406, #31994, #5207, #35813, #20070, #27299, #9055, #34715, #1612, #17597, #1854, #2961, #30653, #46821, #8810, #37821, #31123, #16261, #41851, #5695, #38050, #19832, #32239, #45686, #41608, #14008, #23676, #38283, #20305, #34945, #2092, #10427, #16721, #4978, #46585, #1371, #16028, #12435, #27057, #39858, #25270, #21910, #43457, #29847, #44390, #14970, #43698, #22367, #11366, #10663, #39624, #29393, #3459, #3689, #3917, #6802, #28898, #21422, #7050, #17839, #7512, #36761, #22133, #3209, #25975, #33196, #32482, #32953, #36305, #36050, #47065, #542, #18071, #14256, #25028, #317, #29626, #40559, #32718, #47310, #7291, #10908, #29144, #7750, #25531, #40096, #36533, #36991, #4146, #18313, #74, #18773, #33429, #15198, #14721, #43939, #23562, #26936, #4609, #1490, #26698, #4856, #1021, #23083, #30537, #1257, #16147, #22845, #12556, #774, #23329, #30315, #15912, #34130, #7985, #33660, #22609, #18999, #19716, #8694, #44864, #12073, #41488, #5326, #34355, #44623, #19241, #26226, #19478, #15434, #45343, #41252, #40791, #31001, #30777, #41735, #33902, #8454, #37944, #37222, #37701 ),
 ( #11836, #45100, #4368, #27180, #5093, #26465, #8937, #12318, #15678, #38164, #19946, #8220, #34584, #1737, #16380, #30088, #11604, #41025, #37459, #9656, #9423, #24041, #46291, #45812, #13020, #2672, #13262, #1978, #13706, #31469, #5817, #27890, #17066, #38643, #28342, #42450, #2900, #16828, #35533, #27661, #42218, #28112, #20425, #35058, #24272, #16608, #17537, #45569, #17303, #38868, #12789, #46052, #31938, #2209, #6031, #42675, #20655, #35300, #2438, #31235, #27424, #41967, #46526, #31706, #42914, #10123, #13483, #9172, #9887, #24501, #39095, #6266, #23792, #24732, #38403, #39330, #5576, #6509, #21126, #35759, #20185, #34833, #36478, #10368, #47248, #32424, #46761, #43158, #3865, #47000, #39567, #33133, #18253, #25463, #40037, #14193, #6744, #3397, #39796, #28839, #13, #24972, #18485, #7233, #18008, #261, #40272, #7458, #29082, #29336, #43639, #14662, #43397, #10608, #32172, #13947, #36246, #32662, #14430, #21363, #11081, #35990, #25700, #21853, #28597, #10850, #32895, #43879, #3631, #22079, #36704, #3151, #17776, #25207, #6988, #21612, #2367, #28517, #31873, #43089, #13874, #34997, #13193, #20822, #23972, #2830, #21053, #42389, #10293, #9825, #17004, #46219, #42610, #24207, #6672, #24430, #39498, #2142, #35914, #45984, #27593, #39030, #5969, #20588, #28274, #27829, #9588, #21290, #35461, #31409, #3072, #13419, #35235, #2605, #46452, #31643, #17702, #32350, #16768, #28051, #42142, #17237, #13635, #10048, #17463, #42838, #39261, #6438, #35693, #46929, #9351, #11462, #40656, #47175, #29260, #29492, #178, #418, #17934, #15070, #26081, #44036, #7155, #4016, #43804, #7394, #3565, #25622, #33058, #3792, #18635, #25386, #29717, #3321, #25848, #32819, #18409, #36629, #10534, #36167, #25131, #21529, #22228, #11237, #47412, #14586, #40430, #7853, #36861, #14358, #21779, #28762, #22004, #29006, #22471, #11004, #43332, #33526, #33295, #37089, #36407, #40197, #4237, #39721, #14825, #18867, #14120, #6907, #43563, #10775, #39962, #18178, #4722, #30883, #44492, #40895, #23432, #26569, #29947, #1364, #30416, #38273, #19107, #19346, #44965, #34233, #34000, #45202, #4466, #30641, #12426, #44732, #27046, #37809, #41594, #22711, #41839, #8799, #38040, #5197, #8561, #19823, #12665, #34451, #5440, #1128, #15787, #12176, #20057, #33772, #11948, #1597, #16251, #883, #45443, #27290, #9044, #26800, #37317, #11709, #41124, #642, #23665, #8321, #15295, #26334, #15543, #8088, #41358, #22952, #23195, #4962, #37562, #30187, #19589, #16018, #27528, #43025, #5682, #34700, #46163, #45921, #13136, #35405, #34935, #16709, #39200, #2310, #20292, #2777, #16940, #42330, #31580, #2545, #27770, #17401, #13359, #39440, #27987, #24601, #31338, #9525, #17176, #42554, #9760, #42775, #9991, #6620, #1844, #6377, #20988, #32040, #46631, #13815, #16482, #28456, #10231, #24839, #31111, #45676, #42080, #9285, #23904, #14055, #21957, #33003, #36577, #46870, #40376, #125, #28702, #29201, #17882, #3011, #43275, #44213, #32527, #10476, #26031, #14775, #7344, #3739, #47113, #25074, #3509, #39909, #14304, #11191, #39664, #11413, #18360, #18120, #40606, #18586, #33244, #10951, #7563, #25571, #25802, #28947, #43508, #21233, #35859, #7097, #36356, #32766, #17645, #22176, #36812, #6849, #10717, #32291, #21467, #25323, #3968, #36099, #3257, #43987, #21724, #47363, #29439, #14536, #43751, #40142, #369, #15022, #29675, #41074, #4910, #11659, #37755, #19532, #4420, #40841, #826, #22418, #1071, #29896, #41543, #22898, #37041, #27234, #30590, #37988, #15490, #26513, #34182, #8745, #4192, #8271, #12127, #23385, #44440, #19051, #18820, #26281, #11892, #5148, #33476, #594, #45153, #33719, #15251, #8509, #37511, #45399, #8034, #4667, #19294, #41307, #15732, #1311, #22663, #15966, #12370, #30133, #26994, #44915, #19770, #37266, #1545, #34401, #16194, #30830, #30369, #12610, #7802, #44674, #26748, #23139, #27711, #42274, #31985, #12841, #5628, #38917, #24319, #45624, #28160, #42721, #17116, #9475, #31060, #23609, #20237, #41788, #39146, #2029, #6079, #46339, #1792, #45865, #8987, #31523, #24090, #20704, #31756, #13080, #34640, #38699, #5871, #27472, #20476, #24544, #20938, #42023, #35113, #9706, #27934, #9938, #9229, #6316, #35578, #35345, #34886, #13524, #2258, #16881, #31287, #46105, #13304, #42500, #2720, #16659, #17351, #23844, #2490, #46574, #13757, #38221, #5381, #16431, #20001, #38457, #36522, #25517, #47052, #28889, #10894, #22121, #3677, #13998, #21412, #42964, #21664, #2950, #14708, #43449, #10174, #306, #18301, #11127, #36041, #14247, #40084, #29383, #24780, #10652, #32706, #43927, #17587, #25018, #39378, #46811, #32473, #25748, #6563, #21172, #32943, #6793, #35806, #29133, #25260, #18529, #28647, #39849, #7038, #14476, #36295, #7282, #32230, #21899, #64, #39616, #40317, #18060, #7502, #43204, #36749, #3907, #33183, #28397, #3448, #10418, #3200, #17828, #47299, #43688, #762, #15424, #5083, #33418, #26214, #12063, #44853, #18757, #1247, #15901, #37689, #30072, #4135, #44156, #40781, #14953, #12302, #22597, #26687, #19466, #22353, #18990, #29614, #4597, #44610, #41238, #4841, #33649, #7738, #11826, #26449, #532, #41014, #45085, #41475, #15188, #8205, #30303, #1009, #30525, #29836, #26925, #8681, #8443, #7974, #34119, #22831, #37446, #4354, #19232, #33888, #15665, #23316, #37210, #37930, #44379, #23075, #19705, #34346, #11356, #25964, #36979, #40546, #11589, #9642, #46040, #20171, #31222, #31456, #42661, #24260, #35289, #2429, #6022, #45798, #5318, #30766, #9162, #1477, #13470, #23777, #13247, #20644, #8926, #5561, #45330, #38628, #13005, #27876, #28101, #27648, #41722, #42204, #9406, #19934, #24024, #9877, #24487, #34570, #5802, #16816, #2196, #39081, #1723, #6253, #20878, #42437, #38391, #12547, #20412, #16368, #30992, #45555, #12775, #25197, #40025, #46749, #36466, #24718, #14420, #21349, #39782, #10599, #46514, #10109, #13692, #42899, #43627, #29070, #35978, #3136, #25451, #44498, #7220, #21112, #28581, #2661, #28827, #6495, #21842, #32412, #17292, #8095, #3622, #18875, #10354, #46990, #33533, #647, #28327, #14183, #6976, #15301, #24961, #43387, #21600, #36236, #3386, #11718, #26339, #40900, #35521, #1135, #4473, #23440, #4971, #12902, #41130, #41367, #19597, #8805, #8567, #19828, #26575, #5204, #34456, #19351, #1605, #12433, #16255, #44737, #16488, #30890 ) ),
 .UNSPECIFIED., .F., .F., .T. ) 
 B_SPLINE_SURFACE_WITH_KNOTS ( ( 2, 1, 2 ),
 ( 3, 2, 2, 2, 2, 2, 2, 2, 2, 2, 2, 2, 2, 2, 2, 2, 2, 2, 2, 2, 2, 2, 2, 2, 2, 2, 2, 2, 2, 2, 2, 2, 2, 2, 2, 2, 2, 2, 2, 2, 2, 2, 2, 2, 2, 2, 2, 2, 2, 2, 2, 2, 2, 2, 2, 2, 2, 2, 2, 2, 2, 2, 2, 2, 2, 2, 2, 2, 2, 2, 2, 2, 2, 2, 2, 2, 2, 2, 2, 2, 2, 2, 2, 2, 2, 2, 2, 2, 2, 2, 2, 2, 2, 2, 2, 2, 2, 2, 2, 2, 2, 2, 2, 2, 2, 2, 2, 2, 2, 2, 2, 2, 2, 2, 2, 2, 2, 2, 2, 2, 2, 2, 2, 2, 2, 2, 2, 2, 2, 2, 2, 2, 2, 2, 2, 2, 2, 2, 2, 2, 2, 2, 2, 2, 2, 2, 2, 2, 2, 2, 2, 2, 2, 2, 2, 2, 2, 2, 2, 2, 2, 2, 2, 2, 2, 2, 2, 2, 2, 2, 2, 2, 2, 2, 2, 2, 2, 2, 2, 2, 2, 2, 2, 2, 2, 2, 2, 2, 2, 2, 2, 2, 2, 2, 2, 2, 2, 2, 2, 2, 2, 2, 2, 2, 2, 2, 2, 2, 2, 2, 2, 2, 2, 2, 2, 2, 2, 2, 2, 2, 2, 2, 2, 2, 2, 2, 2, 2, 2, 2, 2, 2, 2, 2, 2, 2, 2, 2, 2, 2, 2, 2, 2, 2, 2, 2, 2, 2, 2, 2, 2, 2, 2, 2, 2, 2, 2, 2, 2, 2, 2, 2, 2, 2, 2, 2, 2, 2, 2, 2, 2, 2, 2, 2, 2, 2, 2, 2, 2, 2, 2, 2, 2, 2, 2, 2, 2, 2, 2, 2, 2, 2, 2, 2, 2, 2, 2, 2, 2, 2, 2, 2, 2, 2, 2, 2, 2, 2, 2, 2, 2, 2, 2, 2, 2, 2, 2, 2, 2, 2, 2, 2, 2, 2, 2, 2, 2, 2, 2, 2, 2, 2, 2, 2, 2, 2, 2, 2, 2, 2, 2, 2, 2, 2, 2, 2, 2, 2, 2, 2, 2, 2, 2, 2, 2, 2, 2, 2, 2, 2, 2, 2, 2, 2, 2, 2, 2, 2, 2, 2, 2, 2, 2, 2, 2, 2, 2, 2, 2, 2, 2, 2, 2, 2, 2, 2, 2, 2, 2, 2, 2, 2, 2, 2, 2, 2, 2, 2, 2, 2, 3 ),
 ( 0.000000000000000000, 1.000000000000000000, 3.225190355106064999 ),
 ( 0.000000000000000000, 0.002500000000000000052, 0.005000000000000000104, 0.007499999999999999722, 0.01000000000000000021, 0.01250000000000000069, 0.01499999999999999944, 0.01750000000000000167, 0.02000000000000000042, 0.02249999999999999917, 0.02500000000000000139, 0.02750000000000000014, 0.02999999999999999889, 0.03250000000000000111, 0.03500000000000000333, 0.03749999999999999861, 0.04000000000000000083, 0.04250000000000000305, 0.04499999999999999833, 0.04750000000000000056, 0.05000000000000000278, 0.05249999999999999806, 0.05500000000000000028, 0.05750000000000000250, 0.05999999999999999778, 0.06250000000000000000, 0.06500000000000000222, 0.06750000000000000444, 0.07000000000000000666, 0.07249999999999999500, 0.07499999999999999722, 0.07749999999999999944, 0.08000000000000000167, 0.08250000000000000389, 0.08500000000000000611, 0.08749999999999999445, 0.08999999999999999667, 0.09249999999999999889, 0.09500000000000000111, 0.09750000000000000333, 0.1000000000000000056, 0.1024999999999999939, 0.1049999999999999961, 0.1074999999999999983, 0.1100000000000000006, 0.1125000000000000028, 0.1150000000000000050, 0.1174999999999999933, 0.1199999999999999956, 0.1224999999999999978, 0.1250000000000000000, 0.1275000000000000022, 0.1300000000000000044, 0.1325000000000000067, 0.1350000000000000089, 0.1375000000000000111, 0.1400000000000000133, 0.1424999999999999878, 0.1449999999999999900, 0.1474999999999999922, 0.1499999999999999944, 0.1524999999999999967, 0.1549999999999999989, 0.1575000000000000011, 0.1600000000000000033, 0.1625000000000000056, 0.1650000000000000078, 0.1675000000000000100, 0.1700000000000000122, 0.1724999999999999867, 0.1749999999999999889, 0.1774999999999999911, 0.1799999999999999933, 0.1824999999999999956, 0.1849999999999999978, 0.1875000000000000000, 0.1900000000000000022, 0.1925000000000000044, 0.1950000000000000067, 0.1975000000000000089, 0.2000000000000000111, 0.2025000000000000133, 0.2049999999999999878, 0.2074999999999999900, 0.2099999999999999922, 0.2124999999999999944, 0.2149999999999999967, 0.2174999999999999989, 0.2200000000000000011, 0.2225000000000000033, 0.2250000000000000056, 0.2275000000000000078, 0.2300000000000000100, 0.2325000000000000122, 0.2349999999999999867, 0.2374999999999999889, 0.2399999999999999911, 0.2424999999999999933, 0.2449999999999999956, 0.2474999999999999978, 0.2500000000000000000, 0.2525000000000000022, 0.2550000000000000044, 0.2575000000000000067, 0.2600000000000000089, 0.2625000000000000111, 0.2650000000000000133, 0.2675000000000000155, 0.2700000000000000178, 0.2725000000000000200, 0.2750000000000000222, 0.2775000000000000244, 0.2800000000000000266, 0.2824999999999999734, 0.2849999999999999756, 0.2874999999999999778, 0.2899999999999999800, 0.2924999999999999822, 0.2949999999999999845, 0.2974999999999999867, 0.2999999999999999889, 0.3024999999999999911, 0.3049999999999999933, 0.3074999999999999956, 0.3099999999999999978, 0.3125000000000000000, 0.3150000000000000022, 0.3175000000000000044, 0.3200000000000000067, 0.3225000000000000089, 0.3250000000000000111, 0.3275000000000000133, 0.3300000000000000155, 0.3325000000000000178, 0.3350000000000000200, 0.3375000000000000222, 0.3400000000000000244, 0.3425000000000000266, 0.3449999999999999734, 0.3474999999999999756, 0.3499999999999999778, 0.3524999999999999800, 0.3549999999999999822, 0.3574999999999999845, 0.3599999999999999867, 0.3624999999999999889, 0.3649999999999999911, 0.3674999999999999933, 0.3699999999999999956, 0.3724999999999999978, 0.3750000000000000000, 0.3775000000000000022, 0.3800000000000000044, 0.3825000000000000067, 0.3850000000000000089, 0.3875000000000000111, 0.3900000000000000133, 0.3925000000000000155, 0.3950000000000000178, 0.3975000000000000200, 0.4000000000000000222, 0.4025000000000000244, 0.4050000000000000266, 0.4074999999999999734, 0.4099999999999999756, 0.4124999999999999778, 0.4149999999999999800, 0.4174999999999999822, 0.4199999999999999845, 0.4224999999999999867, 0.4249999999999999889, 0.4274999999999999911, 0.4299999999999999933, 0.4324999999999999956, 0.4349999999999999978, 0.4375000000000000000, 0.4400000000000000022, 0.4425000000000000044, 0.4450000000000000067, 0.4475000000000000089, 0.4500000000000000111, 0.4525000000000000133, 0.4550000000000000155, 0.4575000000000000178, 0.4600000000000000200, 0.4625000000000000222, 0.4650000000000000244, 0.4675000000000000266, 0.4699999999999999734, 0.4724999999999999756, 0.4749999999999999778, 0.4774999999999999800, 0.4799999999999999822, 0.4824999999999999845, 0.4849999999999999867, 0.4874999999999999889, 0.4899999999999999911, 0.4924999999999999933, 0.4949999999999999956, 0.4974999999999999978, 0.5000000000000000000, 0.5024999999999999467, 0.5050000000000000044, 0.5074999999999999512, 0.5100000000000000089, 0.5124999999999999556, 0.5150000000000000133, 0.5174999999999999600, 0.5200000000000000178, 0.5224999999999999645, 0.5250000000000000222, 0.5274999999999999689, 0.5300000000000000266, 0.5324999999999999734, 0.5350000000000000311, 0.5374999999999999778, 0.5400000000000000355, 0.5424999999999999822, 0.5450000000000000400, 0.5474999999999999867, 0.5500000000000000444, 0.5524999999999999911, 0.5550000000000000488, 0.5574999999999999956, 0.5600000000000000533, 0.5625000000000000000, 0.5649999999999999467, 0.5675000000000000044, 0.5699999999999999512, 0.5725000000000000089, 0.5749999999999999556, 0.5775000000000000133, 0.5799999999999999600, 0.5825000000000000178, 0.5849999999999999645, 0.5875000000000000222, 0.5899999999999999689, 0.5925000000000000266, 0.5949999999999999734, 0.5975000000000000311, 0.5999999999999999778, 0.6025000000000000355, 0.6049999999999999822, 0.6075000000000000400, 0.6099999999999999867, 0.6125000000000000444, 0.6149999999999999911, 0.6175000000000000488, 0.6199999999999999956, 0.6225000000000000533, 0.6250000000000000000, 0.6274999999999999467, 0.6300000000000000044, 0.6324999999999999512, 0.6350000000000000089, 0.6374999999999999556, 0.6400000000000000133, 0.6424999999999999600, 0.6450000000000000178, 0.6474999999999999645, 0.6500000000000000222, 0.6524999999999999689, 0.6550000000000000266, 0.6574999999999999734, 0.6600000000000000311, 0.6624999999999999778, 0.6650000000000000355, 0.6674999999999999822, 0.6700000000000000400, 0.6724999999999999867, 0.6750000000000000444, 0.6774999999999999911, 0.6800000000000000488, 0.6824999999999999956, 0.6850000000000000533, 0.6875000000000000000, 0.6899999999999999467, 0.6925000000000000044, 0.6949999999999999512, 0.6975000000000000089, 0.6999999999999999556, 0.7025000000000000133, 0.7049999999999999600, 0.7075000000000000178, 0.7099999999999999645, 0.7125000000000000222, 0.7149999999999999689, 0.7175000000000000266, 0.7199999999999999734, 0.7225000000000000311, 0.7249999999999999778, 0.7275000000000000355, 0.7299999999999999822, 0.7325000000000000400, 0.7349999999999999867, 0.7375000000000000444, 0.7399999999999999911, 0.7425000000000000488, 0.7449999999999999956, 0.7475000000000000533, 0.7500000000000000000, 0.7524999999999999467, 0.7550000000000000044, 0.7574999999999999512, 0.7600000000000000089, 0.7624999999999999556, 0.7650000000000000133, 0.7674999999999999600, 0.7700000000000000178, 0.7724999999999999645, 0.7750000000000000222, 0.7774999999999999689, 0.7800000000000000266, 0.7824999999999999734, 0.7850000000000000311, 0.7874999999999999778, 0.7900000000000000355, 0.7924999999999999822, 0.7950000000000000400, 0.7974999999999999867, 0.8000000000000000444, 0.8024999999999999911, 0.8050000000000000488, 0.8074999999999999956, 0.8100000000000000533, 0.8125000000000000000, 0.8149999999999999467, 0.8175000000000000044, 0.8199999999999999512, 0.8225000000000000089, 0.8249999999999999556, 0.8275000000000000133, 0.8299999999999999600, 0.8325000000000000178, 0.8349999999999999645, 0.8375000000000000222, 0.8399999999999999689, 0.8425000000000000266, 0.8449999999999999734, 0.8475000000000000311, 0.8499999999999999778, 0.8525000000000000355, 0.8549999999999999822, 0.8575000000000000400, 0.8599999999999999867, 0.8625000000000000444, 0.8649999999999999911, 0.8675000000000000488, 0.8699999999999999956, 0.8725000000000000533, 0.8750000000000000000, 0.8774999999999999467, 0.8800000000000000044, 0.8824999999999999512, 0.8850000000000000089, 0.8874999999999999556, 0.8900000000000000133, 0.8924999999999999600, 0.8950000000000000178, 0.8974999999999999645, 0.9000000000000000222, 0.9024999999999999689, 0.9050000000000000266, 0.9074999999999999734, 0.9100000000000000311, 0.9124999999999999778, 0.9150000000000000355, 0.9174999999999999822, 0.9200000000000000400, 0.9224999999999999867, 0.9250000000000000444, 0.9274999999999999911, 0.9300000000000000488, 0.9324999999999999956, 0.9350000000000000533, 0.9375000000000000000, 0.9399999999999999467, 0.9425000000000000044, 0.9449999999999999512, 0.9475000000000000089, 0.9499999999999999556, 0.9525000000000000133, 0.9549999999999999600, 0.9575000000000000178, 0.9599999999999999645, 0.9625000000000000222, 0.9649999999999999689, 0.9675000000000000266, 0.9699999999999999734, 0.9725000000000000311, 0.9749999999999999778, 0.9775000000000000355, 0.9799999999999999822, 0.9825000000000000400, 0.9849999999999999867, 0.9875000000000000444, 0.9899999999999999911, 0.9925000000000000488, 0.9949999999999999956, 0.9975000000000000533, 1.000000000000000000 ),
 .UNSPECIFIED. ) 
 GEOMETRIC_REPRESENTATION_ITEM ( )  RATIONAL_B_SPLINE_SURFACE ( (
 ( 1.000000000000000000, 0.9238795325112869605, 1.000000000000000000, 0.9238795325112869605, 1.000000000000000000, 0.9238795325112869605, 1.000000000000000000, 0.9238795325112869605, 1.000000000000000000, 0.9238795325112869605, 1.000000000000000000, 0.9238795325112869605, 1.000000000000000000, 0.9238795325112869605, 1.000000000000000000, 0.9238795325112869605, 1.000000000000000000, 0.9238795325112869605, 1.000000000000000000, 0.9238795325112869605, 1.000000000000000000, 0.9238795325112869605, 1.000000000000000000, 0.9238795325112869605, 1.000000000000000000, 0.9238795325112869605, 1.000000000000000000, 0.9238795325112869605, 1.000000000000000000, 0.9238795325112869605, 1.000000000000000000, 0.9238795325112869605, 1.000000000000000000, 0.9238795325112869605, 1.000000000000000000, 0.9238795325112869605, 1.000000000000000000, 0.9238795325112869605, 1.000000000000000000, 0.9238795325112869605, 1.000000000000000000, 0.9238795325112869605, 1.000000000000000000, 0.9238795325112869605, 1.000000000000000000, 0.9238795325112869605, 1.000000000000000000, 0.9238795325112869605, 1.000000000000000000, 0.9238795325112869605, 1.000000000000000000, 0.9238795325112869605, 1.000000000000000000, 0.9238795325112869605, 1.000000000000000000, 0.9238795325112869605, 1.000000000000000000, 0.9238795325112869605, 1.000000000000000000, 0.9238795325112869605, 1.000000000000000000, 0.9238795325112869605, 1.000000000000000000, 0.9238795325112869605, 1.000000000000000000, 0.9238795325112869605, 1.000000000000000000, 0.9238795325112869605, 1.000000000000000000, 0.9238795325112869605, 1.000000000000000000, 0.9238795325112869605, 1.000000000000000000, 0.9238795325112869605, 1.000000000000000000, 0.9238795325112869605, 1.000000000000000000, 0.9238795325112869605, 1.000000000000000000, 0.9238795325112869605, 1.000000000000000000, 0.9238795325112869605, 1.000000000000000000, 0.9238795325112869605, 1.000000000000000000, 0.9238795325112869605, 1.000000000000000000, 0.9238795325112869605, 1.000000000000000000, 0.9238795325112869605, 1.000000000000000000, 0.9238795325112869605, 1.000000000000000000, 0.9238795325112869605, 1.000000000000000000, 0.9238795325112869605, 1.000000000000000000, 0.9238795325112869605, 1.000000000000000000, 0.9238795325112869605, 1.000000000000000000, 0.9238795325112869605, 1.000000000000000000, 0.9238795325112869605, 1.000000000000000000, 0.9238795325112869605, 1.000000000000000000, 0.9238795325112869605, 1.000000000000000000, 0.9238795325112869605, 1.000000000000000000, 0.9238795325112869605, 1.000000000000000000, 0.9238795325112869605, 1.000000000000000000, 0.9238795325112869605, 1.000000000000000000, 0.9238795325112869605, 1.000000000000000000, 0.9238795325112869605, 1.000000000000000000, 0.9238795325112869605, 1.000000000000000000, 0.9238795325112869605, 1.000000000000000000, 0.9238795325112869605, 1.000000000000000000, 0.9238795325112869605, 1.000000000000000000, 0.9238795325112869605, 1.000000000000000000, 0.9238795325112869605, 1.000000000000000000, 0.9238795325112869605, 1.000000000000000000, 0.9238795325112869605, 1.000000000000000000, 0.9238795325112869605, 1.000000000000000000, 0.9238795325112869605, 1.000000000000000000, 0.9238795325112869605, 1.000000000000000000, 0.9238795325112869605, 1.000000000000000000, 0.9238795325112869605, 1.000000000000000000, 0.9238795325112869605, 1.000000000000000000, 0.9238795325112869605, 1.000000000000000000, 0.9238795325112869605, 1.000000000000000000, 0.9238795325112869605, 1.000000000000000000, 0.9238795325112869605, 1.000000000000000000, 0.9238795325112869605, 1.000000000000000000, 0.9238795325112869605, 1.000000000000000000, 0.9238795325112869605, 1.000000000000000000, 0.9238795325112869605, 1.000000000000000000, 0.9238795325112869605, 1.000000000000000000, 0.9238795325112869605, 1.000000000000000000, 0.9238795325112869605, 1.000000000000000000, 0.9238795325112869605, 1.000000000000000000, 0.9238795325112869605, 1.000000000000000000, 0.9238795325112869605, 1.000000000000000000, 0.9238795325112869605, 1.000000000000000000, 0.9238795325112869605, 1.000000000000000000, 0.9238795325112869605, 1.000000000000000000, 0.9238795325112869605, 1.000000000000000000, 0.9238795325112869605, 1.000000000000000000, 0.9238795325112869605, 1.000000000000000000, 0.9238795325112869605, 1.000000000000000000, 0.9238795325112869605, 1.000000000000000000, 0.9238795325112869605, 1.000000000000000000, 0.9238795325112869605, 1.000000000000000000, 0.9238795325112869605, 1.000000000000000000, 0.9238795325112869605, 1.000000000000000000, 0.9238795325112869605, 1.000000000000000000, 0.9238795325112869605, 1.000000000000000000, 0.9238795325112869605, 1.000000000000000000, 0.9238795325112869605, 1.000000000000000000, 0.9238795325112869605, 1.000000000000000000, 0.9238795325112869605, 1.000000000000000000, 0.9238795325112869605, 1.000000000000000000, 0.9238795325112869605, 1.000000000000000000, 0.9238795325112869605, 1.000000000000000000, 0.9238795325112869605, 1.000000000000000000, 0.9238795325112869605, 1.000000000000000000, 0.9238795325112869605, 1.000000000000000000, 0.9238795325112869605, 1.000000000000000000, 0.9238795325112869605, 1.000000000000000000, 0.9238795325112869605, 1.000000000000000000, 0.9238795325112869605, 1.000000000000000000, 0.9238795325112869605, 1.000000000000000000, 0.9238795325112869605, 1.000000000000000000, 0.9238795325112869605, 1.000000000000000000, 0.9238795325112869605, 1.000000000000000000, 0.9238795325112869605, 1.000000000000000000, 0.9238795325112869605, 1.000000000000000000, 0.9238795325112869605, 1.000000000000000000, 0.9238795325112869605, 1.000000000000000000, 0.9238795325112869605, 1.000000000000000000, 0.9238795325112869605, 1.000000000000000000, 0.9238795325112869605, 1.000000000000000000, 0.9238795325112869605, 1.000000000000000000, 0.9238795325112869605, 1.000000000000000000, 0.9238795325112869605, 1.000000000000000000, 0.9238795325112869605, 1.000000000000000000, 0.9238795325112869605, 1.000000000000000000, 0.9238795325112869605, 1.000000000000000000, 0.9238795325112869605, 1.000000000000000000, 0.9238795325112869605, 1.000000000000000000, 0.9238795325112869605, 1.000000000000000000, 0.9238795325112869605, 1.000000000000000000, 0.9238795325112869605, 1.000000000000000000, 0.9238795325112869605, 1.000000000000000000, 0.9238795325112869605, 1.000000000000000000, 0.9238795325112869605, 1.000000000000000000, 0.9238795325112869605, 1.000000000000000000, 0.9238795325112869605, 1.000000000000000000, 0.9238795325112869605, 1.000000000000000000, 0.9238795325112869605, 1.000000000000000000, 0.9238795325112869605, 1.000000000000000000, 0.9238795325112869605, 1.000000000000000000, 0.9238795325112869605, 1.000000000000000000, 0.9238795325112869605, 1.000000000000000000, 0.9238795325112869605, 1.000000000000000000, 0.9238795325112869605, 1.000000000000000000, 0.9238795325112869605, 1.000000000000000000, 0.9238795325112869605, 1.000000000000000000, 0.9238795325112869605, 1.000000000000000000, 0.9238795325112869605, 1.000000000000000000, 0.9238795325112869605, 1.000000000000000000, 0.9238795325112869605, 1.000000000000000000, 0.9238795325112869605, 1.000000000000000000, 0.9238795325112869605, 1.000000000000000000, 0.9238795325112869605, 1.000000000000000000, 0.9238795325112869605, 1.000000000000000000, 0.9238795325112869605, 1.000000000000000000, 0.9238795325112869605, 1.000000000000000000, 0.9238795325112869605, 1.000000000000000000, 0.9238795325112869605, 1.000000000000000000, 0.9238795325112869605, 1.000000000000000000, 0.9238795325112869605, 1.000000000000000000, 0.9238795325112869605, 1.000000000000000000, 0.9238795325112869605, 1.000000000000000000, 0.9238795325112869605, 1.000000000000000000, 0.9238795325112869605, 1.000000000000000000, 0.9238795325112869605, 1.000000000000000000, 0.9238795325112869605, 1.000000000000000000, 0.9238795325112869605, 1.000000000000000000, 0.9238795325112869605, 1.000000000000000000, 0.9238795325112869605, 1.000000000000000000, 0.9238795325112869605, 1.000000000000000000, 0.9238795325112869605, 1.000000000000000000, 0.9238795325112869605, 1.000000000000000000, 0.9238795325112869605, 1.000000000000000000, 0.9238795325112869605, 1.000000000000000000, 0.9238795325112869605, 1.000000000000000000, 0.9238795325112869605, 1.000000000000000000, 0.9238795325112869605, 1.000000000000000000, 0.9238795325112869605, 1.000000000000000000, 0.9238795325112869605, 1.000000000000000000, 0.9238795325112869605, 1.000000000000000000, 0.9238795325112869605, 1.000000000000000000, 0.9238795325112869605, 1.000000000000000000, 0.9238795325112869605, 1.000000000000000000, 0.9238795325112869605, 1.000000000000000000, 0.9238795325112869605, 1.000000000000000000, 0.9238795325112869605, 1.000000000000000000, 0.9238795325112869605, 1.000000000000000000, 0.9238795325112869605, 1.000000000000000000, 0.9238795325112869605, 1.000000000000000000, 0.9238795325112869605, 1.000000000000000000, 0.9238795325112869605, 1.000000000000000000, 0.9238795325112869605, 1.000000000000000000, 0.9238795325112869605, 1.000000000000000000, 0.9238795325112869605, 1.000000000000000000, 0.9238795325112869605, 1.000000000000000000, 0.9238795325112869605, 1.000000000000000000, 0.9238795325112869605, 1.000000000000000000, 0.9238795325112869605, 1.000000000000000000, 0.9238795325112869605, 1.000000000000000000, 0.9238795325112869605, 1.000000000000000000, 0.9238795325112869605, 1.000000000000000000, 0.9238795325112869605, 1.000000000000000000, 0.9238795325112869605, 1.000000000000000000, 0.9238795325112869605, 1.000000000000000000, 0.9238795325112869605, 1.000000000000000000, 0.9238795325112869605, 1.000000000000000000, 0.9238795325112869605, 1.000000000000000000, 0.9238795325112869605, 1.000000000000000000, 0.9238795325112869605, 1.000000000000000000, 0.9238795325112869605, 1.000000000000000000, 0.9238795325112869605, 1.000000000000000000, 0.9238795325112869605, 1.000000000000000000, 0.9238795325112869605, 1.000000000000000000, 0.9238795325112869605, 1.000000000000000000, 0.9238795325112869605, 1.000000000000000000, 0.9238795325112869605, 1.000000000000000000, 0.9238795325112869605, 1.000000000000000000, 0.9238795325112869605, 1.000000000000000000, 0.9238795325112869605, 1.000000000000000000, 0.9238795325112869605, 1.000000000000000000, 0.9238795325112869605, 1.000000000000000000, 0.9238795325112869605, 1.000000000000000000, 0.9238795325112869605, 1.000000000000000000, 0.9238795325112869605, 1.000000000000000000, 0.9238795325112869605, 1.000000000000000000, 0.9238795325112869605, 1.000000000000000000, 0.9238795325112869605, 1.000000000000000000, 0.9238795325112869605, 1.000000000000000000, 0.9238795325112869605, 1.000000000000000000, 0.9238795325112869605, 1.000000000000000000, 0.9238795325112869605, 1.000000000000000000, 0.9238795325112869605, 1.000000000000000000, 0.9238795325112869605, 1.000000000000000000, 0.9238795325112869605, 1.000000000000000000, 0.9238795325112869605, 1.000000000000000000, 0.9238795325112869605, 1.000000000000000000, 0.9238795325112869605, 1.000000000000000000, 0.9238795325112869605, 1.000000000000000000, 0.9238795325112869605, 1.000000000000000000, 0.9238795325112869605, 1.000000000000000000, 0.9238795325112869605, 1.000000000000000000, 0.9238795325112869605, 1.000000000000000000, 0.9238795325112869605, 1.000000000000000000, 0.9238795325112869605, 1.000000000000000000, 0.9238795325112869605, 1.000000000000000000, 0.9238795325112869605, 1.000000000000000000, 0.9238795325112869605, 1.000000000000000000, 0.9238795325112869605, 1.000000000000000000, 0.9238795325112869605, 1.000000000000000000, 0.9238795325112869605, 1.000000000000000000, 0.9238795325112869605, 1.000000000000000000, 0.9238795325112869605, 1.000000000000000000, 0.9238795325112869605, 1.000000000000000000, 0.9238795325112869605, 1.000000000000000000, 0.9238795325112869605, 1.000000000000000000, 0.9238795325112869605, 1.000000000000000000, 0.9238795325112869605, 1.000000000000000000, 0.9238795325112869605, 1.000000000000000000, 0.9238795325112869605, 1.000000000000000000, 0.9238795325112869605, 1.000000000000000000, 0.9238795325112869605, 1.000000000000000000, 0.9238795325112869605, 1.000000000000000000, 0.9238795325112869605, 1.000000000000000000, 0.9238795325112869605, 1.000000000000000000, 0.9238795325112869605, 1.000000000000000000, 0.9238795325112869605, 1.000000000000000000, 0.9238795325112869605, 1.000000000000000000, 0.9238795325112869605, 1.000000000000000000, 0.9238795325112869605, 1.000000000000000000, 0.9238795325112869605, 1.000000000000000000, 0.9238795325112869605, 1.000000000000000000, 0.9238795325112869605, 1.000000000000000000, 0.9238795325112869605, 1.000000000000000000, 0.9238795325112869605, 1.000000000000000000, 0.9238795325112869605, 1.000000000000000000, 0.9238795325112869605, 1.000000000000000000, 0.9238795325112869605, 1.000000000000000000, 0.9238795325112869605, 1.000000000000000000, 0.9238795325112869605, 1.000000000000000000, 0.9238795325112869605, 1.000000000000000000, 0.9238795325112869605, 1.000000000000000000, 0.9238795325112869605, 1.000000000000000000, 0.9238795325112869605, 1.000000000000000000, 0.9238795325112869605, 1.000000000000000000, 0.9238795325112869605, 1.000000000000000000, 0.9238795325112869605, 1.000000000000000000, 0.9238795325112869605, 1.000000000000000000, 0.9238795325112869605, 1.000000000000000000, 0.9238795325112869605, 1.000000000000000000, 0.9238795325112869605, 1.000000000000000000, 0.9238795325112869605, 1.000000000000000000, 0.9238795325112869605, 1.000000000000000000, 0.9238795325112869605, 1.000000000000000000, 0.9238795325112869605, 1.000000000000000000, 0.9238795325112869605, 1.000000000000000000, 0.9238795325112869605, 1.000000000000000000, 0.9238795325112869605, 1.000000000000000000, 0.9238795325112869605, 1.000000000000000000, 0.9238795325112869605, 1.000000000000000000, 0.9238795325112869605, 1.000000000000000000, 0.9238795325112869605, 1.000000000000000000, 0.9238795325112869605, 1.000000000000000000, 0.9238795325112869605, 1.000000000000000000, 0.9238795325112869605, 1.000000000000000000, 0.9238795325112869605, 1.000000000000000000, 0.9238795325112869605, 1.000000000000000000, 0.9238795325112869605, 1.000000000000000000, 0.9238795325112869605, 1.000000000000000000, 0.9238795325112869605, 1.000000000000000000, 0.9238795325112869605, 1.000000000000000000, 0.9238795325112869605, 1.000000000000000000, 0.9238795325112869605, 1.000000000000000000, 0.9238795325112869605, 1.000000000000000000, 0.9238795325112869605, 1.000000000000000000, 0.9238795325112869605, 1.000000000000000000, 0.9238795325112869605, 1.000000000000000000, 0.9238795325112869605, 1.000000000000000000, 0.9238795325112869605, 1.000000000000000000, 0.9238795325112869605, 1.000000000000000000, 0.9238795325112869605, 1.000000000000000000, 0.9238795325112869605, 1.000000000000000000, 0.9238795325112869605, 1.000000000000000000, 0.9238795325112869605, 1.000000000000000000, 0.9238795325112869605, 1.000000000000000000, 0.9238795325112869605, 1.000000000000000000, 0.9238795325112869605, 1.000000000000000000, 0.9238795325112869605, 1.000000000000000000, 0.9238795325112869605, 1.000000000000000000, 0.9238795325112869605, 1.000000000000000000, 0.9238795325112869605, 1.000000000000000000, 0.9238795325112869605, 1.000000000000000000, 0.9238795325112869605, 1.000000000000000000, 0.9238795325112869605, 1.000000000000000000, 0.9238795325112869605, 1.000000000000000000, 0.9238795325112869605, 1.000000000000000000, 0.9238795325112869605, 1.000000000000000000, 0.9238795325112869605, 1.000000000000000000, 0.9238795325112869605, 1.000000000000000000, 0.9238795325112869605, 1.000000000000000000, 0.9238795325112869605, 1.000000000000000000, 0.9238795325112869605, 1.000000000000000000, 0.9238795325112869605, 1.000000000000000000, 0.9238795325112869605, 1.000000000000000000, 0.9238795325112869605, 1.000000000000000000, 0.9238795325112869605, 1.000000000000000000, 0.9238795325112869605, 1.000000000000000000, 0.9238795325112869605, 1.000000000000000000, 0.9238795325112869605, 1.000000000000000000, 0.9238795325112869605, 1.000000000000000000, 0.9238795325112869605, 1.000000000000000000, 0.9238795325112869605, 1.000000000000000000, 0.9238795325112869605, 1.000000000000000000, 0.9238795325112869605, 1.000000000000000000, 0.9238795325112869605, 1.000000000000000000, 0.9238795325112869605, 1.000000000000000000, 0.9238795325112869605, 1.000000000000000000, 0.9238795325112869605, 1.000000000000000000, 0.9238795325112869605, 1.000000000000000000, 0.9238795325112869605, 1.000000000000000000, 0.9238795325112869605, 1.000000000000000000, 0.9238795325112869605, 1.000000000000000000, 0.9238795325112869605, 1.000000000000000000, 0.9238795325112869605, 1.000000000000000000, 0.9238795325112869605, 1.000000000000000000, 0.9238795325112869605, 1.000000000000000000, 0.9238795325112869605, 1.000000000000000000, 0.9238795325112869605, 1.000000000000000000, 0.9238795325112869605, 1.000000000000000000, 0.9238795325112869605, 1.000000000000000000, 0.9238795325112869605, 1.000000000000000000, 0.9238795325112869605, 1.000000000000000000, 0.9238795325112869605, 1.000000000000000000, 0.9238795325112869605, 1.000000000000000000, 0.9238795325112869605, 1.000000000000000000, 0.9238795325112869605, 1.000000000000000000, 0.9238795325112869605, 1.000000000000000000, 0.9238795325112869605, 1.000000000000000000, 0.9238795325112869605, 1.000000000000000000, 0.9238795325112869605, 1.000000000000000000, 0.9238795325112869605, 1.000000000000000000, 0.9238795325112869605, 1.000000000000000000, 0.9238795325112869605, 1.000000000000000000, 0.9238795325112869605, 1.000000000000000000, 0.9238795325112869605, 1.000000000000000000, 0.9238795325112869605, 1.000000000000000000, 0.9238795325112869605, 1.000000000000000000, 0.9238795325112869605, 1.000000000000000000, 0.9238795325112869605, 1.000000000000000000, 0.9238795325112869605, 1.000000000000000000, 0.9238795325112869605, 1.000000000000000000, 0.9238795325112869605, 1.000000000000000000, 0.9238795325112869605, 1.000000000000000000, 0.9238795325112869605, 1.000000000000000000),
 ( 1.000000000000000000, 0.9238795325112869605, 1.000000000000000000, 0.9238795325112869605, 1.000000000000000000, 0.9238795325112869605, 1.000000000000000000, 0.9238795325112869605, 1.000000000000000000, 0.9238795325112869605, 1.000000000000000000, 0.9238795325112869605, 1.000000000000000000, 0.9238795325112869605, 1.000000000000000000, 0.9238795325112869605, 1.000000000000000000, 0.9238795325112869605, 1.000000000000000000, 0.9238795325112869605, 1.000000000000000000, 0.9238795325112869605, 1.000000000000000000, 0.9238795325112869605, 1.000000000000000000, 0.9238795325112869605, 1.000000000000000000, 0.9238795325112869605, 1.000000000000000000, 0.9238795325112869605, 1.000000000000000000, 0.9238795325112869605, 1.000000000000000000, 0.9238795325112869605, 1.000000000000000000, 0.9238795325112869605, 1.000000000000000000, 0.9238795325112869605, 1.000000000000000000, 0.9238795325112869605, 1.000000000000000000, 0.9238795325112869605, 1.000000000000000000, 0.9238795325112869605, 1.000000000000000000, 0.9238795325112869605, 1.000000000000000000, 0.9238795325112869605, 1.000000000000000000, 0.9238795325112869605, 1.000000000000000000, 0.9238795325112869605, 1.000000000000000000, 0.9238795325112869605, 1.000000000000000000, 0.9238795325112869605, 1.000000000000000000, 0.9238795325112869605, 1.000000000000000000, 0.9238795325112869605, 1.000000000000000000, 0.9238795325112869605, 1.000000000000000000, 0.9238795325112869605, 1.000000000000000000, 0.9238795325112869605, 1.000000000000000000, 0.9238795325112869605, 1.000000000000000000, 0.9238795325112869605, 1.000000000000000000, 0.9238795325112869605, 1.000000000000000000, 0.9238795325112869605, 1.000000000000000000, 0.9238795325112869605, 1.000000000000000000, 0.9238795325112869605, 1.000000000000000000, 0.9238795325112869605, 1.000000000000000000, 0.9238795325112869605, 1.000000000000000000, 0.9238795325112869605, 1.000000000000000000, 0.9238795325112869605, 1.000000000000000000, 0.9238795325112869605, 1.000000000000000000, 0.9238795325112869605, 1.000000000000000000, 0.9238795325112869605, 1.000000000000000000, 0.9238795325112869605, 1.000000000000000000, 0.9238795325112869605, 1.000000000000000000, 0.9238795325112869605, 1.000000000000000000, 0.9238795325112869605, 1.000000000000000000, 0.9238795325112869605, 1.000000000000000000, 0.9238795325112869605, 1.000000000000000000, 0.9238795325112869605, 1.000000000000000000, 0.9238795325112869605, 1.000000000000000000, 0.9238795325112869605, 1.000000000000000000, 0.9238795325112869605, 1.000000000000000000, 0.9238795325112869605, 1.000000000000000000, 0.9238795325112869605, 1.000000000000000000, 0.9238795325112869605, 1.000000000000000000, 0.9238795325112869605, 1.000000000000000000, 0.9238795325112869605, 1.000000000000000000, 0.9238795325112869605, 1.000000000000000000, 0.9238795325112869605, 1.000000000000000000, 0.9238795325112869605, 1.000000000000000000, 0.9238795325112869605, 1.000000000000000000, 0.9238795325112869605, 1.000000000000000000, 0.9238795325112869605, 1.000000000000000000, 0.9238795325112869605, 1.000000000000000000, 0.9238795325112869605, 1.000000000000000000, 0.9238795325112869605, 1.000000000000000000, 0.9238795325112869605, 1.000000000000000000, 0.9238795325112869605, 1.000000000000000000, 0.9238795325112869605, 1.000000000000000000, 0.9238795325112869605, 1.000000000000000000, 0.9238795325112869605, 1.000000000000000000, 0.9238795325112869605, 1.000000000000000000, 0.9238795325112869605, 1.000000000000000000, 0.9238795325112869605, 1.000000000000000000, 0.9238795325112869605, 1.000000000000000000, 0.9238795325112869605, 1.000000000000000000, 0.9238795325112869605, 1.000000000000000000, 0.9238795325112869605, 1.000000000000000000, 0.9238795325112869605, 1.000000000000000000, 0.9238795325112869605, 1.000000000000000000, 0.9238795325112869605, 1.000000000000000000, 0.9238795325112869605, 1.000000000000000000, 0.9238795325112869605, 1.000000000000000000, 0.9238795325112869605, 1.000000000000000000, 0.9238795325112869605, 1.000000000000000000, 0.9238795325112869605, 1.000000000000000000, 0.9238795325112869605, 1.000000000000000000, 0.9238795325112869605, 1.000000000000000000, 0.9238795325112869605, 1.000000000000000000, 0.9238795325112869605, 1.000000000000000000, 0.9238795325112869605, 1.000000000000000000, 0.9238795325112869605, 1.000000000000000000, 0.9238795325112869605, 1.000000000000000000, 0.9238795325112869605, 1.000000000000000000, 0.9238795325112869605, 1.000000000000000000, 0.9238795325112869605, 1.000000000000000000, 0.9238795325112869605, 1.000000000000000000, 0.9238795325112869605, 1.000000000000000000, 0.9238795325112869605, 1.000000000000000000, 0.9238795325112869605, 1.000000000000000000, 0.9238795325112869605, 1.000000000000000000, 0.9238795325112869605, 1.000000000000000000, 0.9238795325112869605, 1.000000000000000000, 0.9238795325112869605, 1.000000000000000000, 0.9238795325112869605, 1.000000000000000000, 0.9238795325112869605, 1.000000000000000000, 0.9238795325112869605, 1.000000000000000000, 0.9238795325112869605, 1.000000000000000000, 0.9238795325112869605, 1.000000000000000000, 0.9238795325112869605, 1.000000000000000000, 0.9238795325112869605, 1.000000000000000000, 0.9238795325112869605, 1.000000000000000000, 0.9238795325112869605, 1.000000000000000000, 0.9238795325112869605, 1.000000000000000000, 0.9238795325112869605, 1.000000000000000000, 0.9238795325112869605, 1.000000000000000000, 0.9238795325112869605, 1.000000000000000000, 0.9238795325112869605, 1.000000000000000000, 0.9238795325112869605, 1.000000000000000000, 0.9238795325112869605, 1.000000000000000000, 0.9238795325112869605, 1.000000000000000000, 0.9238795325112869605, 1.000000000000000000, 0.9238795325112869605, 1.000000000000000000, 0.9238795325112869605, 1.000000000000000000, 0.9238795325112869605, 1.000000000000000000, 0.9238795325112869605, 1.000000000000000000, 0.9238795325112869605, 1.000000000000000000, 0.9238795325112869605, 1.000000000000000000, 0.9238795325112869605, 1.000000000000000000, 0.9238795325112869605, 1.000000000000000000, 0.9238795325112869605, 1.000000000000000000, 0.9238795325112869605, 1.000000000000000000, 0.9238795325112869605, 1.000000000000000000, 0.9238795325112869605, 1.000000000000000000, 0.9238795325112869605, 1.000000000000000000, 0.9238795325112869605, 1.000000000000000000, 0.9238795325112869605, 1.000000000000000000, 0.9238795325112869605, 1.000000000000000000, 0.9238795325112869605, 1.000000000000000000, 0.9238795325112869605, 1.000000000000000000, 0.9238795325112869605, 1.000000000000000000, 0.9238795325112869605, 1.000000000000000000, 0.9238795325112869605, 1.000000000000000000, 0.9238795325112869605, 1.000000000000000000, 0.9238795325112869605, 1.000000000000000000, 0.9238795325112869605, 1.000000000000000000, 0.9238795325112869605, 1.000000000000000000, 0.9238795325112869605, 1.000000000000000000, 0.9238795325112869605, 1.000000000000000000, 0.9238795325112869605, 1.000000000000000000, 0.9238795325112869605, 1.000000000000000000, 0.9238795325112869605, 1.000000000000000000, 0.9238795325112869605, 1.000000000000000000, 0.9238795325112869605, 1.000000000000000000, 0.9238795325112869605, 1.000000000000000000, 0.9238795325112869605, 1.000000000000000000, 0.9238795325112869605, 1.000000000000000000, 0.9238795325112869605, 1.000000000000000000, 0.9238795325112869605, 1.000000000000000000, 0.9238795325112869605, 1.000000000000000000, 0.9238795325112869605, 1.000000000000000000, 0.9238795325112869605, 1.000000000000000000, 0.9238795325112869605, 1.000000000000000000, 0.9238795325112869605, 1.000000000000000000, 0.9238795325112869605, 1.000000000000000000, 0.9238795325112869605, 1.000000000000000000, 0.9238795325112869605, 1.000000000000000000, 0.9238795325112869605, 1.000000000000000000, 0.9238795325112869605, 1.000000000000000000, 0.9238795325112869605, 1.000000000000000000, 0.9238795325112869605, 1.000000000000000000, 0.9238795325112869605, 1.000000000000000000, 0.9238795325112869605, 1.000000000000000000, 0.9238795325112869605, 1.000000000000000000, 0.9238795325112869605, 1.000000000000000000, 0.9238795325112869605, 1.000000000000000000, 0.9238795325112869605, 1.000000000000000000, 0.9238795325112869605, 1.000000000000000000, 0.9238795325112869605, 1.000000000000000000, 0.9238795325112869605, 1.000000000000000000, 0.9238795325112869605, 1.000000000000000000, 0.9238795325112869605, 1.000000000000000000, 0.9238795325112869605, 1.000000000000000000, 0.9238795325112869605, 1.000000000000000000, 0.9238795325112869605, 1.000000000000000000, 0.9238795325112869605, 1.000000000000000000, 0.9238795325112869605, 1.000000000000000000, 0.9238795325112869605, 1.000000000000000000, 0.9238795325112869605, 1.000000000000000000, 0.9238795325112869605, 1.000000000000000000, 0.9238795325112869605, 1.000000000000000000, 0.9238795325112869605, 1.000000000000000000, 0.9238795325112869605, 1.000000000000000000, 0.9238795325112869605, 1.000000000000000000, 0.9238795325112869605, 1.000000000000000000, 0.9238795325112869605, 1.000000000000000000, 0.9238795325112869605, 1.000000000000000000, 0.9238795325112869605, 1.000000000000000000, 0.9238795325112869605, 1.000000000000000000, 0.9238795325112869605, 1.000000000000000000, 0.9238795325112869605, 1.000000000000000000, 0.9238795325112869605, 1.000000000000000000, 0.9238795325112869605, 1.000000000000000000, 0.9238795325112869605, 1.000000000000000000, 0.9238795325112869605, 1.000000000000000000, 0.9238795325112869605, 1.000000000000000000, 0.9238795325112869605, 1.000000000000000000, 0.9238795325112869605, 1.000000000000000000, 0.9238795325112869605, 1.000000000000000000, 0.9238795325112869605, 1.000000000000000000, 0.9238795325112869605, 1.000000000000000000, 0.9238795325112869605, 1.000000000000000000, 0.9238795325112869605, 1.000000000000000000, 0.9238795325112869605, 1.000000000000000000, 0.9238795325112869605, 1.000000000000000000, 0.9238795325112869605, 1.000000000000000000, 0.9238795325112869605, 1.000000000000000000, 0.9238795325112869605, 1.000000000000000000, 0.9238795325112869605, 1.000000000000000000, 0.9238795325112869605, 1.000000000000000000, 0.9238795325112869605, 1.000000000000000000, 0.9238795325112869605, 1.000000000000000000, 0.9238795325112869605, 1.000000000000000000, 0.9238795325112869605, 1.000000000000000000, 0.9238795325112869605, 1.000000000000000000, 0.9238795325112869605, 1.000000000000000000, 0.9238795325112869605, 1.000000000000000000, 0.9238795325112869605, 1.000000000000000000, 0.9238795325112869605, 1.000000000000000000, 0.9238795325112869605, 1.000000000000000000, 0.9238795325112869605, 1.000000000000000000, 0.9238795325112869605, 1.000000000000000000, 0.9238795325112869605, 1.000000000000000000, 0.9238795325112869605, 1.000000000000000000, 0.9238795325112869605, 1.000000000000000000, 0.9238795325112869605, 1.000000000000000000, 0.9238795325112869605, 1.000000000000000000, 0.9238795325112869605, 1.000000000000000000, 0.9238795325112869605, 1.000000000000000000, 0.9238795325112869605, 1.000000000000000000, 0.9238795325112869605, 1.000000000000000000, 0.9238795325112869605, 1.000000000000000000, 0.9238795325112869605, 1.000000000000000000, 0.9238795325112869605, 1.000000000000000000, 0.9238795325112869605, 1.000000000000000000, 0.9238795325112869605, 1.000000000000000000, 0.9238795325112869605, 1.000000000000000000, 0.9238795325112869605, 1.000000000000000000, 0.9238795325112869605, 1.000000000000000000, 0.9238795325112869605, 1.000000000000000000, 0.9238795325112869605, 1.000000000000000000, 0.9238795325112869605, 1.000000000000000000, 0.9238795325112869605, 1.000000000000000000, 0.9238795325112869605, 1.000000000000000000, 0.9238795325112869605, 1.000000000000000000, 0.9238795325112869605, 1.000000000000000000, 0.9238795325112869605, 1.000000000000000000, 0.9238795325112869605, 1.000000000000000000, 0.9238795325112869605, 1.000000000000000000, 0.9238795325112869605, 1.000000000000000000, 0.9238795325112869605, 1.000000000000000000, 0.9238795325112869605, 1.000000000000000000, 0.9238795325112869605, 1.000000000000000000, 0.9238795325112869605, 1.000000000000000000, 0.9238795325112869605, 1.000000000000000000, 0.9238795325112869605, 1.000000000000000000, 0.9238795325112869605, 1.000000000000000000, 0.9238795325112869605, 1.000000000000000000, 0.9238795325112869605, 1.000000000000000000, 0.9238795325112869605, 1.000000000000000000, 0.9238795325112869605, 1.000000000000000000, 0.9238795325112869605, 1.000000000000000000, 0.9238795325112869605, 1.000000000000000000, 0.9238795325112869605, 1.000000000000000000, 0.9238795325112869605, 1.000000000000000000, 0.9238795325112869605, 1.000000000000000000, 0.9238795325112869605, 1.000000000000000000, 0.9238795325112869605, 1.000000000000000000, 0.9238795325112869605, 1.000000000000000000, 0.9238795325112869605, 1.000000000000000000, 0.9238795325112869605, 1.000000000000000000, 0.9238795325112869605, 1.000000000000000000, 0.9238795325112869605, 1.000000000000000000, 0.9238795325112869605, 1.000000000000000000, 0.9238795325112869605, 1.000000000000000000, 0.9238795325112869605, 1.000000000000000000, 0.9238795325112869605, 1.000000000000000000, 0.9238795325112869605, 1.000000000000000000, 0.9238795325112869605, 1.000000000000000000, 0.9238795325112869605, 1.000000000000000000, 0.9238795325112869605, 1.000000000000000000, 0.9238795325112869605, 1.000000000000000000, 0.9238795325112869605, 1.000000000000000000, 0.9238795325112869605, 1.000000000000000000, 0.9238795325112869605, 1.000000000000000000, 0.9238795325112869605, 1.000000000000000000, 0.9238795325112869605, 1.000000000000000000, 0.9238795325112869605, 1.000000000000000000, 0.9238795325112869605, 1.000000000000000000, 0.9238795325112869605, 1.000000000000000000, 0.9238795325112869605, 1.000000000000000000, 0.9238795325112869605, 1.000000000000000000, 0.9238795325112869605, 1.000000000000000000, 0.9238795325112869605, 1.000000000000000000, 0.9238795325112869605, 1.000000000000000000, 0.9238795325112869605, 1.000000000000000000, 0.9238795325112869605, 1.000000000000000000, 0.9238795325112869605, 1.000000000000000000, 0.9238795325112869605, 1.000000000000000000, 0.9238795325112869605, 1.000000000000000000, 0.9238795325112869605, 1.000000000000000000, 0.9238795325112869605, 1.000000000000000000, 0.9238795325112869605, 1.000000000000000000, 0.9238795325112869605, 1.000000000000000000, 0.9238795325112869605, 1.000000000000000000, 0.9238795325112869605, 1.000000000000000000, 0.9238795325112869605, 1.000000000000000000, 0.9238795325112869605, 1.000000000000000000, 0.9238795325112869605, 1.000000000000000000, 0.9238795325112869605, 1.000000000000000000, 0.9238795325112869605, 1.000000000000000000, 0.9238795325112869605, 1.000000000000000000, 0.9238795325112869605, 1.000000000000000000, 0.9238795325112869605, 1.000000000000000000, 0.9238795325112869605, 1.000000000000000000, 0.9238795325112869605, 1.000000000000000000, 0.9238795325112869605, 1.000000000000000000, 0.9238795325112869605, 1.000000000000000000, 0.9238795325112869605, 1.000000000000000000, 0.9238795325112869605, 1.000000000000000000, 0.9238795325112869605, 1.000000000000000000, 0.9238795325112869605, 1.000000000000000000, 0.9238795325112869605, 1.000000000000000000, 0.9238795325112869605, 1.000000000000000000, 0.9238795325112869605, 1.000000000000000000, 0.9238795325112869605, 1.000000000000000000, 0.9238795325112869605, 1.000000000000000000, 0.9238795325112869605, 1.000000000000000000, 0.9238795325112869605, 1.000000000000000000, 0.9238795325112869605, 1.000000000000000000, 0.9238795325112869605, 1.000000000000000000, 0.9238795325112869605, 1.000000000000000000, 0.9238795325112869605, 1.000000000000000000, 0.9238795325112869605, 1.000000000000000000, 0.9238795325112869605, 1.000000000000000000, 0.9238795325112869605, 1.000000000000000000, 0.9238795325112869605, 1.000000000000000000, 0.9238795325112869605, 1.000000000000000000, 0.9238795325112869605, 1.000000000000000000, 0.9238795325112869605, 1.000000000000000000, 0.9238795325112869605, 1.000000000000000000, 0.9238795325112869605, 1.000000000000000000, 0.9238795325112869605, 1.000000000000000000, 0.9238795325112869605, 1.000000000000000000, 0.9238795325112869605, 1.000000000000000000, 0.9238795325112869605, 1.000000000000000000, 0.9238795325112869605, 1.000000000000000000, 0.9238795325112869605, 1.000000000000000000, 0.9238795325112869605, 1.000000000000000000, 0.9238795325112869605, 1.000000000000000000, 0.9238795325112869605, 1.000000000000000000, 0.9238795325112869605, 1.000000000000000000, 0.9238795325112869605, 1.000000000000000000, 0.9238795325112869605, 1.000000000000000000, 0.9238795325112869605, 1.000000000000000000, 0.9238795325112869605, 1.000000000000000000, 0.9238795325112869605, 1.000000000000000000, 0.9238795325112869605, 1.000000000000000000, 0.9238795325112869605, 1.000000000000000000, 0.9238795325112869605, 1.000000000000000000, 0.9238795325112869605, 1.000000000000000000, 0.9238795325112869605, 1.000000000000000000, 0.9238795325112869605, 1.000000000000000000, 0.9238795325112869605, 1.000000000000000000, 0.9238795325112869605, 1.000000000000000000, 0.9238795325112869605, 1.000000000000000000, 0.9238795325112869605, 1.000000000000000000, 0.9238795325112869605, 1.000000000000000000, 0.9238795325112869605, 1.000000000000000000, 0.9238795325112869605, 1.000000000000000000, 0.9238795325112869605, 1.000000000000000000, 0.9238795325112869605, 1.000000000000000000, 0.9238795325112869605, 1.000000000000000000, 0.9238795325112869605, 1.000000000000000000, 0.9238795325112869605, 1.000000000000000000, 0.9238795325112869605, 1.000000000000000000, 0.9238795325112869605, 1.000000000000000000, 0.9238795325112869605, 1.000000000000000000, 0.9238795325112869605, 1.000000000000000000, 0.9238795325112869605, 1.000000000000000000, 0.9238795325112869605, 1.000000000000000000, 0.9238795325112869605, 1.000000000000000000, 0.9238795325112869605, 1.000000000000000000, 0.9238795325112869605, 1.000000000000000000, 0.9238795325112869605, 1.000000000000000000, 0.9238795325112869605, 1.000000000000000000),
 ( 1.000000000000000000, 0.9238795325112869605, 1.000000000000000000, 0.9238795325112869605, 1.000000000000000000, 0.9238795325112869605, 1.000000000000000000, 0.9238795325112869605, 1.000000000000000000, 0.9238795325112869605, 1.000000000000000000, 0.9238795325112869605, 1.000000000000000000, 0.9238795325112869605, 1.000000000000000000, 0.9238795325112869605, 1.000000000000000000, 0.9238795325112869605, 1.000000000000000000, 0.9238795325112869605, 1.000000000000000000, 0.9238795325112869605, 1.000000000000000000, 0.9238795325112869605, 1.000000000000000000, 0.9238795325112869605, 1.000000000000000000, 0.9238795325112869605, 1.000000000000000000, 0.9238795325112869605, 1.000000000000000000, 0.9238795325112869605, 1.000000000000000000, 0.9238795325112869605, 1.000000000000000000, 0.9238795325112869605, 1.000000000000000000, 0.9238795325112869605, 1.000000000000000000, 0.9238795325112869605, 1.000000000000000000, 0.9238795325112869605, 1.000000000000000000, 0.9238795325112869605, 1.000000000000000000, 0.9238795325112869605, 1.000000000000000000, 0.9238795325112869605, 1.000000000000000000, 0.9238795325112869605, 1.000000000000000000, 0.9238795325112869605, 1.000000000000000000, 0.9238795325112869605, 1.000000000000000000, 0.9238795325112869605, 1.000000000000000000, 0.9238795325112869605, 1.000000000000000000, 0.9238795325112869605, 1.000000000000000000, 0.9238795325112869605, 1.000000000000000000, 0.9238795325112869605, 1.000000000000000000, 0.9238795325112869605, 1.000000000000000000, 0.9238795325112869605, 1.000000000000000000, 0.9238795325112869605, 1.000000000000000000, 0.9238795325112869605, 1.000000000000000000, 0.9238795325112869605, 1.000000000000000000, 0.9238795325112869605, 1.000000000000000000, 0.9238795325112869605, 1.000000000000000000, 0.9238795325112869605, 1.000000000000000000, 0.9238795325112869605, 1.000000000000000000, 0.9238795325112869605, 1.000000000000000000, 0.9238795325112869605, 1.000000000000000000, 0.9238795325112869605, 1.000000000000000000, 0.9238795325112869605, 1.000000000000000000, 0.9238795325112869605, 1.000000000000000000, 0.9238795325112869605, 1.000000000000000000, 0.9238795325112869605, 1.000000000000000000, 0.9238795325112869605, 1.000000000000000000, 0.9238795325112869605, 1.000000000000000000, 0.9238795325112869605, 1.000000000000000000, 0.9238795325112869605, 1.000000000000000000, 0.9238795325112869605, 1.000000000000000000, 0.9238795325112869605, 1.000000000000000000, 0.9238795325112869605, 1.000000000000000000, 0.9238795325112869605, 1.000000000000000000, 0.9238795325112869605, 1.000000000000000000, 0.9238795325112869605, 1.000000000000000000, 0.9238795325112869605, 1.000000000000000000, 0.9238795325112869605, 1.000000000000000000, 0.9238795325112869605, 1.000000000000000000, 0.9238795325112869605, 1.000000000000000000, 0.9238795325112869605, 1.000000000000000000, 0.9238795325112869605, 1.000000000000000000, 0.9238795325112869605, 1.000000000000000000, 0.9238795325112869605, 1.000000000000000000, 0.9238795325112869605, 1.000000000000000000, 0.9238795325112869605, 1.000000000000000000, 0.9238795325112869605, 1.000000000000000000, 0.9238795325112869605, 1.000000000000000000, 0.9238795325112869605, 1.000000000000000000, 0.9238795325112869605, 1.000000000000000000, 0.9238795325112869605, 1.000000000000000000, 0.9238795325112869605, 1.000000000000000000, 0.9238795325112869605, 1.000000000000000000, 0.9238795325112869605, 1.000000000000000000, 0.9238795325112869605, 1.000000000000000000, 0.9238795325112869605, 1.000000000000000000, 0.9238795325112869605, 1.000000000000000000, 0.9238795325112869605, 1.000000000000000000, 0.9238795325112869605, 1.000000000000000000, 0.9238795325112869605, 1.000000000000000000, 0.9238795325112869605, 1.000000000000000000, 0.9238795325112869605, 1.000000000000000000, 0.9238795325112869605, 1.000000000000000000, 0.9238795325112869605, 1.000000000000000000, 0.9238795325112869605, 1.000000000000000000, 0.9238795325112869605, 1.000000000000000000, 0.9238795325112869605, 1.000000000000000000, 0.9238795325112869605, 1.000000000000000000, 0.9238795325112869605, 1.000000000000000000, 0.9238795325112869605, 1.000000000000000000, 0.9238795325112869605, 1.000000000000000000, 0.9238795325112869605, 1.000000000000000000, 0.9238795325112869605, 1.000000000000000000, 0.9238795325112869605, 1.000000000000000000, 0.9238795325112869605, 1.000000000000000000, 0.9238795325112869605, 1.000000000000000000, 0.9238795325112869605, 1.000000000000000000, 0.9238795325112869605, 1.000000000000000000, 0.9238795325112869605, 1.000000000000000000, 0.9238795325112869605, 1.000000000000000000, 0.9238795325112869605, 1.000000000000000000, 0.9238795325112869605, 1.000000000000000000, 0.9238795325112869605, 1.000000000000000000, 0.9238795325112869605, 1.000000000000000000, 0.9238795325112869605, 1.000000000000000000, 0.9238795325112869605, 1.000000000000000000, 0.9238795325112869605, 1.000000000000000000, 0.9238795325112869605, 1.000000000000000000, 0.9238795325112869605, 1.000000000000000000, 0.9238795325112869605, 1.000000000000000000, 0.9238795325112869605, 1.000000000000000000, 0.9238795325112869605, 1.000000000000000000, 0.9238795325112869605, 1.000000000000000000, 0.9238795325112869605, 1.000000000000000000, 0.9238795325112869605, 1.000000000000000000, 0.9238795325112869605, 1.000000000000000000, 0.9238795325112869605, 1.000000000000000000, 0.9238795325112869605, 1.000000000000000000, 0.9238795325112869605, 1.000000000000000000, 0.9238795325112869605, 1.000000000000000000, 0.9238795325112869605, 1.000000000000000000, 0.9238795325112869605, 1.000000000000000000, 0.9238795325112869605, 1.000000000000000000, 0.9238795325112869605, 1.000000000000000000, 0.9238795325112869605, 1.000000000000000000, 0.9238795325112869605, 1.000000000000000000, 0.9238795325112869605, 1.000000000000000000, 0.9238795325112869605, 1.000000000000000000, 0.9238795325112869605, 1.000000000000000000, 0.9238795325112869605, 1.000000000000000000, 0.9238795325112869605, 1.000000000000000000, 0.9238795325112869605, 1.000000000000000000, 0.9238795325112869605, 1.000000000000000000, 0.9238795325112869605, 1.000000000000000000, 0.9238795325112869605, 1.000000000000000000, 0.9238795325112869605, 1.000000000000000000, 0.9238795325112869605, 1.000000000000000000, 0.9238795325112869605, 1.000000000000000000, 0.9238795325112869605, 1.000000000000000000, 0.9238795325112869605, 1.000000000000000000, 0.9238795325112869605, 1.000000000000000000, 0.9238795325112869605, 1.000000000000000000, 0.9238795325112869605, 1.000000000000000000, 0.9238795325112869605, 1.000000000000000000, 0.9238795325112869605, 1.000000000000000000, 0.9238795325112869605, 1.000000000000000000, 0.9238795325112869605, 1.000000000000000000, 0.9238795325112869605, 1.000000000000000000, 0.9238795325112869605, 1.000000000000000000, 0.9238795325112869605, 1.000000000000000000, 0.9238795325112869605, 1.000000000000000000, 0.9238795325112869605, 1.000000000000000000, 0.9238795325112869605, 1.000000000000000000, 0.9238795325112869605, 1.000000000000000000, 0.9238795325112869605, 1.000000000000000000, 0.9238795325112869605, 1.000000000000000000, 0.9238795325112869605, 1.000000000000000000, 0.9238795325112869605, 1.000000000000000000, 0.9238795325112869605, 1.000000000000000000, 0.9238795325112869605, 1.000000000000000000, 0.9238795325112869605, 1.000000000000000000, 0.9238795325112869605, 1.000000000000000000, 0.9238795325112869605, 1.000000000000000000, 0.9238795325112869605, 1.000000000000000000, 0.9238795325112869605, 1.000000000000000000, 0.9238795325112869605, 1.000000000000000000, 0.9238795325112869605, 1.000000000000000000, 0.9238795325112869605, 1.000000000000000000, 0.9238795325112869605, 1.000000000000000000, 0.9238795325112869605, 1.000000000000000000, 0.9238795325112869605, 1.000000000000000000, 0.9238795325112869605, 1.000000000000000000, 0.9238795325112869605, 1.000000000000000000, 0.9238795325112869605, 1.000000000000000000, 0.9238795325112869605, 1.000000000000000000, 0.9238795325112869605, 1.000000000000000000, 0.9238795325112869605, 1.000000000000000000, 0.9238795325112869605, 1.000000000000000000, 0.9238795325112869605, 1.000000000000000000, 0.9238795325112869605, 1.000000000000000000, 0.9238795325112869605, 1.000000000000000000, 0.9238795325112869605, 1.000000000000000000, 0.9238795325112869605, 1.000000000000000000, 0.9238795325112869605, 1.000000000000000000, 0.9238795325112869605, 1.000000000000000000, 0.9238795325112869605, 1.000000000000000000, 0.9238795325112869605, 1.000000000000000000, 0.9238795325112869605, 1.000000000000000000, 0.9238795325112869605, 1.000000000000000000, 0.9238795325112869605, 1.000000000000000000, 0.9238795325112869605, 1.000000000000000000, 0.9238795325112869605, 1.000000000000000000, 0.9238795325112869605, 1.000000000000000000, 0.9238795325112869605, 1.000000000000000000, 0.9238795325112869605, 1.000000000000000000, 0.9238795325112869605, 1.000000000000000000, 0.9238795325112869605, 1.000000000000000000, 0.9238795325112869605, 1.000000000000000000, 0.9238795325112869605, 1.000000000000000000, 0.9238795325112869605, 1.000000000000000000, 0.9238795325112869605, 1.000000000000000000, 0.9238795325112869605, 1.000000000000000000, 0.9238795325112869605, 1.000000000000000000, 0.9238795325112869605, 1.000000000000000000, 0.9238795325112869605, 1.000000000000000000, 0.9238795325112869605, 1.000000000000000000, 0.9238795325112869605, 1.000000000000000000, 0.9238795325112869605, 1.000000000000000000, 0.9238795325112869605, 1.000000000000000000, 0.9238795325112869605, 1.000000000000000000, 0.9238795325112869605, 1.000000000000000000, 0.9238795325112869605, 1.000000000000000000, 0.9238795325112869605, 1.000000000000000000, 0.9238795325112869605, 1.000000000000000000, 0.9238795325112869605, 1.000000000000000000, 0.9238795325112869605, 1.000000000000000000, 0.9238795325112869605, 1.000000000000000000, 0.9238795325112869605, 1.000000000000000000, 0.9238795325112869605, 1.000000000000000000, 0.9238795325112869605, 1.000000000000000000, 0.9238795325112869605, 1.000000000000000000, 0.9238795325112869605, 1.000000000000000000, 0.9238795325112869605, 1.000000000000000000, 0.9238795325112869605, 1.000000000000000000, 0.9238795325112869605, 1.000000000000000000, 0.9238795325112869605, 1.000000000000000000, 0.9238795325112869605, 1.000000000000000000, 0.9238795325112869605, 1.000000000000000000, 0.9238795325112869605, 1.000000000000000000, 0.9238795325112869605, 1.000000000000000000, 0.9238795325112869605, 1.000000000000000000, 0.9238795325112869605, 1.000000000000000000, 0.9238795325112869605, 1.000000000000000000, 0.9238795325112869605, 1.000000000000000000, 0.9238795325112869605, 1.000000000000000000, 0.9238795325112869605, 1.000000000000000000, 0.9238795325112869605, 1.000000000000000000, 0.9238795325112869605, 1.000000000000000000, 0.9238795325112869605, 1.000000000000000000, 0.9238795325112869605, 1.000000000000000000, 0.9238795325112869605, 1.000000000000000000, 0.9238795325112869605, 1.000000000000000000, 0.9238795325112869605, 1.000000000000000000, 0.9238795325112869605, 1.000000000000000000, 0.9238795325112869605, 1.000000000000000000, 0.9238795325112869605, 1.000000000000000000, 0.9238795325112869605, 1.000000000000000000, 0.9238795325112869605, 1.000000000000000000, 0.9238795325112869605, 1.000000000000000000, 0.9238795325112869605, 1.000000000000000000, 0.9238795325112869605, 1.000000000000000000, 0.9238795325112869605, 1.000000000000000000, 0.9238795325112869605, 1.000000000000000000, 0.9238795325112869605, 1.000000000000000000, 0.9238795325112869605, 1.000000000000000000, 0.9238795325112869605, 1.000000000000000000, 0.9238795325112869605, 1.000000000000000000, 0.9238795325112869605, 1.000000000000000000, 0.9238795325112869605, 1.000000000000000000, 0.9238795325112869605, 1.000000000000000000, 0.9238795325112869605, 1.000000000000000000, 0.9238795325112869605, 1.000000000000000000, 0.9238795325112869605, 1.000000000000000000, 0.9238795325112869605, 1.000000000000000000, 0.9238795325112869605, 1.000000000000000000, 0.9238795325112869605, 1.000000000000000000, 0.9238795325112869605, 1.000000000000000000, 0.9238795325112869605, 1.000000000000000000, 0.9238795325112869605, 1.000000000000000000, 0.9238795325112869605, 1.000000000000000000, 0.9238795325112869605, 1.000000000000000000, 0.9238795325112869605, 1.000000000000000000, 0.9238795325112869605, 1.000000000000000000, 0.9238795325112869605, 1.000000000000000000, 0.9238795325112869605, 1.000000000000000000, 0.9238795325112869605, 1.000000000000000000, 0.9238795325112869605, 1.000000000000000000, 0.9238795325112869605, 1.000000000000000000, 0.9238795325112869605, 1.000000000000000000, 0.9238795325112869605, 1.000000000000000000, 0.9238795325112869605, 1.000000000000000000, 0.9238795325112869605, 1.000000000000000000, 0.9238795325112869605, 1.000000000000000000, 0.9238795325112869605, 1.000000000000000000, 0.9238795325112869605, 1.000000000000000000, 0.9238795325112869605, 1.000000000000000000, 0.9238795325112869605, 1.000000000000000000, 0.9238795325112869605, 1.000000000000000000, 0.9238795325112869605, 1.000000000000000000, 0.9238795325112869605, 1.000000000000000000, 0.9238795325112869605, 1.000000000000000000, 0.9238795325112869605, 1.000000000000000000, 0.9238795325112869605, 1.000000000000000000, 0.9238795325112869605, 1.000000000000000000, 0.9238795325112869605, 1.000000000000000000, 0.9238795325112869605, 1.000000000000000000, 0.9238795325112869605, 1.000000000000000000, 0.9238795325112869605, 1.000000000000000000, 0.9238795325112869605, 1.000000000000000000, 0.9238795325112869605, 1.000000000000000000, 0.9238795325112869605, 1.000000000000000000, 0.9238795325112869605, 1.000000000000000000, 0.9238795325112869605, 1.000000000000000000, 0.9238795325112869605, 1.000000000000000000, 0.9238795325112869605, 1.000000000000000000, 0.9238795325112869605, 1.000000000000000000, 0.9238795325112869605, 1.000000000000000000, 0.9238795325112869605, 1.000000000000000000, 0.9238795325112869605, 1.000000000000000000, 0.9238795325112869605, 1.000000000000000000, 0.9238795325112869605, 1.000000000000000000, 0.9238795325112869605, 1.000000000000000000, 0.9238795325112869605, 1.000000000000000000, 0.9238795325112869605, 1.000000000000000000, 0.9238795325112869605, 1.000000000000000000, 0.9238795325112869605, 1.000000000000000000, 0.9238795325112869605, 1.000000000000000000, 0.9238795325112869605, 1.000000000000000000, 0.9238795325112869605, 1.000000000000000000, 0.9238795325112869605, 1.000000000000000000, 0.9238795325112869605, 1.000000000000000000, 0.9238795325112869605, 1.000000000000000000, 0.9238795325112869605, 1.000000000000000000, 0.9238795325112869605, 1.000000000000000000, 0.9238795325112869605, 1.000000000000000000, 0.9238795325112869605, 1.000000000000000000, 0.9238795325112869605, 1.000000000000000000, 0.9238795325112869605, 1.000000000000000000, 0.9238795325112869605, 1.000000000000000000, 0.9238795325112869605, 1.000000000000000000, 0.9238795325112869605, 1.000000000000000000, 0.9238795325112869605, 1.000000000000000000, 0.9238795325112869605, 1.000000000000000000, 0.9238795325112869605, 1.000000000000000000, 0.9238795325112869605, 1.000000000000000000, 0.9238795325112869605, 1.000000000000000000, 0.9238795325112869605, 1.000000000000000000, 0.9238795325112869605, 1.000000000000000000, 0.9238795325112869605, 1.000000000000000000, 0.9238795325112869605, 1.000000000000000000, 0.9238795325112869605, 1.000000000000000000, 0.9238795325112869605, 1.000000000000000000, 0.9238795325112869605, 1.000000000000000000, 0.9238795325112869605, 1.000000000000000000, 0.9238795325112869605, 1.000000000000000000, 0.9238795325112869605, 1.000000000000000000, 0.9238795325112869605, 1.000000000000000000, 0.9238795325112869605, 1.000000000000000000, 0.9238795325112869605, 1.000000000000000000, 0.9238795325112869605, 1.000000000000000000, 0.9238795325112869605, 1.000000000000000000, 0.9238795325112869605, 1.000000000000000000, 0.9238795325112869605, 1.000000000000000000, 0.9238795325112869605, 1.000000000000000000, 0.9238795325112869605, 1.000000000000000000, 0.9238795325112869605, 1.000000000000000000, 0.9238795325112869605, 1.000000000000000000, 0.9238795325112869605, 1.000000000000000000, 0.9238795325112869605, 1.000000000000000000, 0.9238795325112869605, 1.000000000000000000, 0.9238795325112869605, 1.000000000000000000, 0.9238795325112869605, 1.000000000000000000, 0.9238795325112869605, 1.000000000000000000, 0.9238795325112869605, 1.000000000000000000, 0.9238795325112869605, 1.000000000000000000, 0.9238795325112869605, 1.000000000000000000, 0.9238795325112869605, 1.000000000000000000, 0.9238795325112869605, 1.000000000000000000, 0.9238795325112869605, 1.000000000000000000, 0.9238795325112869605, 1.000000000000000000, 0.9238795325112869605, 1.000000000000000000, 0.9238795325112869605, 1.000000000000000000, 0.9238795325112869605, 1.000000000000000000, 0.9238795325112869605, 1.000000000000000000, 0.9238795325112869605, 1.000000000000000000, 0.9238795325112869605, 1.000000000000000000, 0.9238795325112869605, 1.000000000000000000, 0.9238795325112869605, 1.000000000000000000, 0.9238795325112869605, 1.000000000000000000, 0.9238795325112869605, 1.000000000000000000, 0.9238795325112869605, 1.000000000000000000, 0.9238795325112869605, 1.000000000000000000, 0.9238795325112869605, 1.000000000000000000, 0.9238795325112869605, 1.000000000000000000, 0.9238795325112869605, 1.000000000000000000, 0.9238795325112869605, 1.000000000000000000, 0.9238795325112869605, 1.000000000000000000, 0.9238795325112869605, 1.000000000000000000, 0.9238795325112869605, 1.000000000000000000, 0.9238795325112869605, 1.000000000000000000, 0.9238795325112869605, 1.000000000000000000, 0.9238795325112869605, 1.000000000000000000, 0.9238795325112869605, 1.000000000000000000, 0.9238795325112869605, 1.000000000000000000, 0.9238795325112869605, 1.000000000000000000, 0.9238795325112869605, 1.000000000000000000, 0.9238795325112869605, 1.000000000000000000, 0.9238795325112869605, 1.000000000000000000) ) ) 
 REPRESENTATION_ITEM ( '' )  SURFACE ( )  ) ;
#32302 = LINE ( 'NONE', #34942, #20764 ) ;
#32303 = VERTEX_POINT ( 'NONE', #20204 ) ;
#32304 = ADVANCED_FACE ( 'NONE', ( #31494 ), #29978, .T. ) ;
#32305 = CARTESIAN_POINT ( 'NONE',  ( -1.033464566929133799, 1.928577636452524610E-17, 2.869337061179095023E-17 ) ) ;
#32306 = CARTESIAN_POINT ( 'NONE',  ( -0.8107537697050254399, 0.1574803149606300301, 0.1304133857192446289 ) ) ;
#32307 = CARTESIAN_POINT ( 'NONE',  ( 0.1602931993194444682, 0.1591122789105269553, 0.000000000000000000 ) ) ;
#32308 = CARTESIAN_POINT ( 'NONE',  ( 0.1797182628040039365, -0.8474847544649350972, -2.200913952912460540E-17 ) ) ;
#32309 = CARTESIAN_POINT ( 'NONE',  ( 0.2471922904502826257, 0.07845432542752818483, 0.07637674237069280725 ) ) ;
#32310 = CARTESIAN_POINT ( 'NONE',  ( 1.002407869896990045, 0.1264236179284866091, 0.7012795275052913224 ) ) ;
#32311 = CARTESIAN_POINT ( 'NONE',  ( -0.06523048226347956391, -0.6254921259842515235, -0.1574803149606300301 ) ) ;
#32312 = CARTESIAN_POINT ( 'NONE',  ( -0.1596844025337534889, 0.1273093748619712751, 0.04123610460087424184 ) ) ;
#32313 = CARTESIAN_POINT ( 'NONE',  ( -0.2559055118110236116, 0.03676409477166151657, -0.03301314027812374957 ) ) ;
#32314 = AXIS2_PLACEMENT_3D ( 'NONE', #14436, #6752, #21374 ) ;
#32315 = CARTESIAN_POINT ( 'NONE',  ( 0.7185039370078739607, 1.928577636452523993E-17, 1.210629921259842590 ) ) ;
#32316 = CARTESIAN_POINT ( 'NONE',  ( 0.9496616949729309587, -0.1608514975889442644, 1.989539966078783806 ) ) ;
#32317 = CARTESIAN_POINT ( 'NONE',  ( 1.033464566929134687, -0.06523048226347956391, 1.739665354330709235 ) ) ;
#32318 = CARTESIAN_POINT ( 'NONE',  ( -0.1574803149606297803, -0.6451771652468047957, 0.06523048226347956391 ) ) ;
#32319 = VECTOR ( 'NONE', #13957, 39.37007874015748143 ) ;
#32320 = CARTESIAN_POINT ( 'NONE',  ( 1.002407869896990045, 0.1264236179284866091, 0.6569881889226141247 ) ) ;
#32321 = CARTESIAN_POINT ( 'NONE',  ( 1.033464566929133799, 1.928577636452524610E-17, 4.498031496062992574 ) ) ;
#32322 = CARTESIAN_POINT ( 'NONE',  ( -1.094772975963752103E-17, -0.6402559054580471143, -0.1787899950787401882 ) ) ;
#32323 = ORIENTED_EDGE ( 'NONE', *, *, #7379, .T. ) ;
#32324 = CARTESIAN_POINT ( 'NONE',  ( 0.7646288533564489232, -0.1113553986120547346, 0.6151574802074331050 ) ) ;
#32325 = FACE_OUTER_BOUND ( 'NONE', #6951, .T. ) ;
#32326 = CARTESIAN_POINT ( 'NONE',  ( 1.002407869896990045, -0.1264236179284866091, 0.9227362204186770889 ) ) ;
#32327 = ORIENTED_EDGE ( 'NONE', *, *, #7219, .T. ) ;
#32328 = CARTESIAN_POINT ( 'NONE',  ( 0.7646288533564489232, 0.1113553986120547346, 1.481299212598425230 ) ) ;
#32329 = CARTESIAN_POINT ( 'NONE',  ( -0.9873396505805591694, 0.1113553986120547346, 0.5265748031496062520 ) ) ;
#32330 = CARTESIAN_POINT ( 'NONE',  ( 0.1797182628040039087, 0.09985776522010414435, -0.07444174185955065859 ) ) ;
#32331 = CARTESIAN_POINT ( 'NONE',  ( -0.1264236179284866091, -1.073326771599779628, -0.1264236179284866091 ) ) ;
#32332 = CARTESIAN_POINT ( 'NONE',  ( -0.06523048226347956391, -1.452263779527559251, -0.1574803149606300301 ) ) ;
#32333 = DIRECTION ( 'NONE',  ( 1.822029033848725028E-16, 0.000000000000000000, 1.000000000000000000 ) ) ;
#32334 = EDGE_CURVE ( 'NONE', #23930, #8150, #20518, .T. ) ;
#32335 = VERTEX_POINT ( 'NONE', #13279 ) ;
#32336 = CARTESIAN_POINT ( 'NONE',  ( -0.9500414927467378812, -0.1787899950787401604, 0.1328740156942679607 ) ) ;
#32337 = CARTESIAN_POINT ( 'NONE',  ( 1.002407869896990045, -0.1264236179284866091, 1.990649606245448844 ) ) ;
#32338 = VERTEX_POINT ( 'NONE', #2698 ) ;
#32339 = CARTESIAN_POINT ( 'NONE',  ( -1.054774247047244096, 0.000000000000000000, 1.916830708607653477 ) ) ;
#32340 = CARTESIAN_POINT ( 'NONE',  ( -0.6971942568897648851, -0.07405724077823297447, 1.579724409395055318 ) ) ;
#32341 = CARTESIAN_POINT ( 'NONE',  ( 0.6971942568897648851, 0.07405724077823318263, 0.8316929133320636325 ) ) ;
#32342 = ADVANCED_FACE ( 'NONE', ( #27912 ), #9680, .T. ) ;
#32343 = CARTESIAN_POINT ( 'NONE',  ( -1.054774247047244096, 0.000000000000000000, 1.045767716481669440 ) ) ;
#32344 = CARTESIAN_POINT ( 'NONE',  ( -1.002407869896990045, -0.1264236179284866091, 0.3764763778989925203 ) ) ;
#32345 = CARTESIAN_POINT ( 'NONE',  ( -0.9873396505805591694, -0.1113553986120547346, 0.6742125984251968740 ) ) ;
#32346 = CARTESIAN_POINT ( 'NONE',  ( -0.8759842519685039353, 0.1787899950787401882, 1.847933070812378009 ) ) ;
#32347 = CARTESIAN_POINT ( 'NONE',  ( 0.1564216623530368111, -8.910440797025414093E-13, -0.1403857474672218497 ) ) ;
#32348 = CARTESIAN_POINT ( 'NONE',  ( -1.033464566929134687, -0.06523048226347956391, 1.897145669291339320 ) ) ;
#32349 = CARTESIAN_POINT ( 'NONE',  ( -0.8759842519685039353, 0.000000000000000000, 0.000000000000000000 ) ) ;
#32350 = CARTESIAN_POINT ( 'NONE',  ( -0.1787899950787401604, -0.2944153068119157446, -0.07405724077823318263 ) ) ;
#32351 = CARTESIAN_POINT ( 'NONE',  ( -0.1344623199169003858, -0.09842519685039370636, -0.1216788222333031466 ) ) ;
#32352 = DIRECTION ( 'NONE',  ( 0.000000000000000000, -1.000000000000000000, -0.000000000000000000 ) ) ;
#32353 = CARTESIAN_POINT ( 'NONE',  ( 0.7185039370078746268, -0.06523048226347956391, 1.045767716427905114 ) ) ;
#32354 = CARTESIAN_POINT ( 'NONE',  ( -1.002407869896990045, -0.1264236179284866091, 0.09596456687537027741 ) ) ;
#32355 = VECTOR ( 'NONE', #19279, 39.37007874015748143 ) ;
#32356 = ORIENTED_EDGE ( 'NONE', *, *, #6591, .T. ) ;
#32357 = ORIENTED_EDGE ( 'NONE', *, *, #30294, .F. ) ;
#32358 = CARTESIAN_POINT ( 'NONE',  ( -1.054774247047244540, -0.07405724077823318263, 1.284448818843874518 ) ) ;
#32359 = ORIENTED_EDGE ( 'NONE', *, *, #44668, .T. ) ;
#32360 = AXIS2_PLACEMENT_3D ( 'NONE', #23078, #1969, #12551 ) ;
#32361 = AXIS2_PLACEMENT_3D ( 'NONE', #29108, #9681, #42937 ) ;
#32362 = CARTESIAN_POINT ( 'NONE',  ( -1.094772975963752103E-17, -1.196358267662771757, -0.1787899950787401882 ) ) ;
#32363 = ADVANCED_FACE ( 'NONE', ( #10868 ), #35781, .T. ) ;
#32364 = CARTESIAN_POINT ( 'NONE',  ( -0.07405724077823318263, -1.346456692859623550, -0.1787899950787401604 ) ) ;
#32365 = CARTESIAN_POINT ( 'NONE',  ( -0.9412147342319837628, -0.1574803149606297803, 1.370570866034205748 ) ) ;
#32366 = CARTESIAN_POINT ( 'NONE',  ( 0.000000000000000000, 0.000000000000000000, 0.4921259842519685179 ) ) ;
#32367 = CARTESIAN_POINT ( 'NONE',  ( -0.9412147342319837628, -0.1574803149606297803, 0.7111220472440957785 ) ) ;
#32368 = CARTESIAN_POINT ( 'NONE',  ( 0.8759842519685039353, -0.1787899950787401882, 0.4109251967966299213 ) ) ;
#32369 = CARTESIAN_POINT ( 'NONE',  ( 2.892866454678787531E-17, -0.2145669291338582751, 0.1574803149606299191 ) ) ;
#32370 = CARTESIAN_POINT ( 'NONE',  ( 0.8759842519685039353, 0.1574803149606299191, 1.781496062884598164 ) ) ;
#32371 = VERTEX_POINT ( 'NONE', #13729 ) ;
#32372 = CARTESIAN_POINT ( 'NONE',  ( 0.1377952755905510751, 0.000000000000000000, -0.3149606299212598381 ) ) ;
#32373 = CARTESIAN_POINT ( 'NONE',  ( 0.7185039370078746268, 0.06523048226347956391, 0.8538385826771660581 ) ) ;
#32374 = CARTESIAN_POINT ( 'NONE',  ( 0.3000685424736224127, 4.466152701071653354E-17, 0.000000000000000000 ) ) ;
#32375 = CARTESIAN_POINT ( 'NONE',  ( 0.1574803149606299191, 0.000000000000000000, 2.731847993664263218E-16 ) ) ;
#32377 = CARTESIAN_POINT ( 'NONE',  ( 0.1579024634500865720, -0.1046578554684589463, -0.09958160468961345380 ) ) ;
#32376 = DIRECTION ( 'NONE',  ( 2.055777091826793380E-15, 0.6220299971367094782, -0.7829934116339072325 ) ) ;
#32378 = CARTESIAN_POINT ( 'NONE',  ( 0.9412147342319837628, 0.1574803149606300301, 0.1254921258767249526 ) ) ;
#32379 = ORIENTED_EDGE ( 'NONE', *, *, #19218, .T. ) ;
#32380 = CARTESIAN_POINT ( 'NONE',  ( -0.1264236179284866091, -0.07431102356828367395, 0.1264236179284866091 ) ) ;
#32381 = CARTESIAN_POINT ( 'NONE',  ( -0.8759842519685039353, -0.1574803149606299191, 0.6200787400499527813 ) ) ;
#32382 = CARTESIAN_POINT ( 'NONE',  ( -0.1574803149606297803, -1.471948818790110636, 0.06523048226347956391 ) ) ;
#32383 = CARTESIAN_POINT ( 'NONE',  ( 0.07405724077823318263, -0.5836614172690718361, 0.1787899950787401604 ) ) ;
#32384 = CARTESIAN_POINT ( 'NONE',  ( -0.1113553986120547346, -1.095472440944881942, -0.1113553986120547346 ) ) ;
#32385 = CARTESIAN_POINT ( 'NONE',  ( 0.7185039370078746268, 0.06523048226347956391, 0.9621062991050720603 ) ) ;
#32386 = CARTESIAN_POINT ( 'NONE',  ( 1.033464566929133799, 1.928577636452524610E-17, 4.498031496062992574 ) ) ;
#32387 = ADVANCED_FACE ( 'NONE', ( #35 ), #2442, .F. ) ;
#32388 = CARTESIAN_POINT ( 'NONE',  ( -0.8019270111902717657, 0.1787899950787401604, 0.4281496062454490659 ) ) ;
#32389 = VERTEX_POINT ( 'NONE', #4490 ) ;
#32390 = ORIENTED_EDGE ( 'NONE', *, *, #7103, .F. ) ;
#32391 = CARTESIAN_POINT ( 'NONE',  ( -0.6971942568897648851, -0.07405724077823297447, 1.663385826717890925 ) ) ;
#32392 = CARTESIAN_POINT ( 'NONE',  ( 0.9500414927467378812, 0.1787899950787401604, 1.609251968450173376 ) ) ;
#32393 = ORIENTED_EDGE ( 'NONE', *, *, #33052, .F. ) ;
#32394 = CARTESIAN_POINT ( 'NONE',  ( -0.8759842519685039353, -0.1787899950787401882, 0.7652559054580472253 ) ) ;
#32395 = CONICAL_SURFACE ( 'NONE', #35424, 0.1377952755905509641, 0.9599310885968941331 ) ;
#32396 = CARTESIAN_POINT ( 'NONE',  ( 1.054774247047244540, -0.07405724077823318263, 0.2214566928596220785 ) ) ;
#32397 = CARTESIAN_POINT ( 'NONE',  ( -0.7185039370078739607, 1.928577636452523993E-17, 1.673228346349165285 ) ) ;
#32398 = CARTESIAN_POINT ( 'NONE',  ( 0.9500414927467377701, -0.1787899950787401604, 0.7283464566391492090 ) ) ;
#32399 = CARTESIAN_POINT ( 'NONE',  ( -1.054774247047244540, -0.07405724077823318263, 0.6889763778989936860 ) ) ;
#32400 = ADVANCED_FACE ( 'NONE', ( #33317 ), #33077, .T. ) ;
#32401 = CARTESIAN_POINT ( 'NONE',  ( 0.7646288533564489232, 0.1113553986120547346, 0.9202755904436535905 ) ) ;
#32402 = CARTESIAN_POINT ( 'NONE',  ( 0.3727034120734909473, 4.616380251121755931E-17, 0.000000000000000000 ) ) ;
#32403 = CARTESIAN_POINT ( 'NONE',  ( -0.06523048226347956391, -0.2465551180027093781, 0.1574803149606297803 ) ) ;
#32404 = CARTESIAN_POINT ( 'NONE',  ( -0.7495606340400177148, -0.1264236179284866091, 1.429625984198204858 ) ) ;
#32405 = VERTEX_POINT ( 'NONE', #22491 ) ;
#32406 = CARTESIAN_POINT ( 'NONE',  ( -0.7185039370078739607, 1.928577636452523993E-17, 1.486220472440944906 ) ) ;
#32407 = CIRCLE ( 'NONE', #3258, 0.02900000000000062597 ) ;
#32408 = CARTESIAN_POINT ( 'NONE',  ( -1.033464566929134687, 0.06523048226347956391, 0.4060039370078741272 ) ) ;
#32409 = CARTESIAN_POINT ( 'NONE',  ( 0.6971942568897637749, 2.189545951927499583E-17, 1.424704724355685181 ) ) ;
#32410 = CARTESIAN_POINT ( 'NONE',  ( -0.7185039370078746268, 0.06523048226347956391, 0.3715551180027091283 ) ) ;
#32411 = VERTEX_POINT ( 'NONE', #29971 ) ;
#32412 = CARTESIAN_POINT ( 'NONE',  ( 0.1264236179284866091, -1.724041291063883818, -0.1264236179284866091 ) ) ;
#32413 = ORIENTED_EDGE ( 'NONE', *, *, #405, .F. ) ;
#32414 = ORIENTED_EDGE ( 'NONE', *, *, #29670, .T. ) ;
#32415 = CARTESIAN_POINT ( 'NONE',  ( 0.7495606340400177148, -0.1264236179284866091, 1.424704724355685181 ) ) ;
#32416 = CARTESIAN_POINT ( 'NONE',  ( 0.8070866141732283561, 0.000000000000000000, -0.7574803149606299524 ) ) ;
#32417 = CARTESIAN_POINT ( 'NONE',  ( -0.1264236179284866091, -0.4040354330171023745, -0.1264236179284866091 ) ) ;
#32418 = CARTESIAN_POINT ( 'NONE',  ( 0.1264236179284866091, -0.8912401574265511606, 0.1264236179284866091 ) ) ;
#32419 = AXIS2_PLACEMENT_3D ( 'NONE', #30209, #26591, #43461 ) ;
#32420 = CARTESIAN_POINT ( 'NONE',  ( -0.2471918495545273875, -0.09442133267706703803, -0.03395794428076703841 ) ) ;
#32421 = CARTESIAN_POINT ( 'NONE',  ( 0.000000000000000000, 0.000000000000000000, 0.000000000000000000 ) ) ;
#32422 = PRODUCT_DEFINITION_FORMATION_WITH_SPECIFIED_SOURCE ( 'ANY', '', #33371, .NOT_KNOWN. ) ;
#32423 = AXIS2_PLACEMENT_3D ( 'NONE', #31183, #4797, #19425 ) ;
#32424 = CARTESIAN_POINT ( 'NONE',  ( 0.07405724077823318263, -0.06803735405601045449, -0.1787899950787401604 ) ) ;
#32425 = CARTESIAN_POINT ( 'NONE',  ( -0.1264236179284866091, 0.02903543312462964626, -0.1264236179284866091 ) ) ;
#32426 = CARTESIAN_POINT ( 'NONE',  ( 0.2471922279627869479, -0.07692167320570084121, -0.07932652958025969425 ) ) ;
#32427 = CARTESIAN_POINT ( 'NONE',  ( 0.2519685039370078705, 4.616380251121755931E-17, 0.000000000000000000 ) ) ;
#32428 = CARTESIAN_POINT ( 'NONE',  ( 0.6971942568897626646, -0.07405724077823297447, 0.6742125983714335469 ) ) ;
#32429 = CARTESIAN_POINT ( 'NONE',  ( -1.054774247047244540, -0.07405724077823318263, 0.9301181101824563813 ) ) ;
#32431 = LINE ( 'NONE', #25214, #2514 ) ;
#32430 = CARTESIAN_POINT ( 'NONE',  ( -0.8720834684628424593, 0.1749638022103473245, 0.03937007874015842346 ) ) ;
#32432 = CARTESIAN_POINT ( 'NONE',  ( -0.1797182628040039087, -1.730850896197219768, 0.07444174185955065859 ) ) ;
#32433 = CARTESIAN_POINT ( 'NONE',  ( 0.1264236179284866091, -0.4483267715997795166, -0.1264236179284866091 ) ) ;
#32434 = CARTESIAN_POINT ( 'NONE',  ( -0.7185039370078739607, 1.928577636452523993E-17, 1.486220472440944906 ) ) ;
#32435 = CARTESIAN_POINT ( 'NONE',  ( 1.002407869896990045, 0.1264236179284866091, 1.685531496009228469 ) ) ;
#32437 = CARTESIAN_POINT ( 'NONE',  ( 0.1626913500575924709, 0.1599528086217352763, 1.449618227866108752E-08 ) ) ;
#32436 = DIRECTION ( 'NONE',  ( 0.000000000000000000, -1.000000000000000000, 0.000000000000000000 ) ) ;
#32438 = EDGE_CURVE ( 'NONE', #12102, #19774, #40451, .T. ) ;
#32439 = ORIENTED_EDGE ( 'NONE', *, *, #43868, .F. ) ;
#32440 = ORIENTED_EDGE ( 'NONE', *, *, #37498, .F. ) ;
#32441 = DIRECTION ( 'NONE',  ( -0.000000000000000000, 1.000000000000000000, -0.000000000000000000 ) ) ;
#32442 = CARTESIAN_POINT ( 'NONE',  ( 3.284318927891251994E-17, -0.1136811023084411398, 0.1787899950787401882 ) ) ;
#32443 = CARTESIAN_POINT ( 'NONE',  ( -0.8019270111902717657, 0.1787899950787401604, 0.3937007873478115538 ) ) ;
#32444 = CARTESIAN_POINT ( 'NONE',  ( 0.6971942568897637749, 2.189545951927499583E-17, 0.6717519684501732646 ) ) ;
#32445 = CARTESIAN_POINT ( 'NONE',  ( -0.07405724077823318263, -1.031496062938363822, -0.1787899950787401604 ) ) ;
#32446 = CARTESIAN_POINT ( 'NONE',  ( 0.6971942568897626646, -0.07405724077823297447, 0.1279527558517483676 ) ) ;
#32447 = ( BOUNDED_CURVE ( )  B_SPLINE_CURVE ( 2, ( #22321, #43414, #3414, #36007, #10863, #40049, #17794, #18030, #47019 ),
 .UNSPECIFIED., .F., .T. ) 
 B_SPLINE_CURVE_WITH_KNOTS ( ( 3, 2, 2, 2, 3 ),
 ( 0.6500000000000000222, 0.6524999999999999689, 0.6550000000000000266, 0.6574999999999999734, 0.6600000000000000311 ),
 .UNSPECIFIED. ) 
 CURVE ( )  GEOMETRIC_REPRESENTATION_ITEM ( )  RATIONAL_B_SPLINE_CURVE ( ( 1.000000000000000000, 0.9238795325112899581, 1.000000000000000000, 0.9238795325112869605, 1.000000000000000000, 0.9238795325112869605, 1.000000000000000000, 0.9238795325112869605, 1.000000000000000000 ) ) 
 REPRESENTATION_ITEM ( '' )  ) ;
#32448 = CARTESIAN_POINT ( 'NONE',  ( 0.3425196850393700809, 0.08090551181102362266, 9.908067607274841931E-18 ) ) ;
#32449 = CARTESIAN_POINT ( 'NONE',  ( 0.7495606340400177148, 0.1264236179284866091, 0.5880905511273386566 ) ) ;
#32450 = EDGE_CURVE ( 'NONE', #9930, #31834, #1633, .T. ) ;
#32451 = CARTESIAN_POINT ( 'NONE',  ( -0.6971942568897637749, 2.189545951927499583E-17, 1.616633858213952779 ) ) ;
#32452 = ORIENTED_EDGE ( 'NONE', *, *, #22234, .T. ) ;
#32453 = CARTESIAN_POINT ( 'NONE',  ( -0.6971942568897648851, 0.07405724077823318263, 1.107283464513165949 ) ) ;
#32454 = CARTESIAN_POINT ( 'NONE',  ( -0.2665235116888311495, -0.1584712422872020798, -0.9307722131276843225 ) ) ;
#32455 = CARTESIAN_POINT ( 'NONE',  ( 1.002407869896990045, 0.1264236179284866091, 1.173720472387181246 ) ) ;
#32456 = CARTESIAN_POINT ( 'NONE',  ( -0.7185039370078746268, -0.06523048226347956391, 0.6914370077664893088 ) ) ;
#32457 = CARTESIAN_POINT ( 'NONE',  ( 1.002407869896990045, 0.1264236179284866091, 1.877460629867496067 ) ) ;
#32458 = CARTESIAN_POINT ( 'NONE',  ( -1.033464566929134687, -0.06523048226347956391, 0.5979330708661413363 ) ) ;
#32459 = CARTESIAN_POINT ( 'NONE',  ( -0.8759842519685039353, 0.1787899950787401882, 0.9374999999462362288 ) ) ;
#32460 = CARTESIAN_POINT ( 'NONE',  ( -0.04877781748286048186, -0.2673323462081961810, -0.06129781628410210792 ) ) ;
#32461 = CARTESIAN_POINT ( 'NONE',  ( 0.8759842519685039353, 0.1787899950787401882, 0.2337598424659216578 ) ) ;
#32462 = CARTESIAN_POINT ( 'NONE',  ( -1.002407869896990045, 0.1264236179284866091, 0.2239173227808822775 ) ) ;
#32463 = ADVANCED_FACE ( 'NONE', ( #44520 ), #19128, .T. ) ;
#32464 = CARTESIAN_POINT ( 'NONE',  ( -0.7495606340400177148, 0.1264236179284866091, 0.7062007873478109987 ) ) ;
#32465 = CARTESIAN_POINT ( 'NONE',  ( 0.9873396505805591694, -0.1113553986120547346, 1.530511810916094451 ) ) ;
#32466 = ORIENTED_EDGE ( 'NONE', *, *, #24833, .T. ) ;
#32467 = CARTESIAN_POINT ( 'NONE',  ( 3.284318927891251994E-17, -0.07431102356828367395, 0.1787899950787401882 ) ) ;
#32468 = CARTESIAN_POINT ( 'NONE',  ( 0.8019270111902717657, -0.1787899950787401604, 0.7627952755367881643 ) ) ;
#32469 = CARTESIAN_POINT ( 'NONE',  ( 0.7495606340400177148, -0.1264236179284866091, 1.035925196796629866 ) ) ;
#32470 = CARTESIAN_POINT ( 'NONE',  ( -0.7495606340400177148, -0.1264236179284866091, 1.897145669237574772 ) ) ;
#32471 = ( BOUNDED_CURVE ( )  B_SPLINE_CURVE ( 2, ( #32397, #36917, #11056, #28565, #17508, #21579, #46974, #39546, #13918 ),
 .UNSPECIFIED., .F., .T. ) 
 B_SPLINE_CURVE_WITH_KNOTS ( ( 3, 2, 2, 2, 3 ),
 ( 0.8299999999999999600, 0.8325000000000000178, 0.8349999999999999645, 0.8375000000000000222, 0.8399999999999999689 ),
 .UNSPECIFIED. ) 
 CURVE ( )  GEOMETRIC_REPRESENTATION_ITEM ( )  RATIONAL_B_SPLINE_CURVE ( ( 1.000000000000000000, 0.9238795325112939549, 1.000000000000000000, 0.9238795325112869605, 1.000000000000000000, 0.9238795325112869605, 1.000000000000000000, 0.9238795325112869605, 1.000000000000000000 ) ) 
 REPRESENTATION_ITEM ( '' )  ) ;
#32472 = DIRECTION ( 'NONE',  ( -1.000000000000000000, 0.000000000000000000, 0.000000000000000000 ) ) ;
#32473 = CARTESIAN_POINT ( 'NONE',  ( 0.1787899950787401882, -1.295891684764671314, -2.189545951927503898E-17 ) ) ;
#32474 = VERTEX_POINT ( 'NONE', #42573 ) ;
#32475 = CARTESIAN_POINT ( 'NONE',  ( -0.1264236179284866091, -0.2810039369541106336, -0.1264236179284866091 ) ) ;
#32476 = ORIENTED_EDGE ( 'NONE', *, *, #29559, .F. ) ;
#32477 = CARTESIAN_POINT ( 'NONE',  ( 1.054774247047244540, 0.07405724077823318263, 1.087598425143086578 ) ) ;
#32478 = DIRECTION ( 'NONE',  ( 0.000000000000000000, 0.000000000000000000, 1.000000000000000000 ) ) ;
#32479 = CARTESIAN_POINT ( 'NONE',  ( -0.2471922763370260623, -0.09254788073167596885, 0.04110581524695881839 ) ) ;
#32480 = ADVANCED_BREP_SHAPE_REPRESENTATION ( 'Link Bar', ( #21111, #20860 ), #6323 ) ;
#32481 = CARTESIAN_POINT ( 'NONE',  ( 0.7646288533564489232, 0.1113553986120547346, 1.953740157480315043 ) ) ;
#32482 = CARTESIAN_POINT ( 'NONE',  ( 0.1264236179284866091, -1.634350393647023614, -0.1264236179284866091 ) ) ;
#32483 = CARTESIAN_POINT ( 'NONE',  ( -0.1264236179284866091, -0.7091535432533228045, 0.1264236179284866091 ) ) ;
#32484 = ADVANCED_FACE ( 'NONE', ( #12450, #30904 ), #34956, .T. ) ;
#32485 = CARTESIAN_POINT ( 'NONE',  ( -0.8019270111902716547, -0.1787899950787401604, 0.5265748030958428139 ) ) ;
#32486 = CARTESIAN_POINT ( 'NONE',  ( 0.1270800023317771588, -1.246106801709029321, 0.1270800023317771588 ) ) ;
#32487 = DIRECTION ( 'NONE',  ( 1.000000000000000000, 0.000000000000000000, -0.000000000000000000 ) ) ;
#32488 = CARTESIAN_POINT ( 'NONE',  ( 0.9500414927467378812, 0.1787899950787401604, 1.176181102308441417 ) ) ;
#32489 = CARTESIAN_POINT ( 'NONE',  ( 0.8019270111902716547, -0.1787899950787401604, 1.545275590497419138 ) ) ;
#32490 = EDGE_CURVE ( 'NONE', #22780, #3723, #5703, .T. ) ;
#32491 = CARTESIAN_POINT ( 'NONE',  ( 0.01628405332009578987, 0.1299212598425197041, 0.1749064654736346147 ) ) ;
#32492 = CARTESIAN_POINT ( 'NONE',  ( 0.1558461344925403669, 0.05538344815314961284, 0.1377952755905511861 ) ) ;
#32493 = CARTESIAN_POINT ( 'NONE',  ( 0.8759842519685039353, 0.000000000000000000, 4.498031496062992574 ) ) ;
#32494 = CARTESIAN_POINT ( 'NONE',  ( -0.9873396505805591694, 0.1113553986120547346, 1.737204724301921299 ) ) ;
#32495 = CARTESIAN_POINT ( 'NONE',  ( 0.8019270111902717657, 0.1787899950787401604, 0.1525590550643468046 ) ) ;
#32497 = DIRECTION ( 'NONE',  ( -0.000000000000000000, -1.000000000000000000, -0.000000000000000000 ) ) ;
#32496 = CARTESIAN_POINT ( 'NONE',  ( 1.054774247047244540, -0.07405724077823318263, 1.082677165300567346 ) ) ;
#32498 = CARTESIAN_POINT ( 'NONE',  ( 0.8107537697050253289, -0.1574803149606297803, 0.4601377951680635792 ) ) ;
#32499 = VERTEX_POINT ( 'NONE', #42353 ) ;
#32500 = VECTOR ( 'NONE', #10305, 39.37007874015748143 ) ;
#32501 = CARTESIAN_POINT ( 'NONE',  ( -0.7185039370078739607, 0.000000000000000000, -2.869337061179095023E-17 ) ) ;
#32502 = CARTESIAN_POINT ( 'NONE',  ( 0.9530870782177205403, 0.1508571639167848033, 0.03936674302998629388 ) ) ;
#32503 = CARTESIAN_POINT ( 'NONE',  ( -1.033464566929134687, 0.06523048226347956391, 0.3961614172153076763 ) ) ;
#32504 = CARTESIAN_POINT ( 'NONE',  ( -0.9412147342319837628, -0.1574803149606297803, 1.537893700787401841 ) ) ;
#32505 = CARTESIAN_POINT ( 'NONE',  ( 0.8759842519685039353, 0.1787899950787401882, 1.449311023568283341 ) ) ;
#32506 = CYLINDRICAL_SURFACE ( 'NONE', #31981, 0.09842519685039370636 ) ;
#32508 = CARTESIAN_POINT ( 'NONE',  ( -1.033464566929133799, 0.000000000000000000, 0.2362204723334177248 ) ) ;
#32507 = CARTESIAN_POINT ( 'NONE',  ( -0.9412147342319837628, -0.1574803149606297803, 1.774114173228345859 ) ) ;
#32509 = CARTESIAN_POINT ( 'NONE',  ( 0.1264236179284866091, -0.09399606293836260118, -0.1264236179284866091 ) ) ;
#32510 = ORIENTED_EDGE ( 'NONE', *, *, #3680, .F. ) ;
#32511 = CARTESIAN_POINT ( 'NONE',  ( 0.1592646090380026025, -0.04727201993818823389, -0.1404638620642042202 ) ) ;
#32512 = VERTEX_POINT ( 'NONE', #2335 ) ;
#32513 = DIRECTION ( 'NONE',  ( 1.822029033848725028E-16, 0.000000000000000000, 1.000000000000000000 ) ) ;
#32514 = CARTESIAN_POINT ( 'NONE',  ( 0.1478661631962259748, -0.09575019180978999733, -0.2000608872901662172 ) ) ;
#32515 = ORIENTED_EDGE ( 'NONE', *, *, #30488, .F. ) ;
#32516 = CARTESIAN_POINT ( 'NONE',  ( 0.8759842519685039353, -0.1787899950787401882, 0.6077755904974173617 ) ) ;
#32517 = ORIENTED_EDGE ( 'NONE', *, *, #25221, .F. ) ;
#32518 = CARTESIAN_POINT ( 'NONE',  ( 3.284318927891251994E-17, -1.806594488135212728, 0.1787899950787401882 ) ) ;
#32519 = CARTESIAN_POINT ( 'NONE',  ( -0.7495606340400177148, 0.1264236179284866091, 1.104822834591905556 ) ) ;
#32520 = CARTESIAN_POINT ( 'NONE',  ( -0.9873396505805591694, -0.1113553986120547346, 0.2017716535433070890 ) ) ;
#32521 = ORIENTED_EDGE ( 'NONE', *, *, #44616, .T. ) ;
#32522 = CARTESIAN_POINT ( 'NONE',  ( -0.7495606340400177148, 0.1264236179284866091, 1.060531496009228247 ) ) ;
#32523 = CARTESIAN_POINT ( 'NONE',  ( -1.002407869896990045, -0.1264236179284866091, 0.2583661416785200671 ) ) ;
#32524 = DIRECTION ( 'NONE',  ( 1.822029033848725028E-16, 0.000000000000000000, 1.000000000000000000 ) ) ;
#32525 = AXIS2_PLACEMENT_3D ( 'NONE', #28167, #28894, #47058 ) ;
#32526 = DIRECTION ( 'NONE',  ( 0.000000000000000000, -1.000000000000000000, 0.000000000000000000 ) ) ;
#32527 = CARTESIAN_POINT ( 'NONE',  ( 0.1787899950787401882, -0.7840806611426240913, -2.189545951927503898E-17 ) ) ;
#32528 = EDGE_LOOP ( 'NONE', ( #5117, #32861, #4197, #17118 ) ) ;
#32529 = CARTESIAN_POINT ( 'NONE',  ( -0.04541781944810669575, -0.08956206178171143006, 0.1491237657763354596 ) ) ;
#32530 = CONICAL_SURFACE ( 'NONE', #2621, 0.2471922904502826812, 0.5235987755982992597 ) ;
#32531 = AXIS2_PLACEMENT_3D ( 'NONE', #41802, #9243, #4926 ) ;
#32532 = ORIENTED_EDGE ( 'NONE', *, *, #9224, .T. ) ;
#32533 = CARTESIAN_POINT ( 'NONE',  ( 1.033464566929133799, 0.000000000000000000, 0.6791338582677166613 ) ) ;
#32534 = CARTESIAN_POINT ( 'NONE',  ( 0.6195511811023595161, 0.1864803149606293897, -1.186023622047243986 ) ) ;
#32535 = CARTESIAN_POINT ( 'NONE',  ( -0.7495606340400177148, -0.1264236179284866091, 0.6373031495525354195 ) ) ;
#32536 = CARTESIAN_POINT ( 'NONE',  ( -1.284448818897637956, -0.3937007874015748254, -1.181102362204724310 ) ) ;
#32537 = ORIENTED_EDGE ( 'NONE', *, *, #21534, .T. ) ;
#32538 = CARTESIAN_POINT ( 'NONE',  ( -0.6971942568897637749, 2.189545951927499583E-17, 1.818405511757259729 ) ) ;
#32539 = EDGE_CURVE ( 'NONE', #31906, #31572, #16961, .T. ) ;
#32540 = ORIENTED_EDGE ( 'NONE', *, *, #1941, .T. ) ;
#32541 = FACE_OUTER_BOUND ( 'NONE', #33836, .T. ) ;
#32542 = EDGE_CURVE ( 'NONE', #40321, #21943, #38296, .T. ) ;
#32543 = CARTESIAN_POINT ( 'NONE',  ( -1.002407869896990045, -0.1264236179284866091, 0.06151574797773248782 ) ) ;
#32544 = ORIENTED_EDGE ( 'NONE', *, *, #3519, .T. ) ;
#32545 = CARTESIAN_POINT ( 'NONE',  ( 0.7646288533564489232, 0.1113553986120547346, 0.6938976377952755792 ) ) ;
#32546 = CARTESIAN_POINT ( 'NONE',  ( -0.1797182628040039087, -0.9040792426539112636, 0.07444174185955065859 ) ) ;
#32547 = DIRECTION ( 'NONE',  ( 1.000000000000000000, 0.000000000000000000, 0.000000000000000000 ) ) ;
#32548 = CARTESIAN_POINT ( 'NONE',  ( -0.7646288533564489232, -0.1113553986120547346, 1.402559055010582645 ) ) ;
#32549 = CARTESIAN_POINT ( 'NONE',  ( 0.6971942568897637749, 2.189545951927499583E-17, 0.8341535432533228045 ) ) ;
#32550 = EDGE_CURVE ( 'NONE', #38566, #36909, #20756, .T. ) ;
#32551 = CARTESIAN_POINT ( 'NONE',  ( 0.1113553986120547346, -0.6033464566929134243, 0.1113553986120547346 ) ) ;
#32552 = CARTESIAN_POINT ( 'NONE',  ( -0.1017260139368336425, 0.1228220809759916765, -0.1240740172185132717 ) ) ;
#32553 = EDGE_CURVE ( 'NONE', #18566, #6306, #12918, .T. ) ;
#32554 = CARTESIAN_POINT ( 'NONE',  ( -0.2559055118110236116, 0.1477471161312031434, -0.3149606299212598381 ) ) ;
#32555 = CARTESIAN_POINT ( 'NONE',  ( 0.7185039370078739607, 1.928577636452523993E-17, 1.250000000000000000 ) ) ;
#32557 = CARTESIAN_POINT ( 'NONE',  ( 0.8759842519685039353, 0.000000000000000000, 4.498031496062992574 ) ) ;
#32556 = CARTESIAN_POINT ( 'NONE',  ( -0.2559055118110236116, 0.000000000000000000, -0.3149606299212598381 ) ) ;
#32558 = CARTESIAN_POINT ( 'NONE',  ( 0.8759842519685039353, -0.1574803149606299191, 1.850393700787401619 ) ) ;
#32560 = DIRECTION ( 'NONE',  ( 0.000000000000000000, 0.000000000000000000, 1.000000000000000000 ) ) ;
#32559 = CARTESIAN_POINT ( 'NONE',  ( 0.8019270111902716547, -0.1787899950787401604, 0.6791338582139527791 ) ) ;
#32561 = CARTESIAN_POINT ( 'NONE',  ( 0.02847999302535491814, 0.6072747502901004735, -0.8119482170283445210 ) ) ;
#32563 = AXIS2_PLACEMENT_3D ( 'NONE', #1423, #26150, #16082 ) ;
#32562 = CARTESIAN_POINT ( 'NONE',  ( 0.1264236179284866091, -0.6550196849856062542, 0.1264236179284866091 ) ) ;
#32564 = CARTESIAN_POINT ( 'NONE',  ( -0.8107537697050254399, -0.1574803149606297803, 0.3813976376877488139 ) ) ;
#32565 = VERTEX_POINT ( 'NONE', #9548 ) ;
#32566 = CARTESIAN_POINT ( 'NONE',  ( 0.1643927470033121618, 0.08114304680833644978, 0.1405438797532735651 ) ) ;
#32567 = AXIS2_PLACEMENT_3D ( 'NONE', #38515, #20061, #12180 ) ;
#32568 = CONICAL_SURFACE ( 'NONE', #10350, 0.08090551181102362266, 0.9599310885968742602 ) ;
#32569 = CARTESIAN_POINT ( 'NONE',  ( 0.1644020957507537628, 0.08115590401245532937, -0.1405661490837558925 ) ) ;
#32570 = CARTESIAN_POINT ( 'NONE',  ( 0.7495606340400177148, -0.1264236179284866091, 0.9522637794737952577 ) ) ;
#32571 = FACE_OUTER_BOUND ( 'NONE', #18522, .T. ) ;
#32572 = CARTESIAN_POINT ( 'NONE',  ( -1.094772975963752103E-17, -1.235728346402928945, -0.1787899950787401882 ) ) ;
#32573 = CARTESIAN_POINT ( 'NONE',  ( -0.1113553986120547346, -1.567913385826771755, -0.1113553986120547346 ) ) ;
#32574 = FACE_OUTER_BOUND ( 'NONE', #27917, .T. ) ;
#32575 = UNCERTAINTY_MEASURE_WITH_UNIT (LENGTH_MEASURE( 1.000000000000000082E-05 ), #46283, 'distance_accuracy_value', 'NONE') ;
#32576 = CARTESIAN_POINT ( 'NONE',  ( -0.6971942568897626646, 0.07405724077823318263, 0.07874015742655145200 ) ) ;
#32577 = CARTESIAN_POINT ( 'NONE',  ( 0.7495606340400177148, 0.1264236179284866091, 1.970964566875370139 ) ) ;
#32578 = ORIENTED_EDGE ( 'NONE', *, *, #44779, .F. ) ;
#32579 = CARTESIAN_POINT ( 'NONE',  ( -0.7185039370078739607, 0.000000000000000000, -2.869337061179095023E-17 ) ) ;
#32580 = CARTESIAN_POINT ( 'NONE',  ( -1.002407869896990045, 0.1264236179284866091, 1.719980314906866203 ) ) ;
#32581 = CARTESIAN_POINT ( 'NONE',  ( -0.9500414927467378812, -0.1787899950787401604, 1.117125984198206412 ) ) ;
#32582 = CARTESIAN_POINT ( 'NONE',  ( -0.8759842519685039353, -0.1787899950787401882, 0.3321850393163153226 ) ) ;
#32583 = ( BOUNDED_CURVE ( )  B_SPLINE_CURVE ( 2, ( #21701, #36335, #6597, #43730, #10933, #7323, #21448, #17623, #24585 ),
 .UNSPECIFIED., .F., .T. ) 
 B_SPLINE_CURVE_WITH_KNOTS ( ( 3, 2, 2, 2, 3 ),
 ( 0.04000000000000000083, 0.04250000000000000305, 0.04499999999999999833, 0.04750000000000000056, 0.05000000000000000278 ),
 .UNSPECIFIED. ) 
 CURVE ( )  GEOMETRIC_REPRESENTATION_ITEM ( )  RATIONAL_B_SPLINE_CURVE ( ( 1.000000000000000000, 0.9238795325112869605, 1.000000000000000000, 0.9238795325112869605, 1.000000000000000000, 0.9238795325112869605, 1.000000000000000000, 0.9238795325112869605, 1.000000000000000000 ) ) 
 REPRESENTATION_ITEM ( '' )  ) ;
#32584 = CARTESIAN_POINT ( 'NONE',  ( -0.2471922904502826812, 0.09842519685039370636, 5.914624404477007554E-17 ) ) ;
#32585 = CARTESIAN_POINT ( 'NONE',  ( -1.054774247047244540, 0.07405724077823318263, 1.919291338528913871 ) ) ;
#32586 = CARTESIAN_POINT ( 'NONE',  ( -0.2833714012347086642, 0.1260629598319809863, -0.7654422454633916795 ) ) ;
#32587 = CARTESIAN_POINT ( 'NONE',  ( -0.1673939672668370293, -0.09842519685039370636, -0.05722842092486787879 ) ) ;
#32588 = CARTESIAN_POINT ( 'NONE',  ( 0.1476377952755906220, 0.07627223685636320971, -0.1475485644998805468 ) ) ;
#32589 = DIRECTION ( 'NONE',  ( 0.000000000000000000, 0.000000000000000000, -1.000000000000000000 ) ) ;
#32590 = CARTESIAN_POINT ( 'NONE',  ( -1.002407869896990045, 0.1264236179284866091, 0.1451771653005673179 ) ) ;
#32591 = CARTESIAN_POINT ( 'NONE',  ( -0.3690944881889767215, 5.970426471673286898E-15, -0.7480314960629921295 ) ) ;
#32592 = ORIENTED_EDGE ( 'NONE', *, *, #43036, .F. ) ;
#32593 = ORIENTED_EDGE ( 'NONE', *, *, #26787, .F. ) ;
#32594 = CARTESIAN_POINT ( 'NONE',  ( -1.002407869896990045, 0.1264236179284866091, 1.449311023568283341 ) ) ;
#32595 = ORIENTED_EDGE ( 'NONE', *, *, #34773, .F. ) ;
#32596 = CARTESIAN_POINT ( 'NONE',  ( 0.9500414927467378812, -0.1787899950787401604, 1.471456692859622217 ) ) ;
#32597 = AXIS2_PLACEMENT_3D ( 'NONE', #6149, #1613, #17188 ) ;
#32598 = VECTOR ( 'NONE', #23911, 39.37007874015748143 ) ;
#32599 = CARTESIAN_POINT ( 'NONE',  ( 0.1264236179284866091, -1.211122047190330786, 0.1264236179284866091 ) ) ;
#32600 = CARTESIAN_POINT ( 'NONE',  ( 0.07405724077823318263, -1.351377952702143004, -0.1787899950787401604 ) ) ;
#32601 = ADVANCED_FACE ( 'NONE', ( #9782, #24171 ), #20549, .T. ) ;
#32602 = DIRECTION ( 'NONE',  ( -1.000000000000000000, 0.000000000000000000, 0.000000000000000000 ) ) ;
#32603 = DIRECTION ( 'NONE',  ( -0.9955207525527450807, 0.09454327705773800383, 6.685015436696001980E-15 ) ) ;
#32604 = CARTESIAN_POINT ( 'NONE',  ( 0.9412147342319837628, 0.1574803149606300301, 0.3321850393700786497 ) ) ;
#32605 = LINE ( 'NONE', #31888, #7159 ) ;
#32606 = CARTESIAN_POINT ( 'NONE',  ( -0.9873396505805591694, -0.1113553986120547346, 0.9793307085538898171 ) ) ;
#32607 = CARTESIAN_POINT ( 'NONE',  ( 0.9500414927467378812, 0.1787899950787401604, 0.3887795275052913224 ) ) ;
#32608 = CARTESIAN_POINT ( 'NONE',  ( 0.06523048226347956391, -0.07923228346456692717, -0.1574803149606300301 ) ) ;
#32609 = CARTESIAN_POINT ( 'NONE',  ( 1.033464566929133799, 0.000000000000000000, 1.889763779420031486 ) ) ;
#32610 = ORIENTED_EDGE ( 'NONE', *, *, #45214, .F. ) ;
#32611 = EDGE_CURVE ( 'NONE', #43027, #29787, #19845, .T. ) ;
#32612 = DIRECTION ( 'NONE',  ( 0.000000000000000000, 1.000000000000000000, 0.000000000000000000 ) ) ;
#32613 = CARTESIAN_POINT ( 'NONE',  ( 1.033464566929134687, 0.06523048226347956391, 0.7997047244094482865 ) ) ;
#32614 = DIRECTION ( 'NONE',  ( -1.000000000000000000, -0.000000000000000000, 0.000000000000000000 ) ) ;
#32616 = CARTESIAN_POINT ( 'NONE',  ( 1.033464566929134687, 0.06523048226347956391, 1.508366141732284671 ) ) ;
#32615 = CARTESIAN_POINT ( 'NONE',  ( -1.033464566929134687, -0.06523048226347956391, 0.4798228346456689386 ) ) ;
#32617 = CARTESIAN_POINT ( 'NONE',  ( 1.033464566929133799, 0.000000000000000000, 0.1968503935932602311 ) ) ;
#32618 = ORIENTED_EDGE ( 'NONE', *, *, #31827, .T. ) ;
#32619 = VECTOR ( 'NONE', #25111, 39.37007874015748143 ) ;
#32620 = CYLINDRICAL_SURFACE ( 'NONE', #5749, 0.1574803149606299191 ) ;
#32621 = CARTESIAN_POINT ( 'NONE',  ( -9.642888182262618425E-18, -1.484251968396409493, -0.1574803149606299191 ) ) ;
#32622 = CARTESIAN_POINT ( 'NONE',  ( -0.07405724077823318263, -0.7066929133320629663, 0.1787899950787401604 ) ) ;
#32623 = CARTESIAN_POINT ( 'NONE',  ( -0.9873396505805591694, -0.1113553986120547346, 0.1525590550105832555 ) ) ;
#32624 = CARTESIAN_POINT ( 'NONE',  ( 0.06523048226347956391, -1.063484251968504379, -0.1574803149606300301 ) ) ;
#32625 = CARTESIAN_POINT ( 'NONE',  ( 0.7646288533564489232, 0.1113553986120547346, 1.038385826664126155 ) ) ;
#32626 = CARTESIAN_POINT ( 'NONE',  ( 1.033464566929133799, 0.000000000000000000, 0.5216535433070865757 ) ) ;
#32627 = ORIENTED_EDGE ( 'NONE', *, *, #20772, .F. ) ;
#32628 = ORIENTED_EDGE ( 'NONE', *, *, #3532, .F. ) ;
#32629 = VERTEX_POINT ( 'NONE', #34727 ) ;
#32630 = CARTESIAN_POINT ( 'NONE',  ( -0.8019270111902717657, -0.1787899950787401604, 1.668307086560410157 ) ) ;
#32631 = CARTESIAN_POINT ( 'NONE',  ( 0.7495606340400177148, 0.1264236179284866091, 1.537893700733637736 ) ) ;
#32632 = VECTOR ( 'NONE', #41028, 39.37007874015748143 ) ;
#32633 = CARTESIAN_POINT ( 'NONE',  ( -0.6971942568897637749, 2.189545951927499583E-17, 0.7554133857730077617 ) ) ;
#32634 = CARTESIAN_POINT ( 'NONE',  ( 0.8759842519685039353, 0.1787899950787401882, 0.2337598424659216578 ) ) ;
#32635 = LINE ( 'NONE', #7434, #41128 ) ;
#32636 = CARTESIAN_POINT ( 'NONE',  ( 0.7495606340400177148, -0.1264236179284866091, 0.7997047243556849594 ) ) ;
#32637 = CARTESIAN_POINT ( 'NONE',  ( -0.8759842519685039353, 0.1787899950787401882, 0.7012795275052913224 ) ) ;
#32638 = EDGE_CURVE ( 'NONE', #4710, #38209, #46817, .T. ) ;
#32639 = DIRECTION ( 'NONE',  ( -1.000000000000000000, 0.000000000000000000, 0.000000000000000000 ) ) ;
#32640 = DIRECTION ( 'NONE',  ( -1.000000000000000000, 0.000000000000000000, 0.000000000000000000 ) ) ;
#32641 = CARTESIAN_POINT ( 'NONE',  ( -0.1574803149606300301, -0.1776574802074335768, -0.06523048226347956391 ) ) ;
#32642 = CARTESIAN_POINT ( 'NONE',  ( -0.7646288533564489232, 0.1113553986120547346, 1.943897637687747926 ) ) ;
#32643 = VERTEX_POINT ( 'NONE', #19611 ) ;
#32644 = FACE_OUTER_BOUND ( 'NONE', #41155, .T. ) ;
#32645 = CARTESIAN_POINT ( 'NONE',  ( -0.8107537697050253289, -0.1574803149606297803, 0.4699803149606304742 ) ) ;
#32646 = CARTESIAN_POINT ( 'NONE',  ( 1.054774247047244540, -0.07405724077823318263, 1.520669291284818758 ) ) ;
#32647 = CARTESIAN_POINT ( 'NONE',  ( -0.1730591442732248297, -0.09851383842017420733, 0.004658872311817456938 ) ) ;
#32648 = DIRECTION ( 'NONE',  ( -1.000000000000000000, 0.000000000000000000, 0.000000000000000000 ) ) ;
#32649 = VERTEX_POINT ( 'NONE', #23929 ) ;
#32650 = ORIENTED_EDGE ( 'NONE', *, *, #25450, .T. ) ;
#32651 = CARTESIAN_POINT ( 'NONE',  ( 0.1787899950787401604, -0.6870078739619840391, -0.07405724077823318263 ) ) ;
#32652 = DIRECTION ( 'NONE',  ( 0.000000000000000000, 0.000000000000000000, 1.000000000000000000 ) ) ;
#32653 = VERTEX_POINT ( 'NONE', #38535 ) ;
#32654 = VECTOR ( 'NONE', #1775, 39.37007874015748143 ) ;
#32655 = CARTESIAN_POINT ( 'NONE',  ( 0.2471922904502826812, 0.09842519685039370636, -5.914624404477007554E-17 ) ) ;
#32656 = CARTESIAN_POINT ( 'NONE',  ( 3.284318927891251994E-17, -0.9749015747493857686, 0.1787899950787401882 ) ) ;
#32657 = EDGE_CURVE ( 'NONE', #12042, #29787, #4249, .T. ) ;
#32658 = CARTESIAN_POINT ( 'NONE',  ( -0.2471911544650258752, -0.08539615244838703878, -0.06152421978380465811 ) ) ;
#32659 = CARTESIAN_POINT ( 'NONE',  ( 0.9500414927467378812, -0.1787899950787401604, 1.707677165300566235 ) ) ;
#32660 = CARTESIAN_POINT ( 'NONE',  ( 1.054774247047244540, 0.07405724077823318263, 0.3789370078202520253 ) ) ;
#32661 = CARTESIAN_POINT ( 'NONE',  ( -0.07444174185955065859, -0.1511264867483998187, 0.1797182628040039087 ) ) ;
#32662 = CARTESIAN_POINT ( 'NONE',  ( 0.07405724077823318263, -0.1467775115363254557, -0.1787899950787401604 ) ) ;
#32663 = CARTESIAN_POINT ( 'NONE',  ( 0.1264236179284866091, -0.2514763778989925203, -0.1264236179284866091 ) ) ;
#32664 = ADVANCED_FACE ( 'NONE', ( #23460 ), #28010, .T. ) ;
#32665 = CARTESIAN_POINT ( 'NONE',  ( 0.7495606340400177148, -0.1264236179284866091, 0.5979330708123780092 ) ) ;
#32666 = CARTESIAN_POINT ( 'NONE',  ( -0.9500414927467377701, -0.1787899950787401604, 1.003937007820253413 ) ) ;
#32667 = CARTESIAN_POINT ( 'NONE',  ( 0.9873396505805591694, 0.1113553986120547346, 0.9891732282389291697 ) ) ;
#32668 = CARTESIAN_POINT ( 'NONE',  ( -0.1797182628040039365, -1.654571368638163342, 0.000000000000000000 ) ) ;
#32669 = CARTESIAN_POINT ( 'NONE',  ( 0.7646288533564489232, 0.1113553986120547346, 0.9596456691838111119 ) ) ;
#32670 = CARTESIAN_POINT ( 'NONE',  ( 0.8759842519685039353, 0.1787899950787401882, 1.729822834591905556 ) ) ;
#32672 = CARTESIAN_POINT ( 'NONE',  ( 0.9412147342319837628, 0.1574803149606300301, 0.1254921258767249526 ) ) ;
#32671 = CARTESIAN_POINT ( 'NONE',  ( -0.7185039370078739607, 1.928577636452523993E-17, 0.8858267715460158565 ) ) ;
#32673 = ORIENTED_EDGE ( 'NONE', *, *, #15332, .T. ) ;
#32674 = DIRECTION ( 'NONE',  ( 0.000000000000000000, -1.000000000000000000, 0.000000000000000000 ) ) ;
#32675 = CARTESIAN_POINT ( 'NONE',  ( 0.1588150004739004306, -0.1472798737662755764, 0.02049432688553643953 ) ) ;
#32677 = CARTESIAN_POINT ( 'NONE',  ( 0.1787899950787401882, -0.3006889763241893943, -2.189545951927503898E-17 ) ) ;
#32676 = CARTESIAN_POINT ( 'NONE',  ( 0.1113553986120547346, -0.8986220471365670148, -0.1113553986120547346 ) ) ;
#32678 = CARTESIAN_POINT ( 'NONE',  ( -0.8019270111902717657, -0.1787899950787401604, 0.4478346456155276045 ) ) ;
#32679 = CARTESIAN_POINT ( 'NONE',  ( 1.054774247047244096, 0.000000000000000000, 0.5339566928596221063 ) ) ;
#32680 = CARTESIAN_POINT ( 'NONE',  ( 0.07405724077823318263, -1.036417322780882833, -0.1787899950787401604 ) ) ;
#32681 = CARTESIAN_POINT ( 'NONE',  ( 0.6971942568897637749, 2.189545951927499583E-17, 0.08612204719033110523 ) ) ;
#32682 = CARTESIAN_POINT ( 'NONE',  ( 0.9873396505805591694, 0.1113553986120547346, 1.107283464459401623 ) ) ;
#32683 = CARTESIAN_POINT ( 'NONE',  ( -0.6971942568897648851, -0.07405724077823297447, 1.658464566875369472 ) ) ;
#32684 = ORIENTED_EDGE ( 'NONE', *, *, #7511, .T. ) ;
#32685 = CARTESIAN_POINT ( 'NONE',  ( -0.2801779484932497843, -0.1329283866310993489, -0.9781771623220059109 ) ) ;
#32686 = CARTESIAN_POINT ( 'NONE',  ( 0.6971942568897648851, 0.07405724077823318263, 1.146653543253323582 ) ) ;
#32687 = CARTESIAN_POINT ( 'NONE',  ( 1.002407869896990045, -0.1264236179284866091, 1.828248031442299082 ) ) ;
#32688 = CARTESIAN_POINT ( 'NONE',  ( -0.7185039370078746268, 0.06523048226347956391, 0.6176181102362200415 ) ) ;
#32689 = CARTESIAN_POINT ( 'NONE',  ( -0.6971942568897626646, -0.07405724077823297447, 0.9498031495525356416 ) ) ;
#32690 = CARTESIAN_POINT ( 'NONE',  ( -0.8759842519685039353, -0.1574803149606299191, 1.614173228346456712 ) ) ;
#32691 = CARTESIAN_POINT ( 'NONE',  ( -0.1789895911306832177, -0.1921545436409667906, -0.04147023971061550990 ) ) ;
#32692 = CARTESIAN_POINT ( 'NONE',  ( 0.8019270111902716547, 0.1787899950787401604, 0.3543307086076538659 ) ) ;
#32693 = CARTESIAN_POINT ( 'NONE',  ( -0.7495606340400177148, 0.1264236179284866091, 0.2731299212060791515 ) ) ;
#32694 = PRODUCT_DEFINITION_CONTEXT ( 'detailed design', #44058, 'design' ) ;
#32695 = CARTESIAN_POINT ( 'NONE',  ( -0.7495606340400177148, 0.1264236179284866091, 0.7849409448281259305 ) ) ;
#32696 = CARTESIAN_POINT ( 'NONE',  ( 0.7646288533564489232, 0.1113553986120547346, 1.550196850286173156 ) ) ;
#32697 = ORIENTED_EDGE ( 'NONE', *, *, #575, .F. ) ;
#32698 = EDGE_CURVE ( 'NONE', #32512, #39036, #6636, .T. ) ;
#32699 = CARTESIAN_POINT ( 'NONE',  ( -0.1787899950787401604, -0.04724409443442544737, -0.07405724077823318263 ) ) ;
#32700 = CARTESIAN_POINT ( 'NONE',  ( 0.6971942568897637749, 2.189545951927499583E-17, 0.7947834645131652831 ) ) ;
#32701 = CARTESIAN_POINT ( 'NONE',  ( 0.8019270111902716547, 0.1787899950787401604, 1.102362204670646495 ) ) ;
#32702 = CARTESIAN_POINT ( 'NONE',  ( -0.6971942568897648851, -0.07405724077823297447, 1.855314960576157635 ) ) ;
#32703 = CARTESIAN_POINT ( 'NONE',  ( 0.9500414927467378812, 0.1787899950787401604, 1.919291338528913871 ) ) ;
#32704 = ORIENTED_EDGE ( 'NONE', *, *, #5522, .F. ) ;
#32705 = CARTESIAN_POINT ( 'NONE',  ( 0.3980944881889764142, 2.762335417273529347E-15, 0.7480314960629921295 ) ) ;
#32706 = CARTESIAN_POINT ( 'NONE',  ( -0.1264236179284866091, -1.281127905237112286, -0.1264236179284866091 ) ) ;
#32707 = EDGE_LOOP ( 'NONE', ( #27653, #35959, #31398, #37905 ) ) ;
#32708 = CARTESIAN_POINT ( 'NONE',  ( -0.1787899950787401604, -0.2342519684501733479, 0.07405724077823318263 ) ) ;
#32709 = ADVANCED_FACE ( 'NONE', ( #24624 ), #29223, .T. ) ;
#32710 = CARTESIAN_POINT ( 'NONE',  ( -0.4955489724641236604, -0.5708661417322835607, 0.3997690233743834698 ) ) ;
#32711 = VERTEX_POINT ( 'NONE', #43048 ) ;
#32712 = CARTESIAN_POINT ( 'NONE',  ( 0.8759842519685039353, 0.1787899950787401882, 1.134350393647023614 ) ) ;
#32713 = DIRECTION ( 'NONE',  ( -1.000000000000000000, 0.000000000000000000, 0.000000000000000000 ) ) ;
#32714 = FACE_OUTER_BOUND ( 'NONE', #35242, .T. ) ;
#32715 = CONICAL_SURFACE ( 'NONE', #17357, 0.1377952755905511861, 1.047197551196598297 ) ;
#32716 = ADVANCED_FACE ( 'NONE', ( #14081 ), #11608, .T. ) ;
#32717 = CARTESIAN_POINT ( 'NONE',  ( 1.033464566929134687, -0.06523048226347956391, 1.936515748031494955 ) ) ;
#32718 = CARTESIAN_POINT ( 'NONE',  ( -0.1264236179284866091, -1.663877952702141672, -0.1264236179284866091 ) ) ;
#32719 = CARTESIAN_POINT ( 'NONE',  ( -0.1264236179284866091, -0.7583661416785196785, -0.1264236179284866091 ) ) ;
#32720 = ( BOUNDED_CURVE ( )  B_SPLINE_CURVE ( 2, ( #10390, #24521, #39120, #28861, #24995, #6294, #20683, #6056, #35323 ),
 .UNSPECIFIED., .F., .F. ) 
 B_SPLINE_CURVE_WITH_KNOTS ( ( 3, 2, 2, 2, 3 ),
 ( 0.4500000000000000111, 0.4525000000000000133, 0.4550000000000000155, 0.4575000000000000178, 0.4600000000000000200 ),
 .UNSPECIFIED. ) 
 CURVE ( )  GEOMETRIC_REPRESENTATION_ITEM ( )  RATIONAL_B_SPLINE_CURVE ( ( 1.000000000000000000, 0.9238795325112869605, 1.000000000000000000, 0.9238795325112869605, 1.000000000000000000, 0.9238795325112869605, 1.000000000000000000, 0.9238795325112869605, 1.000000000000000000 ) ) 
 REPRESENTATION_ITEM ( '' )  ) ;
#32721 = CARTESIAN_POINT ( 'NONE',  ( -0.8019270111902716547, 0.1787899950787401604, 0.4330708660879683536 ) ) ;
#32722 = CARTESIAN_POINT ( 'NONE',  ( 0.2204724409448818867, 2.548376702365417207E-17, -0.2047244094488188948 ) ) ;
#32723 = CARTESIAN_POINT ( 'NONE',  ( -0.07444174185955065859, -1.268252471000367976, -0.1797182628040039087 ) ) ;
#32724 = CARTESIAN_POINT ( 'NONE',  ( -0.05712600390865770622, 0.2625125185280161588, -0.05471869868084688199 ) ) ;
#32725 = CARTESIAN_POINT ( 'NONE',  ( 0.7495606340400177148, -0.1264236179284866091, 1.272145669237574772 ) ) ;
#32726 = CARTESIAN_POINT ( 'NONE',  ( 0.6971942568897648851, -0.07405724077823297447, 1.619094488135213838 ) ) ;
#32727 = CARTESIAN_POINT ( 'NONE',  ( -0.5314960629921260393, 0.000000000000000000, 4.498031496062992574 ) ) ;
#32729 = CARTESIAN_POINT ( 'NONE',  ( -0.7672715001790547662, 0.1194512761122965006, 1.980665997130102163 ) ) ;
#32728 = CARTESIAN_POINT ( 'NONE',  ( 0.3690944881889778317, 3.409318977613033647E-15, -0.7480314960629921295 ) ) ;
#32730 = CARTESIAN_POINT ( 'NONE',  ( 0.8107537697050254399, -0.1574803149606297803, 0.8144685038294804391 ) ) ;
#32731 = CARTESIAN_POINT ( 'NONE',  ( -0.7185039370078739607, 1.928577636452523993E-17, 1.712598425089322918 ) ) ;
#32732 = CARTESIAN_POINT ( 'NONE',  ( 0.7495606340400177148, -0.1264236179284866091, 0.1648622046706460786 ) ) ;
#32733 = CARTESIAN_POINT ( 'NONE',  ( 0.7010592508071858964, 0.01453562945798193839, 0.03937031133914711128 ) ) ;
#32735 = CARTESIAN_POINT ( 'NONE',  ( -0.4330708661417345673, 3.105646754637360326E-15, -0.9891732283464564901 ) ) ;
#32734 = CARTESIAN_POINT ( 'NONE',  ( 0.8759842519685039353, -0.1787899950787401882, 1.114665354276944909 ) ) ;
#32736 = CARTESIAN_POINT ( 'NONE',  ( 1.033464566929134687, -0.06523048226347956391, 1.227854330708661124 ) ) ;
#32737 = CARTESIAN_POINT ( 'NONE',  ( -0.9500414927467378812, -0.1787899950787401604, 1.235236220418678199 ) ) ;
#32738 = CARTESIAN_POINT ( 'NONE',  ( 1.033464566929133799, 0.000000000000000000, 0.5118110235145204578 ) ) ;
#32739 = ORIENTED_EDGE ( 'NONE', *, *, #44779, .T. ) ;
#32740 = FILL_AREA_STYLE_COLOUR ( '', #10039 ) ;
#32741 = CARTESIAN_POINT ( 'NONE',  ( 0.8636164050717508589, 0.1748576815465697487, 0.03937204453775523805 ) ) ;
#32742 = CARTESIAN_POINT ( 'NONE',  ( -0.8759842519685039353, 0.1574803149606299191, 0.4035433069790866356 ) ) ;
#32743 = VERTEX_POINT ( 'NONE', #21492 ) ;
#32744 = CARTESIAN_POINT ( 'NONE',  ( 0.8759842519685039353, -0.1787899950787401882, 1.390255905458047447 ) ) ;
#32746 = CARTESIAN_POINT ( 'NONE',  ( 1.033464566929133799, 0.000000000000000000, 1.663385826771653697 ) ) ;
#32745 = CARTESIAN_POINT ( 'NONE',  ( -0.9412147342319837628, 0.1574803149606300301, 1.631397637795275468 ) ) ;
#32747 = CARTESIAN_POINT ( 'NONE',  ( -0.07405724077823318263, 0.006889763833291078637, 0.1787899950787401604 ) ) ;
#32748 = EDGE_LOOP ( 'NONE', ( #36714, #8513, #14958, #41726, #36260 ) ) ;
#32749 = VECTOR ( 'NONE', #10270, 39.37007874015748143 ) ;
#32750 = CARTESIAN_POINT ( 'NONE',  ( -0.1235961452251415349, -0.09842519685039370636, -0.2140748031496062798 ) ) ;
#32751 = ( BOUNDED_CURVE ( )  B_SPLINE_CURVE ( 2, ( #25614, #21517, #29248, #43797, #31863, #6187, #172, #15778, #40885 ),
 .UNSPECIFIED., .F., .T. ) 
 B_SPLINE_CURVE_WITH_KNOTS ( ( 3, 2, 2, 2, 3 ),
 ( 0.9300000000000000488, 0.9324999999999999956, 0.9350000000000000533, 0.9375000000000000000, 0.9399999999999999467 ),
 .UNSPECIFIED. ) 
 CURVE ( )  GEOMETRIC_REPRESENTATION_ITEM ( )  RATIONAL_B_SPLINE_CURVE ( ( 1.000000000000000000, 0.9238795325112869605, 1.000000000000000000, 0.9238795325112869605, 1.000000000000000000, 0.9238795325112869605, 1.000000000000000000, 0.9238795325112829637, 1.000000000000000000 ) ) 
 REPRESENTATION_ITEM ( '' )  ) ;
#32752 = LINE ( 'NONE', #7787, #35933 ) ;
#32753 = DIRECTION ( 'NONE',  ( -1.000000000000000000, 0.000000000000000000, 0.000000000000000000 ) ) ;
#32754 = ( BOUNDED_CURVE ( )  B_SPLINE_CURVE ( 2, ( #9326, #30916, #20333, #37849, #2115, #30679, #16745, #12703, #31386 ),
 .UNSPECIFIED., .F., .F. ) 
 B_SPLINE_CURVE_WITH_KNOTS ( ( 3, 2, 2, 2, 3 ),
 ( 0.5799999999999999600, 0.5825000000000000178, 0.5849999999999999645, 0.5875000000000000222, 0.5899999999999999689 ),
 .UNSPECIFIED. ) 
 CURVE ( )  GEOMETRIC_REPRESENTATION_ITEM ( )  RATIONAL_B_SPLINE_CURVE ( ( 1.000000000000000000, 0.9238795325112869605, 1.000000000000000000, 0.9238795325112869605, 1.000000000000000000, 0.9238795325112869605, 1.000000000000000000, 0.9238795325112869605, 1.000000000000000000 ) ) 
 REPRESENTATION_ITEM ( '' )  ) ;
#32755 = CARTESIAN_POINT ( 'NONE',  ( 0.8019270111902717657, 0.1787899950787401604, 0.6299212597887560161 ) ) ;
#32756 = ORIENTED_EDGE ( 'NONE', *, *, #19047, .T. ) ;
#32757 = CARTESIAN_POINT ( 'NONE',  ( 2.892866454678787531E-17, 0.07086614183981043702, 0.1574803149606299191 ) ) ;
#32758 = CARTESIAN_POINT ( 'NONE',  ( -0.8019270111902717657, -0.1787899950787401604, 1.117125984198206412 ) ) ;
#32759 = ORIENTED_EDGE ( 'NONE', *, *, #16203, .T. ) ;
#32760 = EDGE_CURVE ( 'NONE', #20293, #14046, #7081, .T. ) ;
#32761 = CARTESIAN_POINT ( 'NONE',  ( -0.8759842519685039353, -0.1787899950787401882, 1.075295275536787276 ) ) ;
#32762 = CARTESIAN_POINT ( 'NONE',  ( -1.054774247047244096, 0.000000000000000000, 0.8538385826234016207 ) ) ;
#32763 = CARTESIAN_POINT ( 'NONE',  ( -1.054774247047244540, 0.07405724077823318263, 0.1870078739619845387 ) ) ;
#32764 = CARTESIAN_POINT ( 'NONE',  ( -0.8107537697050254399, -0.1574803149606297803, 0.3518700787401575769 ) ) ;
#32765 = CARTESIAN_POINT ( 'NONE',  ( 0.7185039370078766252, -0.06523048226348168721, 1.636318897530268490 ) ) ;
#32766 = CARTESIAN_POINT ( 'NONE',  ( 0.07405724077823318263, -0.8554389288591597307, -0.1787899950787401604 ) ) ;
#32767 = ORIENTED_EDGE ( 'NONE', *, *, #28278, .T. ) ;
#32768 = CARTESIAN_POINT ( 'NONE',  ( -9.642888182262618425E-18, -0.02755905501058318954, -0.1574803149606299191 ) ) ;
#32769 = CARTESIAN_POINT ( 'NONE',  ( -0.8759842519685039353, -0.1574803149606299191, 0.8562992124908976876 ) ) ;
#32770 = EDGE_CURVE ( 'NONE', #34774, #2394, #11463, .T. ) ;
#32771 = APPLICATION_CONTEXT ( 'automotive_design' ) ;
#32772 = ORIENTED_EDGE ( 'NONE', *, *, #27742, .F. ) ;
#32773 = CARTESIAN_POINT ( 'NONE',  ( 0.000000000000000000, 0.000000000000000000, -0.1321438491773566926 ) ) ;
#32774 = CARTESIAN_POINT ( 'NONE',  ( -0.9500414927467378812, 0.1787899950787401604, 0.7775590550643479704 ) ) ;
#32775 = AXIS2_PLACEMENT_3D ( 'NONE', #42470, #8955, #37958 ) ;
#32776 = CARTESIAN_POINT ( 'NONE',  ( -0.8019270111902716547, -0.1787899950787401604, 1.747047244040724312 ) ) ;
#32777 = VERTEX_POINT ( 'NONE', #18143 ) ;
#32778 = AXIS2_PLACEMENT_3D ( 'NONE', #467, #8613, #33343 ) ;
#32779 = LENGTH_MEASURE_WITH_UNIT ( LENGTH_MEASURE( 0.02539999999999999897 ), #40618 ) ;
#32780 = CARTESIAN_POINT ( 'NONE',  ( 0.8107537697050253289, -0.1574803149606297803, 0.7062007874015745479 ) ) ;
#32781 = CARTESIAN_POINT ( 'NONE',  ( 0.1797182628040039087, -0.8843942032838323364, -0.07444174185955065859 ) ) ;
#32782 = CARTESIAN_POINT ( 'NONE',  ( 0.1062722551331691384, -0.2341365745593732284, -0.3142669362052405435 ) ) ;
#32783 = CARTESIAN_POINT ( 'NONE',  ( -0.7185039370078746268, 0.06523048226347956391, 1.355807086506646275 ) ) ;
#32784 = CARTESIAN_POINT ( 'NONE',  ( 0.8759842519685039353, 0.1787899950787401882, 0.8243110235682834519 ) ) ;
#32785 = CARTESIAN_POINT ( 'NONE',  ( -0.1113553986120547346, -0.6131889763779527769, 0.1113553986120547346 ) ) ;
#32786 = CARTESIAN_POINT ( 'NONE',  ( -0.8070866141732283561, -0.3937007874015746034, 0.8559055118110230342 ) ) ;
#32787 = CARTESIAN_POINT ( 'NONE',  ( -0.2559055118110236116, 0.04268984771565554476, -0.03498110359409837417 ) ) ;
#32788 = CARTESIAN_POINT ( 'NONE',  ( 0.7185039370078739607, 1.928577636452523993E-17, 1.446850393700787274 ) ) ;
#32790 = CARTESIAN_POINT ( 'NONE',  ( 0.9412147342319837628, -0.1574803149606297803, 1.567421259734991690 ) ) ;
#32789 = CARTESIAN_POINT ( 'NONE',  ( 0.9408631620327171374, -0.1642324321402740817, 1.989367024862866540 ) ) ;
#32791 = CARTESIAN_POINT ( 'NONE',  ( 0.7185039370078739607, 1.928577636452523993E-17, 1.712598425089322918 ) ) ;
#32793 = CARTESIAN_POINT ( 'NONE',  ( 0.9412147342319837628, -0.1574803149606297803, 0.2682086613097960370 ) ) ;
#32792 = CARTESIAN_POINT ( 'NONE',  ( 0.6971942568897648851, 0.07405724077823318263, 0.6692913385289143147 ) ) ;
#32794 = CARTESIAN_POINT ( 'NONE',  ( 0.1787899950787401604, -0.6870078739619840391, -0.07405724077823318263 ) ) ;
#32795 = CYLINDRICAL_SURFACE ( 'NONE', #45275, 0.1968503937007874127 ) ;
#32796 = ORIENTED_EDGE ( 'NONE', *, *, #36582, .F. ) ;
#32797 = DIRECTION ( 'NONE',  ( 1.000000000000000000, 0.000000000000000000, -4.336808689942015271E-16 ) ) ;
#32798 = CARTESIAN_POINT ( 'NONE',  ( 0.000000000000000000, -0.1193342091828949042, 0.06889763779527559306 ) ) ;
#32799 = CARTESIAN_POINT ( 'NONE',  ( 1.002407869896990045, -0.1264236179284866091, 0.9621062991588346103 ) ) ;
#32800 = CARTESIAN_POINT ( 'NONE',  ( 1.033464566929133799, 0.000000000000000000, 1.496062992018456494 ) ) ;
#32801 = CARTESIAN_POINT ( 'NONE',  ( 0.1264236179284866091, -1.171751968450173154, 0.1264236179284866091 ) ) ;
#32802 = CARTESIAN_POINT ( 'NONE',  ( -0.1574803149606297803, -1.521161417322834497, 0.06523048226347956391 ) ) ;
#32803 = DIRECTION ( 'NONE',  ( -0.000000000000000000, -1.000000000000000000, -0.000000000000000000 ) ) ;
#32804 = CARTESIAN_POINT ( 'NONE',  ( -0.8759842519685039353, 0.1787899950787401882, 0.1107283464029295283 ) ) ;
#32805 = CARTESIAN_POINT ( 'NONE',  ( -0.9412147342319837628, 0.1574803149606300301, 0.6077755905511815770 ) ) ;
#32806 = VERTEX_POINT ( 'NONE', #32786 ) ;
#32808 = CARTESIAN_POINT ( 'NONE',  ( -0.07405724077823318263, -1.430118110182456714, -0.1787899950787401604 ) ) ;
#32807 = CARTESIAN_POINT ( 'NONE',  ( -0.1574803149606297803, -0.3302165353255438474, 0.06523048226347956391 ) ) ;
#32809 = CARTESIAN_POINT ( 'NONE',  ( -0.6971942568897637749, 2.189545951927499583E-17, 1.897145669237574772 ) ) ;
#32810 = CARTESIAN_POINT ( 'NONE',  ( -0.8019270111902717657, -0.1787899950787401604, 1.742125984198204858 ) ) ;
#32811 = ADVANCED_FACE ( 'NONE', ( #47381 ), #14553, .T. ) ;
#32812 = CONICAL_SURFACE ( 'NONE', #10604, 0.1574803149606299191, 1.047197551196598297 ) ;
#32813 = CARTESIAN_POINT ( 'NONE',  ( -0.7495606340400177148, -0.1264236179284866091, 0.4060039369541102450 ) ) ;
#32814 = EDGE_CURVE ( 'NONE', #39269, #46651, #28235, .T. ) ;
#32815 = CARTESIAN_POINT ( 'NONE',  ( -0.2471922904502826812, 0.07746962187842153236, 0.07828042841527922679 ) ) ;
#32816 = CARTESIAN_POINT ( 'NONE',  ( 0.9873396505805591694, 0.1113553986120547346, 0.3986220471365669038 ) ) ;
#32817 = CARTESIAN_POINT ( 'NONE',  ( 1.054774247047244540, 0.07405724077823318263, 0.02460629915883492599 ) ) ;
#32818 = DIRECTION ( 'NONE',  ( -1.000000000000000000, 0.000000000000000000, 0.000000000000000000 ) ) ;
#32819 = CARTESIAN_POINT ( 'NONE',  ( 0.1787899950787401604, -0.3879192438197899273, -0.07405724077823318263 ) ) ;
#32820 = CARTESIAN_POINT ( 'NONE',  ( -0.1407286617981055310, -0.09842519685039370636, -0.1134193063733844598 ) ) ;
#32821 = DIRECTION ( 'NONE',  ( -0.000000000000000000, 1.000000000000000000, -0.000000000000000000 ) ) ;
#32822 = CARTESIAN_POINT ( 'NONE',  ( 0.000000000000000000, 0.000000000000000000, -0.1045766232635885612 ) ) ;
#32823 = EDGE_CURVE ( 'NONE', #35433, #2521, #37712, .T. ) ;
#32824 = ADVANCED_FACE ( 'NONE', ( #5338 ), #30325, .F. ) ;
#32825 = CARTESIAN_POINT ( 'NONE',  ( -1.054774247047244540, -0.07405724077823318263, 0.3346456692375748831 ) ) ;
#32826 = EDGE_LOOP ( 'NONE', ( #34277, #23018, #30059, #21204 ) ) ;
#32827 = ORIENTED_EDGE ( 'NONE', *, *, #6381, .F. ) ;
#32828 = CARTESIAN_POINT ( 'NONE',  ( -0.6971942568897648851, -0.07405724077823297447, 1.348425196796630976 ) ) ;
#32829 = ORIENTED_EDGE ( 'NONE', *, *, #3183, .F. ) ;
#32830 = CARTESIAN_POINT ( 'NONE',  ( 0.1787899950787401604, -1.208661417269070393, 0.07405724077823318263 ) ) ;
#32831 = CARTESIAN_POINT ( 'NONE',  ( -1.094772975963752103E-17, -1.427657480261196987, -0.1787899950787401882 ) ) ;
#32832 = CIRCLE ( 'NONE', #3764, 0.1377952755905510474 ) ;
#32833 = CARTESIAN_POINT ( 'NONE',  ( -0.7185039370078739607, 0.000000000000000000, -2.869337061179095023E-17 ) ) ;
#32834 = CARTESIAN_POINT ( 'NONE',  ( 0.000000000000000000, 0.000000000000000000, -0.6196850393700787940 ) ) ;
#32835 = CARTESIAN_POINT ( 'NONE',  ( 0.9873396505805591694, 0.1113553986120547346, 0.4084645669291339098 ) ) ;
#32836 = CARTESIAN_POINT ( 'NONE',  ( 0.1797182628040039087, -0.6137249119452504731, 0.07444174185955046430 ) ) ;
#32837 = DIRECTION ( 'NONE',  ( -0.000000000000000000, 1.000000000000000000, -0.000000000000000000 ) ) ;
#32838 = CARTESIAN_POINT ( 'NONE',  ( -0.7185039370078746268, -0.06523048226347956391, 0.9670275589475911815 ) ) ;
#32839 = VECTOR ( 'NONE', #45949, 39.37007874015748143 ) ;
#32840 = CARTESIAN_POINT ( 'NONE',  ( 0.1113553986120547346, -0.09153543307086613179, 0.1113553986120547346 ) ) ;
#32841 = B_SPLINE_CURVE_WITH_KNOTS ( 'NONE', 3,
 ( #568, #4885, #41282, #11390, #346, #22639, #26251, #22391, #44188, #7775, #8482, #26003, #1285, #4396, #37244, #8010 ),
 .UNSPECIFIED., .F., .F.,
 ( 4, 2, 2, 2, 2, 2, 2, 4 ),
 ( 0.000000000000000000, 0.001193518611021448031, 0.002387037222042896062, 0.003580555833064344093, 0.004177315138575062904, 0.004475694791330420141, 0.004624884617708099194, 0.004774074444085778246 ),
 .UNSPECIFIED. ) ;
#32842 = CARTESIAN_POINT ( 'NONE',  ( 0.9873396505805591694, -0.1113553986120547346, 1.806102362097196767 ) ) ;
#32843 = ORIENTED_EDGE ( 'NONE', *, *, #38703, .T. ) ;
#32844 = DIRECTION ( 'NONE',  ( 0.000000000000000000, 1.000000000000000000, 0.000000000000000000 ) ) ;
#32845 = CARTESIAN_POINT ( 'NONE',  ( 0.9873396505805591694, -0.1113553986120547346, 0.8316929133858268486 ) ) ;
#32846 = VECTOR ( 'NONE', #5196, 39.37007874015748854 ) ;
#32847 = CARTESIAN_POINT ( 'NONE',  ( -1.284448818897637956, 0.000000000000000000, 1.181102362204724310 ) ) ;
#32849 = CARTESIAN_POINT ( 'NONE',  ( -0.8107537697050254399, -0.1574803149606297803, 0.8243110236220465570 ) ) ;
#32848 = PLANE ( 'NONE',  #35482 ) ;
#32850 = CARTESIAN_POINT ( 'NONE',  ( 0.7185039370078739607, 1.928577636452523993E-17, 0.7677165353255432922 ) ) ;
#32851 = ORIENTED_EDGE ( 'NONE', *, *, #29117, .F. ) ;
#32852 = ORIENTED_EDGE ( 'NONE', *, *, #43981, .T. ) ;
#32853 = CARTESIAN_POINT ( 'NONE',  ( -0.1574803149606299191, 0.1003937008949285503, 0.000000000000000000 ) ) ;
#32854 = CARTESIAN_POINT ( 'NONE',  ( 0.1787899950787401882, -1.634350393647023614, -2.189545951927503898E-17 ) ) ;
#32855 = CARTESIAN_POINT ( 'NONE',  ( -0.1574803149606300301, -1.476870078632629868, -0.06523048226347956391 ) ) ;
#32856 = CARTESIAN_POINT ( 'NONE',  ( 0.1264236179284866091, -0.7288385826234015097, -0.1264236179284866091 ) ) ;
#32857 = CARTESIAN_POINT ( 'NONE',  ( -0.8107537697050253289, 0.1574803149606300301, 0.1697834644594022058 ) ) ;
#32858 = CARTESIAN_POINT ( 'NONE',  ( 0.1113553986120547346, -1.026574803149606474, -0.1113553986120547346 ) ) ;
#32859 = CARTESIAN_POINT ( 'NONE',  ( 0.9873396505805591694, 0.1113553986120547346, 0.9498031494987716483 ) ) ;
#32860 = ( BOUNDED_CURVE ( )  B_SPLINE_CURVE ( 2, ( #3514, #28461, #24606, #32045, #18125, #13579, #43032, #43282, #39670 ),
 .UNSPECIFIED., .F., .T. ) 
 B_SPLINE_CURVE_WITH_KNOTS ( ( 3, 2, 2, 2, 3 ),
 ( 0.8699999999999999956, 0.8725000000000000533, 0.8750000000000000000, 0.8774999999999999467, 0.8800000000000000044 ),
 .UNSPECIFIED. ) 
 CURVE ( )  GEOMETRIC_REPRESENTATION_ITEM ( )  RATIONAL_B_SPLINE_CURVE ( ( 1.000000000000000000, 0.9238795325112869605, 1.000000000000000000, 0.9238795325112869605, 1.000000000000000000, 0.9238795325112869605, 1.000000000000000000, 0.9238795325112869605, 1.000000000000000000 ) ) 
 REPRESENTATION_ITEM ( '' )  ) ;
#32861 = ORIENTED_EDGE ( 'NONE', *, *, #36274, .T. ) ;
#32862 = ORIENTED_EDGE ( 'NONE', *, *, #42616, .F. ) ;
#32863 = CARTESIAN_POINT ( 'NONE',  ( -0.7495606340400177148, -0.1264236179284866091, 1.665846456639149764 ) ) ;
#32864 = ORIENTED_EDGE ( 'NONE', *, *, #32024, .F. ) ;
#32865 = CARTESIAN_POINT ( 'NONE',  ( 0.7495606340400177148, -0.1264236179284866091, 1.547736220418677089 ) ) ;
#32866 = CARTESIAN_POINT ( 'NONE',  ( -0.1113553986120547346, -1.321850393593259732, -0.1113553986120547346 ) ) ;
#32867 = CARTESIAN_POINT ( 'NONE',  ( -1.054774247047244540, -0.07405724077823318263, 0.8513779527021426707 ) ) ;
#32868 = CARTESIAN_POINT ( 'NONE',  ( 0.8019270111902717657, 0.1787899950787401604, 0.2755905511273391006 ) ) ;
#32869 = CARTESIAN_POINT ( 'NONE',  ( 0.9500414927467377701, 0.1787899950787401604, 0.7037401574265510495 ) ) ;
#32870 = CARTESIAN_POINT ( 'NONE',  ( -0.8759842519685039353, -0.1787899950787401882, 0.7209645668753701386 ) ) ;
#32871 = CARTESIAN_POINT ( 'NONE',  ( 0.005401850751818003393, -0.09279043093872742232, 0.1148724510410191468 ) ) ;
#32872 = EDGE_CURVE ( 'NONE', #41698, #13201, #22854, .T. ) ;
#32873 = CARTESIAN_POINT ( 'NONE',  ( -1.033464566929133799, 0.000000000000000000, 0.8759842519685039353 ) ) ;
#32874 = CARTESIAN_POINT ( 'NONE',  ( -0.6971942568897648851, -0.07405724077823297447, 1.545275590497416696 ) ) ;
#32875 = CARTESIAN_POINT ( 'NONE',  ( -0.7185039370078746268, -0.06523048226347956391, 1.833169291231055542 ) ) ;
#32876 = ORIENTED_EDGE ( 'NONE', *, *, #22835, .T. ) ;
#32877 = CARTESIAN_POINT ( 'NONE',  ( 0.5660731898098425585, 1.205361022782824954E-17, -0.09842519685039370636 ) ) ;
#32878 = LINE ( 'NONE', #14644, #46563 ) ;
#32879 = CARTESIAN_POINT ( 'NONE',  ( 0.6971942568897648851, -0.07405724077823297447, 1.505905511757261062 ) ) ;
#32880 = CARTESIAN_POINT ( 'NONE',  ( 0.1188652514094255819, -0.09851384370095650489, -0.1576607626576320975 ) ) ;
#32881 = CARTESIAN_POINT ( 'NONE',  ( 0.1184675242425285574, -0.5708661417322835607, 1.224299699984019663 ) ) ;
#32882 = ORIENTED_EDGE ( 'NONE', *, *, #9376, .F. ) ;
#32883 = EDGE_CURVE ( 'NONE', #40149, #28164, #12378, .T. ) ;
#32884 = AXIS2_PLACEMENT_3D ( 'NONE', #22662, #27233, #30368 ) ;
#32885 = ORIENTED_EDGE ( 'NONE', *, *, #30888, .F. ) ;
#32886 = VECTOR ( 'NONE', #618, 39.37007874015748143 ) ;
#32887 = ORIENTED_EDGE ( 'NONE', *, *, #15044, .T. ) ;
#32888 = DIRECTION ( 'NONE',  ( 0.000000000000000000, -1.000000000000000000, 0.000000000000000000 ) ) ;
#32889 = CARTESIAN_POINT ( 'NONE',  ( -0.07405724077823318263, -0.9133858267178897039, -0.1787899950787401604 ) ) ;
#32890 = DIRECTION ( 'NONE',  ( 0.000000000000000000, -1.000000000000000000, 0.000000000000000000 ) ) ;
#32891 = DIRECTION ( 'NONE',  ( -1.000000000000000000, 0.000000000000000000, 0.000000000000000000 ) ) ;
#32892 = CARTESIAN_POINT ( 'NONE',  ( 0.7495606340400177148, 0.1264236179284866091, 1.769192913332062966 ) ) ;
#32893 = CARTESIAN_POINT ( 'NONE',  ( 0.8759842519685039353, -0.1787899950787401882, 0.3666338582139531677 ) ) ;
#32894 = CARTESIAN_POINT ( 'NONE',  ( -0.1270800023317771588, -0.2323272741499747829, 0.1270800023317771588 ) ) ;
#32895 = CARTESIAN_POINT ( 'NONE',  ( -0.1264236179284866091, -0.1689231808276639435, 0.1264236179284866091 ) ) ;
#32896 = CARTESIAN_POINT ( 'NONE',  ( 0.07405724077823318263, -0.3031496062454492879, 0.1787899950787401604 ) ) ;
#32897 = CARTESIAN_POINT ( 'NONE',  ( -0.1787899950787401604, -0.08661417317458304510, -0.07405724077823318263 ) ) ;
#32898 = CARTESIAN_POINT ( 'NONE',  ( 0.2471883443658805524, -0.06218794471796348922, -0.1039611462658963509 ) ) ;
#32899 = CARTESIAN_POINT ( 'NONE',  ( 1.054774247047244096, 0.000000000000000000, 0.6520669290800944484 ) ) ;
#32900 = AXIS2_PLACEMENT_3D ( 'NONE', #14868, #17972, #29528 ) ;
#32902 = CARTESIAN_POINT ( 'NONE',  ( 0.8759842519685039353, 0.000000000000000000, 4.498031496062992574 ) ) ;
#32901 = CARTESIAN_POINT ( 'NONE',  ( -0.9225890239890590649, 0.1652722632748837295, 0.03937007874015842346 ) ) ;
#32904 = CARTESIAN_POINT ( 'NONE',  ( -0.8561525976674764227, -0.1729235199935184042, 1.987843333062883522 ) ) ;
#32903 = CARTESIAN_POINT ( 'NONE',  ( -0.8070866141732283561, 0.000000000000000000, -0.6580708661417323802 ) ) ;
#32905 = CARTESIAN_POINT ( 'NONE',  ( -0.07405724077823318263, -0.4655511810485986057, 0.1787899950787401604 ) ) ;
#32906 = CARTESIAN_POINT ( 'NONE',  ( 0.7185039370078741827, 0.06523048226347841205, 0.9621062991050717272 ) ) ;
#32907 = CARTESIAN_POINT ( 'NONE',  ( 0.7495606340400177148, -0.1264236179284866091, 1.744586614119464807 ) ) ;
#32909 = CARTESIAN_POINT ( 'NONE',  ( 0.7185039370078746268, 0.06523048226347956391, 0.1353346455617644717 ) ) ;
#32908 = CARTESIAN_POINT ( 'NONE',  ( -0.1528784791658471254, -0.09445537554013620773, 0.1971681403758093198 ) ) ;
#32910 = CARTESIAN_POINT ( 'NONE',  ( 0.9500414927467377701, 0.1787899950787401604, 0.5019685038832443214 ) ) ;
#32911 = CARTESIAN_POINT ( 'NONE',  ( 0.1787899950787401882, -0.3400590550643468601, -2.189545951927503898E-17 ) ) ;
#32913 = CARTESIAN_POINT ( 'NONE',  ( -0.8107537697050254399, 0.1574803149606300301, 0.1796259842519686567 ) ) ;
#32912 = CARTESIAN_POINT ( 'NONE',  ( -0.9500414927467378812, 0.1787899950787401604, 0.4675196849856070869 ) ) ;
#32914 = AXIS2_PLACEMENT_3D ( 'NONE', #24479, #39071, #35511 ) ;
#32915 = CARTESIAN_POINT ( 'NONE',  ( 0.1264236179284866091, -1.127460629867496067, 0.1264236179284866091 ) ) ;
#32916 = CARTESIAN_POINT ( 'NONE',  ( 1.002407869896990045, 0.1264236179284866091, 0.1107283464029293202 ) ) ;
#32917 = LINE ( 'NONE', #43900, #26225 ) ;
#32918 = CARTESIAN_POINT ( 'NONE',  ( -0.8019270111902717657, -0.1787899950787401604, 1.663385826717890925 ) ) ;
#32919 = VERTEX_POINT ( 'NONE', #4377 ) ;
#32920 = CARTESIAN_POINT ( 'NONE',  ( -0.7495606340400177148, -0.1264236179284866091, 1.154035433017102319 ) ) ;
#32922 = CIRCLE ( 'NONE', #711, 0.5708661417322833387 ) ;
#32921 = CARTESIAN_POINT ( 'NONE',  ( -0.7646288533564489232, 0.1113553986120547346, 0.3395669291338583307 ) ) ;
#32923 = CARTESIAN_POINT ( 'NONE',  ( 1.054774247047244540, -0.07405724077823318263, 1.166338582623402509 ) ) ;
#32924 = CARTESIAN_POINT ( 'NONE',  ( 0.06523048226347956391, -1.132381889656252527, -0.1574803149606300301 ) ) ;
#32925 = CARTESIAN_POINT ( 'NONE',  ( 0.6971942568897648851, 0.07405724077823318263, 1.889763779473794258 ) ) ;
#32926 = CARTESIAN_POINT ( 'NONE',  ( -1.002407869896990045, -0.1264236179284866091, 1.119586614119464585 ) ) ;
#32927 = CARTESIAN_POINT ( 'NONE',  ( 0.1592537043533390206, 0.09805585504226257965, -0.1110897172142509826 ) ) ;
#32928 = CARTESIAN_POINT ( 'NONE',  ( -0.1982027233128455801, -0.1810618366036195193, -0.05428606100832154835 ) ) ;
#32929 = CARTESIAN_POINT ( 'NONE',  ( 0.8759842519685039353, -0.1787899950787401882, 0.2928149605761578567 ) ) ;
#32930 = CARTESIAN_POINT ( 'NONE',  ( -0.8019270111902716547, 0.1787899950787401604, 0.1919291338045042705 ) ) ;
#32931 = CARTESIAN_POINT ( 'NONE',  ( -0.9500414927467378812, 0.1787899950787401604, 0.7381889763241898939 ) ) ;
#32932 = ORIENTED_EDGE ( 'NONE', *, *, #42126, .T. ) ;
#32933 = EDGE_CURVE ( 'NONE', #27914, #11128, #34362, .T. ) ;
#32934 = CARTESIAN_POINT ( 'NONE',  ( 3.284318927891251994E-17, 0.04379921265218874454, 0.1787899950787401882 ) ) ;
#32935 = CARTESIAN_POINT ( 'NONE',  ( 0.8759842519685039353, 0.1787899950787401882, 0.7849409448281259305 ) ) ;
#32936 = CARTESIAN_POINT ( 'NONE',  ( 0.6971942568897648851, -0.07405724077823297447, 1.112204724355684959 ) ) ;
#32937 = CARTESIAN_POINT ( 'NONE',  ( -0.6971942568897648851, -0.07405724077823297447, 1.934055118056471567 ) ) ;
#32938 = VERTEX_POINT ( 'NONE', #12329 ) ;
#32939 = EDGE_CURVE ( 'NONE', #36616, #36603, #12566, .T. ) ;
#32940 = CARTESIAN_POINT ( 'NONE',  ( 1.002407869896990045, 0.1264236179284866091, 1.877460629867496067 ) ) ;
#32941 = VECTOR ( 'NONE', #38736, 39.37007874015748143 ) ;
#32942 = LINE ( 'NONE', #43203, #19057 ) ;
#32943 = CARTESIAN_POINT ( 'NONE',  ( 3.284318927891251994E-17, -1.305734204449710889, 0.1787899950787401882 ) ) ;
#32944 = EDGE_LOOP ( 'NONE', ( #20384, #35526, #31694 ) ) ;
#32945 = CARTESIAN_POINT ( 'NONE',  ( -0.1787899950787401882, -0.3154527558517483676, 0.000000000000000000 ) ) ;
#32946 = CARTESIAN_POINT ( 'NONE',  ( -0.9412147342319837628, 0.1574803149606300301, 1.700295275483023172 ) ) ;
#32947 = EDGE_LOOP ( 'NONE', ( #17628, #46011 ) ) ;
#32948 = CARTESIAN_POINT ( 'NONE',  ( 1.054774247047244540, 0.07405724077823318263, 1.205708661363558365 ) ) ;
#32949 = CARTESIAN_POINT ( 'NONE',  ( -0.8759842519685039353, 0.1574803149606299191, 0.8366141731208189825 ) ) ;
#32950 = CIRCLE ( 'NONE', #33714, 0.5905511811023621549 ) ;
#32951 = CARTESIAN_POINT ( 'NONE',  ( -0.7185039370078739607, 0.000000000000000000, -2.869337061179095023E-17 ) ) ;
#32952 = CARTESIAN_POINT ( 'NONE',  ( 0.7185039370078746268, 0.06523048226347956391, 1.956200787401575880 ) ) ;
#32953 = CARTESIAN_POINT ( 'NONE',  ( 0.1787899950787401604, -1.636811023568283341, -0.07405724077823318263 ) ) ;
#32954 = CARTESIAN_POINT ( 'NONE',  ( -0.8759842519685039353, -0.1787899950787401882, 0.4502952755367874427 ) ) ;
#32955 = CARTESIAN_POINT ( 'NONE',  ( -1.033464566929133799, 0.000000000000000000, 0.6692913384751496553 ) ) ;
#32957 = CARTESIAN_POINT ( 'NONE',  ( -0.7123214566016451421, -0.03363891151877827779, 1.983890876906730716 ) ) ;
#32956 = CARTESIAN_POINT ( 'NONE',  ( -0.07444174185955065859, -1.425732785961000282, -0.1797182628040039087 ) ) ;
#32958 = FACE_OUTER_BOUND ( 'NONE', #21390, .T. ) ;
#32959 = CARTESIAN_POINT ( 'NONE',  ( 0.8759842519685039353, -0.1787899950787401882, 1.198326771599779628 ) ) ;
#32960 = CARTESIAN_POINT ( 'NONE',  ( 1.054774247047244540, -0.07405724077823318263, 1.751968503883245987 ) ) ;
#32961 = CARTESIAN_POINT ( 'NONE',  ( 0.3849708276051176936, 0.09842519685039370636, 0.000000000000000000 ) ) ;
#32962 = CARTESIAN_POINT ( 'NONE',  ( 0.1526806705396661357, 0.02761996292092228425, 0.1377952755905511861 ) ) ;
#32963 = CYLINDRICAL_SURFACE ( 'NONE', #8305, 0.1574803149606299191 ) ;
#32965 = CARTESIAN_POINT ( 'NONE',  ( 0.07405724077823318263, 0.1250000000537635492, 0.1787899950787401604 ) ) ;
#32964 = CARTESIAN_POINT ( 'NONE',  ( -0.1113553986120547346, -0.7608267715460158565, 0.1113553986120547346 ) ) ;
#32966 = DIRECTION ( 'NONE',  ( -3.124924761047754241E-15, -0.9006982393225890782, -0.4344452574044144755 ) ) ;
#32967 = CARTESIAN_POINT ( 'NONE',  ( 0.6971942568897626646, -0.07405724077823297447, 0.2017716534895435399 ) ) ;
#32969 = DIRECTION ( 'NONE',  ( 0.000000000000000000, 0.000000000000000000, 1.000000000000000000 ) ) ;
#32968 = CARTESIAN_POINT ( 'NONE',  ( 1.002407869896990045, -0.1264236179284866091, 1.237696850339937038 ) ) ;
#32970 = AXIS2_PLACEMENT_3D ( 'NONE', #30440, #43891, #3875 ) ;
#32971 = DIRECTION ( 'NONE',  ( -2.038787975192215258E-30, -1.000000000000000000, -2.891205793294680298E-16 ) ) ;
#32972 = CARTESIAN_POINT ( 'NONE',  ( -1.054774247047244540, 0.07405724077823318263, 1.245078740103716886 ) ) ;
#32973 = CARTESIAN_POINT ( 'NONE',  ( 0.8107537697050253289, 0.1574803149606300301, 0.7209645668216065895 ) ) ;
#32974 = ORIENTED_EDGE ( 'NONE', *, *, #26366, .F. ) ;
#32975 = CARTESIAN_POINT ( 'NONE',  ( 0.9651916757672701630, 0.1428679945500031245, 0.03937007847211974887 ) ) ;
#32976 = CARTESIAN_POINT ( 'NONE',  ( 0.7185039370078739607, 1.928577636452523993E-17, 0.2657480314960630197 ) ) ;
#32977 = DIRECTION ( 'NONE',  ( 0.000000000000000000, -0.7880107536067200158, 0.6156614753256608452 ) ) ;
#32978 = PRODUCT_DEFINITION_SHAPE ( 'NONE', 'NONE',  #47468 ) ;
#32979 = AXIS2_PLACEMENT_3D ( 'NONE', #30793, #1754, #16397 ) ;
#32980 = CARTESIAN_POINT ( 'NONE',  ( -0.9873396505805591694, -0.1113553986120547346, 0.04429133858267716300 ) ) ;
#32981 = CARTESIAN_POINT ( 'NONE',  ( 1.054774247047244096, 0.000000000000000000, 1.439468503883244210 ) ) ;
#32982 = CARTESIAN_POINT ( 'NONE',  ( -0.9873396505805591694, 0.1113553986120547346, 1.156496062992125928 ) ) ;
#32984 = CARTESIAN_POINT ( 'NONE',  ( -0.8759842519685039353, -0.1574803149606299191, 0.1181102362204724532 ) ) ;
#32983 = DIRECTION ( 'NONE',  ( 1.000000000000000000, 0.000000000000000000, -1.822029033848725275E-16 ) ) ;
#32986 = CIRCLE ( 'NONE', #42135, 0.04921259842519683236 ) ;
#32985 = CARTESIAN_POINT ( 'NONE',  ( 0.1264236179284866091, -0.2121062991588350544, -0.1264236179284866091 ) ) ;
#32987 = EDGE_LOOP ( 'NONE', ( #45129, #6387, #46205, #12473 ) ) ;
#32988 = CYLINDRICAL_SURFACE ( 'NONE', #3100, 0.1574803149606299191 ) ;
#32989 = EDGE_CURVE ( 'NONE', #45437, #27963, #31496, .T. ) ;
#32990 = DIRECTION ( 'NONE',  ( 0.000000000000000000, -1.406820448837680035E-16, -1.000000000000000000 ) ) ;
#32991 = ORIENTED_EDGE ( 'NONE', *, *, #11981, .F. ) ;
#32992 = CARTESIAN_POINT ( 'NONE',  ( 0.6971942568897626646, 0.07405724077823318263, 0.5167322834108034613 ) ) ;
#32993 = ORIENTED_EDGE ( 'NONE', *, *, #34489, .T. ) ;
#32994 = CARTESIAN_POINT ( 'NONE',  ( 0.1113553986120547346, 0.07578740168233012720, 0.1113553986120547346 ) ) ;
#32995 = CARTESIAN_POINT ( 'NONE',  ( -0.6971942568897637749, 2.189545951927499583E-17, 1.109744094434425232 ) ) ;
#32996 = LINE ( 'NONE', #25797, #34843 ) ;
#32997 = EDGE_CURVE ( 'NONE', #3165, #33762, #41264, .T. ) ;
#32998 = CARTESIAN_POINT ( 'NONE',  ( -1.054774247047244096, 0.000000000000000000, 0.8144685038832440993 ) ) ;
#32999 = ADVANCED_FACE ( 'NONE', ( #8229 ), #37471, .T. ) ;
#33000 = CARTESIAN_POINT ( 'NONE',  ( -0.8759842519685039353, 0.1787899950787401882, 0.2731299212060791515 ) ) ;
#33001 = CARTESIAN_POINT ( 'NONE',  ( 0.7185039370078746268, -0.06523048226347956391, 0.6619094488188971281 ) ) ;
#33002 = CARTESIAN_POINT ( 'NONE',  ( -0.4338976377952755703, 0.2362204724409449064, 2.892866454678787531E-17 ) ) ;
#33003 = CARTESIAN_POINT ( 'NONE',  ( -0.07405724077823318263, -0.7570137320087666488, 0.1787899950787401604 ) ) ;
#33004 = EDGE_LOOP ( 'NONE', ( #42081, #26311, #40418 ) ) ;
#33005 = CARTESIAN_POINT ( 'NONE',  ( 0.7185039370078746268, -0.06523048226347956391, 1.055610236220473341 ) ) ;
#33006 = ORIENTED_EDGE ( 'NONE', *, *, #32490, .T. ) ;
#33007 = DIRECTION ( 'NONE',  ( 0.000000000000000000, 0.000000000000000000, 1.000000000000000000 ) ) ;
#33008 = CARTESIAN_POINT ( 'NONE',  ( -0.6971942568897626646, -0.07405724077823297447, 0.7923228345919055560 ) ) ;
#33009 = DIRECTION ( 'NONE',  ( 0.000000000000000000, -0.7880107536067206819, 0.6156614753256598460 ) ) ;
#33010 = AXIS2_PLACEMENT_3D ( 'NONE', #44993, #37840, #26832 ) ;
#33011 = CARTESIAN_POINT ( 'NONE',  ( -0.8019270111902716547, -0.1787899950787401604, 1.786417322780882388 ) ) ;
#33012 = TOROIDAL_SURFACE ( 'NONE', #18435, 0.3444881889763780070, 0.1574803149606299191 ) ;
#33013 = AXIS2_PLACEMENT_3D ( 'NONE', #43351, #32612, #47199 ) ;
#33014 = CARTESIAN_POINT ( 'NONE',  ( 1.033464566929133799, 0.000000000000000000, 0.2755905510735752184 ) ) ;
#33015 = CARTESIAN_POINT ( 'NONE',  ( 1.033464566929134687, 0.06523048226347956391, 0.6422244094488182009 ) ) ;
#33016 = CARTESIAN_POINT ( 'NONE',  ( 0.1797182628040039087, -0.8499453843861957125, 0.07444174185955046430 ) ) ;
#33017 = CARTESIAN_POINT ( 'NONE',  ( 0.09806891812721182933, -0.2388741431486400835, -0.3136338785705766741 ) ) ;
#33018 = CARTESIAN_POINT ( 'NONE',  ( -0.9873396505805591694, -0.1113553986120547346, 1.530511810916094451 ) ) ;
#33019 = CARTESIAN_POINT ( 'NONE',  ( 1.054774247047244540, -0.07405724077823318263, 0.6938976377415123631 ) ) ;
#33020 = LINE ( 'NONE', #36833, #40648 ) ;
#33021 = CARTESIAN_POINT ( 'NONE',  ( 1.033464566929133799, 0.000000000000000000, 1.387795275590551158 ) ) ;
#33023 = CARTESIAN_POINT ( 'NONE',  ( 0.7646288533564489232, -0.1113553986120547346, 1.560039369971212508 ) ) ;
#33022 = CARTESIAN_POINT ( 'NONE',  ( 0.8845810845758348417, -0.1747031431852734129, 1.988336823050417035 ) ) ;
#33024 = CARTESIAN_POINT ( 'NONE',  ( 0.8107537697050254399, 0.1574803149606300301, 0.3272637794200322636 ) ) ;
#33025 = EDGE_LOOP ( 'NONE', ( #37447, #31759 ) ) ;
#33026 = ( BOUNDED_CURVE ( )  B_SPLINE_CURVE ( 2, ( #19097, #22458, #44723, #40188, #40421, #37081, #7605, #22219, #18858 ),
 .UNSPECIFIED., .F., .F. ) 
 B_SPLINE_CURVE_WITH_KNOTS ( ( 3, 2, 2, 2, 3 ),
 ( 0.1499999999999999944, 0.1524999999999999967, 0.1549999999999999989, 0.1575000000000000011, 0.1600000000000000033 ),
 .UNSPECIFIED. ) 
 CURVE ( )  GEOMETRIC_REPRESENTATION_ITEM ( )  RATIONAL_B_SPLINE_CURVE ( ( 1.000000000000000000, 0.9238795325112869605, 1.000000000000000000, 0.9238795325112869605, 1.000000000000000000, 0.9238795325112869605, 1.000000000000000000, 0.9238795325112869605, 1.000000000000000000 ) ) 
 REPRESENTATION_ITEM ( '' )  ) ;
#33028 = CARTESIAN_POINT ( 'NONE',  ( -0.9500414927467378812, -0.1787899950787401604, 1.983267716481667886 ) ) ;
#33027 = CARTESIAN_POINT ( 'NONE',  ( 0.6971942568897648851, 0.07405724077823318263, 0.8267716534895444003 ) ) ;
#33029 = CARTESIAN_POINT ( 'NONE',  ( 0.1264236179284866091, -0.8026574802611967652, -0.1264236179284866091 ) ) ;
#33031 = ( BOUNDED_CURVE ( )  B_SPLINE_CURVE ( 2, ( #31313, #13104, #27735, #41566, #19790, #31083, #30389, #42300, #45648, #19557, #24117, #37780, #30612, #15755, #38010, #34423, #44936, #45177, #5404, #33971, #26772, #1097, #41331, #1570, #12149, #8532, #8772, #30853, #12866, #4934, #42049, #20026, #12397, #23407, #14023, #17140, #21435, #31551, #25286, #20957, #10440, #35603, #13328, #10197, #2742, #17370, #13547, #32007, #35831, #46599, #28423, #24344, #6584, #3219, #39875, #38941, #2977, #6105, #20731, #17610, #43237, #46367, #28184, #32256, #29034, #36436, #42241, #14149, #10563, #43834, #35082, #36199, #24933, #36659, #38667, #5836, #16849, #31490, #17963, #13276, #25165, #17730, #9677, #39751, #32380, #6941, #14386, #20036, #23175, #35147, #12409, #9264, #46142, #27967, #20271 ),
 .UNSPECIFIED., .F., .T. ) 
 B_SPLINE_CURVE_WITH_KNOTS ( ( 3, 2, 2, 2, 2, 2, 2, 2, 2, 2, 2, 2, 2, 2, 2, 2, 2, 2, 2, 2, 2, 2, 2, 2, 2, 2, 2, 2, 2, 2, 2, 2, 2, 2, 2, 2, 2, 2, 2, 2, 2, 2, 2, 2, 2, 2, 2, 3 ),
 ( 0.01375000002627235936, 0.01499999999999999944, 0.01750000000000000167, 0.02000000000000000042, 0.02249999999999999917, 0.02500000000000000139, 0.02750000000000000014, 0.02999999999999999889, 0.03250000000000000111, 0.03500000000000000333, 0.03749999999999999861, 0.04000000000000000083, 0.04250000000000000305, 0.04499999999999999833, 0.04750000000000000056, 0.05000000000000000278, 0.05249999999999999806, 0.05500000000000000028, 0.05750000000000000250, 0.05999999999999999778, 0.06250000000000000000, 0.06500000000000000222, 0.06750000000000000444, 0.07000000000000000666, 0.07249999999999999500, 0.07499999999999999722, 0.07749999999999999944, 0.08000000000000000167, 0.08250000000000000389, 0.08500000000000000611, 0.08749999999999999445, 0.08999999999999999667, 0.09250000000000001277, 0.09500000000000000111, 0.09750000000000000333, 0.1000000000000000056, 0.1024999999999999939, 0.1050000000000000100, 0.1074999999999999983, 0.1100000000000000006, 0.1125000000000000028, 0.1150000000000000050, 0.1174999999999999933, 0.1199999999999999956, 0.1224999999999999978, 0.1250000000000000000, 0.1275000000000000022, 0.1297356019617244005 ),
 .UNSPECIFIED. ) 
 CURVE ( )  GEOMETRIC_REPRESENTATION_ITEM ( )  RATIONAL_B_SPLINE_CURVE ( ( 0.9619397662556429252, 0.9619397670555889235, 1.000000000000000000, 0.9238795325112869605, 1.000000000000000000, 0.9238795325112869605, 1.000000000000000000, 0.9238795325112869605, 1.000000000000000000, 0.9238795325112869605, 1.000000000000000000, 0.9238795325112869605, 1.000000000000000000, 0.9238795325112869605, 1.000000000000000000, 0.9238795325112869605, 1.000000000000000000, 0.9238795325112869605, 1.000000000000000000, 0.9238795325112869605, 1.000000000000000000, 0.9238795325112869605, 1.000000000000000000, 0.9238795325112869605, 1.000000000000000000, 0.9238795325112869605, 1.000000000000000000, 0.9238795325112869605, 1.000000000000000000, 0.9238795325112869605, 1.000000000000000000, 0.9238795325112869605, 1.000000000000000000, 0.9238795325112869605, 1.000000000000000000, 0.9238795325112869605, 1.000000000000000000, 0.9238795325112869605, 1.000000000000000000, 0.9238795325112869605, 1.000000000000000000, 0.9238795325112869605, 1.000000000000000000, 0.9238795325112869605, 1.000000000000000000, 0.9238795325112869605, 1.000000000000000000, 0.9238795325112869605, 1.000000000000000000, 0.9238795325112869605, 1.000000000000000000, 0.9238795325112869605, 1.000000000000000000, 0.9238795325112869605, 1.000000000000000000, 0.9238795325112869605, 1.000000000000000000, 0.9238795325112869605, 1.000000000000000000, 0.9238795325112869605, 1.000000000000000000, 0.9238795325112869605, 1.000000000000000000, 0.9238795325112869605, 1.000000000000000000, 0.9238795325112869605, 1.000000000000000000, 0.9238795325112869605, 1.000000000000000000, 0.9238795325112869605, 1.000000000000000000, 0.9238795325112869605, 1.000000000000000000, 0.9238795325112869605, 1.000000000000000000, 0.9238795325112869605, 1.000000000000000000, 0.9238795325112869605, 1.000000000000000000, 0.9238795325112869605, 1.000000000000000000, 0.9238795325112869605, 1.000000000000000000, 0.9238795325112869605, 1.000000000000000000, 0.9238795325112869605, 1.000000000000000000, 0.9238795325112869605, 1.000000000000000000, 0.9238795325112869605, 1.000000000000000000, 0.9238795325112869605, 1.000000000000000000, 0.9319299734219380626, 0.9856019348059209539 ) ) 
 REPRESENTATION_ITEM ( '' )  ) ;
#33030 = LINE ( 'NONE', #42808, #17754 ) ;
#33032 = EDGE_CURVE ( 'NONE', #24404, #26580, #2379, .T. ) ;
#33033 = CARTESIAN_POINT ( 'NONE',  ( -0.9412147342319837628, 0.1574803149606300301, 1.158956692913385655 ) ) ;
#33034 = CARTESIAN_POINT ( 'NONE',  ( 0.001106411046829922822, -0.1325885082366765888, 0.04596204078548394439 ) ) ;
#33035 = CARTESIAN_POINT ( 'NONE',  ( 0.8759842519685039353, 0.1787899950787401882, 0.9374999999462362288 ) ) ;
#33036 = DIRECTION ( 'NONE',  ( -0.000000000000000000, 0.7880107536067207930, -0.6156614753256598460 ) ) ;
#33037 = CARTESIAN_POINT ( 'NONE',  ( -0.1574803149606300301, -1.604822834645670104, -0.06523048226347956391 ) ) ;
#33038 = DIRECTION ( 'NONE',  ( 0.000000000000000000, 1.000000000000000000, 0.000000000000000000 ) ) ;
#33039 = AXIS2_PLACEMENT_3D ( 'NONE', #3418, #29357, #43899 ) ;
#33040 = UNCERTAINTY_MEASURE_WITH_UNIT (LENGTH_MEASURE( 1.000000000000000082E-05 ), #21619, 'distance_accuracy_value', 'NONE') ;
#33041 = ORIENTED_EDGE ( 'NONE', *, *, #23264, .F. ) ;
#33042 = CARTESIAN_POINT ( 'NONE',  ( -1.002407869896990045, 0.1264236179284866091, 0.1058070865604098382 ) ) ;
#33043 = CARTESIAN_POINT ( 'NONE',  ( -0.9412147342319837628, -0.1574803149606297803, 0.7111220472440957785 ) ) ;
#33045 = CARTESIAN_POINT ( 'NONE',  ( -1.094772975963752103E-17, -1.432578740103716664, -0.1787899950787401882 ) ) ;
#33044 = CARTESIAN_POINT ( 'NONE',  ( -0.06523048226347956391, -0.3006889762704259006, -0.1574803149606300301 ) ) ;
#33046 = CIRCLE ( 'NONE', #29983, 0.3100393700787401619 ) ;
#33047 = STYLED_ITEM ( 'NONE', ( #18576 ), #21111 ) ;
#33048 = CARTESIAN_POINT ( 'NONE',  ( -1.054774247047244540, 0.07405724077823318263, 1.717519684985606476 ) ) ;
#33049 = ORIENTED_EDGE ( 'NONE', *, *, #36965, .F. ) ;
#33050 = VECTOR ( 'NONE', #143, 39.37007874015748143 ) ;
#33051 = CARTESIAN_POINT ( 'NONE',  ( -0.9500414927467378812, -0.1787899950787401604, 0.4133858267178901480 ) ) ;
#33052 = EDGE_CURVE ( 'NONE', #7313, #43008, #15438, .T. ) ;
#33053 = DIRECTION ( 'NONE',  ( 3.469446951953614189E-15, 1.000000000000000000, 1.040834085586084257E-15 ) ) ;
#33054 = CARTESIAN_POINT ( 'NONE',  ( 0.1605321103696441820, 0.05726506528285952441, 0.1404876550525328283 ) ) ;
#33055 = CARTESIAN_POINT ( 'NONE',  ( 0.08438807215046524590, -0.09131796649090889728, -0.2367113086200097749 ) ) ;
#33056 = CARTESIAN_POINT ( 'NONE',  ( 0.7495606340400177148, 0.1264236179284866091, 0.03690944876513417572 ) ) ;
#33057 = DIRECTION ( 'NONE',  ( 1.944138416145897342E-15, -0.6156614753256602901, -0.7880107536067203489 ) ) ;
#33058 = CARTESIAN_POINT ( 'NONE',  ( -0.1787899950787401882, -0.3706948343709712823, 0.000000000000000000 ) ) ;
#33059 = CARTESIAN_POINT ( 'NONE',  ( -0.1623394077312214634, -0.09842519685039370636, 0.05010053824418583129 ) ) ;
#33060 = DIRECTION ( 'NONE',  ( 1.000000000000000000, 0.000000000000000000, -1.822029033848725275E-16 ) ) ;
#33061 = CARTESIAN_POINT ( 'NONE',  ( -1.054774247047244540, -0.07405724077823318263, 0.3740157479777325711 ) ) ;
#33062 = ORIENTED_EDGE ( 'NONE', *, *, #20241, .F. ) ;
#33063 = ORIENTED_EDGE ( 'NONE', *, *, #16090, .F. ) ;
#33064 = CARTESIAN_POINT ( 'NONE',  ( -0.9500414927467377701, -0.1787899950787401604, 1.358267716481669662 ) ) ;
#33065 = ORIENTED_EDGE ( 'NONE', *, *, #8665, .F. ) ;
#33066 = CARTESIAN_POINT ( 'NONE',  ( 0.07405724077823318263, -1.395669291284819868, -0.1787899950787401604 ) ) ;
#33067 = CARTESIAN_POINT ( 'NONE',  ( -1.094772975963752103E-17, -1.388287401521039355, -0.1787899950787401882 ) ) ;
#33068 = FACE_OUTER_BOUND ( 'NONE', #40901, .T. ) ;
#33069 = CARTESIAN_POINT ( 'NONE',  ( -0.07444174185955065859, -0.5841973528901317492, 0.1797182628040039087 ) ) ;
#33070 = LINE ( 'NONE', #195, #46173 ) ;
#33071 = CARTESIAN_POINT ( 'NONE',  ( -0.7185039370078746268, 0.06523048226347956391, 1.119586614065702035 ) ) ;
#33072 = CARTESIAN_POINT ( 'NONE',  ( 0.8019270111902717657, 0.1787899950787401604, 0.4330708660879683536 ) ) ;
#33073 = CARTESIAN_POINT ( 'NONE',  ( -9.642888182262618425E-18, -0.3129921259842520231, -0.1574803149606299191 ) ) ;
#33074 = CIRCLE ( 'NONE', #12420, 0.09940944881889761386 ) ;
#33075 = AXIS2_PLACEMENT_3D ( 'NONE', #16165, #12339, #5349 ) ;
#33076 = VERTEX_POINT ( 'NONE', #41500 ) ;
#33077 = CYLINDRICAL_SURFACE ( 'NONE', #10833, 0.09842519685039370636 ) ;
#33078 = ORIENTED_EDGE ( 'NONE', *, *, #12457, .T. ) ;
#33079 = EDGE_CURVE ( 'NONE', #21785, #45855, #18472, .T. ) ;
#33080 = CARTESIAN_POINT ( 'NONE',  ( -0.7185039370078739607, 1.928577636452523993E-17, 1.437007873908220601 ) ) ;
#33081 = CARTESIAN_POINT ( 'NONE',  ( 0.8107537697050253289, -0.1574803149606297803, 0.9424212598425207865 ) ) ;
#33082 = FACE_BOUND ( 'NONE', #31720, .T. ) ;
#33083 = EDGE_CURVE ( 'NONE', #25562, #3799, #42939, .T. ) ;
#33085 = DIRECTION ( 'NONE',  ( 0.000000000000000000, 0.2432573283306646017, -0.9699617890481188054 ) ) ;
#33084 = CARTESIAN_POINT ( 'NONE',  ( -0.1586641775163213364, 1.690605217543008632, -0.5092277576975117181 ) ) ;
#33086 = CARTESIAN_POINT ( 'NONE',  ( 1.033464566929133799, 0.000000000000000000, 0.7972440944881890035 ) ) ;
#33087 = EDGE_CURVE ( 'NONE', #3668, #29530, #9178, .T. ) ;
#33088 = CARTESIAN_POINT ( 'NONE',  ( -0.2610236670165032025, 0.1673052798952541498, 0.8873490049157347626 ) ) ;
#33089 = ORIENTED_EDGE ( 'NONE', *, *, #29757, .F. ) ;
#33090 = DIRECTION ( 'NONE',  ( 0.000000000000000000, 1.000000000000000000, 0.000000000000000000 ) ) ;
#33091 = CARTESIAN_POINT ( 'NONE',  ( 0.8107537697050254399, 0.1574803149606300301, 1.154035432963338659 ) ) ;
#33092 = CARTESIAN_POINT ( 'NONE',  ( -0.1787899950787401604, -1.577755905458046115, -0.07405724077823318263 ) ) ;
#33093 = CARTESIAN_POINT ( 'NONE',  ( 0.06523048226347956391, -1.486712598317670553, -0.1574803149606300301 ) ) ;
#33094 = CARTESIAN_POINT ( 'NONE',  ( -0.1787899950787401604, -0.7509842519147402751, 0.07405724077823318263 ) ) ;
#33095 = CARTESIAN_POINT ( 'NONE',  ( 0.06523048226347956391, -1.078248031496062076, 0.1574803149606297803 ) ) ;
#33096 = CARTESIAN_POINT ( 'NONE',  ( 0.8759842519685039353, -0.1574803149606299191, 0.9350393699712126194 ) ) ;
#33097 = CARTESIAN_POINT ( 'NONE',  ( 0.8107537697050254399, 0.1574803149606300301, 0.5339566929133854334 ) ) ;
#33098 = VERTEX_POINT ( 'NONE', #31478 ) ;
#33099 = VERTEX_POINT ( 'NONE', #13718 ) ;
#33100 = ORIENTED_EDGE ( 'NONE', *, *, #31858, .T. ) ;
#33101 = CARTESIAN_POINT ( 'NONE',  ( -0.9500414927467378812, 0.1787899950787401604, 1.609251968450173376 ) ) ;
#33102 = ORIENTED_EDGE ( 'NONE', *, *, #6931, .F. ) ;
#33103 = CARTESIAN_POINT ( 'NONE',  ( 0.7495606340400177148, -0.1264236179284866091, 1.626476377898992132 ) ) ;
#33104 = VERTEX_POINT ( 'NONE', #16838 ) ;
#33105 = CARTESIAN_POINT ( 'NONE',  ( -0.6971942568897626646, 0.07405724077823318263, 0.8710629920722218200 ) ) ;
#33106 = DIRECTION ( 'NONE',  ( 1.000000000000000000, 0.000000000000000000, 0.000000000000000000 ) ) ;
#33107 = CARTESIAN_POINT ( 'NONE',  ( 1.054774247047244540, -0.07405724077823318263, 0.3395669290800945039 ) ) ;
#33108 = CARTESIAN_POINT ( 'NONE',  ( -0.9412147342319837628, 0.1574803149606300301, 0.2534448818897638289 ) ) ;
#33109 = CARTESIAN_POINT ( 'NONE',  ( -0.8759842519685039353, 0.1787899950787401882, 1.213090551127338435 ) ) ;
#33110 = CARTESIAN_POINT ( 'NONE',  ( -0.6971942568897648851, -0.07405724077823297447, 0.6348425196312760255 ) ) ;
#33111 = CARTESIAN_POINT ( 'NONE',  ( 0.000000000000000000, -0.1193342091828949042, 0.06889763779527559306 ) ) ;
#33112 = VECTOR ( 'NONE', #24868, 39.37007874015748143 ) ;
#33113 = CYLINDRICAL_SURFACE ( 'NONE', #14558, 0.1574803149606299191 ) ;
#33114 = CARTESIAN_POINT ( 'NONE',  ( -1.054774247047244540, -0.07405724077823318263, 1.560039370024977057 ) ) ;
#33115 = CARTESIAN_POINT ( 'NONE',  ( -0.9873396505805591694, 0.1113553986120547346, 1.934055118002708573 ) ) ;
#33116 = EDGE_LOOP ( 'NONE', ( #9515, #22422, #41430, #17046 ) ) ;
#33117 = FACE_OUTER_BOUND ( 'NONE', #32826, .T. ) ;
#33118 = CARTESIAN_POINT ( 'NONE',  ( -0.9873396505805591694, -0.1113553986120547346, 1.658464566929134021 ) ) ;
#33119 = CARTESIAN_POINT ( 'NONE',  ( 0.8107537697050254399, 0.1574803149606300301, 1.636318897637794922 ) ) ;
#33120 = CARTESIAN_POINT ( 'NONE',  ( 0.6971942568897648851, -0.07405724077823297447, 1.466535433017102763 ) ) ;
#33121 = CARTESIAN_POINT ( 'NONE',  ( 0.08208618821883129080, -0.09851384146206398906, -0.1770150493296937244 ) ) ;
#33122 = CARTESIAN_POINT ( 'NONE',  ( 0.3246033735368759610, 4.766607801171850497E-17, 0.000000000000000000 ) ) ;
#33123 = AXIS2_PLACEMENT_3D ( 'NONE', #43209, #39619, #36045 ) ;
#33124 = VERTEX_POINT ( 'NONE', #28355 ) ;
#33125 = CIRCLE ( 'NONE', #7833, 0.009842519685039428923 ) ;
#33126 = ORIENTED_EDGE ( 'NONE', *, *, #8219, .F. ) ;
#33127 = ORIENTED_EDGE ( 'NONE', *, *, #33675, .F. ) ;
#33128 = FACE_OUTER_BOUND ( 'NONE', #27574, .T. ) ;
#33129 = CARTESIAN_POINT ( 'NONE',  ( -0.07405724077823318263, -0.4311023621509605386, 0.1787899950787401604 ) ) ;
#33130 = CARTESIAN_POINT ( 'NONE',  ( -1.094772975963752103E-17, -0.9158464566391496531, -0.1787899950787401882 ) ) ;
#33131 = CARTESIAN_POINT ( 'NONE',  ( 0.8019270111902717657, 0.1787899950787401604, 1.806102362150961316 ) ) ;
#33132 = CARTESIAN_POINT ( 'NONE',  ( 3.301370929368692659E-17, -0.2667760930476126280, 0.1797182628040039365 ) ) ;
#33133 = CARTESIAN_POINT ( 'NONE',  ( 0.07405724077823318263, -0.08280113358356940012, 0.1787899950787401604 ) ) ;
#33134 = CARTESIAN_POINT ( 'NONE',  ( 3.284318927891251994E-17, -0.1136811023084411398, 0.1787899950787401882 ) ) ;
#33135 = CARTESIAN_POINT ( 'NONE',  ( 0.2471922904502826812, -0.03219022224904102836, -0.1427165354330708902 ) ) ;
#33136 = EDGE_CURVE ( 'NONE', #23920, #11484, #75, .T. ) ;
#33137 = CARTESIAN_POINT ( 'NONE',  ( 0.7495606340400177148, -0.1264236179284866091, 0.7160433070328504623 ) ) ;
#33138 = ( BOUNDED_CURVE ( )  B_SPLINE_CURVE ( 2, ( #14425, #18004, #47243, #11077, #25696, #2669, #29077, #43635, #10844 ),
 .UNSPECIFIED., .F., .T. ) 
 B_SPLINE_CURVE_WITH_KNOTS ( ( 3, 2, 2, 2, 3 ),
 ( 0.5200000000000000178, 0.5224999999999999645, 0.5250000000000000222, 0.5274999999999999689, 0.5300000000000000266 ),
 .UNSPECIFIED. ) 
 CURVE ( )  GEOMETRIC_REPRESENTATION_ITEM ( )  RATIONAL_B_SPLINE_CURVE ( ( 1.000000000000000000, 0.9238795325112869605, 1.000000000000000000, 0.9238795325112869605, 1.000000000000000000, 0.9238795325112869605, 1.000000000000000000, 0.9238795325112869605, 1.000000000000000000 ) ) 
 REPRESENTATION_ITEM ( '' )  ) ;
#33139 = ADVANCED_FACE ( 'NONE', ( #17547 ), #12802, .F. ) ;
#33140 = VECTOR ( 'NONE', #23927, 39.37007874015748143 ) ;
#33142 = LENGTH_MEASURE_WITH_UNIT ( LENGTH_MEASURE( 0.02539999999999999897 ), #26172 ) ;
#33141 = DIRECTION ( 'NONE',  ( -1.000000000000000000, 0.000000000000000000, 0.000000000000000000 ) ) ;
#33143 = CARTESIAN_POINT ( 'NONE',  ( 1.229559056033039366E-16, 0.000000000000000000, 0.4921259842519680183 ) ) ;
#33144 = CARTESIAN_POINT ( 'NONE',  ( 0.8759842519685039353, 0.000000000000000000, 4.498031496062992574 ) ) ;
#33145 = CARTESIAN_POINT ( 'NONE',  ( 0.6971942568897648851, -0.07405724077823297447, 1.781496062938362934 ) ) ;
#33147 = FACE_OUTER_BOUND ( 'NONE', #46284, .T. ) ;
#33146 = CARTESIAN_POINT ( 'NONE',  ( -0.2471922904502826812, -0.03219022224904102836, 0.1427165354330708902 ) ) ;
#33148 = CARTESIAN_POINT ( 'NONE',  ( 0.6971942568897648851, 0.07405724077823318263, 0.5118110235682844511 ) ) ;
#33149 = EDGE_CURVE ( 'NONE', #19564, #30530, #12274, .T. ) ;
#33150 = AXIS2_PLACEMENT_3D ( 'NONE', #4109, #29101, #25486 ) ;
#33151 = ORIENTED_EDGE ( 'NONE', *, *, #12809, .T. ) ;
#33152 = EDGE_CURVE ( 'NONE', #35903, #6796, #17159, .T. ) ;
#33153 = CARTESIAN_POINT ( 'NONE',  ( 0.7185039370078746268, -0.06523048226347956391, 0.07135826771653554224 ) ) ;
#33154 = CARTESIAN_POINT ( 'NONE',  ( 0.1608809465420316664, -0.07793157280922068109, 0.1406091075617787456 ) ) ;
#33155 = CARTESIAN_POINT ( 'NONE',  ( -0.1264236179284866091, -0.2465551180564728440, -0.1264236179284866091 ) ) ;
#33157 = CARTESIAN_POINT ( 'NONE',  ( 0.1599045142068304115, 0.09467125711649578002, 0.1169792578045390219 ) ) ;
#33156 = CARTESIAN_POINT ( 'NONE',  ( -0.8019270111902717657, -0.1787899950787401604, 0.4084645668753704717 ) ) ;
#33158 = CARTESIAN_POINT ( 'NONE',  ( 0.1787899950787401604, -1.006889763725763220, 0.07405724077823318263 ) ) ;
#33159 = CARTESIAN_POINT ( 'NONE',  ( 0.8759842519685039353, 0.1787899950787401882, 0.2337598424659216578 ) ) ;
#33160 = LINE ( 'NONE', #30965, #23928 ) ;
#33161 = CARTESIAN_POINT ( 'NONE',  ( -0.9500414927467378812, -0.1787899950787401604, 1.550196850339937926 ) ) ;
#33162 = ORIENTED_EDGE ( 'NONE', *, *, #18298, .F. ) ;
#33163 = CIRCLE ( 'NONE', #26282, 0.2047244094488188948 ) ;
#33164 = CARTESIAN_POINT ( 'NONE',  ( -0.7495606340400177148, 0.1264236179284866091, 1.144192913332062966 ) ) ;
#33165 = CARTESIAN_POINT ( 'NONE',  ( 0.1377952755905511306, 0.000000000000000000, -0.3149606299212598381 ) ) ;
#33166 = CARTESIAN_POINT ( 'NONE',  ( 0.7495606340400177148, -0.1264236179284866091, 1.936515747977732405 ) ) ;
#33167 = CARTESIAN_POINT ( 'NONE',  ( -0.8107537697050253289, -0.1574803149606297803, 0.6274606299212601712 ) ) ;
#33168 = CARTESIAN_POINT ( 'NONE',  ( -1.054774247047244540, -0.07405724077823318263, 1.122047244040725644 ) ) ;
#33169 = CARTESIAN_POINT ( 'NONE',  ( 0.1566053014577397373, 0.1284161769476721560, -0.05833949276666106076 ) ) ;
#33170 = CARTESIAN_POINT ( 'NONE',  ( -0.1635016310872839662, -0.2010965215412215124, -0.03441347972012470668 ) ) ;
#33171 = CARTESIAN_POINT ( 'NONE',  ( 0.8019270111902716547, -0.1787899950787401604, 0.3690944881352128393 ) ) ;
#33172 = CARTESIAN_POINT ( 'NONE',  ( -0.8759842519685039353, -0.1787899950787401882, 0.1697834645131655606 ) ) ;
#33173 = CARTESIAN_POINT ( 'NONE',  ( -1.054774247047244540, 0.07405724077823318263, 0.8120078739619844832 ) ) ;
#33174 = ORIENTED_EDGE ( 'NONE', *, *, #4210, .F. ) ;
#33175 = ( BOUNDED_CURVE ( )  B_SPLINE_CURVE ( 2, ( #41658, #1662, #20355, #34992, #27111, #9583, #41895, #13414, #9347 ),
 .UNSPECIFIED., .F., .T. ) 
 B_SPLINE_CURVE_WITH_KNOTS ( ( 3, 2, 2, 2, 3 ),
 ( 0.7900000000000000355, 0.7924999999999999822, 0.7950000000000000400, 0.7974999999999999867, 0.8000000000000000444 ),
 .UNSPECIFIED. ) 
 CURVE ( )  GEOMETRIC_REPRESENTATION_ITEM ( )  RATIONAL_B_SPLINE_CURVE ( ( 1.000000000000000000, 0.9238795325112869605, 1.000000000000000000, 0.9238795325112869605, 1.000000000000000000, 0.9238795325112869605, 1.000000000000000000, 0.9238795325112869605, 1.000000000000000000 ) ) 
 REPRESENTATION_ITEM ( '' )  ) ;
#33176 = CARTESIAN_POINT ( 'NONE',  ( 0.1264236179284866091, -0.03001968498560653523, 0.1264236179284866091 ) ) ;
#33177 = EDGE_LOOP ( 'NONE', ( #4082, #3333, #18991, #41529 ) ) ;
#33178 = CARTESIAN_POINT ( 'NONE',  ( 0.8759842519685039353, -0.1787899950787401882, 0.8833661416785196785 ) ) ;
#33179 = CARTESIAN_POINT ( 'NONE',  ( 1.002407869896990045, 0.1264236179284866091, 1.055610236166708793 ) ) ;
#33180 = CARTESIAN_POINT ( 'NONE',  ( -1.054774247047244540, -0.07405724077823318263, 1.791338582623401177 ) ) ;
#33181 = ORIENTED_EDGE ( 'NONE', *, *, #23599, .F. ) ;
#33182 = DIRECTION ( 'NONE',  ( 0.000000000000000000, 1.000000000000000000, 0.000000000000000000 ) ) ;
#33183 = CARTESIAN_POINT ( 'NONE',  ( -0.1264236179284866091, -1.359868062717427328, -0.1264236179284866091 ) ) ;
#33184 = ORIENTED_EDGE ( 'NONE', *, *, #29757, .T. ) ;
#33185 = CARTESIAN_POINT ( 'NONE',  ( -0.1787899950787401604, -0.2391732282926934683, -0.07405724077823318263 ) ) ;
#33186 = LINE ( 'NONE', #32710, #20830 ) ;
#33187 = ORIENTED_EDGE ( 'NONE', *, *, #16149, .F. ) ;
#33188 = CARTESIAN_POINT ( 'NONE',  ( 0.9500414927467378812, 0.1787899950787401604, 1.249999999946235896 ) ) ;
#33189 = ADVANCED_FACE ( 'NONE', ( #24721 ), #39321, .T. ) ;
#33190 = AXIS2_PLACEMENT_3D ( 'NONE', #37559, #16015, #8319 ) ;
#33192 = ADVANCED_FACE ( 'NONE', ( #4099 ), #47011, .T. ) ;
#33191 = CYLINDRICAL_SURFACE ( 'NONE', #17209, 0.1574803149606299191 ) ;
#33193 = DIRECTION ( 'NONE',  ( -0.000000000000000000, 1.000000000000000000, -0.000000000000000000 ) ) ;
#33194 = AXIS2_PLACEMENT_3D ( 'NONE', #22645, #8253, #351 ) ;
#33195 = CARTESIAN_POINT ( 'NONE',  ( 0.7495606340400177148, -0.1264236179284866091, 0.1254921259304885850 ) ) ;
#33196 = CARTESIAN_POINT ( 'NONE',  ( 0.07405724077823318263, -1.631889763725764553, -0.1787899950787401604 ) ) ;
#33197 = CARTESIAN_POINT ( 'NONE',  ( 0.1264236179284866091, -1.668799212544661348, -0.1264236179284866091 ) ) ;
#33198 = PRODUCT_CONTEXT ( 'NONE', #1229, 'mechanical' ) ;
#33199 = EDGE_CURVE ( 'NONE', #34892, #22479, #18721, .T. ) ;
#33200 = CARTESIAN_POINT ( 'NONE',  ( -1.002407869896990045, 0.1264236179284866091, 0.5044291338045039375 ) ) ;
#33201 = DIRECTION ( 'NONE',  ( -0.000000000000000000, 0.7880107536067207930, -0.6156614753256598460 ) ) ;
#33202 = CARTESIAN_POINT ( 'NONE',  ( 0.07444174185955065859, -1.366677667850763056, 0.1797182628040039087 ) ) ;
#33203 = CARTESIAN_POINT ( 'NONE',  ( 1.054774247047244096, 0.000000000000000000, 1.995570866087968520 ) ) ;
#33204 = CARTESIAN_POINT ( 'NONE',  ( 1.054774247047244096, 0.000000000000000000, 1.365649606245448844 ) ) ;
#33205 = CARTESIAN_POINT ( 'NONE',  ( 0.6971942568897637749, 2.189545951927499583E-17, 1.695374015694267822 ) ) ;
#33206 = CARTESIAN_POINT ( 'NONE',  ( 0.9873396505805591694, 0.1113553986120547346, 1.500984251860976171 ) ) ;
#33207 = EDGE_CURVE ( 'NONE', #1339, #38506, #269, .T. ) ;
#33208 = CARTESIAN_POINT ( 'NONE',  ( -1.033464566929133799, 0.000000000000000000, 0.2066929133858267931 ) ) ;
#33209 = PLANE ( 'NONE',  #44248 ) ;
#33210 = CARTESIAN_POINT ( 'NONE',  ( 0.1574803149606299191, -0.5708661417322835607, 0.9783464566929134243 ) ) ;
#33211 = DIRECTION ( 'NONE',  ( -1.000000000000000000, 0.000000000000000000, 0.000000000000000000 ) ) ;
#33212 = CARTESIAN_POINT ( 'NONE',  ( 1.054774247047244540, 0.07405724077823318263, 0.3001968503399373711 ) ) ;
#33213 = CARTESIAN_POINT ( 'NONE',  ( 0.7111015311219361923, -0.04729053972105573544, 0.03937016857757889149 ) ) ;
#33215 = CARTESIAN_POINT ( 'NONE',  ( -0.7185039370078739607, 1.928577636452523993E-17, 1.712598425089322918 ) ) ;
#33214 = CARTESIAN_POINT ( 'NONE',  ( 1.054774247047244540, 0.07405724077823318263, 1.284448818843874518 ) ) ;
#33216 = CARTESIAN_POINT ( 'NONE',  ( 0.000000000000000000, 0.000000000000000000, 0.000000000000000000 ) ) ;
#33217 = CARTESIAN_POINT ( 'NONE',  ( 0.1574803149606299746, 0.3883517482604934012, -0.6419475548153109612 ) ) ;
#33218 = CARTESIAN_POINT ( 'NONE',  ( -0.6971942568897648851, -0.07405724077823297447, 1.264763779473795813 ) ) ;
#33219 = CARTESIAN_POINT ( 'NONE',  ( 0.7185039370078746268, -0.06523048226347956391, 0.6126968502861739330 ) ) ;
#33220 = ORIENTED_EDGE ( 'NONE', *, *, #25514, .F. ) ;
#33221 = DIRECTION ( 'NONE',  ( -1.000000000000000000, -6.679788269418529283E-17, 0.000000000000000000 ) ) ;
#33222 = CARTESIAN_POINT ( 'NONE',  ( 0.8823777864880867350, 0.1740654330852410558, 0.03936977449015421904 ) ) ;
#33223 = CARTESIAN_POINT ( 'NONE',  ( 0.07405724077823318263, -1.799212598371432659, 0.1787899950787401604 ) ) ;
#33224 = ORIENTED_EDGE ( 'NONE', *, *, #37607, .F. ) ;
#33225 = CARTESIAN_POINT ( 'NONE',  ( -0.9412147342319837628, 0.1574803149606300301, 1.592027559055119612 ) ) ;
#33226 = CARTESIAN_POINT ( 'NONE',  ( 1.002407869896990045, 0.1264236179284866091, 1.641240157426551161 ) ) ;
#33228 = CARTESIAN_POINT ( 'NONE',  ( 0.8107537697050254399, 0.1574803149606300301, 1.675688976377952999 ) ) ;
#33227 = FACE_OUTER_BOUND ( 'NONE', #43183, .T. ) ;
#33229 = CARTESIAN_POINT ( 'NONE',  ( -1.094772975963752103E-17, -0.2071850393163153503, -0.1787899950787401882 ) ) ;
#33230 = VERTEX_POINT ( 'NONE', #11089 ) ;
#33231 = DIRECTION ( 'NONE',  ( 1.822029033848725028E-16, 0.000000000000000000, 1.000000000000000000 ) ) ;
#33232 = CARTESIAN_POINT ( 'NONE',  ( -0.07968303789191254205, -0.08956740676301865045, 0.2394271090160087212 ) ) ;
#33233 = AXIS2_PLACEMENT_3D ( 'NONE', #31935, #46523, #6505 ) ;
#33234 = CARTESIAN_POINT ( 'NONE',  ( 0.6971942568897626646, 0.07405724077823318263, 0.6348425196312760255 ) ) ;
#33235 = ORIENTED_EDGE ( 'NONE', *, *, #7906, .T. ) ;
#33236 = CARTESIAN_POINT ( 'NONE',  ( 1.054774247047244540, 0.07405724077823318263, 0.8169291338045038264 ) ) ;
#33237 = CARTESIAN_POINT ( 'NONE',  ( 0.1113553986120547346, 0.1151574804224878013, 0.1113553986120547346 ) ) ;
#33238 = CARTESIAN_POINT ( 'NONE',  ( -0.7495606340400177148, -0.1264236179284866091, 1.232775590497417362 ) ) ;
#33239 = ORIENTED_EDGE ( 'NONE', *, *, #70, .F. ) ;
#33240 = CARTESIAN_POINT ( 'NONE',  ( 1.033464566929133799, 0.000000000000000000, 1.299212598317669221 ) ) ;
#33241 = CARTESIAN_POINT ( 'NONE',  ( -1.002407869896990045, 0.1264236179284866091, 0.1500984251430867999 ) ) ;
#33242 = CARTESIAN_POINT ( 'NONE',  ( 0.8759842519685039353, -0.1574803149606299191, 0.6692913385826771977 ) ) ;
#33243 = FACE_OUTER_BOUND ( 'NONE', #13578, .T. ) ;
#33244 = CARTESIAN_POINT ( 'NONE',  ( 0.1264236179284866091, -0.8283719997253012890, 0.1264236179284866091 ) ) ;
#33245 = ORIENTED_EDGE ( 'NONE', *, *, #25107, .T. ) ;
#33246 = CARTESIAN_POINT ( 'NONE',  ( -0.1787899950787401604, 0.1151574803687242243, -0.07405724077823318263 ) ) ;
#33247 = ORIENTED_EDGE ( 'NONE', *, *, #2899, .F. ) ;
#33248 = CARTESIAN_POINT ( 'NONE',  ( 1.033464566929133799, 0.000000000000000000, 1.220472440837354400 ) ) ;
#33249 = CARTESIAN_POINT ( 'NONE',  ( -0.7495606340400177148, -0.1264236179284866091, 0.7160433070328504623 ) ) ;
#33250 = CARTESIAN_POINT ( 'NONE',  ( -0.9873396505805591694, -0.1113553986120547346, 0.5856299211523150472 ) ) ;
#33251 = ORIENTED_EDGE ( 'NONE', *, *, #39533, .T. ) ;
#33252 = CARTESIAN_POINT ( 'NONE',  ( -0.9500414927467377701, 0.1787899950787401604, 1.766732283410803239 ) ) ;
#33253 = AXIS2_PLACEMENT_3D ( 'NONE', #18375, #14548, #3752 ) ;
#33254 = EDGE_CURVE ( 'NONE', #21841, #11723, #6755, .T. ) ;
#33255 = EDGE_CURVE ( 'NONE', #30178, #30877, #13164, .T. ) ;
#33256 = EDGE_CURVE ( 'NONE', #40227, #46224, #29092, .T. ) ;
#33257 = ( CONVERSION_BASED_UNIT ( 'INCH', #32779 ) LENGTH_UNIT ( ) NAMED_UNIT ( #20658 ) ) ;
#33258 = CARTESIAN_POINT ( 'NONE',  ( -0.8107537697050253289, -0.1574803149606297803, 0.8243110236220465570 ) ) ;
#33259 = CARTESIAN_POINT ( 'NONE',  ( 0.07444174185955065859, -1.051717037929502885, 0.1797182628040039087 ) ) ;
#33260 = CARTESIAN_POINT ( 'NONE',  ( 0.8070866141732283561, -0.0009842519685049383633, -0.7574803149606299524 ) ) ;
#33261 = CARTESIAN_POINT ( 'NONE',  ( -1.033464566929134687, 0.06523048226347956391, 1.577263779420032153 ) ) ;
#33262 = CARTESIAN_POINT ( 'NONE',  ( 0.6971942568897637749, 2.189545951927499583E-17, 0.7947834645131652831 ) ) ;
#33263 = CARTESIAN_POINT ( 'NONE',  ( 0.9500414927467377701, -0.1787899950787401604, 1.353346456639149986 ) ) ;
#33264 = CARTESIAN_POINT ( 'NONE',  ( 0.4755220087074803481, 4.766607801171850497E-17, 0.000000000000000000 ) ) ;
#33265 = CARTESIAN_POINT ( 'NONE',  ( 0.7646288533564489232, 0.1113553986120547346, 1.402559055118110187 ) ) ;
#33267 = DIRECTION ( 'NONE',  ( 1.000000000000000000, 0.000000000000000000, 0.000000000000000000 ) ) ;
#33266 = CARTESIAN_POINT ( 'NONE',  ( 0.8335474968540336205, -0.1679597360014907503, 1.987423594222797574 ) ) ;
#33268 = CARTESIAN_POINT ( 'NONE',  ( 0.8759842519685039353, -0.1574803149606299191, 1.486220472333417142 ) ) ;
#33269 = CARTESIAN_POINT ( 'NONE',  ( 0.1574803149606300301, -0.7042322833570394680, -0.06523048226347956391 ) ) ;
#33271 = CARTESIAN_POINT ( 'NONE',  ( -0.7646288533564489232, -0.1113553986120547346, 1.412401574803149540 ) ) ;
#33270 = CARTESIAN_POINT ( 'NONE',  ( 0.9500414927467377701, 0.1787899950787401604, 0.7775590550643457499 ) ) ;
#33272 = CARTESIAN_POINT ( 'NONE',  ( 0.1264236179284866091, -0.8420275590013542866, -0.1264236179284866091 ) ) ;
#33273 = DIRECTION ( 'NONE',  ( 1.000000000000000000, 0.000000000000000000, -1.822029033848725275E-16 ) ) ;
#33274 = VERTEX_POINT ( 'NONE', #40279 ) ;
#33275 = CARTESIAN_POINT ( 'NONE',  ( 0.8107537697050254399, 0.1574803149606300301, 0.9276574803149607584 ) ) ;
#33276 = CARTESIAN_POINT ( 'NONE',  ( -1.033464566929133799, 1.928577636452524610E-17, 2.869337061179095023E-17 ) ) ;
#33277 = CARTESIAN_POINT ( 'NONE',  ( 0.8019270111902717657, -0.1787899950787401604, 1.033464566875371027 ) ) ;
#33278 = DIRECTION ( 'NONE',  ( 0.000000000000000000, 0.000000000000000000, 1.000000000000000000 ) ) ;
#33279 = CARTESIAN_POINT ( 'NONE',  ( 0.1113553986120547346, -1.705708661417322913, 0.1113553986120547346 ) ) ;
#33280 = DIRECTION ( 'NONE',  ( -3.375873585268818961E-16, -0.2432573283306649070, 0.9699617890481186944 ) ) ;
#33281 = EDGE_LOOP ( 'NONE', ( #12309, #25078, #23734 ) ) ;
#33283 = FACE_OUTER_BOUND ( 'NONE', #39072, .T. ) ;
#33282 = VECTOR ( 'NONE', #22361, 39.37007874015748143 ) ;
#33284 = CARTESIAN_POINT ( 'NONE',  ( -1.054774247047244540, -0.07405724077823318263, 0.2559055117572600624 ) ) ;
#33285 = CARTESIAN_POINT ( 'NONE',  ( -0.9873396505805591694, 0.1113553986120547346, 0.6053149606299212948 ) ) ;
#33286 = VECTOR ( 'NONE', #33732, 39.37007874015748143 ) ;
#33287 = AXIS2_PLACEMENT_3D ( 'NONE', #7757, #33434, #18076 ) ;
#33288 = CARTESIAN_POINT ( 'NONE',  ( -0.9500414927467378812, 0.1787899950787401604, 1.722440944828125930 ) ) ;
#33289 = CARTESIAN_POINT ( 'NONE',  ( -0.7495606340400177148, -0.1264236179284866091, 0.3272637794737956463 ) ) ;
#33290 = CARTESIAN_POINT ( 'NONE',  ( 0.1113553986120547346, -0.03248031485310291788, -0.1113553986120547346 ) ) ;
#33291 = DIRECTION ( 'NONE',  ( 0.000000000000000000, -0.7880107536067225693, 0.6156614753256574035 ) ) ;
#33292 = DIRECTION ( 'NONE',  ( -1.000000000000000000, 0.000000000000000000, 0.000000000000000000 ) ) ;
#33293 = CARTESIAN_POINT ( 'NONE',  ( 0.8759842519685039353, 0.1787899950787401882, 0.03198818892261445085 ) ) ;
#33294 = CARTESIAN_POINT ( 'NONE',  ( -0.2926984831716178959, 0.1026671379286199781, -1.008549658312261510 ) ) ;
#33295 = CARTESIAN_POINT ( 'NONE',  ( -0.1264236179284866091, -0.4445137320087661492, 0.1264236179284866091 ) ) ;
#33296 = CARTESIAN_POINT ( 'NONE',  ( -0.1723610762456844747, -0.08955972947387973171, 0.1519892194067951063 ) ) ;
#33297 = CARTESIAN_POINT ( 'NONE',  ( -0.9500414927467378812, -0.1787899950787401604, 1.043307086560409269 ) ) ;
#33298 = LINE ( 'NONE', #19595, #14212 ) ;
#33299 = CARTESIAN_POINT ( 'NONE',  ( -0.8759842519685039353, -0.1787899950787401882, 0.2878937007336381804 ) ) ;
#33300 = ADVANCED_FACE ( 'NONE', ( #17787 ), #868, .T. ) ;
#33301 = CARTESIAN_POINT ( 'NONE',  ( -0.8759842519685039353, -0.1787899950787401882, 1.395177165300567124 ) ) ;
#33302 = VERTEX_POINT ( 'NONE', #32434 ) ;
#33303 = CARTESIAN_POINT ( 'NONE',  ( 0.07405724077823318263, -1.316929133804503937, -0.1787899950787401604 ) ) ;
#33304 = CARTESIAN_POINT ( 'NONE',  ( 0.1264236179284866091, -1.550688976324188895, -0.1264236179284866091 ) ) ;
#33305 = EDGE_CURVE ( 'NONE', #34485, #43921, #24982, .T. ) ;
#33306 = CARTESIAN_POINT ( 'NONE',  ( 2.892866454678787531E-17, 0.1102362205799679168, 0.1574803149606299191 ) ) ;
#33307 = CARTESIAN_POINT ( 'NONE',  ( 1.001134792037559063, 0.9202755905599605546, 0.000000000000000000 ) ) ;
#33308 = CARTESIAN_POINT ( 'NONE',  ( 0.9412147342319837628, -0.1574803149606297803, 0.3174212598425196763 ) ) ;
#33309 = VECTOR ( 'NONE', #43566, 39.37007874015748143 ) ;
#33310 = DIRECTION ( 'NONE',  ( -1.000000000000000000, 0.000000000000000000, 0.000000000000000000 ) ) ;
#33311 = ( BOUNDED_CURVE ( )  B_SPLINE_CURVE ( 2, ( #16467, #20519, #8789, #5670, #41826, #31329, #9271, #31102, #20279 ),
 .UNSPECIFIED., .F., .T. ) 
 B_SPLINE_CURVE_WITH_KNOTS ( ( 3, 2, 2, 2, 3 ),
 ( 0.6700000000000000400, 0.6724999999999999867, 0.6750000000000000444, 0.6774999999999999911, 0.6800000000000000488 ),
 .UNSPECIFIED. ) 
 CURVE ( )  GEOMETRIC_REPRESENTATION_ITEM ( )  RATIONAL_B_SPLINE_CURVE ( ( 1.000000000000000000, 0.9238795325112899581, 1.000000000000000000, 0.9238795325112869605, 1.000000000000000000, 0.9238795325112869605, 1.000000000000000000, 0.9238795325112869605, 1.000000000000000000 ) ) 
 REPRESENTATION_ITEM ( '' )  ) ;
#33312 = CARTESIAN_POINT ( 'NONE',  ( -0.9873396505805591694, 0.1113553986120547346, 1.028543306979086802 ) ) ;
#33313 = CARTESIAN_POINT ( 'NONE',  ( 0.6971942568897637749, 2.189545951927499583E-17, 0.4404527558517480901 ) ) ;
#33314 = DIRECTION ( 'NONE',  ( -0.000000000000000000, 1.000000000000000000, -0.000000000000000000 ) ) ;
#33315 = CARTESIAN_POINT ( 'NONE',  ( 2.892866454678787531E-17, -0.2539370078740157410, 0.1574803149606299191 ) ) ;
#33316 = AXIS2_PLACEMENT_3D ( 'NONE', #11958, #12434, #26577 ) ;
#33317 = FACE_OUTER_BOUND ( 'NONE', #15671, .T. ) ;
#33318 = EDGE_LOOP ( 'NONE', ( #18507, #2032, #28825, #23372 ) ) ;
#33319 = DIRECTION ( 'NONE',  ( -1.000000000000000000, 0.000000000000000000, 0.000000000000000000 ) ) ;
#33320 = CARTESIAN_POINT ( 'NONE',  ( 0.8107537697050253289, -0.1574803149606297803, 0.9030511811023627100 ) ) ;
#33321 = CARTESIAN_POINT ( 'NONE',  ( 0.7185039370078739607, 1.928577636452523993E-17, 1.368110236220472675 ) ) ;
#33322 = CARTESIAN_POINT ( 'NONE',  ( -0.1574803149606299191, -0.5295275589475905154, 0.000000000000000000 ) ) ;
#33323 = EDGE_CURVE ( 'NONE', #13881, #20346, #25135, .T. ) ;
#33324 = PRODUCT_RELATED_PRODUCT_CATEGORY ( 'part', '', ( #5552 ) ) ;
#33325 = CARTESIAN_POINT ( 'NONE',  ( 0.7185039370078739607, 1.928577636452523993E-17, 1.043307086506645831 ) ) ;
#33326 = CARTESIAN_POINT ( 'NONE',  ( -0.1677809954247694024, -0.08956119031328269031, 0.01526780091050135638 ) ) ;
#33327 = ORIENTED_EDGE ( 'NONE', *, *, #33254, .T. ) ;
#33328 = CARTESIAN_POINT ( 'NONE',  ( 0.7646288533564489232, 0.1113553986120547346, 1.904527558947590515 ) ) ;
#33329 = CARTESIAN_POINT ( 'NONE',  ( 1.033464566929133799, 0.000000000000000000, 1.141732283357039357 ) ) ;
#33330 = CARTESIAN_POINT ( 'NONE',  ( 0.1264236179284866091, -1.560531496009228247, 0.1264236179284866091 ) ) ;
#33331 = CARTESIAN_POINT ( 'NONE',  ( -0.1264236179284866091, -0.6796259841982046357, -0.1264236179284866091 ) ) ;
#33332 = CARTESIAN_POINT ( 'NONE',  ( 0.06523048226347956391, -1.235728346456692384, 0.1574803149606297803 ) ) ;
#33333 = CARTESIAN_POINT ( 'NONE',  ( 1.033464566929133799, 0.000000000000000000, 0.9055118109160944506 ) ) ;
#33334 = DIRECTION ( 'NONE',  ( -1.000000000000000000, 0.000000000000000000, 0.000000000000000000 ) ) ;
#33335 = EDGE_LOOP ( 'NONE', ( #27935, #13368, #44669, #34497 ) ) ;
#33336 = VERTEX_POINT ( 'NONE', #43650 ) ;
#33337 = ORIENTED_EDGE ( 'NONE', *, *, #28155, .F. ) ;
#33338 = CARTESIAN_POINT ( 'NONE',  ( -0.6971942568897648851, 0.07405724077823318263, 1.579724409395055318 ) ) ;
#33339 = CARTESIAN_POINT ( 'NONE',  ( 0.9500414927467378812, 0.1787899950787401604, 1.727362204670645385 ) ) ;
#33340 = CARTESIAN_POINT ( 'NONE',  ( -0.8759842519685039353, 0.1787899950787401882, 0.7849409448281259305 ) ) ;
#33341 = CARTESIAN_POINT ( 'NONE',  ( -0.1171103306480026085, -0.2278805513378966141, -0.3149606299212598381 ) ) ;
#33342 = CARTESIAN_POINT ( 'NONE',  ( 0.9500414927467378812, -0.1787899950787401604, 0.2952755904974176393 ) ) ;
#33343 = DIRECTION ( 'NONE',  ( 0.000000000000000000, 0.000000000000000000, -1.000000000000000000 ) ) ;
#33344 = CARTESIAN_POINT ( 'NONE',  ( -0.8019270111902716547, 0.1787899950787401604, 1.294291338528913204 ) ) ;
#33345 = CARTESIAN_POINT ( 'NONE',  ( -0.8759842519685039353, 0.1787899950787401882, 0.7800196849856062542 ) ) ;
#33346 = CARTESIAN_POINT ( 'NONE',  ( 0.002094777259458696639, -0.1034000088770426068, 0.09649716854689870116 ) ) ;
#33347 = FACE_OUTER_BOUND ( 'NONE', #40225, .T. ) ;
#33348 = CARTESIAN_POINT ( 'NONE',  ( -1.054774247047244096, 0.000000000000000000, 1.601870078686393750 ) ) ;
#33349 = CARTESIAN_POINT ( 'NONE',  ( -0.7646288533564489232, -0.1113553986120547346, 1.874999999892472458 ) ) ;
#33350 = ORIENTED_EDGE ( 'NONE', *, *, #26158, .F. ) ;
#33351 = AXIS2_PLACEMENT_3D ( 'NONE', #42333, #16712, #31583 ) ;
#33353 = LINE ( 'NONE', #33826, #12658 ) ;
#33352 = AXIS2_PLACEMENT_3D ( 'NONE', #7855, #8090, #33774 ) ;
#33354 = CARTESIAN_POINT ( 'NONE',  ( -0.8107537697050253289, -0.1574803149606297803, 1.651082677165354839 ) ) ;
#33355 = CARTESIAN_POINT ( 'NONE',  ( 0.2056049205965837234, -0.3271121446598783677, -1.056443147991412923 ) ) ;
#33356 = CARTESIAN_POINT ( 'NONE',  ( 0.6971942568897637749, 2.189545951927499583E-17, 1.464074803095842370 ) ) ;
#33357 = CARTESIAN_POINT ( 'NONE',  ( 0.0003609363526977173468, -0.09851383234819251211, 0.1560916676376958856 ) ) ;
#33358 = CARTESIAN_POINT ( 'NONE',  ( -0.9412147342319837628, 0.1574803149606300301, 0.3617125983176697201 ) ) ;
#33359 = CIRCLE ( 'NONE', #26463, 0.6872114956789353579 ) ;
#33360 = CIRCLE ( 'NONE', #5034, 0.1003937007874010356 ) ;
#33361 = ORIENTED_EDGE ( 'NONE', *, *, #30319, .F. ) ;
#33362 = EDGE_CURVE ( 'NONE', #31223, #34218, #46028, .T. ) ;
#33363 = EDGE_CURVE ( 'NONE', #17196, #44204, #14088, .T. ) ;
#33364 = EDGE_LOOP ( 'NONE', ( #20759, #7199, #665, #38624, #2344 ) ) ;
#33365 = CARTESIAN_POINT ( 'NONE',  ( 0.1787899950787401882, -0.9699803149068660924, -2.189545951927503898E-17 ) ) ;
#33366 = CARTESIAN_POINT ( 'NONE',  ( 0.1787899950787401604, -0.4557086613635593086, -0.07405724077823318263 ) ) ;
#33367 = CARTESIAN_POINT ( 'NONE',  ( -0.1787899950787401882, -0.8666338582139527791, 0.000000000000000000 ) ) ;
#33368 = CARTESIAN_POINT ( 'NONE',  ( 0.9500414927467378812, -0.1787899950787401604, 1.747047244040724312 ) ) ;
#33369 = CARTESIAN_POINT ( 'NONE',  ( 3.301370929368692659E-17, -0.2274060143074551343, 0.1797182628040039365 ) ) ;
#33370 = CARTESIAN_POINT ( 'NONE',  ( 0.1574803149606300301, 0.1126968503937008509, -0.06523048226347956391 ) ) ;
#33371 = PRODUCT ( 'Side Bracket', 'Side Bracket', '', ( #42452 ) ) ;
#33372 = CARTESIAN_POINT ( 'NONE',  ( 0.1787899950787401604, -0.02263779522182706935, -0.07405724077823318263 ) ) ;
#33373 = CARTESIAN_POINT ( 'NONE',  ( 0.6971942568897626646, 0.07405724077823318263, 0.7874015747493863238 ) ) ;
#33374 = EDGE_CURVE ( 'NONE', #35698, #4424, #32146, .T. ) ;
#33376 = FILL_AREA_STYLE_COLOUR ( '', #34636 ) ;
#33375 = CARTESIAN_POINT ( 'NONE',  ( 0.3727034120734909473, 4.616380251121755931E-17, 0.000000000000000000 ) ) ;
#33378 = CARTESIAN_POINT ( 'NONE',  ( -0.9215977125122606362, -0.1699356664333222244, 1.989001160739882312 ) ) ;
#33377 = CARTESIAN_POINT ( 'NONE',  ( 0.2397010884053811242, 0.09842519685039370636, 1.205361022782828805E-17 ) ) ;
#33379 = CARTESIAN_POINT ( 'NONE',  ( 0.7646288533564489232, 0.1113553986120547346, 0.4576771653543307283 ) ) ;
#33380 = CARTESIAN_POINT ( 'NONE',  ( 0.6971942568897637749, 2.189545951927499583E-17, 1.857775590497417362 ) ) ;
#33381 = CARTESIAN_POINT ( 'NONE',  ( 0.000000000000000000, 0.000000000000000000, -0.2886241641379866385 ) ) ;
#33382 = AXIS2_PLACEMENT_3D ( 'NONE', #31238, #38871, #6035 ) ;
#33383 = AXIS2_PLACEMENT_3D ( 'NONE', #17835, #21671, #32478 ) ;
#33384 = CARTESIAN_POINT ( 'NONE',  ( 0.8107537697050253289, 0.1574803149606300301, 0.06151574803149607168 ) ) ;
#33385 = CARTESIAN_POINT ( 'NONE',  ( 0.1237557312196568837, 0.6131769916351970107, -0.8165595533554412810 ) ) ;
#33387 = ADVANCED_FACE ( 'NONE', ( #15154 ), #38127, .T. ) ;
#33386 = CARTESIAN_POINT ( 'NONE',  ( -0.1264236179284866091, -0.2071850393163153503, -0.1264236179284866091 ) ) ;
#33388 = CARTESIAN_POINT ( 'NONE',  ( 0.1644020957507539848, 0.1623118080249112138, 1.367956046207553540E-19 ) ) ;
#33389 = CARTESIAN_POINT ( 'NONE',  ( 0.1787899950787401604, -1.277559055064345861, -0.07405724077823318263 ) ) ;
#33390 = CARTESIAN_POINT ( 'NONE',  ( 0.7495606340400177148, 0.1264236179284866091, 0.1993110235682838682 ) ) ;
#33391 = CARTESIAN_POINT ( 'NONE',  ( 0.1638905441110397043, 0.08063435062917849450, -0.1396622675802317859 ) ) ;
#33392 = CARTESIAN_POINT ( 'NONE',  ( -0.8019270111902717657, -0.1787899950787401604, 1.545275590497416696 ) ) ;
#33393 = ORIENTED_EDGE ( 'NONE', *, *, #45212, .F. ) ;
#33394 = CARTESIAN_POINT ( 'NONE',  ( -0.9500414927467378812, -0.1787899950787401604, 1.161417322780881278 ) ) ;
#33395 = CARTESIAN_POINT ( 'NONE',  ( -0.7185039370078739607, 1.928577636452523993E-17, 0.3444881889763780070 ) ) ;
#33396 = ( REPRESENTATION_RELATIONSHIP ('NONE','NONE', #9609, #7769 ) REPRESENTATION_RELATIONSHIP_WITH_TRANSFORMATION ( #28344 )SHAPE_REPRESENTATION_RELATIONSHIP( ) ) ;
#33397 = CARTESIAN_POINT ( 'NONE',  ( 0.7495606340400177148, -0.1264236179284866091, 1.272145669237574772 ) ) ;
#33398 = CARTESIAN_POINT ( 'NONE',  ( 0.6971942568897648851, 0.07405724077823318263, 1.968503936954110189 ) ) ;
#33399 = CARTESIAN_POINT ( 'NONE',  ( -0.8019270111902717657, -0.1787899950787401604, 1.033464566875371027 ) ) ;
#33400 = CARTESIAN_POINT ( 'NONE',  ( 0.1573602050224861826, 0.1351575695125303012, -0.04671412196441625253 ) ) ;
#33401 = CARTESIAN_POINT ( 'NONE',  ( -0.1976644210311677141, -0.1813726255708516255, -0.05388431474956710543 ) ) ;
#33402 = CARTESIAN_POINT ( 'NONE',  ( 1.054774247047244540, 0.07405724077823318263, 0.3838582676627718127 ) ) ;
#33403 = CARTESIAN_POINT ( 'NONE',  ( -1.054774247047244096, 0.000000000000000000, 0.1796259841982051075 ) ) ;
#33404 = CARTESIAN_POINT ( 'NONE',  ( -0.7495606340400177148, 0.1264236179284866091, 0.7455708660879684091 ) ) ;
#33405 = CARTESIAN_POINT ( 'NONE',  ( 1.033464566929134687, -0.06523048226347956391, 1.729822834538142784 ) ) ;
#33406 = CARTESIAN_POINT ( 'NONE',  ( -1.033464566929133799, 0.000000000000000000, 0.8661417321759370402 ) ) ;
#33407 = EDGE_LOOP ( 'NONE', ( #26021, #40364, #19747, #23770 ) ) ;
#33408 = CARTESIAN_POINT ( 'NONE',  ( 0.7495606340400177148, 0.1264236179284866091, 0.9079724408911180600 ) ) ;
#33409 = CARTESIAN_POINT ( 'NONE',  ( -0.7646288533564489232, -0.1113553986120547346, 0.1131889763779527630 ) ) ;
#33410 = CARTESIAN_POINT ( 'NONE',  ( 0.7495606340400177148, -0.1264236179284866091, 0.9965551180564724554 ) ) ;
#33411 = CARTESIAN_POINT ( 'NONE',  ( -1.002407869896990045, -0.1264236179284866091, 1.985728346402929168 ) ) ;
#33412 = EDGE_LOOP ( 'NONE', ( #15528, #14893, #43606 ) ) ;
#33413 = CIRCLE ( 'NONE', #31117, 0.7874015748031495399 ) ;
#33414 = EDGE_CURVE ( 'NONE', #23956, #7655, #11553, .T. ) ;
#33415 = CARTESIAN_POINT ( 'NONE',  ( 0.8759842519685039353, 0.1787899950787401882, 1.882381889710015743 ) ) ;
#33416 = EDGE_CURVE ( 'NONE', #20097, #27388, #21783, .T. ) ;
#33417 = CARTESIAN_POINT ( 'NONE',  ( -0.7495606340400177148, -0.1264236179284866091, 0.04675196845017354913 ) ) ;
#33418 = CARTESIAN_POINT ( 'NONE',  ( -0.07405724077823318263, -1.386934991851286769, 0.1787899950787401604 ) ) ;
#33419 = EDGE_LOOP ( 'NONE', ( #7035, #23906, #12108, #3364 ) ) ;
#33420 = CARTESIAN_POINT ( 'NONE',  ( -1.094772975963752103E-17, -0.4040354330171023745, -0.1787899950787401882 ) ) ;
#33421 = EDGE_CURVE ( 'NONE', #28468, #41308, #44509, .T. ) ;
#33422 = ORIENTED_EDGE ( 'NONE', *, *, #35122, .T. ) ;
#33423 = CARTESIAN_POINT ( 'NONE',  ( 0.9500414927467378812, -0.1787899950787401604, 1.156496062938362046 ) ) ;
#33424 = EDGE_CURVE ( 'NONE', #19175, #26131, #44577, .T. ) ;
#33425 = LINE ( 'NONE', #538, #29507 ) ;
#33426 = CARTESIAN_POINT ( 'NONE',  ( 0.4330708661417322913, -0.08090551181102362266, 1.098083891755157578E-17 ) ) ;
#33427 = ( BOUNDED_CURVE ( )  B_SPLINE_CURVE ( 2, ( #23408, #29286, #3815, #38012, #12398, #11032, #18208, #26537, #33086 ),
 .UNSPECIFIED., .F., .T. ) 
 B_SPLINE_CURVE_WITH_KNOTS ( ( 3, 2, 2, 2, 3 ),
 ( 0.3900000000000000133, 0.3925000000000000155, 0.3950000000000000178, 0.3975000000000000200, 0.4000000000000000222 ),
 .UNSPECIFIED. ) 
 CURVE ( )  GEOMETRIC_REPRESENTATION_ITEM ( )  RATIONAL_B_SPLINE_CURVE ( ( 1.000000000000000000, 0.9238795325112869605, 1.000000000000000000, 0.9238795325112869605, 1.000000000000000000, 0.9238795325112869605, 1.000000000000000000, 0.9238795325112869605, 1.000000000000000000 ) ) 
 REPRESENTATION_ITEM ( '' )  ) ;
#33428 = CARTESIAN_POINT ( 'NONE',  ( 0.8759842519685039353, 0.1787899950787401882, 0.1107283464029295283 ) ) ;
#33429 = CARTESIAN_POINT ( 'NONE',  ( -0.1787899950787401882, -1.698326771599779628, 0.000000000000000000 ) ) ;
#33430 = CARTESIAN_POINT ( 'NONE',  ( 0.07405724077823318263, -1.666338582623402953, -0.1787899950787401604 ) ) ;
#33431 = LINE ( 'NONE', #32305, #7361 ) ;
#33432 = CARTESIAN_POINT ( 'NONE',  ( -0.8759842519685039353, 0.1787899950787401882, 0.7062007873478109987 ) ) ;
#33433 = CARTESIAN_POINT ( 'NONE',  ( -0.1797182628040039087, -1.381441447378320531, -0.07444174185955065859 ) ) ;
#33434 = DIRECTION ( 'NONE',  ( 1.000000000000000000, 0.000000000000000000, 0.000000000000000000 ) ) ;
#33435 = CARTESIAN_POINT ( 'NONE',  ( 0.8019270111902717657, -0.1787899950787401604, 1.313976377898992132 ) ) ;
#33436 = CARTESIAN_POINT ( 'NONE',  ( 0.7495606340400177148, -0.1264236179284866091, 1.700295275536787498 ) ) ;
#33437 = DIRECTION ( 'NONE',  ( -2.114720919224289611E-16, 1.000000000000000000, 0.000000000000000000 ) ) ;
#33438 = CARTESIAN_POINT ( 'NONE',  ( 1.033464566929134687, -0.06523048226347956391, 0.9030511809948349455 ) ) ;
#33439 = CARTESIAN_POINT ( 'NONE',  ( -0.2066929133858267931, 0.2573565155132529481, -0.3015174453633730489 ) ) ;
#33440 = CARTESIAN_POINT ( 'NONE',  ( -0.07405724077823318263, 0.1446850394238423654, -0.1787899950787401604 ) ) ;
#33441 = CARTESIAN_POINT ( 'NONE',  ( 1.033464566929133799, 0.000000000000000000, 0.8759842519685039353 ) ) ;
#33443 = CARTESIAN_POINT ( 'NONE',  ( 1.054774247047244540, 0.07405724077823318263, 0.2608267715997796832 ) ) ;
#33442 = ( BOUNDED_CURVE ( )  B_SPLINE_CURVE ( 2, ( #16680, #5887, #35135, #27730, #45885, #42043, #42293, #5397, #5646 ),
 .UNSPECIFIED., .F., .T. ) 
 B_SPLINE_CURVE_WITH_KNOTS ( ( 3, 2, 2, 2, 3 ),
 ( 0.1100000000000000006, 0.1125000000000000028, 0.1150000000000000050, 0.1174999999999999933, 0.1199999999999999956 ),
 .UNSPECIFIED. ) 
 CURVE ( )  GEOMETRIC_REPRESENTATION_ITEM ( )  RATIONAL_B_SPLINE_CURVE ( ( 1.000000000000000000, 0.9238795325112869605, 1.000000000000000000, 0.9238795325112869605, 1.000000000000000000, 0.9238795325112869605, 1.000000000000000000, 0.9238795325112869605, 1.000000000000000000 ) ) 
 REPRESENTATION_ITEM ( '' )  ) ;
#33445 = CARTESIAN_POINT ( 'NONE',  ( -0.9873396505805591694, 0.1113553986120547346, 1.707677165354330562 ) ) ;
#33444 = CARTESIAN_POINT ( 'NONE',  ( 1.054774247047244540, -0.07405724077823318263, 1.240157480261197875 ) ) ;
#33446 = CARTESIAN_POINT ( 'NONE',  ( 0.6195511811023590720, -5.463695987328343027E-16, 1.186023622047243986 ) ) ;
#33447 = CARTESIAN_POINT ( 'NONE',  ( 0.1574803149606299746, 1.086379535891617065, -0.03715491745705640919 ) ) ;
#33448 = CARTESIAN_POINT ( 'NONE',  ( -0.6971942568897648851, -0.07405724077823297447, 1.186023621993481658 ) ) ;
#33449 = CARTESIAN_POINT ( 'NONE',  ( 1.033464566929133799, 0.000000000000000000, 0.6692913384751496553 ) ) ;
#33450 = EDGE_LOOP ( 'NONE', ( #2030, #46775, #29298, #12077 ) ) ;
#33451 = CARTESIAN_POINT ( 'NONE',  ( -0.8759842519685039353, 0.1574803149606299191, 1.751968503937007871 ) ) ;
#33452 = CARTESIAN_POINT ( 'NONE',  ( -1.033464566929133799, 1.928577636452524610E-17, 2.869337061179095023E-17 ) ) ;
#33453 = ORIENTED_EDGE ( 'NONE', *, *, #47018, .F. ) ;
#33454 = CARTESIAN_POINT ( 'NONE',  ( -0.1797182628040039087, -0.003488691472809330677, -0.07444174185955065859 ) ) ;
#33455 = EDGE_LOOP ( 'NONE', ( #2374, #40827, #39759, #14059 ) ) ;
#33456 = CARTESIAN_POINT ( 'NONE',  ( 0.2431102362204724532, 3.299925748462481561E-17, 0.000000000000000000 ) ) ;
#33457 = CARTESIAN_POINT ( 'NONE',  ( 0.8019270111902717657, 0.1787899950787401604, 1.648622047190331230 ) ) ;
#33458 = CARTESIAN_POINT ( 'NONE',  ( -1.033464566929133799, 0.000000000000000000, 1.102362204616881947 ) ) ;
#33460 = CARTESIAN_POINT ( 'NONE',  ( -1.033464566929134687, -0.06523048226347956391, 0.1254921259842521064 ) ) ;
#33459 = CARTESIAN_POINT ( 'NONE',  ( -0.06523048226347956391, 0.05856299212598428672, 0.1574803149606297803 ) ) ;
#33461 = CARTESIAN_POINT ( 'NONE',  ( 0.7185039370078739607, 1.928577636452523993E-17, 0.3740157479239689664 ) ) ;
#33462 = CARTESIAN_POINT ( 'NONE',  ( 0.1264236179284866091, -0.1825787401037169411, 0.1264236179284866091 ) ) ;
#33463 = ORIENTED_EDGE ( 'NONE', *, *, #28266, .F. ) ;
#33464 = CARTESIAN_POINT ( 'NONE',  ( -0.9873396505805591694, 0.1113553986120547346, 0.3690944881889763884 ) ) ;
#33465 = CARTESIAN_POINT ( 'NONE',  ( -0.08640460078248797526, -0.09201407021823122812, 0.2355472506763592044 ) ) ;
#33466 = ORIENTED_EDGE ( 'NONE', *, *, #40725, .T. ) ;
#33467 = CARTESIAN_POINT ( 'NONE',  ( 1.002407869896990045, 0.1264236179284866091, 0.8981299212060788184 ) ) ;
#33468 = CARTESIAN_POINT ( 'NONE',  ( -0.1574803149606300301, 0.1373031497138262058, -0.06523048226347956391 ) ) ;
#33469 = EDGE_LOOP ( 'NONE', ( #18106, #24298 ) ) ;
#33470 = VECTOR ( 'NONE', #6024, 39.37007874015748143 ) ;
#33471 = EDGE_CURVE ( 'NONE', #4000, #21227, #26414, .T. ) ;
#33472 = DIRECTION ( 'NONE',  ( 1.000000000000000000, 0.000000000000000000, 0.000000000000000000 ) ) ;
#33473 = CARTESIAN_POINT ( 'NONE',  ( -0.6971942568897637749, 2.189545951927499583E-17, 0.2829724408911185041 ) ) ;
#33474 = FACE_OUTER_BOUND ( 'NONE', #33335, .T. ) ;
#33475 = CARTESIAN_POINT ( 'NONE',  ( -0.2066929133858267931, -0.5115148015943089543, -0.8998816658763667542 ) ) ;
#33476 = CARTESIAN_POINT ( 'NONE',  ( 0.1264236179284866091, -0.9858523146859311526, 0.1264236179284866091 ) ) ;
#33477 = ORIENTED_EDGE ( 'NONE', *, *, #998, .T. ) ;
#33478 = DIRECTION ( 'NONE',  ( -0.000000000000000000, 1.000000000000000000, -3.995705278811693553E-31 ) ) ;
#33479 = VERTEX_POINT ( 'NONE', #29798 ) ;
#33480 = CARTESIAN_POINT ( 'NONE',  ( 0.8019270111902717657, 0.1787899950787401604, 1.018700787347811110 ) ) ;
#33481 = EDGE_CURVE ( 'NONE', #41157, #6624, #5286, .T. ) ;
#33482 = CARTESIAN_POINT ( 'NONE',  ( 0.7185039370078746268, -0.06523048226347956391, 1.203248031388535200 ) ) ;
#33483 = DIRECTION ( 'NONE',  ( -1.000000000000000000, 0.000000000000000000, 0.000000000000000000 ) ) ;
#33484 = CARTESIAN_POINT ( 'NONE',  ( 0.5555748031496099415, 0.6449983665207552619, -0.7480314960629921295 ) ) ;
#33485 = CARTESIAN_POINT ( 'NONE',  ( 0.1264236179284866091, -0.5319881889226142357, -0.1264236179284866091 ) ) ;
#33486 = CARTESIAN_POINT ( 'NONE',  ( -1.054774247047244540, 0.07405724077823318263, 0.1082677164816695514 ) ) ;
#33487 = CARTESIAN_POINT ( 'NONE',  ( -0.7185039370078739607, 1.928577636452523993E-17, 0.8169291338582678197 ) ) ;
#33488 = CARTESIAN_POINT ( 'NONE',  ( -0.5314960629921260393, -1.928577636452524610E-17, 4.498031496062992574 ) ) ;
#33489 = CARTESIAN_POINT ( 'NONE',  ( -0.1797182628040039087, -1.061559557614541349, 0.07444174185955065859 ) ) ;
#33490 = CARTESIAN_POINT ( 'NONE',  ( 0.06863485658970966408, -0.2558675481226387327, -0.3097625555229703842 ) ) ;
#33491 = CARTESIAN_POINT ( 'NONE',  ( -0.9412147342319837628, 0.1574803149606300301, 1.582185039262551607 ) ) ;
#33492 = CARTESIAN_POINT ( 'NONE',  ( 1.054774247047244540, 0.07405724077823318263, 0.8562992125446617919 ) ) ;
#33493 = CARTESIAN_POINT ( 'NONE',  ( 0.8019270111902716547, 0.1787899950787401604, 1.373031496009229357 ) ) ;
#33494 = CARTESIAN_POINT ( 'NONE',  ( 0.9412147342319837628, 0.1574803149606300301, 0.5191929132782994172 ) ) ;
#33495 = CARTESIAN_POINT ( 'NONE',  ( 1.033464566929134687, -0.06523048226347956391, 1.385334645669290987 ) ) ;
#33497 = CARTESIAN_POINT ( 'NONE',  ( 0.000000000000000000, 0.000000000000000000, 0.000000000000000000 ) ) ;
#33496 = CARTESIAN_POINT ( 'NONE',  ( 0.7099058204916336434, -0.002335345252131881735, 1.983306857452649341 ) ) ;
#33498 = LINE ( 'NONE', #4214, #20558 ) ;
#33499 = CARTESIAN_POINT ( 'NONE',  ( -0.06523048226347956391, -0.6796259841444414196, 0.1574803149606297803 ) ) ;
#33500 = AXIS2_PLACEMENT_3D ( 'NONE', #3936, #18559, #29641 ) ;
#33501 = CARTESIAN_POINT ( 'NONE',  ( 1.002407869896990045, -0.1264236179284866091, 0.7652559054580472253 ) ) ;
#33502 = CARTESIAN_POINT ( 'NONE',  ( -0.1787899950787401604, -0.7066929133320629663, 0.07405724077823318263 ) ) ;
#33503 = LINE ( 'NONE', #22924, #6242 ) ;
#33504 = ORIENTED_EDGE ( 'NONE', *, *, #42120, .F. ) ;
#33505 = CARTESIAN_POINT ( 'NONE',  ( 0.7185039370078739607, 1.928577636452523993E-17, 0.4133858266641267654 ) ) ;
#33506 = CARTESIAN_POINT ( 'NONE',  ( 0.6195511811023624027, 0.9842519685039370358, -0.7135826771653542844 ) ) ;
#33507 = CARTESIAN_POINT ( 'NONE',  ( 1.054774247047244096, 0.000000000000000000, 1.124507873961984261 ) ) ;
#33508 = LINE ( 'NONE', #34219, #9649 ) ;
#33509 = CARTESIAN_POINT ( 'NONE',  ( 0.06523048226347956391, -1.614665354330708347, -0.1574803149606300301 ) ) ;
#33510 = DIRECTION ( 'NONE',  ( -1.000000000000000000, 0.000000000000000000, 0.000000000000000000 ) ) ;
#33511 = VERTEX_POINT ( 'NONE', #1442 ) ;
#33512 = DIRECTION ( 'NONE',  ( 0.000000000000000000, 1.000000000000000000, 0.000000000000000000 ) ) ;
#33513 = CARTESIAN_POINT ( 'NONE',  ( -0.6971942568897626646, 0.07405724077823318263, 0.2362204723871814960 ) ) ;
#33514 = CARTESIAN_POINT ( 'NONE',  ( 0.7185039370078746268, 0.06523048226347956391, 0.3420275590551182798 ) ) ;
#33515 = CARTESIAN_POINT ( 'NONE',  ( 0.1574803149606299191, -0.3129921258767248138, -1.928577636452523993E-17 ) ) ;
#33516 = LINE ( 'NONE', #31920, #25688 ) ;
#33517 = CARTESIAN_POINT ( 'NONE',  ( -0.6971942568897648851, 0.07405724077823318263, 1.692913385773008539 ) ) ;
#33518 = CARTESIAN_POINT ( 'NONE',  ( -0.8759842519685039353, 0.1787899950787401882, 0.8587598424659212970 ) ) ;
#33519 = CARTESIAN_POINT ( 'NONE',  ( -1.002407869896990045, -0.1264236179284866091, 0.5733267715997795166 ) ) ;
#33520 = EDGE_CURVE ( 'NONE', #28038, #6061, #26988, .T. ) ;
#33521 = CARTESIAN_POINT ( 'NONE',  ( -1.033464566929133799, 0.000000000000000000, 0.6791338582677166613 ) ) ;
#33522 = CARTESIAN_POINT ( 'NONE',  ( -0.8759842519685039353, -0.1787899950787401882, 1.985728346402929168 ) ) ;
#33523 = DIRECTION ( 'NONE',  ( -1.000000000000000000, 0.000000000000000000, 0.000000000000000000 ) ) ;
#33524 = CARTESIAN_POINT ( 'NONE',  ( 0.6971942568897637749, 2.189545951927499583E-17, 0.04183070860765386589 ) ) ;
#33525 = CARTESIAN_POINT ( 'NONE',  ( -0.3100393700787402174, 0.01114154383210021713, -0.7086614173228347191 ) ) ;
#33526 = CARTESIAN_POINT ( 'NONE',  ( -0.07405724077823318263, -0.4420531020875061445, 0.1787899950787401604 ) ) ;
#33527 = CARTESIAN_POINT ( 'NONE',  ( -0.1377300245925881794, -0.08955984809379961831, 0.1824063869217125988 ) ) ;
#33528 = DIRECTION ( 'NONE',  ( 0.000000000000000000, 0.000000000000000000, 1.000000000000000000 ) ) ;
#33529 = EDGE_CURVE ( 'NONE', #26918, #41311, #34083, .T. ) ;
#33530 = CARTESIAN_POINT ( 'NONE',  ( 0.2559055118110208360, -0.01436877235161249967, -0.02740704184215201136 ) ) ;
#33531 = AXIS2_PLACEMENT_3D ( 'NONE', #37367, #11999, #37138 ) ;
#33532 = CARTESIAN_POINT ( 'NONE',  ( -0.6971942568897626646, 0.07405724077823318263, 0.3937007873478115538 ) ) ;
#33533 = CARTESIAN_POINT ( 'NONE',  ( -0.07405724077823318263, -1.741265700512703019, 0.1787899950787401604 ) ) ;
#33534 = VERTEX_POINT ( 'NONE', #8408 ) ;
#33535 = CARTESIAN_POINT ( 'NONE',  ( 0.7185039370078739607, 1.928577636452523993E-17, 1.604330708661417360 ) ) ;
#33536 = VERTEX_POINT ( 'NONE', #37651 ) ;
#33537 = CARTESIAN_POINT ( 'NONE',  ( -0.6971942568897648851, 0.07405724077823318263, 1.304133858213953667 ) ) ;
#33538 = ORIENTED_EDGE ( 'NONE', *, *, #20979, .T. ) ;
#33539 = CARTESIAN_POINT ( 'NONE',  ( -1.094772975963752103E-17, -1.275098425143086578, -0.1787899950787401882 ) ) ;
#33540 = CARTESIAN_POINT ( 'NONE',  ( -0.1787899950787401604, -1.533464566875370805, 0.07405724077823318263 ) ) ;
#33541 = CARTESIAN_POINT ( 'NONE',  ( -0.2066929133858267931, -0.9875035750853327077, -1.463737590216208861 ) ) ;
#33542 = SHAPE_REPRESENTATION_RELATIONSHIP ( 'NONE' , 'NONE' ,  #20643, #47308 ) ;
#33543 = CYLINDRICAL_SURFACE ( 'NONE', #10245, 0.1574803149606299191 ) ;
#33544 = CARTESIAN_POINT ( 'NONE',  ( -1.033464566929133799, 0.000000000000000000, 1.023622047136567126 ) ) ;
#33545 = CARTESIAN_POINT ( 'NONE',  ( 0.9500414927467378812, -0.1787899950787401604, 0.6102362204186774219 ) ) ;
#33546 = CARTESIAN_POINT ( 'NONE',  ( 0.7646288533564489232, 0.1113553986120547346, 0.5659448817822370081 ) ) ;
#33547 = CARTESIAN_POINT ( 'NONE',  ( -0.1574803149606297803, -0.2613188976377954220, 0.06523048226347956391 ) ) ;
#33548 = CARTESIAN_POINT ( 'NONE',  ( 0.8759842519685039353, -0.1574803149606299191, 1.998031495955464587 ) ) ;
#33549 = ORIENTED_EDGE ( 'NONE', *, *, #92, .F. ) ;
#33550 = DIRECTION ( 'NONE',  ( 0.000000000000000000, 0.000000000000000000, 1.000000000000000000 ) ) ;
#33551 = CARTESIAN_POINT ( 'NONE',  ( -0.9500414927467377701, 0.1787899950787401604, 1.018700787347811110 ) ) ;
#33552 = CARTESIAN_POINT ( 'NONE',  ( 0.7185039370078746268, -0.06523048226347956391, 1.016240157480315487 ) ) ;
#33553 = CARTESIAN_POINT ( 'NONE',  ( 0.2066929133858268486, -0.2274162997038020051, -0.9219983537151217323 ) ) ;
#33554 = CARTESIAN_POINT ( 'NONE',  ( -0.1691510595345104007, -0.08955828895034714798, -0.02489612667484852188 ) ) ;
#33555 = VERTEX_POINT ( 'NONE', #1213 ) ;
#33556 = CARTESIAN_POINT ( 'NONE',  ( 0.1554374527100134684, -0.02743359356286620768, -0.1377952755905450799 ) ) ;
#33557 = CARTESIAN_POINT ( 'NONE',  ( -0.3100393700787402174, 0.01114154383210022407, 1.043307086614173151 ) ) ;
#33558 = ORIENTED_EDGE ( 'NONE', *, *, #20832, .T. ) ;
#33559 = CARTESIAN_POINT ( 'NONE',  ( 0.6971942568897626646, 0.07405724077823318263, 0.7086614172690703928 ) ) ;
#33560 = ORIENTED_EDGE ( 'NONE', *, *, #21586, .F. ) ;
#33561 = CARTESIAN_POINT ( 'NONE',  ( -0.1476377952755905387, -0.4950321721878530035, -0.8627979602685655891 ) ) ;
#33562 = CARTESIAN_POINT ( 'NONE',  ( 0.3161444924769511999, 0.9382165298418956301, -1.070508272602716637 ) ) ;
#33563 = CARTESIAN_POINT ( 'NONE',  ( -0.07405724077823318263, -1.582677165300567346, -0.1787899950787401604 ) ) ;
#33564 = CARTESIAN_POINT ( 'NONE',  ( -0.1787899950787401882, -0.7928149605761574126, 0.000000000000000000 ) ) ;
#33566 = CIRCLE ( 'NONE', #12900, 0.2559055118110236116 ) ;
#33565 = CARTESIAN_POINT ( 'NONE',  ( 0.1113553986120547346, -1.262795275590551158, -0.1113553986120547346 ) ) ;
#33567 = CARTESIAN_POINT ( 'NONE',  ( 0.7646288533564489232, 0.1113553986120547346, 1.117125984144440975 ) ) ;
#33568 = DIRECTION ( 'NONE',  ( 1.000000000000000000, -3.469446951953613794E-15, 0.000000000000000000 ) ) ;
#33569 = CARTESIAN_POINT ( 'NONE',  ( -0.8759842519685039353, -0.1787899950787401882, 0.4847440944344252323 ) ) ;
#33570 = EDGE_LOOP ( 'NONE', ( #38193, #18754, #24707, #17388 ) ) ;
#33571 = EDGE_LOOP ( 'NONE', ( #308, #8736, #25454, #40881, #40595, #5753, #28890, #37664 ) ) ;
#33572 = CARTESIAN_POINT ( 'NONE',  ( -1.054774247047244540, -0.07405724077823318263, 1.835629921206078485 ) ) ;
#33573 = EDGE_CURVE ( 'NONE', #1467, #14891, #31879, .T. ) ;
#33574 = CARTESIAN_POINT ( 'NONE',  ( 0.6971942568897637749, 2.189545951927499583E-17, 1.700295275536787498 ) ) ;
#33575 = CARTESIAN_POINT ( 'NONE',  ( 0.06523048226347956391, -1.329232283357040467, -0.1574803149606300301 ) ) ;
#33576 = CARTESIAN_POINT ( 'NONE',  ( -1.002407869896990045, 0.1264236179284866091, 0.8981299212060788184 ) ) ;
#33577 = LINE ( 'NONE', #37136, #2653 ) ;
#33578 = DIRECTION ( 'NONE',  ( 0.000000000000000000, 0.000000000000000000, 1.000000000000000000 ) ) ;
#33579 = CARTESIAN_POINT ( 'NONE',  ( -0.8759842519685039353, 0.1787899950787401882, 1.252460629867496067 ) ) ;
#33580 = CARTESIAN_POINT ( 'NONE',  ( -0.8019270111902717657, 0.1787899950787401604, 0.9399606298674970661 ) ) ;
#33581 = ADVANCED_FACE ( 'NONE', ( #27802 ), #12701, .T. ) ;
#33582 = CARTESIAN_POINT ( 'NONE',  ( -0.7495606340400177148, 0.1264236179284866091, 0.04183070860765386589 ) ) ;
#33583 = ADVANCED_FACE ( 'NONE', ( #27081 ), #11654, .T. ) ;
#33584 = CARTESIAN_POINT ( 'NONE',  ( 0.05940473271390560306, 0.07959431159476453022, 0.2511357324426306548 ) ) ;
#33585 = CARTESIAN_POINT ( 'NONE',  ( -0.6971942568897637749, 2.189545951927499583E-17, 1.542814960576157413 ) ) ;
#33586 = CARTESIAN_POINT ( 'NONE',  ( -0.9873396505805591694, -0.1113553986120547346, 1.924212598317669221 ) ) ;
#33587 = EDGE_LOOP ( 'NONE', ( #2751, #28892, #36800, #39141, #14870, #36344, #3230, #27930, #26154 ) ) ;
#33588 = CARTESIAN_POINT ( 'NONE',  ( -0.7185039370078746268, -0.06523048226347956391, 1.646161417322835385 ) ) ;
#33589 = CARTESIAN_POINT ( 'NONE',  ( 0.5717220857807087109, -3.032960542342102697E-32, 0.09842519685039370636 ) ) ;
#33590 = CARTESIAN_POINT ( 'NONE',  ( 0.9500414927467377701, -0.1787899950787401604, 1.555118110182457158 ) ) ;
#33591 = CARTESIAN_POINT ( 'NONE',  ( -0.1854798818493685053, -0.09842519685039370636, 0.1431202509172336546 ) ) ;
#33592 = CARTESIAN_POINT ( 'NONE',  ( 1.033464566929133799, 0.000000000000000000, 1.023622047136567126 ) ) ;
#33593 = CARTESIAN_POINT ( 'NONE',  ( -0.2559055118110236116, 0.006260861050427609514, -0.3149606299212598381 ) ) ;
#33594 = EDGE_LOOP ( 'NONE', ( #45915, #26450, #40683, #36673 ) ) ;
#33595 = EDGE_CURVE ( 'NONE', #20346, #47229, #9794, .T. ) ;
#33596 = AXIS2_PLACEMENT_3D ( 'NONE', #32493, #24342, #38940 ) ;
#33597 = ORIENTED_EDGE ( 'NONE', *, *, #10016, .F. ) ;
#33598 = ORIENTED_EDGE ( 'NONE', *, *, #3361, .F. ) ;
#33599 = B_SPLINE_CURVE_WITH_KNOTS ( 'NONE', 3,
 ( #33741, #38479, #8530, #19555, #12631, #20024, #27256, #15986, #41808, #44695, #9007, #33968, #38242, #45173, #34664, #1095, #41562 ),
 .UNSPECIFIED., .F., .F.,
 ( 4, 2, 2, 2, 2, 1, 2, 2, 4 ),
 ( 0.000000000000000000, 0.1249999999999983902, 0.1874999999999975853, 0.2499999999999967804, 0.3749999999999956146, 0.4374999999999951150, 0.4687499999999949485, 0.4999999999999947820, 1.000000000000000000 ),
 .UNSPECIFIED. ) ;
#33600 = CARTESIAN_POINT ( 'NONE',  ( 0.07405724077823318263, -0.9232283464029299447, -0.1787899950787401604 ) ) ;
#33601 = VECTOR ( 'NONE', #23608, 39.37007874015748143 ) ;
#33602 = CARTESIAN_POINT ( 'NONE',  ( -1.094772975963752103E-17, -1.033956692859621995, -0.1787899950787401882 ) ) ;
#33603 = DIRECTION ( 'NONE',  ( 0.000000000000000000, 0.000000000000000000, 1.000000000000000000 ) ) ;
#33604 = CARTESIAN_POINT ( 'NONE',  ( 1.054774247047244096, 0.000000000000000000, 1.715059055064346527 ) ) ;
#33605 = CARTESIAN_POINT ( 'NONE',  ( 0.1270800023317771588, -0.3799650694255653494, 0.1270800023317771588 ) ) ;
#33606 = CARTESIAN_POINT ( 'NONE',  ( -0.1113553986120547346, 0.09547244094488190058, 0.1113553986120547346 ) ) ;
#33607 = CARTESIAN_POINT ( 'NONE',  ( -0.1787899950787401604, -0.04232283459190575720, 0.07405724077823318263 ) ) ;
#33609 = ( NAMED_UNIT ( * ) SI_UNIT ( $, .STERADIAN. ) SOLID_ANGLE_UNIT ( ) ) ;
#33608 = DIRECTION ( 'NONE',  ( -1.000000000000000000, 0.000000000000000000, 0.000000000000000000 ) ) ;
#33611 = DIRECTION ( 'NONE',  ( -1.000000000000000000, 0.000000000000000000, 0.000000000000000000 ) ) ;
#33610 = DIRECTION ( 'NONE',  ( 0.000000000000000000, 0.000000000000000000, -1.000000000000000000 ) ) ;
#33612 = CARTESIAN_POINT ( 'NONE',  ( 0.9873396505805591694, 0.1113553986120547346, 0.4478346456692913202 ) ) ;
#33613 = CARTESIAN_POINT ( 'NONE',  ( 0.8019270111902717657, 0.1787899950787401604, 1.811023621993480548 ) ) ;
#33614 = CARTESIAN_POINT ( 'NONE',  ( 0.7185039370078739607, 1.928577636452523993E-17, 1.870078740049952559 ) ) ;
#33616 = ORIENTED_EDGE ( 'NONE', *, *, #32106, .F. ) ;
#33615 = ADVANCED_FACE ( 'NONE', ( #5715 ), #26188, .F. ) ;
#33617 = DIRECTION ( 'NONE',  ( 0.4230299666438205319, 5.180622945937663512E-17, -0.9061156920180379881 ) ) ;
#33618 = CARTESIAN_POINT ( 'NONE',  ( 0.1787899950787401882, -0.2613188975840319284, -2.189545951927503898E-17 ) ) ;
#33619 = CARTESIAN_POINT ( 'NONE',  ( -0.7185039370078746268, 0.06523048226347956391, 0.1845472440944882775 ) ) ;
#33620 = CARTESIAN_POINT ( 'NONE',  ( -0.1787899950787401882, -1.260334645615527549, 0.000000000000000000 ) ) ;
#33621 = CARTESIAN_POINT ( 'NONE',  ( 0.6971942568897626646, -0.07405724077823297447, 0.1673228345919059168 ) ) ;
#33622 = CARTESIAN_POINT ( 'NONE',  ( 0.1634463062185840532, 0.08033005673471317609, -0.1391367933297039394 ) ) ;
#33623 = AXIS2_PLACEMENT_3D ( 'NONE', #37898, #23285, #44581 ) ;
#33624 = CARTESIAN_POINT ( 'NONE',  ( -0.6971942568897637749, 2.189545951927499583E-17, 1.734744094434425232 ) ) ;
#33625 = ORIENTED_EDGE ( 'NONE', *, *, #27196, .T. ) ;
#33626 = CARTESIAN_POINT ( 'NONE',  ( -0.6971942568897648851, -0.07405724077823297447, 1.269685039316314601 ) ) ;
#33627 = LINE ( 'NONE', #26192, #21481 ) ;
#33628 = EDGE_CURVE ( 'NONE', #8992, #30331, #14685, .T. ) ;
#33629 = CARTESIAN_POINT ( 'NONE',  ( 1.054774247047244540, 0.07405724077823318263, 1.328740157426552049 ) ) ;
#33630 = CARTESIAN_POINT ( 'NONE',  ( 0.9500414927467378812, 0.1787899950787401604, 1.919291338528913871 ) ) ;
#33631 = CARTESIAN_POINT ( 'NONE',  ( -1.054774247047244096, 0.000000000000000000, 1.006397637741511808 ) ) ;
#33632 = CARTESIAN_POINT ( 'NONE',  ( 0.001029233576901327765, -0.09840078316628074473, -0.1790406922995744221 ) ) ;
#33633 = FACE_OUTER_BOUND ( 'NONE', #43436, .T. ) ;
#33634 = CARTESIAN_POINT ( 'NONE',  ( 0.8759842519685039353, -0.1787899950787401882, 0.4896653542769449086 ) ) ;
#33635 = CARTESIAN_POINT ( 'NONE',  ( -0.8759842519685039353, 0.1787899950787401882, 0.3469488188438744070 ) ) ;
#33636 = CARTESIAN_POINT ( 'NONE',  ( -0.8019270111902717657, -0.1787899950787401604, 0.8366141731745828647 ) ) ;
#33637 = CARTESIAN_POINT ( 'NONE',  ( 0.7646288533564489232, -0.1113553986120547346, 1.717519684931842594 ) ) ;
#33638 = ORIENTED_EDGE ( 'NONE', *, *, #38107, .T. ) ;
#33639 = VECTOR ( 'NONE', #18528, 39.37007874015748854 ) ;
#33640 = CARTESIAN_POINT ( 'NONE',  ( -0.7185039370078714072, 0.06523048226347728795, 1.365649606299213614 ) ) ;
#33641 = EDGE_LOOP ( 'NONE', ( #43368, #6251, #20039, #46342 ) ) ;
#33642 = CARTESIAN_POINT ( 'NONE',  ( -0.7185039370078739607, 1.928577636452523993E-17, 0.1476377952755905387 ) ) ;
#33643 = VECTOR ( 'NONE', #18097, 39.37007874015748854 ) ;
#33644 = CARTESIAN_POINT ( 'NONE',  ( 0.9500414927467377701, -0.1787899950787401604, 1.200787401521039355 ) ) ;
#33645 = CARTESIAN_POINT ( 'NONE',  ( 0.7646288533564489232, 0.1113553986120547346, 1.943897637687747926 ) ) ;
#33646 = ORIENTED_EDGE ( 'NONE', *, *, #34767, .F. ) ;
#33647 = FACE_OUTER_BOUND ( 'NONE', #34068, .T. ) ;
#33648 = CARTESIAN_POINT ( 'NONE',  ( 0.2362204724409449064, -0.5708661417322835607, 0.9783464566929134243 ) ) ;
#33649 = CARTESIAN_POINT ( 'NONE',  ( 0.07405724077823318263, -1.445990109961521553, -0.1787899950787401604 ) ) ;
#33650 = VERTEX_POINT ( 'NONE', #5230 ) ;
#33651 = CARTESIAN_POINT ( 'NONE',  ( 0.1787899950787401882, -0.4532480314422991929, -2.189545951927503898E-17 ) ) ;
#33652 = VERTEX_POINT ( 'NONE', #19858 ) ;
#33653 = CARTESIAN_POINT ( 'NONE',  ( 0.7495606340400177148, -0.1264236179284866091, 1.267224409395055096 ) ) ;
#33654 = DIRECTION ( 'NONE',  ( 0.000000000000000000, 1.000000000000000000, 0.000000000000000000 ) ) ;
#33655 = DIRECTION ( 'NONE',  ( 0.000000000000000000, 1.000000000000000000, 0.000000000000000000 ) ) ;
#33656 = AXIS2_PLACEMENT_3D ( 'NONE', #37856, #33334, #34272 ) ;
#33657 = CARTESIAN_POINT ( 'NONE',  ( 0.000000000000000000, -0.1193342091828950846, -0.06889763779527559306 ) ) ;
#33658 = CARTESIAN_POINT ( 'NONE',  ( 0.6971942568897648851, 0.07405724077823318263, 1.496062992072220821 ) ) ;
#33659 = CARTESIAN_POINT ( 'NONE',  ( 0.6971942568897637749, 2.189545951927499583E-17, 0.1993110235682838682 ) ) ;
#33660 = CARTESIAN_POINT ( 'NONE',  ( 0.1787899950787401604, -1.754921259788755128, -0.07405724077823318263 ) ) ;
#33661 = CARTESIAN_POINT ( 'NONE',  ( 0.07405724077823318263, -1.705708661363559253, -0.1787899950787401604 ) ) ;
#33662 = DIRECTION ( 'NONE',  ( 1.000000000000000000, 0.000000000000000000, 0.000000000000000000 ) ) ;
#33663 = DIRECTION ( 'NONE',  ( 1.822029033848725028E-16, 0.000000000000000000, 1.000000000000000000 ) ) ;
#33664 = AXIS2_PLACEMENT_3D ( 'NONE', #2021, #45615, #5863 ) ;
#33665 = CARTESIAN_POINT ( 'NONE',  ( -0.8019270111902716547, 0.1787899950787401604, 0.6299212597887560161 ) ) ;
#33667 = CARTESIAN_POINT ( 'NONE',  ( 0.7185039370078739607, 1.928577636452523993E-17, 0.2952755904436539236 ) ) ;
#33666 = CARTESIAN_POINT ( 'NONE',  ( -0.1113553986120547346, -0.8100393700787401619, 0.1113553986120547346 ) ) ;
#33668 = CARTESIAN_POINT ( 'NONE',  ( 0.1270800023317771588, -1.364217037929501997, 0.1270800023317771588 ) ) ;
#33669 = CARTESIAN_POINT ( 'NONE',  ( -0.7185039370078739607, 1.928577636452523993E-17, 1.751968503829480106 ) ) ;
#33670 = CARTESIAN_POINT ( 'NONE',  ( -1.033464566929133799, 1.928577636452524610E-17, 2.869337061179095023E-17 ) ) ;
#33671 = CARTESIAN_POINT ( 'NONE',  ( 0.9500414927467378812, 0.1787899950787401604, 1.412401574749386990 ) ) ;
#33672 = VECTOR ( 'NONE', #28199, 39.37007874015748143 ) ;
#33673 = CARTESIAN_POINT ( 'NONE',  ( 1.002407869896990045, 0.1264236179284866091, 1.759350393647023614 ) ) ;
#33675 = EDGE_CURVE ( 'NONE', #37113, #6940, #2113, .T. ) ;
#33674 = CARTESIAN_POINT ( 'NONE',  ( 0.7646288533564489232, 0.1113553986120547346, 0.1427165354330708902 ) ) ;
#33676 = CARTESIAN_POINT ( 'NONE',  ( 1.033464566929133799, 0.000000000000000000, 0.9055118109160944506 ) ) ;
#33677 = DIRECTION ( 'NONE',  ( -1.000000000000000000, 0.000000000000000000, 0.000000000000000000 ) ) ;
#33679 = CARTESIAN_POINT ( 'NONE',  ( -0.1787899950787401882, 0.1520669291876218521, 0.000000000000000000 ) ) ;
#33678 = CARTESIAN_POINT ( 'NONE',  ( 0.06523048226347956391, -0.8321850392625521620, 0.1574803149606297803 ) ) ;
#33680 = CARTESIAN_POINT ( 'NONE',  ( 0.8759842519685039353, 0.1787899950787401882, 0.3469488188438744070 ) ) ;
#33681 = ADVANCED_FACE ( 'NONE', ( #9561 ), #7796, .T. ) ;
#33682 = CARTESIAN_POINT ( 'NONE',  ( 0.7331056760640133341, -0.08919270234511263162, 0.03937007864081804726 ) ) ;
#33683 = LINE ( 'NONE', #7770, #44519 ) ;
#33684 = DIRECTION ( 'NONE',  ( 0.000000000000000000, -1.000000000000000000, 0.000000000000000000 ) ) ;
#33685 = CARTESIAN_POINT ( 'NONE',  ( -1.033464566929133799, 0.000000000000000000, 0.7578740157480314821 ) ) ;
#33686 = CARTESIAN_POINT ( 'NONE',  ( -0.6971942568897648851, -0.07405724077823297447, 1.343503936954111744 ) ) ;
#33687 = CARTESIAN_POINT ( 'NONE',  ( 0.8759842519685039353, 0.1574803149606299191, 0.6003937006798740761 ) ) ;
#33688 = ORIENTED_EDGE ( 'NONE', *, *, #34767, .T. ) ;
#33689 = FILL_AREA_STYLE ('',( #36785 ) ) ;
#33690 = EDGE_CURVE ( 'NONE', #27577, #7744, #42224, .T. ) ;
#33691 = DIRECTION ( 'NONE',  ( -0.000000000000000000, 0.6156614753256598460, 0.7880107536067207930 ) ) ;
#33692 = ORIENTED_EDGE ( 'NONE', *, *, #41363, .F. ) ;
#33693 = CARTESIAN_POINT ( 'NONE',  ( 0.07444174185955065859, -0.06746506942556518283, 0.1797182628040039087 ) ) ;
#33694 = CARTESIAN_POINT ( 'NONE',  ( 1.033464566929134687, 0.06523048226347956391, 0.8292322833570401341 ) ) ;
#33696 = CARTESIAN_POINT ( 'NONE',  ( 0.1787899950787401604, -1.282480314906867314, -0.07405724077823318263 ) ) ;
#33695 = CARTESIAN_POINT ( 'NONE',  ( 0.06523048226347956391, -1.053641732175938595, -0.1574803149606300301 ) ) ;
#33697 = CARTESIAN_POINT ( 'NONE',  ( -0.9412147342319918675, -0.1574803149606224251, 0.04183070866141774813 ) ) ;
#33698 = CARTESIAN_POINT ( 'NONE',  ( -0.7185039370078746268, 0.06523048226347956391, 1.208169291338584417 ) ) ;
#33699 = EDGE_CURVE ( 'NONE', #43030, #38536, #33030, .T. ) ;
#33700 = CARTESIAN_POINT ( 'NONE',  ( 0.9873396505805591694, 0.1113553986120547346, 0.5659448818897637734 ) ) ;
#33702 = DIRECTION ( 'NONE',  ( 1.000000000000000000, -3.368395098984090098E-15, 0.000000000000000000 ) ) ;
#33701 = CARTESIAN_POINT ( 'NONE',  ( -0.7646288533564489232, 0.1113553986120547346, 0.9301181102362204856 ) ) ;
#33703 = CARTESIAN_POINT ( 'NONE',  ( 1.033464566929133799, 1.928577636452524610E-17, 4.498031496062992574 ) ) ;
#33704 = CARTESIAN_POINT ( 'NONE',  ( -0.1264236179284866091, -0.1628937007336379861, -0.1264236179284866091 ) ) ;
#33705 = ORIENTED_EDGE ( 'NONE', *, *, #36841, .F. ) ;
#33706 = VECTOR ( 'NONE', #32333, 39.37007874015748143 ) ;
#33707 = CARTESIAN_POINT ( 'NONE',  ( 0.7185039370078739607, 1.928577636452523993E-17, 1.003937007766488199 ) ) ;
#33708 = ORIENTED_EDGE ( 'NONE', *, *, #32933, .F. ) ;
#33709 = ORIENTED_EDGE ( 'NONE', *, *, #41235, .T. ) ;
#33710 = CARTESIAN_POINT ( 'NONE',  ( -0.7495606340400177148, 0.1264236179284866091, 1.532972440891118060 ) ) ;
#33711 = CARTESIAN_POINT ( 'NONE',  ( -0.1113553986120547346, -0.01279527548302413463, 0.1113553986120547346 ) ) ;
#33712 = CARTESIAN_POINT ( 'NONE',  ( -0.9500414927467378812, 0.1787899950787401604, 1.294291338528912982 ) ) ;
#33713 = ORIENTED_EDGE ( 'NONE', *, *, #13482, .T. ) ;
#33714 = AXIS2_PLACEMENT_3D ( 'NONE', #22765, #28046, #16998 ) ;
#33715 = ( BOUNDED_CURVE ( )  B_SPLINE_CURVE ( 2, ( #5474, #34735, #31378, #12458, #27559, #16280, #16739, #38779, #35198 ),
 .UNSPECIFIED., .F., .F. ) 
 B_SPLINE_CURVE_WITH_KNOTS ( ( 3, 2, 2, 2, 3 ),
 ( 0.08000000000000000167, 0.08250000000000000389, 0.08500000000000000611, 0.08749999999999999445, 0.08999999999999999667 ),
 .UNSPECIFIED. ) 
 CURVE ( )  GEOMETRIC_REPRESENTATION_ITEM ( )  RATIONAL_B_SPLINE_CURVE ( ( 1.000000000000000000, 0.9238795325112869605, 1.000000000000000000, 0.9238795325112869605, 1.000000000000000000, 0.9238795325112869605, 1.000000000000000000, 0.9238795325112869605, 1.000000000000000000 ) ) 
 REPRESENTATION_ITEM ( '' )  ) ;
#33716 = CARTESIAN_POINT ( 'NONE',  ( -1.054774247047244096, 0.000000000000000000, 0.3420275590013546751 ) ) ;
#33717 = DIRECTION ( 'NONE',  ( 0.000000000000000000, 0.000000000000000000, 1.000000000000000000 ) ) ;
#33718 = CARTESIAN_POINT ( 'NONE',  ( 0.8759842519685039353, 0.000000000000000000, 2.007874015640504162 ) ) ;
#33719 = CARTESIAN_POINT ( 'NONE',  ( -0.07405724077823318263, -0.9932342044497125544, 0.1787899950787401604 ) ) ;
#33720 = ORIENTED_EDGE ( 'NONE', *, *, #6320, .F. ) ;
#33721 = CARTESIAN_POINT ( 'NONE',  ( -0.1787899950787401604, 0.08070866147108628208, 0.07405724077823318263 ) ) ;
#33722 = ORIENTED_EDGE ( 'NONE', *, *, #4640, .T. ) ;
#33723 = ORIENTED_EDGE ( 'NONE', *, *, #2802, .F. ) ;
#33724 = CARTESIAN_POINT ( 'NONE',  ( -0.8759842519685039353, 0.000000000000000000, 0.000000000000000000 ) ) ;
#33725 = DIRECTION ( 'NONE',  ( 0.000000000000000000, 0.000000000000000000, 1.000000000000000000 ) ) ;
#33726 = CARTESIAN_POINT ( 'NONE',  ( 0.7185039370078739607, 0.000000000000000000, 4.498031496062992574 ) ) ;
#33727 = CARTESIAN_POINT ( 'NONE',  ( 0.1787899950787401604, -0.5393700786863945273, 0.07405724077823318263 ) ) ;
#33728 = ( BOUNDED_CURVE ( )  B_SPLINE_CURVE ( 2, ( #7501, #36294, #3447, #14707, #1246, #26448, #45329, #38154, #41013 ),
 .UNSPECIFIED., .F., .T. ) 
 B_SPLINE_CURVE_WITH_KNOTS ( ( 3, 2, 2, 2, 3 ),
 ( 0.08999999999999999667, 0.09249999999999999889, 0.09500000000000000111, 0.09750000000000000333, 0.1000000000000000056 ),
 .UNSPECIFIED. ) 
 CURVE ( )  GEOMETRIC_REPRESENTATION_ITEM ( )  RATIONAL_B_SPLINE_CURVE ( ( 1.000000000000000000, 0.9238795325112869605, 1.000000000000000000, 0.9238795325112869605, 1.000000000000000000, 0.9238795325112869605, 1.000000000000000000, 0.9238795325112869605, 1.000000000000000000 ) ) 
 REPRESENTATION_ITEM ( '' )  ) ;
#33729 = CARTESIAN_POINT ( 'NONE',  ( -1.054774247047244096, 0.000000000000000000, 0.1845472440407248116 ) ) ;
#33730 = CARTESIAN_POINT ( 'NONE',  ( -1.033464566929134687, -0.06523048226347956391, 0.9522637795275590289 ) ) ;
#33731 = CARTESIAN_POINT ( 'NONE',  ( -0.02900000000000056352, 1.086379535891621506, -0.03715491745705966353 ) ) ;
#33732 = DIRECTION ( 'NONE',  ( 0.000000000000000000, 0.000000000000000000, 1.000000000000000000 ) ) ;
#33733 = CARTESIAN_POINT ( 'NONE',  ( -0.07444174185955065859, -1.032031998559423736, -0.1797182628040039087 ) ) ;
#33734 = DIRECTION ( 'NONE',  ( -1.000000000000000000, 0.000000000000000000, 0.000000000000000000 ) ) ;
#33735 = CARTESIAN_POINT ( 'NONE',  ( -0.8759842519685039353, -0.1574803149606299191, 1.486220472333417142 ) ) ;
#33736 = CARTESIAN_POINT ( 'NONE',  ( 0.9500414927467378812, 0.1787899950787401604, 0.9399606298674970661 ) ) ;
#33737 = VECTOR ( 'NONE', #10755, 39.37007874015748143 ) ;
#33738 = DIRECTION ( 'NONE',  ( 0.000000000000000000, 1.000000000000000000, 0.000000000000000000 ) ) ;
#33739 = CARTESIAN_POINT ( 'NONE',  ( 0.8107537697050253289, 0.1574803149606300301, 1.439468503937006538 ) ) ;
#33741 = CARTESIAN_POINT ( 'NONE',  ( -0.1279527559055118058, -0.2216206741968047289, -0.3149606299212598381 ) ) ;
#33740 = CARTESIAN_POINT ( 'NONE',  ( 0.7133215388179315886, 0.02839841869291725301, 1.982739101751397781 ) ) ;
#33742 = AXIS2_PLACEMENT_3D ( 'NONE', #34229, #37805, #35165 ) ;
#33743 = DIRECTION ( 'NONE',  ( 0.000000000000000000, 0.000000000000000000, 1.000000000000000000 ) ) ;
#33744 = CARTESIAN_POINT ( 'NONE',  ( -9.642888182262618425E-18, -0.6968503935932598425, -0.1574803149606299191 ) ) ;
#33745 = ADVANCED_FACE ( 'NONE', ( #10264 ), #32795, .T. ) ;
#33747 = CARTESIAN_POINT ( 'NONE',  ( 0.1558458267876559056, 0.1470250908559905534, 0.02093562383109653577 ) ) ;
#33746 = CARTESIAN_POINT ( 'NONE',  ( 0.8759842519685039353, 0.1787899950787401882, 0.8193897637257637756 ) ) ;
#33748 = CARTESIAN_POINT ( 'NONE',  ( 0.7495606340400177148, 0.1264236179284866091, 1.852854330654897685 ) ) ;
#33749 = CARTESIAN_POINT ( 'NONE',  ( 3.284318927891251994E-17, -0.6993110235682834519, 0.1787899950787401882 ) ) ;
#33750 = ORIENTED_EDGE ( 'NONE', *, *, #33529, .F. ) ;
#33751 = EDGE_CURVE ( 'NONE', #10497, #34560, #47151, .T. ) ;
#33752 = CARTESIAN_POINT ( 'NONE',  ( -0.8107537697050253289, 0.1574803149606300301, 0.09104330697908720460 ) ) ;
#33753 = CARTESIAN_POINT ( 'NONE',  ( 0.6971942568897637749, 2.189545951927499583E-17, 1.104822834591905556 ) ) ;
#33754 = EDGE_CURVE ( 'NONE', #43921, #8495, #24871, .T. ) ;
#33755 = DIRECTION ( 'NONE',  ( 0.000000000000000000, 0.000000000000000000, -1.000000000000000000 ) ) ;
#33756 = CARTESIAN_POINT ( 'NONE',  ( 0.1574803149606300301, -1.663877952755905332, 0.06523048226347956391 ) ) ;
#33757 = DIRECTION ( 'NONE',  ( -0.000000000000000000, 1.000000000000000000, -0.000000000000000000 ) ) ;
#33758 = CARTESIAN_POINT ( 'NONE',  ( -1.002407869896990045, 0.1264236179284866091, 0.4995078739619842612 ) ) ;
#33759 = ORIENTED_EDGE ( 'NONE', *, *, #18368, .T. ) ;
#33760 = CARTESIAN_POINT ( 'NONE',  ( 0.1555687797274980522, -0.09281549603114075397, -0.1148293963254592570 ) ) ;
#33761 = CARTESIAN_POINT ( 'NONE',  ( -0.6971942568897637749, 2.189545951927499583E-17, 0.2780511810485988278 ) ) ;
#33762 = VERTEX_POINT ( 'NONE', #14092 ) ;
#33763 = CARTESIAN_POINT ( 'NONE',  ( -0.8759842519685039353, 0.1574803149606299191, 0.6102362204724409711 ) ) ;
#33764 = CARTESIAN_POINT ( 'NONE',  ( 0.1264236179284866091, -1.594980314906866203, -0.1264236179284866091 ) ) ;
#33765 = CARTESIAN_POINT ( 'NONE',  ( -0.7495606340400177148, 0.1264236179284866091, 1.808562992072220377 ) ) ;
#33766 = CARTESIAN_POINT ( 'NONE',  ( -1.054774247047244540, 0.07405724077823318263, 0.9301181101824563813 ) ) ;
#33767 = CARTESIAN_POINT ( 'NONE',  ( -0.6971942568897626646, 0.07405724077823318263, 0.5561023621509617598 ) ) ;
#33768 = CARTESIAN_POINT ( 'NONE',  ( 0.5113546317124669782, 4.466152701071653354E-17, 0.000000000000000000 ) ) ;
#33769 = CARTESIAN_POINT ( 'NONE',  ( 1.033464566929134687, 0.06523048226347956391, 0.3961614172153076763 ) ) ;
#33770 = CARTESIAN_POINT ( 'NONE',  ( 0.05635946233522097504, 0.07780450164205243713, -0.2528939201155193106 ) ) ;
#33771 = CARTESIAN_POINT ( 'NONE',  ( -0.8759842519685039353, 0.1574803149606299191, 1.673228346456693050 ) ) ;
#33772 = CARTESIAN_POINT ( 'NONE',  ( -0.1787899950787401604, -0.5700058579930178393, -0.07405724077823318263 ) ) ;
#33773 = CARTESIAN_POINT ( 'NONE',  ( 0.007747115091317480218, -0.08955984173353109812, 0.2203066983908811283 ) ) ;
#33774 = DIRECTION ( 'NONE',  ( 0.000000000000000000, 0.000000000000000000, 1.000000000000000000 ) ) ;
#33775 = CARTESIAN_POINT ( 'NONE',  ( 0.9412147342319837628, 0.1574803149606300301, 1.788877952755905554 ) ) ;
#33776 = CIRCLE ( 'NONE', #26117, 0.04921259842519686012 ) ;
#33778 = CARTESIAN_POINT ( 'NONE',  ( 0.2559046595376678335, -0.05435615997519514797, -0.03956173954060922260 ) ) ;
#33777 = CONICAL_SURFACE ( 'NONE', #29990, 0.1574803149606299191, 0.9599310885968713736 ) ;
#33779 = CARTESIAN_POINT ( 'NONE',  ( -1.054774247047244540, 0.07405724077823318263, 0.2608267715997796832 ) ) ;
#33780 = CARTESIAN_POINT ( 'NONE',  ( 3.624546087963248077E-17, -0.09842519685039370636, 0.2854330708661417804 ) ) ;
#33781 = ORIENTED_EDGE ( 'NONE', *, *, #3376, .T. ) ;
#33782 = DIRECTION ( 'NONE',  ( 1.000000000000000000, 0.000000000000000000, 0.000000000000000000 ) ) ;
#33783 = CIRCLE ( 'NONE', #28534, 0.1377952755905511861 ) ;
#33784 = EDGE_LOOP ( 'NONE', ( #27818, #22253, #19889, #38602 ) ) ;
#33785 = EDGE_CURVE ( 'NONE', #25810, #38992, #3725, .T. ) ;
#33786 = CARTESIAN_POINT ( 'NONE',  ( 0.1602931993194442739, 0.07955613945526338049, 0.1377952755905511861 ) ) ;
#33787 = LINE ( 'NONE', #18422, #260 ) ;
#33788 = CARTESIAN_POINT ( 'NONE',  ( -0.8107537697050253289, -0.1574803149606297803, 1.050688976270426567 ) ) ;
#33789 = CARTESIAN_POINT ( 'NONE',  ( 0.8759842519685039353, -0.1787899950787401882, 0.4896653542769449086 ) ) ;
#33791 = CARTESIAN_POINT ( 'NONE',  ( 0.3108999017613323090, 0.9251089822459547252, -1.060267534067256046 ) ) ;
#33790 = CARTESIAN_POINT ( 'NONE',  ( 0.06523048226347956391, -0.2514763779527561249, 0.1574803149606297803 ) ) ;
#33792 = CARTESIAN_POINT ( 'NONE',  ( 0.000000000000000000, 0.000000000000000000, 1.181102362204724310 ) ) ;
#33793 = ORIENTED_EDGE ( 'NONE', *, *, #1789, .T. ) ;
#33794 = CARTESIAN_POINT ( 'NONE',  ( -0.1305514342443539477, -0.09246813122503681759, -0.1221825334204538205 ) ) ;
#33795 = CARTESIAN_POINT ( 'NONE',  ( -1.002407869896990045, 0.1264236179284866091, 0.8981299212060788184 ) ) ;
#33796 = CARTESIAN_POINT ( 'NONE',  ( 0.8759842519685039353, -0.1574803149606299191, 0.9448818897637796255 ) ) ;
#33797 = CARTESIAN_POINT ( 'NONE',  ( 0.000000000000000000, -0.3937007874015748254, 0.000000000000000000 ) ) ;
#33798 = EDGE_CURVE ( 'NONE', #43609, #12706, #46661, .T. ) ;
#33799 = DIRECTION ( 'NONE',  ( 3.469446951953614583E-15, 1.000000000000000000, -0.000000000000000000 ) ) ;
#33800 = CARTESIAN_POINT ( 'NONE',  ( -0.1539388023598581845, -0.08956124721700792213, 0.06042638813536082426 ) ) ;
#33801 = EDGE_LOOP ( 'NONE', ( #23673, #19963, #27297, #33597 ) ) ;
#33802 = PLANE ( 'NONE',  #46713 ) ;
#33803 = VECTOR ( 'NONE', #34006, 39.37007874015748143 ) ;
#33804 = ORIENTED_EDGE ( 'NONE', *, *, #40395, .F. ) ;
#33805 = CARTESIAN_POINT ( 'NONE',  ( 0.7495606340400177148, -0.1264236179284866091, 0.7160433070328504623 ) ) ;
#33806 = ADVANCED_FACE ( 'NONE', ( #25105 ), #10754, .T. ) ;
#33807 = ORIENTED_EDGE ( 'NONE', *, *, #19766, .F. ) ;
#33808 = CARTESIAN_POINT ( 'NONE',  ( 1.033464566929134687, -0.06523048226347956391, 0.8341535433070870198 ) ) ;
#33809 = CARTESIAN_POINT ( 'NONE',  ( 0.1264236179284866091, -1.590059055064346305, -0.1264236179284866091 ) ) ;
#33810 = CARTESIAN_POINT ( 'NONE',  ( -0.07405724077823318263, -0.8248031495525351975, 0.1787899950787401604 ) ) ;
#33811 = AXIS2_PLACEMENT_3D ( 'NONE', #8585, #34026, #19373 ) ;
#33812 = CARTESIAN_POINT ( 'NONE',  ( 0.1574803149606300301, -1.230807086614172929, 0.06523048226347956391 ) ) ;
#33813 = CARTESIAN_POINT ( 'NONE',  ( 0.9873396505805591694, 0.1113553986120547346, 1.067913385719243990 ) ) ;
#33814 = CARTESIAN_POINT ( 'NONE',  ( -1.033464566929133799, 0.000000000000000000, 1.663385826771653697 ) ) ;
#33815 = VERTEX_POINT ( 'NONE', #24636 ) ;
#33816 = VERTEX_POINT ( 'NONE', #32072 ) ;
#33817 = CARTESIAN_POINT ( 'NONE',  ( -0.8759842519685039353, 0.1787899950787401882, 1.808562992072220377 ) ) ;
#33818 = CARTESIAN_POINT ( 'NONE',  ( 0.7495606340400177148, 0.1264236179284866091, 1.656003936954110412 ) ) ;
#33819 = CARTESIAN_POINT ( 'NONE',  ( -0.7185039370078739607, 0.000000000000000000, -2.869337061179095023E-17 ) ) ;
#33820 = CARTESIAN_POINT ( 'NONE',  ( 1.002407869896990045, 0.1264236179284866091, 0.2682086613635594752 ) ) ;
#33821 = CARTESIAN_POINT ( 'NONE',  ( -1.002407869896990045, -0.1264236179284866091, 1.434547244040724534 ) ) ;
#33822 = CARTESIAN_POINT ( 'NONE',  ( -1.054774247047244540, -0.07405724077823318263, 1.318897637741511364 ) ) ;
#33823 = CYLINDRICAL_SURFACE ( 'NONE', #43614, 0.1864803149606299171 ) ;
#33824 = CARTESIAN_POINT ( 'NONE',  ( -0.8019270111902717657, 0.1787899950787401604, 1.535433070812378675 ) ) ;
#33825 = CARTESIAN_POINT ( 'NONE',  ( -0.7646288533564489232, -0.1113553986120547346, 1.993110236112944911 ) ) ;
#33826 = CARTESIAN_POINT ( 'NONE',  ( 0.000000000000000000, 1.205361022782826802E-17, -0.09842519685039370636 ) ) ;
#33827 = CARTESIAN_POINT ( 'NONE',  ( -0.9412147342319837628, 0.1574803149606300301, 1.592027559055119390 ) ) ;
#33828 = CARTESIAN_POINT ( 'NONE',  ( 1.033464566929134687, -0.06523048226347956391, 0.9817913384751512096 ) ) ;
#33829 = CARTESIAN_POINT ( 'NONE',  ( -0.1713132547969852260, -0.09842519685039370636, 0.1581802318308832833 ) ) ;
#33830 = CARTESIAN_POINT ( 'NONE',  ( 0.7185039370078739607, 1.928577636452523993E-17, 1.003937007766488199 ) ) ;
#33831 = CARTESIAN_POINT ( 'NONE',  ( -0.7185039370078746268, 0.06523048226347956391, 1.798720472440944240 ) ) ;
#33832 = ORIENTED_EDGE ( 'NONE', *, *, #18300, .T. ) ;
#33833 = DIMENSIONAL_EXPONENTS ( 1.000000000000000000, 0.000000000000000000, 0.000000000000000000, 0.000000000000000000, 0.000000000000000000, 0.000000000000000000, 0.000000000000000000 ) ;
#33834 = EDGE_CURVE ( 'NONE', #370, #40880, #27717, .T. ) ;
#33835 = VECTOR ( 'NONE', #41202, 39.37007874015748143 ) ;
#33836 = EDGE_LOOP ( 'NONE', ( #28153, #30134, #39429, #38249 ) ) ;
#33837 = CARTESIAN_POINT ( 'NONE',  ( -1.054774247047244540, -0.07405724077823318263, 1.166338582623402731 ) ) ;
#33838 = ORIENTED_EDGE ( 'NONE', *, *, #47184, .F. ) ;
#33839 = AXIS2_PLACEMENT_3D ( 'NONE', #43631, #10841, #35984 ) ;
#33840 = CARTESIAN_POINT ( 'NONE',  ( 0.1787899950787401882, -0.9306102361667086820, -2.189545951927503898E-17 ) ) ;
#33841 = CARTESIAN_POINT ( 'NONE',  ( 3.284318927891251994E-17, -1.014271653489543290, 0.1787899950787401882 ) ) ;
#33842 = CARTESIAN_POINT ( 'NONE',  ( 0.1797182628040039087, -0.3775044395043055112, 0.07444174185955046430 ) ) ;
#33843 = CARTESIAN_POINT ( 'NONE',  ( -0.1113553986120547346, 0.08562992125984252023, -0.1113553986120547346 ) ) ;
#33844 = CARTESIAN_POINT ( 'NONE',  ( -0.1586641775163213364, 1.209494567139727250, -1.479906699140296045 ) ) ;
#33845 = EDGE_CURVE ( 'NONE', #11565, #1914, #36758, .T. ) ;
#33847 = EDGE_CURVE ( 'NONE', #39709, #43013, #24632, .T. ) ;
#33846 = CARTESIAN_POINT ( 'NONE',  ( 0.7495606340400177148, 0.1264236179284866091, 0.7455708660879684091 ) ) ;
#33848 = ADVANCED_FACE ( 'NONE', ( #40173 ), #7374, .T. ) ;
#33850 = ( NAMED_UNIT ( * ) PLANE_ANGLE_UNIT ( ) SI_UNIT ( $, .RADIAN. ) ) ;
#33849 = CARTESIAN_POINT ( 'NONE',  ( 0.009895589093209080853, 0.2897810112356523082, -0.09996720075266637973 ) ) ;
#33851 = CARTESIAN_POINT ( 'NONE',  ( 1.033464566929133799, 1.928577636452524610E-17, 4.498031496062992574 ) ) ;
#33852 = CARTESIAN_POINT ( 'NONE',  ( 1.033464566929133799, 0.000000000000000000, 1.269685039370078705 ) ) ;
#33853 = CARTESIAN_POINT ( 'NONE',  ( 0.9500414927467378812, -0.1787899950787401604, 1.791338582623401177 ) ) ;
#33854 = ( GEOMETRIC_REPRESENTATION_CONTEXT ( 3 ) GLOBAL_UNCERTAINTY_ASSIGNED_CONTEXT ( ( #26848 ) ) GLOBAL_UNIT_ASSIGNED_CONTEXT ( ( #44575, #33850, #33609 ) ) REPRESENTATION_CONTEXT ( 'NONE', 'WORKASPACE' ) ) ;
#33855 = EDGE_CURVE ( 'NONE', #29883, #40089, #33503, .T. ) ;
#33856 = CARTESIAN_POINT ( 'NONE',  ( 0.7185039370078746268, -0.06523048226347956391, 0.1107283464566929249 ) ) ;
#33857 = DIRECTION ( 'NONE',  ( 1.000000000000000000, 0.000000000000000000, -1.822029033848725275E-16 ) ) ;
#33858 = CARTESIAN_POINT ( 'NONE',  ( -0.1787899950787401604, -0.4409448818359998357, -0.07405724077823318263 ) ) ;
#33859 = FACE_OUTER_BOUND ( 'NONE', #10298, .T. ) ;
#33860 = CARTESIAN_POINT ( 'NONE',  ( -0.1787899950787401604, -1.297244094434425010, 0.07405724077823318263 ) ) ;
#33861 = CARTESIAN_POINT ( 'NONE',  ( 1.054774247047244540, -0.07405724077823318263, 0.3001968503399373711 ) ) ;
#33862 = FACE_OUTER_BOUND ( 'NONE', #29779, .T. ) ;
#33863 = VECTOR ( 'NONE', #33799, 39.37007874015748143 ) ;
#33864 = CARTESIAN_POINT ( 'NONE',  ( -0.7495606340400177148, 0.1264236179284866091, 1.769192913332062966 ) ) ;
#33865 = ORIENTED_EDGE ( 'NONE', *, *, #9953, .T. ) ;
#33866 = CARTESIAN_POINT ( 'NONE',  ( -1.054774247047244540, -0.07405724077823318263, 1.323818897584032817 ) ) ;
#33867 = CARTESIAN_POINT ( 'NONE',  ( -0.7185039370078746268, 0.06523048226347956391, 0.8932086614173216921 ) ) ;
#33868 = CARTESIAN_POINT ( 'NONE',  ( 0.6971942568897648851, -0.07405724077823297447, 1.309055118056472899 ) ) ;
#33869 = CARTESIAN_POINT ( 'NONE',  ( -1.054774247047244540, -0.07405724077823318263, 0.4970472440407249226 ) ) ;
#33870 = VECTOR ( 'NONE', #21351, 39.37007874015748143 ) ;
#33871 = CARTESIAN_POINT ( 'NONE',  ( 1.054774247047244096, 0.000000000000000000, 1.990649606245448844 ) ) ;
#33872 = CARTESIAN_POINT ( 'NONE',  ( -0.7495606340400177148, 0.1264236179284866091, 0.9817913385289134265 ) ) ;
#33873 = CARTESIAN_POINT ( 'NONE',  ( 0.1579024634500894864, 0.1385691271450621709, -0.04084555919648127226 ) ) ;
#33874 = CARTESIAN_POINT ( 'NONE',  ( 0.9412147342319837628, 0.1574803149606300301, 1.198326771653543732 ) ) ;
#33875 = CARTESIAN_POINT ( 'NONE',  ( 0.6971942568897648851, -0.07405724077823297447, 0.5216535432533228045 ) ) ;
#33876 = CARTESIAN_POINT ( 'NONE',  ( -1.002407869896990045, -0.1264236179284866091, 0.3321850393163153226 ) ) ;
#33877 = CARTESIAN_POINT ( 'NONE',  ( -1.054774247047244096, 0.000000000000000000, 0.8489173227808819444 ) ) ;
#33878 = ORIENTED_EDGE ( 'NONE', *, *, #37506, .F. ) ;
#33879 = VECTOR ( 'NONE', #45417, 39.37007874015748143 ) ;
#33880 = CARTESIAN_POINT ( 'NONE',  ( -0.7646288533564489232, 0.1113553986120547346, 0.1427165354330708902 ) ) ;
#33881 = CARTESIAN_POINT ( 'NONE',  ( 0.6971942568897648851, 0.07405724077823318263, 1.186023621993481658 ) ) ;
#33882 = CARTESIAN_POINT ( 'NONE',  ( -1.054774247047244096, 0.000000000000000000, 1.990649606245448844 ) ) ;
#33883 = EDGE_LOOP ( 'NONE', ( #12808, #46540, #30307, #10943, #27451 ) ) ;
#33884 = CARTESIAN_POINT ( 'NONE',  ( 0.2395294000716133853, 3.423225304703229610E-16, -0.7086614173228351632 ) ) ;
#33885 = CARTESIAN_POINT ( 'NONE',  ( -0.7495606340400177148, 0.1264236179284866091, 0.8686023621509606496 ) ) ;
#33886 = CARTESIAN_POINT ( 'NONE',  ( -0.7185039370078739607, 1.928577636452523993E-17, 0.3051181102362204856 ) ) ;
#33887 = CARTESIAN_POINT ( 'NONE',  ( -0.9500414927467378812, -0.1787899950787401604, 0.05413385821395302888 ) ) ;
#33888 = CARTESIAN_POINT ( 'NONE',  ( 3.284318927891251994E-17, -1.502584598150498163, 0.1787899950787401882 ) ) ;
#33889 = VERTEX_POINT ( 'NONE', #29466 ) ;
#33890 = CARTESIAN_POINT ( 'NONE',  ( -1.094772975963752103E-17, -0.3646653542769452971, -0.1787899950787401882 ) ) ;
#33891 = FACE_OUTER_BOUND ( 'NONE', #12451, .T. ) ;
#33892 = ORIENTED_EDGE ( 'NONE', *, *, #2487, .T. ) ;
#33893 = CARTESIAN_POINT ( 'NONE',  ( 1.002407869896990045, -0.1264236179284866091, 1.277066929080094448 ) ) ;
#33894 = VECTOR ( 'NONE', #22553, 39.37007874015748143 ) ;
#33895 = CARTESIAN_POINT ( 'NONE',  ( -0.9412147342319837628, 0.1574803149606300301, 0.8341535431995593664 ) ) ;
#33896 = CARTESIAN_POINT ( 'NONE',  ( 0.2471922904502826812, 0.03219022224904106305, 0.1427165354330708902 ) ) ;
#33897 = CONICAL_SURFACE ( 'NONE', #13995, 0.08090551181102362266, 0.9599310885968742602 ) ;
#33898 = CARTESIAN_POINT ( 'NONE',  ( -8.737111503174280059E-18, -0.1126122229443935058, -0.08054045948813907951 ) ) ;
#33899 = CARTESIAN_POINT ( 'NONE',  ( 1.054774247047244540, 0.07405724077823318263, 0.2214566928596220785 ) ) ;
#33900 = EDGE_CURVE ( 'NONE', #1846, #3606, #7593, .T. ) ;
#33901 = VECTOR ( 'NONE', #44882, 39.37007874015748143 ) ;
#33902 = CARTESIAN_POINT ( 'NONE',  ( 3.284318927891251994E-17, -1.806594488135212728, 0.1787899950787401882 ) ) ;
#33903 = PRODUCT_CONTEXT ( 'NONE', #320, 'mechanical' ) ;
#33904 = FACE_OUTER_BOUND ( 'NONE', #39712, .T. ) ;
#33905 = CARTESIAN_POINT ( 'NONE',  ( -0.6971942568897648851, -0.07405724077823297447, 0.6397637794737947026 ) ) ;
#33906 = ADVANCED_FACE ( 'NONE', ( #4444 ), #4938, .T. ) ;
#33908 = CARTESIAN_POINT ( 'NONE',  ( 0.1733357866104492107, -0.5708661417322835607, 1.025733466389925352 ) ) ;
#33907 = CARTESIAN_POINT ( 'NONE',  ( -9.642888182262618425E-18, -0.6673228346456693272, -0.1574803149606299191 ) ) ;
#33909 = CARTESIAN_POINT ( 'NONE',  ( 0.1797182628040039087, -1.474945384386196379, -0.07444174185955065859 ) ) ;
#33910 = CARTESIAN_POINT ( 'NONE',  ( 0.7185039370078739607, 1.928577636452523993E-17, 1.446850393700787274 ) ) ;
#33911 = CARTESIAN_POINT ( 'NONE',  ( -0.2066929133858267931, -0.5253304731389190074, -0.9015780170405504057 ) ) ;
#33912 = CARTESIAN_POINT ( 'NONE',  ( 0.7495606340400177148, 0.1264236179284866091, 1.887303149552535420 ) ) ;
#33913 = CARTESIAN_POINT ( 'NONE',  ( 0.7185039370078746268, 0.06523048226347977208, 0.1451771653543309226 ) ) ;
#33914 = DIRECTION ( 'NONE',  ( -1.000000000000000000, 0.000000000000000000, 0.000000000000000000 ) ) ;
#33916 = CARTESIAN_POINT ( 'NONE',  ( 0.4736248074375716821, -2.599213366583078641E-15, 2.030728043535499967E-15 ) ) ;
#33915 = CARTESIAN_POINT ( 'NONE',  ( -0.1574803149606300301, -0.8075787400499540025, -0.06523048226347956391 ) ) ;
#33917 = CARTESIAN_POINT ( 'NONE',  ( -0.8759842519685039353, 0.1574803149606299191, 1.230314960522393752 ) ) ;
#33918 = CARTESIAN_POINT ( 'NONE',  ( 0.8019270111902717657, -0.1787899950787401604, 0.3641732282926931630 ) ) ;
#33919 = CARTESIAN_POINT ( 'NONE',  ( -0.8759842519685039353, -0.1574803149606299191, 1.722440944774362270 ) ) ;
#33920 = PRODUCT_DEFINITION ( 'UNKNOWN', '', #46138, #39368 ) ;
#33921 = DIRECTION ( 'NONE',  ( 0.000000000000000000, 0.000000000000000000, -1.000000000000000000 ) ) ;
#33922 = CARTESIAN_POINT ( 'NONE',  ( 0.8107537697050253289, 0.1574803149606300301, 0.6422244093412926569 ) ) ;
#33923 = ORIENTED_EDGE ( 'NONE', *, *, #16294, .F. ) ;
#33924 = CARTESIAN_POINT ( 'NONE',  ( -0.8019270111902717657, -0.1787899950787401604, 1.077755905458048113 ) ) ;
#33925 = DIRECTION ( 'NONE',  ( 0.7986355100472766200, 1.652401737524974224E-15, -0.6018150231520698057 ) ) ;
#33926 = CARTESIAN_POINT ( 'NONE',  ( 0.1574803149606300301, -0.04970472440944883469, 0.06523048226347956391 ) ) ;
#33927 = EDGE_LOOP ( 'NONE', ( #28613, #17092 ) ) ;
#33928 = CARTESIAN_POINT ( 'NONE',  ( 0.1270800023317771588, -0.09453199855942362451, -0.1270800023317771588 ) ) ;
#33929 = CARTESIAN_POINT ( 'NONE',  ( 0.1787899950787401604, -1.248031496009228913, 0.07405724077823318263 ) ) ;
#33930 = CARTESIAN_POINT ( 'NONE',  ( -0.8759842519685039353, 0.1574803149606299191, 0.4822834644594015674 ) ) ;
#33931 = PLANE ( 'NONE',  #20898 ) ;
#33932 = CARTESIAN_POINT ( 'NONE',  ( 1.054774247047244540, -0.07405724077823318263, 1.594488188922613237 ) ) ;
#33933 = CARTESIAN_POINT ( 'NONE',  ( -1.033464566929134687, -0.06523048226347956391, 1.188484251968505268 ) ) ;
#33934 = CARTESIAN_POINT ( 'NONE',  ( -0.9873396505805591694, 0.1113553986120547346, 1.146653543199559033 ) ) ;
#33936 = DIRECTION ( 'NONE',  ( 0.000000000000000000, 0.000000000000000000, 1.000000000000000000 ) ) ;
#33935 = CARTESIAN_POINT ( 'NONE',  ( 0.2204724409448818867, 0.000000000000000000, 0.000000000000000000 ) ) ;
#33937 = VERTEX_POINT ( 'NONE', #30161 ) ;
#33938 = AXIS2_PLACEMENT_3D ( 'NONE', #47039, #43670, #36024 ) ;
#33939 = CARTESIAN_POINT ( 'NONE',  ( -7.939671275311751530E-17, -0.03219022224904082713, -0.2854330708661417804 ) ) ;
#33940 = VERTEX_POINT ( 'NONE', #397 ) ;
#33941 = CARTESIAN_POINT ( 'NONE',  ( -0.7495606340400177148, 0.1264236179284866091, 1.572342519631275692 ) ) ;
#33942 = CARTESIAN_POINT ( 'NONE',  ( 2.892866454678787531E-17, -0.1259842518609769757, 0.1574803149606299191 ) ) ;
#33943 = CARTESIAN_POINT ( 'NONE',  ( -1.002407869896990045, 0.1264236179284866091, 1.252460629867496067 ) ) ;
#33944 = VECTOR ( 'NONE', #41926, 39.37007874015748143 ) ;
#33945 = ORIENTED_EDGE ( 'NONE', *, *, #7736, .F. ) ;
#33946 = CLOSED_SHELL ( 'NONE', ( #31676, #28858, #8696, #42014, #11186, #5189, #21657, #11267, #9819, #33581, #12495, #35225, #40075, #44563, #3896, #43504, #18393, #4425, #17264, #8489, #37226, #46361, #20072, #30181, #26093, #31345, #7768, #12705, #31796, #1025, #6263, #3950, #43337, #28544, #24310, #27954, #19860, #29665, #37992, #46747 ) ) ;
#33947 = DIRECTION ( 'NONE',  ( -1.000000000000000000, 0.000000000000000000, 0.000000000000000000 ) ) ;
#33948 = CARTESIAN_POINT ( 'NONE',  ( -1.054774247047244096, 0.000000000000000000, 0.3813976377415121966 ) ) ;
#33949 = CARTESIAN_POINT ( 'NONE',  ( 0.000000000000000000, 0.5288907983920094757, -0.7507079620615707549 ) ) ;
#33950 = CARTESIAN_POINT ( 'NONE',  ( 1.033464566929134687, 0.06523048226347956391, 0.8686023620971983217 ) ) ;
#33951 = ORIENTED_EDGE ( 'NONE', *, *, #27705, .T. ) ;
#33952 = CARTESIAN_POINT ( 'NONE',  ( -0.1787899950787401604, 0.04133858273092887170, 0.07405724077823318263 ) ) ;
#33953 = ORIENTED_EDGE ( 'NONE', *, *, #14257, .T. ) ;
#33954 = EDGE_CURVE ( 'NONE', #7920, #25562, #44239, .T. ) ;
#33955 = CARTESIAN_POINT ( 'NONE',  ( 0.001099666138426426583, -0.02645731785581961759, 0.1377950862353125028 ) ) ;
#33956 = DIRECTION ( 'NONE',  ( 1.000000000000000000, 0.000000000000000000, 0.000000000000000000 ) ) ;
#33957 = EDGE_CURVE ( 'NONE', #14401, #19175, #44697, .T. ) ;
#33958 = PLANE ( 'NONE',  #14776 ) ;
#33959 = CARTESIAN_POINT ( 'NONE',  ( 0.1264236179284866091, -0.5418307086076535883, 0.1264236179284866091 ) ) ;
#33960 = CIRCLE ( 'NONE', #22461, 0.7874015748031495399 ) ;
#33961 = CARTESIAN_POINT ( 'NONE',  ( -1.002407869896990045, -0.1264236179284866091, 0.2189960629383626012 ) ) ;
#33962 = CARTESIAN_POINT ( 'NONE',  ( -1.033464566929134687, -0.06523048226347956391, 0.9128937007874008414 ) ) ;
#33963 = CARTESIAN_POINT ( 'NONE',  ( 3.301370929368692659E-17, -1.014807589110604313, 0.1797182628040039365 ) ) ;
#33964 = CARTESIAN_POINT ( 'NONE',  ( -0.8107537697050254399, 0.1574803149606300301, 1.941437007766490863 ) ) ;
#33965 = CARTESIAN_POINT ( 'NONE',  ( 0.6971942568897626646, 0.07405724077823318263, 0.8710629920722218200 ) ) ;
#33966 = CARTESIAN_POINT ( 'NONE',  ( 0.9412147342319837628, 0.1574803149606300301, 1.631397637795275468 ) ) ;
#33968 = CARTESIAN_POINT ( 'NONE',  ( -0.1872703683833633059, -0.1873733034530705444, -0.3097625555229961969 ) ) ;
#33967 = CARTESIAN_POINT ( 'NONE',  ( 0.7409552448146143888, -0.1027862860257732214, 1.985316688754235948 ) ) ;
#33969 = CARTESIAN_POINT ( 'NONE',  ( -0.02739131347899105909, -0.09752745740044843625, 0.1550798682808147422 ) ) ;
#33970 = CARTESIAN_POINT ( 'NONE',  ( -0.1113553986120547346, -0.6919291337507401662, -0.1113553986120547346 ) ) ;
#33971 = CARTESIAN_POINT ( 'NONE',  ( -0.07405724077823318263, 0.08562992131360593062, 0.1787899950787401604 ) ) ;
#33972 = FACE_OUTER_BOUND ( 'NONE', #23845, .T. ) ;
#33974 = CARTESIAN_POINT ( 'NONE',  ( -0.8759842519685039353, -0.1574803149606299191, 1.417322834645669216 ) ) ;
#33973 = CARTESIAN_POINT ( 'NONE',  ( 1.002407869896990045, 0.1264236179284866091, 0.8932086613635591421 ) ) ;
#33975 = CARTESIAN_POINT ( 'NONE',  ( 0.9500414927467377701, -0.1787899950787401604, 1.830708661363559253 ) ) ;
#33976 = CARTESIAN_POINT ( 'NONE',  ( 0.1787899950787401882, -0.7682086613635590311, -2.189545951927503898E-17 ) ) ;
#33977 = VERTEX_POINT ( 'NONE', #18899 ) ;
#33978 = CARTESIAN_POINT ( 'NONE',  ( 0.4330708661417297933, 0.1864803149606300281, 1.186023622047243986 ) ) ;
#33979 = CARTESIAN_POINT ( 'NONE',  ( -0.06523048226347956391, -1.467027558947591848, 0.1574803149606297803 ) ) ;
#33980 = CARTESIAN_POINT ( 'NONE',  ( -0.8107537697050253289, 0.1574803149606300301, 0.05167322823892971095 ) ) ;
#33981 = CARTESIAN_POINT ( 'NONE',  ( 1.054774247047244540, -0.07405724077823318263, 1.161417322780881278 ) ) ;
#33982 = DIRECTION ( 'NONE',  ( 0.000000000000000000, -0.7880107536067199048, 0.6156614753256609562 ) ) ;
#33983 = CARTESIAN_POINT ( 'NONE',  ( -0.06523048226347956391, -1.673720472440946017, 0.1574803149606297803 ) ) ;
#33984 = FACE_OUTER_BOUND ( 'NONE', #33419, .T. ) ;
#33985 = ( BOUNDED_CURVE ( )  B_SPLINE_CURVE ( 2, ( #13433, #46467, #43101, #47193, #24680, #35930, #9835, #21547, #36185 ),
 .UNSPECIFIED., .F., .T. ) 
 B_SPLINE_CURVE_WITH_KNOTS ( ( 3, 2, 2, 2, 3 ),
 ( 0.1100000000000000006, 0.1125000000000000028, 0.1150000000000000050, 0.1174999999999999933, 0.1199999999999999956 ),
 .UNSPECIFIED. ) 
 CURVE ( )  GEOMETRIC_REPRESENTATION_ITEM ( )  RATIONAL_B_SPLINE_CURVE ( ( 1.000000000000000000, 0.9238795325112869605, 1.000000000000000000, 0.9238795325112869605, 1.000000000000000000, 0.9238795325112869605, 1.000000000000000000, 0.9238795325112869605, 1.000000000000000000 ) ) 
 REPRESENTATION_ITEM ( '' )  ) ;
#33986 = ORIENTED_EDGE ( 'NONE', *, *, #12809, .F. ) ;
#33987 = CARTESIAN_POINT ( 'NONE',  ( 0.1574803149606299746, -0.5708661417322835607, 1.713085361781126803 ) ) ;
#33988 = CARTESIAN_POINT ( 'NONE',  ( -0.6971942568897626646, -0.07405724077823297447, 0.2411417322297011168 ) ) ;
#33989 = CARTESIAN_POINT ( 'NONE',  ( 0.1264236179284866091, 0.09793307091990532953, -0.1264236179284866091 ) ) ;
#33991 = CARTESIAN_POINT ( 'NONE',  ( 0.1264236179284866091, -1.476870078686393750, -0.1264236179284866091 ) ) ;
#33990 = CARTESIAN_POINT ( 'NONE',  ( 0.1574803149606300301, -0.3548228345381419513, 0.06523048226347956391 ) ) ;
#33992 = CARTESIAN_POINT ( 'NONE',  ( -0.7495606340400177148, -0.1264236179284866091, 1.857775590497417362 ) ) ;
#33993 = CARTESIAN_POINT ( 'NONE',  ( -0.6971942568897637749, 2.189545951927499583E-17, 0.9079724408911180600 ) ) ;
#33994 = VECTOR ( 'NONE', #12582, 39.37007874015748143 ) ;
#33995 = CARTESIAN_POINT ( 'NONE',  ( -1.054774247047244096, 0.000000000000000000, 0.5782480314422993040 ) ) ;
#33996 = FACE_OUTER_BOUND ( 'NONE', #15417, .T. ) ;
#33997 = CARTESIAN_POINT ( 'NONE',  ( 0.5962569168439626477, 4.766607801171850497E-17, 0.000000000000000000 ) ) ;
#33998 = DIRECTION ( 'NONE',  ( 8.659560562353054383E-17, 0.7071067811867007835, -0.7071067811863941399 ) ) ;
#33999 = DIRECTION ( 'NONE',  ( 1.363218471095259303E-17, 0.6156614753256575145, 0.7880107536067225693 ) ) ;
#34000 = CARTESIAN_POINT ( 'NONE',  ( 0.1264236179284866091, -0.5134113698040417839, 0.1264236179284866091 ) ) ;
#34001 = DIRECTION ( 'NONE',  ( 0.000000000000000000, -0.2126700594527834998, 0.9771240687918549828 ) ) ;
#34002 = CARTESIAN_POINT ( 'NONE',  ( 1.033464566929134687, -0.06523048226347956391, 1.936515748031494510 ) ) ;
#34003 = EDGE_CURVE ( 'NONE', #29529, #649, #10095, .T. ) ;
#34004 = ( BOUNDED_CURVE ( )  B_SPLINE_CURVE ( 2, ( #8913, #31446, #13239, #6243, #31213, #45789, #27867, #23543, #24013 ),
 .UNSPECIFIED., .F., .T. ) 
 B_SPLINE_CURVE_WITH_KNOTS ( ( 3, 2, 2, 2, 3 ),
 ( 0.1250000000000000000, 0.1275000000000000022, 0.1300000000000000044, 0.1325000000000000067, 0.1350000000000000089 ),
 .UNSPECIFIED. ) 
 CURVE ( )  GEOMETRIC_REPRESENTATION_ITEM ( )  RATIONAL_B_SPLINE_CURVE ( ( 1.000000000000000000, 0.9238795325112869605, 1.000000000000000000, 0.9238795325112869605, 1.000000000000000000, 0.9238795325112869605, 1.000000000000000000, 0.9238795325112869605, 1.000000000000000000 ) ) 
 REPRESENTATION_ITEM ( '' )  ) ;
#34005 = CARTESIAN_POINT ( 'NONE',  ( -1.002407869896990045, 0.1264236179284866091, 0.4995078739619842612 ) ) ;
#34006 = DIRECTION ( 'NONE',  ( 1.822029033848725028E-16, 0.000000000000000000, 1.000000000000000000 ) ) ;
#34007 = EDGE_CURVE ( 'NONE', #44611, #9478, #36874, .T. ) ;
#34008 = VERTEX_POINT ( 'NONE', #40688 ) ;
#34009 = CARTESIAN_POINT ( 'NONE',  ( 0.2471921300642929697, -0.09379707428445169248, 0.03645430680490753528 ) ) ;
#34010 = EDGE_CURVE ( 'NONE', #45765, #36143, #613, .T. ) ;
#34011 = CARTESIAN_POINT ( 'NONE',  ( -0.9500414927467377701, -0.1787899950787401604, 1.476377952702141449 ) ) ;
#34012 = EDGE_CURVE ( 'NONE', #35433, #29301, #11264, .T. ) ;
#34013 = CARTESIAN_POINT ( 'NONE',  ( 0.1787899950787401604, -1.326771653489542402, 0.07405724077823318263 ) ) ;
#34014 = CARTESIAN_POINT ( 'NONE',  ( 0.1787899950787401882, -1.476870078686393750, -2.189545951927503898E-17 ) ) ;
#34015 = CARTESIAN_POINT ( 'NONE',  ( 0.7185039370078739607, 1.928577636452523993E-17, 0.1870078740157480324 ) ) ;
#34016 = FACE_OUTER_BOUND ( 'NONE', #19633, .T. ) ;
#34017 = CARTESIAN_POINT ( 'NONE',  ( 0.9873396505805591694, -0.1113553986120547346, 0.4379921259842519676 ) ) ;
#34018 = CARTESIAN_POINT ( 'NONE',  ( 0.5358894627757212481, 4.766607801171850497E-17, 0.000000000000000000 ) ) ;
#34019 = CARTESIAN_POINT ( 'NONE',  ( -0.7185039370078746268, 0.06523048226347956391, 1.040846456585385882 ) ) ;
#34020 = CARTESIAN_POINT ( 'NONE',  ( 0.7495606340400177148, 0.1264236179284866091, 0.5536417322297008115 ) ) ;
#34021 = CARTESIAN_POINT ( 'NONE',  ( 1.002407869896990045, 0.1264236179284866091, 0.06643700782025216411 ) ) ;
#34023 = CARTESIAN_POINT ( 'NONE',  ( 1.033464566929133799, 0.000000000000000000, 0.3641732283464567121 ) ) ;
#34022 = CARTESIAN_POINT ( 'NONE',  ( -0.06523048226347956391, -0.2170275590551181411, 0.1574803149606297803 ) ) ;
#34024 = CARTESIAN_POINT ( 'NONE',  ( 0.8759842519685039353, 0.1574803149606299191, 1.899606299105070839 ) ) ;
#34025 = ORIENTED_EDGE ( 'NONE', *, *, #8528, .F. ) ;
#34026 = DIRECTION ( 'NONE',  ( -0.000000000000000000, 0.000000000000000000, 1.000000000000000000 ) ) ;
#34027 = CARTESIAN_POINT ( 'NONE',  ( -0.6971942568897648851, 0.07405724077823318263, 1.067913385773007651 ) ) ;
#34028 = CARTESIAN_POINT ( 'NONE',  ( 1.033464566929134687, 0.06523048226347956391, 0.9571850393700783721 ) ) ;
#34029 = CARTESIAN_POINT ( 'NONE',  ( 0.7185039370078739607, 0.000000000000000000, 4.498031496062992574 ) ) ;
#34030 = CARTESIAN_POINT ( 'NONE',  ( 0.2559055118110236116, -0.1477471161312047254, -0.1122047244094488277 ) ) ;
#34031 = DIRECTION ( 'NONE',  ( -1.000000000000000000, 0.000000000000000000, 0.000000000000000000 ) ) ;
#34032 = DIRECTION ( 'NONE',  ( 0.000000000000000000, 0.6156614753256591799, 0.7880107536067213481 ) ) ;
#34033 = ORIENTED_EDGE ( 'NONE', *, *, #4470, .T. ) ;
#34034 = CARTESIAN_POINT ( 'NONE',  ( 0.1527637205565704759, 0.02877039512963421378, -0.1377952755905511861 ) ) ;
#34035 = AXIS2_PLACEMENT_3D ( 'NONE', #38767, #35184, #43292 ) ;
#34036 = CYLINDRICAL_SURFACE ( 'NONE', #5411, 0.1574803149606299191 ) ;
#34037 = CARTESIAN_POINT ( 'NONE',  ( 0.8019270111902717657, -0.1787899950787401604, 0.7185039369541108556 ) ) ;
#34038 = CARTESIAN_POINT ( 'NONE',  ( 1.033464566929133799, 0.000000000000000000, 1.269685039370078705 ) ) ;
#34039 = CARTESIAN_POINT ( 'NONE',  ( -1.033464566929134687, 0.06523048226347956391, 0.4355314959554649201 ) ) ;
#34040 = CARTESIAN_POINT ( 'NONE',  ( 0.1264236179284866091, -1.708169291284818980, -0.1264236179284866091 ) ) ;
#34041 = CARTESIAN_POINT ( 'NONE',  ( 0.07405724077823318263, -0.9232283464029299447, -0.1787899950787401604 ) ) ;
#34042 = CARTESIAN_POINT ( 'NONE',  ( 0.1574803149606299191, -1.149606299212598381, -1.928577636452523993E-17 ) ) ;
#34043 = CARTESIAN_POINT ( 'NONE',  ( 1.033464566929134687, 0.06523048226347956391, 1.104822834538142340 ) ) ;
#34044 = CARTESIAN_POINT ( 'NONE',  ( 0.000000000000000000, 0.000000000000000000, -0.3149606299212598381 ) ) ;
#34045 = ORIENTED_EDGE ( 'NONE', *, *, #10681, .F. ) ;
#34046 = ORIENTED_EDGE ( 'NONE', *, *, #1873, .F. ) ;
#34047 = VECTOR ( 'NONE', #23588, 39.37007874015748854 ) ;
#34048 = CARTESIAN_POINT ( 'NONE',  ( -0.6971942568897648851, 0.07405724077823318263, 1.776574803095843924 ) ) ;
#34049 = CARTESIAN_POINT ( 'NONE',  ( 1.054774247047244540, 0.07405724077823318263, 1.722440944828125930 ) ) ;
#34050 = EDGE_LOOP ( 'NONE', ( #12343, #10033, #15136, #9902, #26683 ) ) ;
#34051 = CARTESIAN_POINT ( 'NONE',  ( -0.04256392708709098860, -0.2709142457700946527, -0.3044102143378214498 ) ) ;
#34052 = CARTESIAN_POINT ( 'NONE',  ( 0.6971942568897626646, -0.07405724077823297447, 0.4429133857730075952 ) ) ;
#34053 = CARTESIAN_POINT ( 'NONE',  ( -0.7495606340400177148, -0.1264236179284866091, 1.306594488135212728 ) ) ;
#34054 = DIRECTION ( 'NONE',  ( 1.822029033848725028E-16, 0.000000000000000000, 1.000000000000000000 ) ) ;
#34055 = CARTESIAN_POINT ( 'NONE',  ( -0.7495606340400177148, 0.1264236179284866091, 1.178641732229700922 ) ) ;
#34056 = CARTESIAN_POINT ( 'NONE',  ( -0.8759842519685039353, 0.1787899950787401882, 0.07627952750529173875 ) ) ;
#34057 = CARTESIAN_POINT ( 'NONE',  ( -0.1586641775163213364, 1.798092712879851174, -3.826876940038414610 ) ) ;
#34058 = CARTESIAN_POINT ( 'NONE',  ( -0.6971942568897648851, -0.07405724077823297447, 1.702755905458047003 ) ) ;
#34059 = CARTESIAN_POINT ( 'NONE',  ( -1.033464566929134687, 0.06523048226347956391, 1.970964566821606034 ) ) ;
#34060 = CARTESIAN_POINT ( 'NONE',  ( -0.8107537697050253289, 0.1574803149606300301, 1.636318897637794700 ) ) ;
#34061 = CARTESIAN_POINT ( 'NONE',  ( 0.6656920301128459450, -0.5708661417322835607, 0.3829649962626329729 ) ) ;
#34062 = CARTESIAN_POINT ( 'NONE',  ( -0.1749890002391197019, -0.09842519685039370636, -0.1786399317641141626 ) ) ;
#34063 = CARTESIAN_POINT ( 'NONE',  ( 0.9412147342319837628, -0.1574803149606297803, 1.016240157372787722 ) ) ;
#34064 = CARTESIAN_POINT ( 'NONE',  ( 0.2519685039370078705, 0.08090551181102362266, 9.908067607274841931E-18 ) ) ;
#34065 = ORIENTED_EDGE ( 'NONE', *, *, #16420, .F. ) ;
#34066 = AXIS2_PLACEMENT_3D ( 'NONE', #30801, #33090, #39526 ) ;
#34067 = EDGE_CURVE ( 'NONE', #3336, #8777, #11031, .T. ) ;
#34068 = EDGE_LOOP ( 'NONE', ( #4409, #13308, #22514, #23389 ) ) ;
#34069 = VECTOR ( 'NONE', #34987, 39.37007874015748143 ) ;
#34070 = ORIENTED_EDGE ( 'NONE', *, *, #2635, .F. ) ;
#34071 = AXIS2_PLACEMENT_3D ( 'NONE', #3264, #39204, #9995 ) ;
#34072 = AXIS2_PLACEMENT_3D ( 'NONE', #43705, #32487, #10669 ) ;
#34073 = EDGE_CURVE ( 'NONE', #38112, #25810, #41610, .T. ) ;
#34074 = CARTESIAN_POINT ( 'NONE',  ( -1.094772975963752103E-17, -0.9207677164816693294, -0.1787899950787401882 ) ) ;
#34075 = CARTESIAN_POINT ( 'NONE',  ( -0.07405724077823318263, -1.070866141678519456, -0.1787899950787401604 ) ) ;
#34076 = ( LENGTH_UNIT ( ) NAMED_UNIT ( * ) SI_UNIT ( $, .METRE. ) ) ;
#34077 = CARTESIAN_POINT ( 'NONE',  ( -0.1270800023317771588, -0.3996501087956441101, -0.1270800023317771588 ) ) ;
#34078 = CARTESIAN_POINT ( 'NONE',  ( 0.1113553986120547346, -1.813976377845228249, 0.1113553986120547346 ) ) ;
#34079 = CARTESIAN_POINT ( 'NONE',  ( 0.1913749512857760571, 0.1850038654768927093, -0.3090319486758464906 ) ) ;
#34080 = CARTESIAN_POINT ( 'NONE',  ( -0.7185039370078746268, 0.06523048226347977208, 0.1451771653543309226 ) ) ;
#34081 = CARTESIAN_POINT ( 'NONE',  ( 0.8759842519685039353, 0.1787899950787401882, 0.8193897637257637756 ) ) ;
#34082 = SURFACE_STYLE_FILL_AREA ( #26412 ) ;
#34083 = LINE ( 'NONE', #26655, #33835 ) ;
#34084 = CARTESIAN_POINT ( 'NONE',  ( 0.8019270111902717657, 0.1787899950787401604, 1.850393700733638624 ) ) ;
#34085 = CARTESIAN_POINT ( 'NONE',  ( 0.9873396505805591694, -0.1113553986120547346, 0.1624015748031496231 ) ) ;
#34086 = CARTESIAN_POINT ( 'NONE',  ( 0.3604359965418638123, 4.466152701071653354E-17, 0.000000000000000000 ) ) ;
#34087 = CARTESIAN_POINT ( 'NONE',  ( 0.1787899950787401882, -0.3794291338045042705, -2.189545951927503898E-17 ) ) ;
#34088 = LINE ( 'NONE', #1693, #7091 ) ;
#34089 = CARTESIAN_POINT ( 'NONE',  ( -0.07405724077823318263, -1.307086614119465695, -0.1787899950787401604 ) ) ;
#34090 = CARTESIAN_POINT ( 'NONE',  ( 0.8019270111902717657, -0.1787899950787401604, 0.1722440944344256208 ) ) ;
#34091 = DIRECTION ( 'NONE',  ( 0.000000000000000000, -0.2126700594527977661, 0.9771240687918517631 ) ) ;
#34092 = CARTESIAN_POINT ( 'NONE',  ( -0.6971942568897637749, 2.189545951927499583E-17, 1.774114173174582643 ) ) ;
#34093 = VERTEX_POINT ( 'NONE', #25648 ) ;
#34094 = AXIS2_PLACEMENT_3D ( 'NONE', #47178, #21780, #14361 ) ;
#34095 = CARTESIAN_POINT ( 'NONE',  ( -0.8759842519685039353, 0.1787899950787401882, 1.296751968450173154 ) ) ;
#34096 = CARTESIAN_POINT ( 'NONE',  ( -0.8107537697050254399, 0.1574803149606300301, 1.321358267716534751 ) ) ;
#34097 = CARTESIAN_POINT ( 'NONE',  ( 0.8759842519685039353, 0.1787899950787401882, 1.296751968450173154 ) ) ;
#34098 = CIRCLE ( 'NONE', #32567, 0.09842519685039370636 ) ;
#34099 = CONICAL_SURFACE ( 'NONE', #24876, 0.2559055118110236116, 1.047197551196597409 ) ;
#34100 = CARTESIAN_POINT ( 'NONE',  ( -0.7495606340400177148, 0.1264236179284866091, 0.5142716534895434011 ) ) ;
#34101 = CARTESIAN_POINT ( 'NONE',  ( -0.7495606340400177148, 0.1264236179284866091, 1.218011810969858111 ) ) ;
#34102 = CYLINDRICAL_SURFACE ( 'NONE', #27609, 0.1574803149606299191 ) ;
#34103 = CARTESIAN_POINT ( 'NONE',  ( 0.04296924029584964916, -0.09842683234878628340, -0.1736138147098973683 ) ) ;
#34104 = CARTESIAN_POINT ( 'NONE',  ( -0.7646288533564489232, 0.1113553986120547346, 1.353346456585388102 ) ) ;
#34105 = CARTESIAN_POINT ( 'NONE',  ( 1.054774247047244096, 0.000000000000000000, 0.5388779527021417826 ) ) ;
#34106 = CARTESIAN_POINT ( 'NONE',  ( -0.8759842519685039353, 0.1787899950787401882, 0.3863188975840318173 ) ) ;
#34107 = ORIENTED_EDGE ( 'NONE', *, *, #1994, .F. ) ;
#34108 = CARTESIAN_POINT ( 'NONE',  ( -1.033464566929134687, 0.06523048226347956391, 1.350885826771654141 ) ) ;
#34109 = ORIENTED_EDGE ( 'NONE', *, *, #13674, .F. ) ;
#34110 = CARTESIAN_POINT ( 'NONE',  ( -0.9873396505805591694, 0.1113553986120547346, 0.2509842519685039353 ) ) ;
#34111 = CARTESIAN_POINT ( 'NONE',  ( 0.6971942568897648851, -0.07405724077823297447, 1.190944881836001112 ) ) ;
#34112 = CARTESIAN_POINT ( 'NONE',  ( 1.614954907737318939E-16, 0.1564960629921311464, 0.3937007874015748254 ) ) ;
#34113 = CARTESIAN_POINT ( 'NONE',  ( -0.2559055118110236116, -0.06560852000721112409, -0.04485359485310594363 ) ) ;
#34114 = EDGE_LOOP ( 'NONE', ( #31383, #33558, #41997, #21598 ) ) ;
#34115 = ( BOUNDED_CURVE ( )  B_SPLINE_CURVE ( 2, ( #17765, #35981, #10601, #28331, #42902, #10112, #25200, #20647, #17058 ),
 .UNSPECIFIED., .F., .F. ) 
 B_SPLINE_CURVE_WITH_KNOTS ( ( 3, 2, 2, 2, 3 ),
 ( 0.2399999999999999911, 0.2424999999999999933, 0.2449999999999999956, 0.2474999999999999978, 0.2500000000000000000 ),
 .UNSPECIFIED. ) 
 CURVE ( )  GEOMETRIC_REPRESENTATION_ITEM ( )  RATIONAL_B_SPLINE_CURVE ( ( 1.000000000000000000, 0.9238795325112869605, 1.000000000000000000, 0.9238795325112869605, 1.000000000000000000, 0.9238795325112869605, 1.000000000000000000, 0.9238795325112869605, 1.000000000000000000 ) ) 
 REPRESENTATION_ITEM ( '' )  ) ;
#34116 = EDGE_CURVE ( 'NONE', #1914, #12042, #445, .T. ) ;
#34117 = CARTESIAN_POINT ( 'NONE',  ( 0.1564636162838570765, -0.1073287318776653676, -0.09487486835524251705 ) ) ;
#34118 = CARTESIAN_POINT ( 'NONE',  ( -0.8019270111902717657, 0.1787899950787401604, 0.07381889758403178958 ) ) ;
#34119 = CARTESIAN_POINT ( 'NONE',  ( 0.1787899950787401604, -1.490281448544198639, -0.07405724077823318263 ) ) ;
#34120 = VERTEX_POINT ( 'NONE', #918 ) ;
#34121 = CARTESIAN_POINT ( 'NONE',  ( 0.7185039370078746268, 0.06523048226347956391, 1.011318897637796033 ) ) ;
#34122 = CARTESIAN_POINT ( 'NONE',  ( 0.1787899950787401604, -0.4901574802611972093, -0.07405724077823318263 ) ) ;
#34123 = CARTESIAN_POINT ( 'NONE',  ( -1.033464566929133799, 0.000000000000000000, 1.338582677057826853 ) ) ;
#34124 = ORIENTED_EDGE ( 'NONE', *, *, #19305, .F. ) ;
#34125 = CIRCLE ( 'NONE', #1972, 0.1864803149606299448 ) ;
#34126 = CARTESIAN_POINT ( 'NONE',  ( -0.04257025887456828556, 0.2709160761542590556, -0.3049284531892009209 ) ) ;
#34127 = DIRECTION ( 'NONE',  ( -0.000000000000000000, 1.000000000000000000, -3.995705278811693553E-31 ) ) ;
#34128 = DIRECTION ( 'NONE',  ( -1.000000000000000000, 0.000000000000000000, 0.000000000000000000 ) ) ;
#34129 = CIRCLE ( 'NONE', #41703, 0.02900000000000052189 ) ;
#34130 = CARTESIAN_POINT ( 'NONE',  ( 0.07405724077823318263, -1.749999999946236340, -0.1787899950787401604 ) ) ;
#34131 = DIRECTION ( 'NONE',  ( -1.000000000000000078E-15, -1.000000000000000000, -1.000000000000000078E-15 ) ) ;
#34132 = CARTESIAN_POINT ( 'NONE',  ( 0.1678155187887284683, -0.09842519685039373412, 0.05062837720671468922 ) ) ;
#34133 = CARTESIAN_POINT ( 'NONE',  ( -1.002407869896990045, -0.1264236179284866091, 0.6126968503399370380 ) ) ;
#34135 = FACE_OUTER_BOUND ( 'NONE', #18937, .T. ) ;
#34134 = CARTESIAN_POINT ( 'NONE',  ( 0.1574803149606299191, -0.7559055118110236116, -1.928577636452523993E-17 ) ) ;
#34136 = CARTESIAN_POINT ( 'NONE',  ( 0.1797182628040039087, -1.558606801709029543, 0.07444174185955046430 ) ) ;
#34137 = CARTESIAN_POINT ( 'NONE',  ( -0.8107537697050254399, -0.1574803149606297803, 1.601870078632630756 ) ) ;
#34138 = DIRECTION ( 'NONE',  ( 1.822029033848725028E-16, 0.000000000000000000, 1.000000000000000000 ) ) ;
#34139 = CARTESIAN_POINT ( 'NONE',  ( 0.7495606340400177148, -0.1264236179284866091, 1.857775590497417362 ) ) ;
#34140 = CARTESIAN_POINT ( 'NONE',  ( 1.054774247047244540, -0.07405724077823318263, 0.2559055117572600624 ) ) ;
#34141 = ORIENTED_EDGE ( 'NONE', *, *, #29501, .T. ) ;
#34142 = CARTESIAN_POINT ( 'NONE',  ( 0.1627249056762490320, 1.099487083487566963, -0.04739565599252346800 ) ) ;
#34143 = CARTESIAN_POINT ( 'NONE',  ( -0.8107537697050254399, -0.1574803149606297803, 1.444389763672000671 ) ) ;
#34144 = CARTESIAN_POINT ( 'NONE',  ( -1.033464566929133799, 0.000000000000000000, 1.584645669291338654 ) ) ;
#34145 = CARTESIAN_POINT ( 'NONE',  ( -0.1264236179284866091, -0.03986220467064590517, 0.1264236179284866091 ) ) ;
#34146 = CARTESIAN_POINT ( 'NONE',  ( 0.6971942568897626646, -0.07405724077823297447, 0.4773622046706456068 ) ) ;
#34147 = EDGE_CURVE ( 'NONE', #12585, #30476, #29285, .T. ) ;
#34148 = CARTESIAN_POINT ( 'NONE',  ( 0.7330336333443192576, -0.08909248707107361720, 0.03937010521645695205 ) ) ;
#34150 = LINE ( 'NONE', #20206, #20080 ) ;
#34149 = CARTESIAN_POINT ( 'NONE',  ( 0.6971942568897648851, 0.07405724077823318263, 1.299212598371434435 ) ) ;
#34151 = DIRECTION ( 'NONE',  ( -1.000000000000000000, -0.000000000000000000, -0.000000000000000000 ) ) ;
#34152 = CARTESIAN_POINT ( 'NONE',  ( 0.6195511811023604043, 0.4133858267716528090, 1.186023622047243986 ) ) ;
#34153 = CARTESIAN_POINT ( 'NONE',  ( -1.054774247047244096, 0.000000000000000000, 1.281988188922614125 ) ) ;
#34154 = CARTESIAN_POINT ( 'NONE',  ( 0.7185039370078746268, 0.06523048226347956391, 0.7652559054042838982 ) ) ;
#34155 = ORIENTED_EDGE ( 'NONE', *, *, #33136, .T. ) ;
#34156 = CARTESIAN_POINT ( 'NONE',  ( -1.033464566929134687, 0.06523048226347956391, 0.1993110235145201248 ) ) ;
#34157 = CARTESIAN_POINT ( 'NONE',  ( 0.8488709075541929217, 0.1740638475949229103, 0.03937009123436348290 ) ) ;
#34158 = ORIENTED_EDGE ( 'NONE', *, *, #31931, .T. ) ;
#34159 = CARTESIAN_POINT ( 'NONE',  ( -0.07444174185955065859, -0.07238632926808483137, 0.1797182628040039087 ) ) ;
#34160 = CARTESIAN_POINT ( 'NONE',  ( -0.1264236179284866091, -1.309547244040724312, -0.1264236179284866091 ) ) ;
#34161 = CARTESIAN_POINT ( 'NONE',  ( 0.7495606340400177148, -0.1264236179284866091, 1.621555118056472455 ) ) ;
#34162 = CARTESIAN_POINT ( 'NONE',  ( -0.9412147342319837628, 0.1574803149606300301, 1.277066929133857442 ) ) ;
#34163 = AXIS2_PLACEMENT_3D ( 'NONE', #41525, #23829, #16863 ) ;
#34164 = CARTESIAN_POINT ( 'NONE',  ( -0.8759842519685039353, 0.1574803149606299191, 1.151574803042078710 ) ) ;
#34166 = CARTESIAN_POINT ( 'NONE',  ( -0.8107537697050254399, 0.1574803149606300301, 0.7603346455617647770 ) ) ;
#34165 = LINE ( 'NONE', #19516, #18828 ) ;
#34167 = CARTESIAN_POINT ( 'NONE',  ( -0.7646288533564489232, -0.1113553986120547346, 0.4970472439869613734 ) ) ;
#34168 = B_SPLINE_CURVE_WITH_KNOTS ( 'NONE', 3,
 ( #14887, #30010, #11758, #22531, #29316, #7917, #37149, #11294, #18929, #11527, #702, #37377, #25906, #33355, #11064, #15360 ),
 .UNSPECIFIED., .F., .F.,
 ( 4, 2, 2, 2, 2, 2, 2, 4 ),
 ( 0.000000000000000000, 0.0001515175770179333456, 0.0003030351540358666913, 0.0006060703080717382615, 0.001212140616143477607, 0.002424281232286962587, 0.003636421848430447783, 0.004848562464573932980 ),
 .UNSPECIFIED. ) ;
#34169 = VERTEX_POINT ( 'NONE', #33325 ) ;
#34170 = ORIENTED_EDGE ( 'NONE', *, *, #12189, .T. ) ;
#34171 = CARTESIAN_POINT ( 'NONE',  ( -0.05769093565148274150, -0.07859528327913033185, -0.2521251929553486315 ) ) ;
#34172 = EDGE_CURVE ( 'NONE', #7028, #26907, #30216, .T. ) ;
#34173 = CARTESIAN_POINT ( 'NONE',  ( -0.1574803149606297803, -0.01525590540428398145, 0.06523048226347956391 ) ) ;
#34174 = CARTESIAN_POINT ( 'NONE',  ( -1.002407869896990045, 0.1264236179284866091, 1.291830708607653477 ) ) ;
#34175 = CIRCLE ( 'NONE', #28808, 0.3937007874015748254 ) ;
#34176 = VERTEX_POINT ( 'NONE', #15100 ) ;
#34177 = EDGE_CURVE ( 'NONE', #21269, #30249, #20827, .T. ) ;
#34178 = CARTESIAN_POINT ( 'NONE',  ( -0.8759842519685039353, 0.1574803149606299191, 0.2460629920184571051 ) ) ;
#34179 = CARTESIAN_POINT ( 'NONE',  ( -0.6971942568897626646, 0.07405724077823318263, 0.2805118109698587214 ) ) ;
#34180 = CARTESIAN_POINT ( 'NONE',  ( 0.9412147342319837628, 0.1574803149606300301, 1.857775590443653480 ) ) ;
#34181 = LINE ( 'NONE', #41787, #19852 ) ;
#34182 = CARTESIAN_POINT ( 'NONE',  ( -0.1264236179284866091, -0.9563247556308129838, 0.1264236179284866091 ) ) ;
#34183 = ORIENTED_EDGE ( 'NONE', *, *, #43038, .F. ) ;
#34184 = CARTESIAN_POINT ( 'NONE',  ( 0.07405724077823318263, -0.01279527553678768380, -0.1787899950787401604 ) ) ;
#34185 = ORIENTED_EDGE ( 'NONE', *, *, #9610, .T. ) ;
#34186 = EDGE_CURVE ( 'NONE', #11484, #22073, #151, .T. ) ;
#34187 = DIRECTION ( 'NONE',  ( -1.000000000000000000, 0.000000000000000000, 0.000000000000000000 ) ) ;
#34188 = CARTESIAN_POINT ( 'NONE',  ( -0.8759842519685039353, 0.000000000000000000, 0.000000000000000000 ) ) ;
#34189 = EDGE_CURVE ( 'NONE', #11117, #43450, #18962, .T. ) ;
#34190 = DIRECTION ( 'NONE',  ( 1.000000000000000000, 0.000000000000000000, -1.822029033848725275E-16 ) ) ;
#34191 = CARTESIAN_POINT ( 'NONE',  ( -0.07405724077823318263, -0.5885826771115909573, 0.1787899950787401604 ) ) ;
#34192 = CARTESIAN_POINT ( 'NONE',  ( -1.002407869896990045, 0.1264236179284866091, 0.1500984251430867999 ) ) ;
#34193 = CARTESIAN_POINT ( 'NONE',  ( -0.8759842519685039353, 0.1574803149606299191, 0.8858267716535432879 ) ) ;
#34194 = CARTESIAN_POINT ( 'NONE',  ( -0.1377952755905510751, 1.687505431895957647E-17, -0.3149606299212598381 ) ) ;
#34195 = CARTESIAN_POINT ( 'NONE',  ( 0.07444174185955046430, -1.036953258401943412, -0.1797182628040039087 ) ) ;
#34196 = CARTESIAN_POINT ( 'NONE',  ( 0.7185039370078746268, -0.06523048226347956391, 1.094980314960629419 ) ) ;
#34197 = CARTESIAN_POINT ( 'NONE',  ( 0.6971942568897637749, 2.189545951927499583E-17, 0.8735236219934803259 ) ) ;
#34198 = CARTESIAN_POINT ( 'NONE',  ( 0.6971942568897648851, -0.07405724077823297447, 1.422244094434425898 ) ) ;
#34199 = CARTESIAN_POINT ( 'NONE',  ( -0.8759842519685039353, 0.000000000000000000, 0.000000000000000000 ) ) ;
#34200 = CARTESIAN_POINT ( 'NONE',  ( 0.7185039370078746268, -0.06523048226347956391, 1.528051181102361600 ) ) ;
#34202 = DIRECTION ( 'NONE',  ( 0.000000000000000000, 0.000000000000000000, -1.000000000000000000 ) ) ;
#34201 = CARTESIAN_POINT ( 'NONE',  ( 0.7353396263524580867, -0.09417691312399201209, 1.985127456826107251 ) ) ;
#34203 = CYLINDRICAL_SURFACE ( 'NONE', #32038, 0.1574803149606299191 ) ;
#34204 = CARTESIAN_POINT ( 'NONE',  ( 0.1113553986120547346, -0.6624015746956219974, -0.1113553986120547346 ) ) ;
#34205 = DIRECTION ( 'NONE',  ( 1.000000000000000000, -3.469446951953625233E-15, -0.000000000000000000 ) ) ;
#34207 = PLANE ( 'NONE',  #21551 ) ;
#34206 = CARTESIAN_POINT ( 'NONE',  ( 0.7495606340400177148, -0.1264236179284866091, 1.031003936954110189 ) ) ;
#34208 = CARTESIAN_POINT ( 'NONE',  ( 0.7495606340400177148, -0.1264236179284866091, 1.783956692859621995 ) ) ;
#34209 = CARTESIAN_POINT ( 'NONE',  ( 0.1787899950787401604, -0.8494094487651332459, 0.07405724077823318263 ) ) ;
#34210 = EDGE_LOOP ( 'NONE', ( #673, #19434, #8921, #40155 ) ) ;
#34211 = CARTESIAN_POINT ( 'NONE',  ( -0.8107537697050254399, 0.1574803149606300301, 0.8489173228346468258 ) ) ;
#34212 = CARTESIAN_POINT ( 'NONE',  ( 0.1574803149606299191, 0.3740157480314960647, 0.9783464566929134243 ) ) ;
#34213 = CARTESIAN_POINT ( 'NONE',  ( -9.642888182262618425E-18, -1.641732283357039357, -0.1574803149606299191 ) ) ;
#34214 = CARTESIAN_POINT ( 'NONE',  ( -0.7185039370078746268, 0.06523048226347956391, 0.09596456682160688090 ) ) ;
#34215 = CARTESIAN_POINT ( 'NONE',  ( 0.006378642920406700847, -0.1475107277140030593, 0.02009854774583735501 ) ) ;
#34216 = CARTESIAN_POINT ( 'NONE',  ( 0.8019270111902717657, 0.1787899950787401604, 1.136811023568283119 ) ) ;
#34217 = EDGE_CURVE ( 'NONE', #21986, #18116, #10749, .T. ) ;
#34218 = VERTEX_POINT ( 'NONE', #45472 ) ;
#34219 = CARTESIAN_POINT ( 'NONE',  ( 0.2066929133858268486, -0.4410959923581754816, -0.9673892061308019263 ) ) ;
#34220 = CARTESIAN_POINT ( 'NONE',  ( 0.1574803149606300301, -1.781988188976379117, 0.06523048226347956391 ) ) ;
#34221 = CARTESIAN_POINT ( 'NONE',  ( -0.3980944881889762477, 0.1574803149606354702, 0.7480314960629921295 ) ) ;
#34222 = CARTESIAN_POINT ( 'NONE',  ( 1.033464566929134687, 0.06523048226347956391, 0.2485236220472441526 ) ) ;
#34223 = CARTESIAN_POINT ( 'NONE',  ( -1.054774247047244540, -0.07405724077823318263, 0.2165354330171024577 ) ) ;
#34224 = EDGE_CURVE ( 'NONE', #2888, #40610, #1695, .T. ) ;
#34225 = CARTESIAN_POINT ( 'NONE',  ( -1.094772975963752103E-17, -1.590059055064346305, -0.1787899950787401882 ) ) ;
#34226 = CARTESIAN_POINT ( 'NONE',  ( -0.9500414927467378812, -0.1787899950787401604, 1.825787401521040243 ) ) ;
#34227 = CARTESIAN_POINT ( 'NONE',  ( -0.6971942568897648851, 0.07405724077823318263, 0.8661417322297002563 ) ) ;
#34228 = CARTESIAN_POINT ( 'NONE',  ( -0.8759842519685039353, 0.1787899950787401882, 0.4699803149068661479 ) ) ;
#34229 = CARTESIAN_POINT ( 'NONE',  ( 0.000000000000000000, 0.000000000000000000, 0.000000000000000000 ) ) ;
#34230 = CARTESIAN_POINT ( 'NONE',  ( -0.1377952755905511584, 0.1574803149606320007, -0.9074803149606294195 ) ) ;
#34231 = CYLINDRICAL_SURFACE ( 'NONE', #23388, 0.1574803149606299191 ) ;
#34232 = DIRECTION ( 'NONE',  ( -1.000000000000000000, 0.000000000000000000, 0.000000000000000000 ) ) ;
#34233 = CARTESIAN_POINT ( 'NONE',  ( 0.1787899950787401604, -0.5109507398827820568, 0.07405724077823318263 ) ) ;
#34234 = CARTESIAN_POINT ( 'NONE',  ( -0.08566400215306142762, -0.08956101637306594643, -0.1598881813297279575 ) ) ;
#34235 = CARTESIAN_POINT ( 'NONE',  ( 0.8107537697050254399, 0.1574803149606300301, 1.793799212598424342 ) ) ;
#34236 = CARTESIAN_POINT ( 'NONE',  ( -0.7185039370078739607, 1.928577636452523993E-17, 0.1476377952755905387 ) ) ;
#34237 = CARTESIAN_POINT ( 'NONE',  ( -1.002407869896990045, -0.1264236179284866091, 0.4502952755367874427 ) ) ;
#34238 = CARTESIAN_POINT ( 'NONE',  ( 0.7185039370078746268, 0.06523048226347956391, 1.198326771546015967 ) ) ;
#34239 = ORIENTED_EDGE ( 'NONE', *, *, #28209, .F. ) ;
#34240 = CARTESIAN_POINT ( 'NONE',  ( -0.4620708661417322616, 0.6102362204724408601, 0.5167322834645649010 ) ) ;
#34241 = CARTESIAN_POINT ( 'NONE',  ( -0.7495606340400177148, -0.1264236179284866091, 1.468996062938362046 ) ) ;
#34242 = CARTESIAN_POINT ( 'NONE',  ( -0.07405724077823318263, -1.469488188922614791, -0.1787899950787401604 ) ) ;
#34243 = CARTESIAN_POINT ( 'NONE',  ( -1.094772975963752103E-17, -1.506397637741511586, -0.1787899950787401882 ) ) ;
#34244 = CIRCLE ( 'NONE', #38025, 0.08090551181102362266 ) ;
#34245 = LINE ( 'NONE', #41611, #7832 ) ;
#34246 = DIRECTION ( 'NONE',  ( 0.000000000000000000, 0.000000000000000000, -1.000000000000000000 ) ) ;
#34247 = CARTESIAN_POINT ( 'NONE',  ( -0.7646288533564489232, -0.1113553986120547346, 1.284448818790110192 ) ) ;
#34249 = CARTESIAN_POINT ( 'NONE',  ( 0.7185039370078739607, 1.928577636452523993E-17, 1.751968503829480106 ) ) ;
#34248 = CARTESIAN_POINT ( 'NONE',  ( -0.1574803149606299191, -0.4212598425196850127, 0.000000000000000000 ) ) ;
#34250 = VERTEX_POINT ( 'NONE', #12928 ) ;
#34251 = CARTESIAN_POINT ( 'NONE',  ( 0.000000000000000000, 0.000000000000000000, 0.000000000000000000 ) ) ;
#34252 = CARTESIAN_POINT ( 'NONE',  ( 0.7185039370078739607, 1.928577636452523993E-17, 1.131889763779527547 ) ) ;
#34253 = CARTESIAN_POINT ( 'NONE',  ( 0.000000000000000000, 1.205361022782826802E-17, -0.09842519685039370636 ) ) ;
#34254 = ( BOUNDED_SURFACE ( )  B_SPLINE_SURFACE ( 1, 2, ( 
 ( #33679, #18787, #3704, #33440, #557, #40805, #15213, #44406, #30105, #11622, #791, #32965, #89, #1039, #15697, #30558, #5345, #31025, #1998, #16847, #30797, #16625, #26956, #41508, #41987, #8714, #12337, #8957, #45120, #31488, #12094, #31255, #45362, #9444, #45832, #23349, #26717, #16400, #37961, #34369, #5111, #23577, #5835, #41272, #19734, #4873, #12813, #9191, #2228, #12575, #27203, #23809, #19501, #19968, #1509, #38428, #13041, #27678, #20201, #5594, #34608, #34854, #41753, #45591, #16163, #1275, #38185, #15929, #42240, #24060, #1758, #8472, #38665, #27443, #20444, #35080, #23106, #37722, #34145, #28364, #2695, #6291, #36264, #18031, #46075, #17322, #13725, #10143, #42472, #3166, #27909, #17795, #46780, #3415, #39115, #36009, #24752, #14216, #39586, #42933, #2920, #28855, #13275, #38890, #31959, #9676, #24292, #20911, #32442, #46543, #6052, #31724, #39347, #20679, #21383, #6767, #13501, #47020, #6529, #10624, #28133, #21142, #35319, #25226, #35778, #39814, #2459, #17555, #42690, #28617, #17086, #7003, #32193, #21630, #46317, #9907, #24517, #13967, #35551, #43177, #10385, #24991, #26420, #14445, #3648, #25484, #33386, #29804, #22799, #18498, #276, #44351, #40050, #40518, #29354, #11558, #4325, #733, #40750, #26183, #7707, #7947, #33155, #18727, #11094, #21872, #14921, #36493, #33618, #22565, #44127, #47264, #44582, #18268, #4108, #30039, #11801, #22323, #18958, #29586, #36716, #40286, #37407, #4564, #32677, #3879, #11326, #25938, #29099, #37181, #43657, #15395, #501, #10864, #25717, #40988, #36951, #8173, #7250, #15160, #32911, #31, #14680, #43896, #7471, #22091, #23999, #12268, #23749, #37899, #26659, #4814, #45300, #15634, #41925, #12753, #34087, #38360, #1448, #34791, #1217, #5057, #8412, #45768, #16106, #1931, #12036, #30731, #15868, #1692, #38598, #30496, #45056, #19910, #19437, #26891, #5531, #34316, #23040, #30272, #19199, #33858, #16565, #37658, #12518, #38130, #9132, #977, #19674, #20146, #41448, #8649, #16341, #23286, #27141, #41693, #8895, #44824, #23526, #41206, #5290, #34540, #30962, #45529, #27382, #12978, #31195, #27616, #42170, #9378, #2859, #43361, #39058, #20851, #17496, #46013, #13665, #2399, #32127, #24936, #21321, #13905, #46718, #28301, #28552, #6227, #39293, #31669, #42412, #35493, #9616, #6708, #43120, #17267, #20379, #17733, #24235, #24692, #3109, #32383, #42866, #39529, #2633, #9847, #13446, #10568, #25170, #5773, #24457, #31903, #46484, #2168, #10324, #35017, #35952, #6466, #16791, #46247, #46964, #10081, #14153, #28797, #21084, #35724, #31431, #13218, #27853, #38832, #5995, #20616, #28075, #35264, #17032, #42636, #25422, #18443, #36204, #15107, #33331, #7189, #11503, #22039, #7891, #21814, #25657, #29039, #18908, #36665, #22509, #32622, #3823, #36442, #22265, #11750, #3594, #18214, #40466, #39996, #32856, #44300, #7421, #43598, #3356, #44534, #39754, #4274, #10809, #33094, #25884, #29752, #6944, #11041, #26124, #47450, #14622, #36902, #29292, #43840, #215, #40232, #21566, #17968, #40695, #14865, #33564, #682, #29524, #44075, #15337, #29989, #47209, #7649, #14389, #4056, #18671, #454, #45006, #33810, #11986, #5008, #22749, #1646, #19867, #41161, #45482, #8600, #41880, #8365, #12219, #15585, #5486, #23240, #9086, #19144, #37853, #22991, #8845, #45721, #37602, #4763, #27090, #26609, #19390, #30921, #41402, #30223, #37355, #31152, #26371, #23706, #44770, #19627, #45248, #16291, #40930, #26842, #12710, #34041, #1166, #23482, #15825, #30450, #34268, #1398, #8126, #4509, #27335, #16058, #38313, #20101, #30685, #927, #12469, #41641, #38083, #5240, #34492, #34747, #1888, #16523, #5723, #13613, #10028, #3051, #46202, #28031, #24648, #20339, #20803, #9570, #39242, #32080, #28502, #21033, #6416, #35444, #35678, #13401, #46433, #38791, #2122, #42590, #16751, #13855, #2815, #24411, #27570, #24882, #31392, #31855, #10272, #39479, #2582, #46669, #9802, #16983, #20571, #17680, #32331, #12937, #31622, #39015, #6179, #9332, #17446, #42118, #43068, #28253, #23952, #5948, #6656, #17220, #21273, #35898, #38558, #34977, #42816, #45961, #13175, #27812, #42372, #24189, #35212, #2350, #30346, #44894, #39948, #18161, #44650, #28747, #15229, #37490, #19511, #15711, #36146, #43545, #43311, #3549, #32801, #10515, #10759, #39702, #22878, #25366, #25113, #572, #26732, #14101, #21508, #21759, #22644, #23120, #29876, #11867, #3300, #30117, #26492, #7138, #41054, #37249, #8252, #12107, #44418, #8013, #32572, #4646, #4401, #19273, #41285, #33929, #37733, #11635, #36395, #26255, #4889, #17919, #40818, #1052, #8485, #47157, #46911, #19028, #6890, #33696, #14341, #28987, #804, #15469, #13053, #41764, #31267, #38679, #41521, #38198, #34160, #23821, #34619, #16636, #24071, #5359, #5122, #1769, #19979, #34382, #31036, #16858, #9686, #1521, #45603, #2239, #46083, #45846, #5847, #38901, #6062, #2010, #27214, #1289, #15944, #8967, #30569, #12822, #5607, #38439, #16174, #45375, #12591, #27455, #27690, #41998, #9203, #20215, #42253, #43554, #47164, #21767, #21516, #3555, #3309, #40187, #21996, #3780, #18169, #32808, #33045, #171, #44024, #15061, #11228, #25839, #40420, #7604, #36850, #4004, #4712, #37307, #12168, #41349, #19096, #19340, #874, #30875, #33991, #4456, #26792, #34690, #22701, #30179, #30407, #30635, #31104, #8551, #5190, #11939, #38031, #19814, #1116, #34442, #45197, #1590, #5430, #23187, #16010, #41119, #16243, #12419, #45436, #20048, #12655, #45667, #37800, #15777, #4951, #12885, #26560, #44956, #27282, #41830, #8313, #9033, #19580, #27518, #41589, #23655, #22943, #38265, #1833, #16472, #34225, #8079, #33764, #15536, #1353, #44720, #27040, #8793, #37551, #23427, #13350, #34927, #9750, #27978, #45912, #42547, #24829, #21224, #13128, #24364, #28449, #6610, #24593, #17394, #43016, #35850, #9984, #35159, #3002, #46860, #2303, #39431, #6127, #13568, #31806, #46623, #5674, #42323, #32033, #39191, #20281, #42072, #16931, #24141, #16702, #38503, #2075, #2770, #31331, #10223, #46155, #31573, #20524, #14047, #27762, #38962, #9275, #35394, #9517, #17636, #35628, #23895, #6366, #38745, #20751, #13807, #5909, #32282, #2539, #17167, #46391, #28204, #42767, #20982, #25314, #21460, #3957, #7089, #10467, #47354, #7792, #43263, #3248, #3500, #3730, #4184, #14527, #25794, #32518, #11181, #40366, #39901, #7555 ),
 ( #39656, #33468, #588, #44206, #47104, #21949, #117, #18579, #28695, #29193, #33237, #43499, #10709, #22165, #21714, #28938, #25564, #14294, #25064, #6839, #364, #43740, #26023, #15014, #36346, #36091, #32994, #18114, #32757, #10945, #40136, #22409, #17874, #7333, #36571, #29434, #36804, #18811, #18350, #14764, #29667, #43977, #11405, #40598, #37035, #34397, #30821, #23377, #41534, #23131, #37984, #1065, #1306, #41067, #4414, #44907, #19044, #16190, #5138, #26741, #29889, #27227, #33711, #34173, #12606, #41780, #4903, #1537, #12120, #19288, #22890, #5374, #34634, #15244, #15961, #12365, #19995, #15723, #30359, #26983, #8027, #37745, #11882, #8741, #45391, #8981, #19764, #23602, #19524, #38214, #41300, #30581, #8265, #820, #8501, #15482, #44434, #11649, #45145, #26272, #40835, #30126, #22656, #37261, #44666, #26507, #37503, #4661, #33942, #10098, #40014, #21832, #1784, #21103, #17513, #13926, #45618, #6965, #31053, #21587, #3126, #7210, #42887, #39774, #28570, #17987, #43380, #32148, #6723, #32641, #16425, #42016, #35741, #12836, #27468, #24708, #36227, #2877, #9222, #34880, #43137, #23840, #25187, #10590, #16655, #3379, #46739, #47227, #31282, #10343, #38452, #29061, #24952, #14411, #5623, #39550, #45859, #32403, #20231, #13072, #28320, #17757, #2025, #39309, #43617, #21339, #6483, #35970, #46979, #14172, #10825, #28817, #25441, #26072, #29938, #44719, #11227, #44481, #7387, #33044, #22457, #40643, #37078, #4229, #33515, #25374, #39953, #26326, #19095, #21766, #18168, #32807, #47404, #14576, #37799, #1352, #12167, #8792, #8312, #22942, #45196, #33990, #38502, #27281, #12418, #37550, #27039, #1589, #30874, #41829, #9032, #5429, #45666, #34689, #42071, #43015, #32032, #38744, #13127, #6126, #42546, #2302, #16930, #46390, #24828, #42766, #6609, #9983, #20981, #35627, #27761, #32281, #21223, #8463, #34597, #30548, #24051, #31246, #23092, #20435, #46063, #41263, #30786, #38173, #37710, #19490, #19957, #12328, #41498, #23340, #1747, #16391, #31011, #23799, #28353, #20666, #6278, #46302, #206, #35542, #2682, #24742, #7642, #31950, #6517, #32184, #22029, #4045, #25873, #40458, #36891, #18662, #33322, #27899, #12206, #1156, #26831, #23467, #917, #22979, #15577, #41387, #15811, #23226, #38069, #19615, #44288, #8354, #11492, #4266, #9073, #31140, #27557, #13387, #42579, #45708, #31840, #34964, #9315, #16969, #6169, #31377, #9788, #46424, #42360, #25101, #14560, #18384, #24866, #39691, #2801, #25357, #3287, #18149, #149, #47147, #28484, #28976, #21750, #32318, #3538, #29463, #11211, #7588, #17433, #13841, #34204, #19321, #23161, #37779, #4933, #41564, #37287, #33499, #19072, #22203, #11681, #26306, #33970, #15754, #33744, #1331, #854, #33269, #30610, #11915, #9009, #20500, #20729, #31550, #45647, #46128, #17138, #30852, #27498, #5170, #9495, #9251, #19789, #27258, #42048, #23869, #34909, #31312, #46597, #14021, #32964, #88, #28421, #10438, #29157, #14735, #7060, #18084, #10918, #42742, #10677, #17608, #32004, #39400, #21687, #3472, #47323, #790, #19013, #33915, #7527, #25992, #44880, #26478, #335, #14982, #11621, #37004, #4383, #33678, #44638, #23105, #11854, #46074, #12812, #41986, #34853, #15928, #5110, #31254, #26955, #27677, #34368, #2227, #9443, #45361, #35079, #38889, #6051, #38664, #20443, #27202, #46316, #46779, #7002, #17085, #32676, #28363, #6528, #28132, #2919, #24990, #42689, #6766, #36008, #21629, #28854, #43415, #36263, #30, #11093, #3878, #22322, #26182, #275, #36950, #26419, #14920, #18957, #8172, #29585, #37406, #22564, #4107, #18726, #41692, #45767, #5056, #38597, #20378, #13217, #45055, #12267, #26890, #41447, #1447, #2398, #3108, #9615, #13445, #4508, #25656, #46140, #19389, #35380, #28192, #2755, #28680, #3229, #36556, #17861, #28434, #29173, #43725, #18568, #7778, #37248, #4645, #41520, #33695, #15710, #29875, #23360, #350, #44192, #20456, #42252, #16857, #17096, #9202, #24070, #5358, #27919, #35091, #31736, #5121, #19746, #12590, #38438, #1768, #23820, #12821, #5606, #20214, #21641, #7015, #28377, #40063, #25000, #14691, #18042, #32924, #24762, #47277, #43, #29365, #21393, #43905, #17332, #13736, #3177, #6540, #14224, #47034, #2928, #987, #29816, #18510, #40761, #44361, #14934, #22576, #23049, #40298, #44139, #37191, #12045, #7481, #37419, #30282, #36729, #287, #19209, #15172, #25949, #22333, #744, #30049, #5542, #16577, #31207, #46020, #1456, #8904, #9625, #42181, #5300, #41458, #45779, #12988, #38606, #20625, #2407, #39765, #24468, #14402, #17506, #3119, #39300, #46258, #6233, #28809, #46493, #3370, #28310, #10819, #21823, #6475, #37364, #15594, #37134, #44781, #41170, #18916, #37612, #44310, #18680, #26135, #32866, #25669, #22050, #33575, #15345, #29998, #18456, #226, #11283, #40939, #8135, #42379, #12478, #5732, #16301, #20347, #45731, #34754, #1896, #45969, #1175, #12228, #31161, #30458, #41412, #27101, #27819, #37863, #5017, #19637, #16068, #8856, #43319, #6897, #20811, #36155, #2821, #3308, #2592, #6424, #28039, #14347, #43076, #28996, #31632, #10281, #46442, #38798, #35220, #42824, #10037, #39487, #6664, #42599, #18442, #29038, #17732, #24935, #19330, #33979, #29523, #32382, #7188, #32855, #3822, #13904, #32621, #33093, #28796, #43360, #43839, #10567, #14152, #10808, #46963, #28551, #43119, #214, #47208, #11271, #14864, #25169, #10323, #18213, #39753, #36203, #6943, #25421, #7648, #39528, #21565, #6707, #14621, #11040, #4699, #14388, #43597, #25655, #21320, #21813, #3355, #40231, #44074, #25883, #22038, #7420, #36441, #36664, #39995, #47449, #17967, #3107, #3593, #29291, #40465, #22929, #37540, #35951, #13113, #4942, #19569, #31094, #12873, #45185, #45655, #38253, #27507, #45898, #19799, #9019, #34213, #42058, #23640, #9261, #27746, #38492, #38729, #1578, #12406, #34431, #5898, #1343, #27028, #23880, #5661, #15997, #34917, #16229, #20510, #34675, #20269, #30621, #2061, #16693, #31321, #8780, #42311, #9503, #8540, #5179, #1106, #5415, #30863, #24124, #15765, #45425, #41340, #12642, #27268, #41577, #41817, #30397, #44946, #23417, #20034, #12157, #26781, #23173, #37790, #38019, #1822, #16458, #30716, #2156, #42402, #19896, #35008, #1683, #38345, #27371, #42157, #1206, #37887, #9365, #1922, #23271, #37643, #16329, #19665, #5045, #34078, #34307, #45757, #1434, #38587, #41913, #5521 ) ),
 .UNSPECIFIED., .F., .F., .T. ) 
 B_SPLINE_SURFACE_WITH_KNOTS ( ( 2, 2 ),
 ( 3, 2, 2, 2, 2, 2, 2, 2, 2, 2, 2, 2, 2, 2, 2, 2, 2, 2, 2, 2, 2, 2, 2, 2, 2, 2, 2, 2, 2, 2, 2, 2, 2, 2, 2, 2, 2, 2, 2, 2, 2, 2, 2, 2, 2, 2, 2, 2, 2, 2, 2, 2, 2, 2, 2, 2, 2, 2, 2, 2, 2, 2, 2, 2, 2, 2, 2, 2, 2, 2, 2, 2, 2, 2, 2, 2, 2, 2, 2, 2, 2, 2, 2, 2, 2, 2, 2, 2, 2, 2, 2, 2, 2, 2, 2, 2, 2, 2, 2, 2, 2, 2, 2, 2, 2, 2, 2, 2, 2, 2, 2, 2, 2, 2, 2, 2, 2, 2, 2, 2, 2, 2, 2, 2, 2, 2, 2, 2, 2, 2, 2, 2, 2, 2, 2, 2, 2, 2, 2, 2, 2, 2, 2, 2, 2, 2, 2, 2, 2, 2, 2, 2, 2, 2, 2, 2, 2, 2, 2, 2, 2, 2, 2, 2, 2, 2, 2, 2, 2, 2, 2, 2, 2, 2, 2, 2, 2, 2, 2, 2, 2, 2, 2, 2, 2, 2, 2, 2, 2, 2, 2, 2, 2, 2, 2, 2, 2, 2, 2, 2, 2, 2, 2, 2, 2, 2, 2, 2, 2, 2, 2, 2, 2, 2, 2, 2, 2, 2, 2, 2, 2, 2, 2, 2, 2, 2, 2, 2, 2, 2, 2, 2, 2, 2, 2, 2, 2, 2, 2, 2, 2, 2, 2, 2, 2, 2, 2, 2, 2, 2, 2, 2, 2, 2, 2, 2, 2, 2, 2, 2, 2, 2, 2, 2, 2, 2, 2, 2, 2, 2, 2, 2, 2, 2, 2, 2, 2, 2, 2, 2, 2, 2, 2, 2, 2, 2, 2, 2, 2, 2, 2, 2, 2, 2, 2, 2, 2, 2, 2, 2, 2, 2, 2, 2, 2, 2, 2, 2, 2, 2, 2, 2, 2, 2, 2, 2, 2, 2, 2, 2, 2, 2, 2, 2, 2, 2, 2, 2, 2, 2, 2, 2, 2, 2, 2, 2, 2, 2, 2, 2, 2, 2, 2, 2, 2, 2, 2, 2, 2, 2, 2, 2, 2, 2, 2, 2, 2, 2, 2, 2, 2, 2, 2, 2, 2, 2, 2, 2, 2, 2, 2, 2, 2, 2, 2, 2, 2, 2, 2, 2, 2, 2, 2, 2, 2, 2, 2, 2, 2, 2, 2, 2, 2, 2, 2, 2, 2, 2, 2, 2, 3 ),
 ( 0.000000000000000000, 1.000000000000000000 ),
 ( 0.000000000000000000, 0.002500000000000000052, 0.005000000000000000104, 0.007499999999999999722, 0.01000000000000000021, 0.01250000000000000069, 0.01499999999999999944, 0.01750000000000000167, 0.02000000000000000042, 0.02249999999999999917, 0.02500000000000000139, 0.02750000000000000014, 0.02999999999999999889, 0.03250000000000000111, 0.03500000000000000333, 0.03749999999999999861, 0.04000000000000000083, 0.04250000000000000305, 0.04499999999999999833, 0.04750000000000000056, 0.05000000000000000278, 0.05249999999999999806, 0.05500000000000000028, 0.05750000000000000250, 0.05999999999999999778, 0.06250000000000000000, 0.06500000000000000222, 0.06750000000000000444, 0.07000000000000000666, 0.07249999999999999500, 0.07499999999999999722, 0.07749999999999999944, 0.08000000000000000167, 0.08250000000000000389, 0.08500000000000000611, 0.08749999999999999445, 0.08999999999999999667, 0.09249999999999999889, 0.09500000000000000111, 0.09750000000000000333, 0.1000000000000000056, 0.1024999999999999939, 0.1049999999999999961, 0.1074999999999999983, 0.1100000000000000006, 0.1125000000000000028, 0.1150000000000000050, 0.1174999999999999933, 0.1199999999999999956, 0.1224999999999999978, 0.1250000000000000000, 0.1275000000000000022, 0.1300000000000000044, 0.1325000000000000067, 0.1350000000000000089, 0.1375000000000000111, 0.1400000000000000133, 0.1424999999999999878, 0.1449999999999999900, 0.1474999999999999922, 0.1499999999999999944, 0.1524999999999999967, 0.1549999999999999989, 0.1575000000000000011, 0.1600000000000000033, 0.1625000000000000056, 0.1650000000000000078, 0.1675000000000000100, 0.1700000000000000122, 0.1724999999999999867, 0.1749999999999999889, 0.1774999999999999911, 0.1799999999999999933, 0.1824999999999999956, 0.1849999999999999978, 0.1875000000000000000, 0.1900000000000000022, 0.1925000000000000044, 0.1950000000000000067, 0.1975000000000000089, 0.2000000000000000111, 0.2025000000000000133, 0.2049999999999999878, 0.2074999999999999900, 0.2099999999999999922, 0.2124999999999999944, 0.2149999999999999967, 0.2174999999999999989, 0.2200000000000000011, 0.2225000000000000033, 0.2250000000000000056, 0.2275000000000000078, 0.2300000000000000100, 0.2325000000000000122, 0.2349999999999999867, 0.2374999999999999889, 0.2399999999999999911, 0.2424999999999999933, 0.2449999999999999956, 0.2474999999999999978, 0.2500000000000000000, 0.2525000000000000022, 0.2550000000000000044, 0.2575000000000000067, 0.2600000000000000089, 0.2625000000000000111, 0.2650000000000000133, 0.2675000000000000155, 0.2700000000000000178, 0.2725000000000000200, 0.2750000000000000222, 0.2775000000000000244, 0.2800000000000000266, 0.2824999999999999734, 0.2849999999999999756, 0.2874999999999999778, 0.2899999999999999800, 0.2924999999999999822, 0.2949999999999999845, 0.2974999999999999867, 0.2999999999999999889, 0.3024999999999999911, 0.3049999999999999933, 0.3074999999999999956, 0.3099999999999999978, 0.3125000000000000000, 0.3150000000000000022, 0.3175000000000000044, 0.3200000000000000067, 0.3225000000000000089, 0.3250000000000000111, 0.3275000000000000133, 0.3300000000000000155, 0.3325000000000000178, 0.3350000000000000200, 0.3375000000000000222, 0.3400000000000000244, 0.3425000000000000266, 0.3449999999999999734, 0.3474999999999999756, 0.3499999999999999778, 0.3524999999999999800, 0.3549999999999999822, 0.3574999999999999845, 0.3599999999999999867, 0.3624999999999999889, 0.3649999999999999911, 0.3674999999999999933, 0.3699999999999999956, 0.3724999999999999978, 0.3750000000000000000, 0.3775000000000000022, 0.3800000000000000044, 0.3825000000000000067, 0.3850000000000000089, 0.3875000000000000111, 0.3900000000000000133, 0.3925000000000000155, 0.3950000000000000178, 0.3975000000000000200, 0.4000000000000000222, 0.4025000000000000244, 0.4050000000000000266, 0.4074999999999999734, 0.4099999999999999756, 0.4124999999999999778, 0.4149999999999999800, 0.4174999999999999822, 0.4199999999999999845, 0.4224999999999999867, 0.4249999999999999889, 0.4274999999999999911, 0.4299999999999999933, 0.4324999999999999956, 0.4349999999999999978, 0.4375000000000000000, 0.4400000000000000022, 0.4425000000000000044, 0.4450000000000000067, 0.4475000000000000089, 0.4500000000000000111, 0.4525000000000000133, 0.4550000000000000155, 0.4575000000000000178, 0.4600000000000000200, 0.4625000000000000222, 0.4650000000000000244, 0.4675000000000000266, 0.4699999999999999734, 0.4724999999999999756, 0.4749999999999999778, 0.4774999999999999800, 0.4799999999999999822, 0.4824999999999999845, 0.4849999999999999867, 0.4874999999999999889, 0.4899999999999999911, 0.4924999999999999933, 0.4949999999999999956, 0.4974999999999999978, 0.5000000000000000000, 0.5024999999999999467, 0.5050000000000000044, 0.5074999999999999512, 0.5100000000000000089, 0.5124999999999999556, 0.5150000000000000133, 0.5174999999999999600, 0.5200000000000000178, 0.5224999999999999645, 0.5250000000000000222, 0.5274999999999999689, 0.5300000000000000266, 0.5324999999999999734, 0.5350000000000000311, 0.5374999999999999778, 0.5400000000000000355, 0.5424999999999999822, 0.5450000000000000400, 0.5474999999999999867, 0.5500000000000000444, 0.5524999999999999911, 0.5550000000000000488, 0.5574999999999999956, 0.5600000000000000533, 0.5625000000000000000, 0.5649999999999999467, 0.5675000000000000044, 0.5699999999999999512, 0.5725000000000000089, 0.5749999999999999556, 0.5775000000000000133, 0.5799999999999999600, 0.5825000000000000178, 0.5849999999999999645, 0.5875000000000000222, 0.5899999999999999689, 0.5925000000000000266, 0.5949999999999999734, 0.5975000000000000311, 0.5999999999999999778, 0.6025000000000000355, 0.6049999999999999822, 0.6075000000000000400, 0.6099999999999999867, 0.6125000000000000444, 0.6149999999999999911, 0.6175000000000000488, 0.6199999999999999956, 0.6225000000000000533, 0.6250000000000000000, 0.6274999999999999467, 0.6300000000000000044, 0.6324999999999999512, 0.6350000000000000089, 0.6374999999999999556, 0.6400000000000000133, 0.6424999999999999600, 0.6450000000000000178, 0.6474999999999999645, 0.6500000000000000222, 0.6524999999999999689, 0.6550000000000000266, 0.6574999999999999734, 0.6600000000000000311, 0.6624999999999999778, 0.6650000000000000355, 0.6674999999999999822, 0.6700000000000000400, 0.6724999999999999867, 0.6750000000000000444, 0.6774999999999999911, 0.6800000000000000488, 0.6824999999999999956, 0.6850000000000000533, 0.6875000000000000000, 0.6899999999999999467, 0.6925000000000000044, 0.6949999999999999512, 0.6975000000000000089, 0.6999999999999999556, 0.7025000000000000133, 0.7049999999999999600, 0.7075000000000000178, 0.7099999999999999645, 0.7125000000000000222, 0.7149999999999999689, 0.7175000000000000266, 0.7199999999999999734, 0.7225000000000000311, 0.7249999999999999778, 0.7275000000000000355, 0.7299999999999999822, 0.7325000000000000400, 0.7349999999999999867, 0.7375000000000000444, 0.7399999999999999911, 0.7425000000000000488, 0.7449999999999999956, 0.7475000000000000533, 0.7500000000000000000, 0.7524999999999999467, 0.7550000000000000044, 0.7574999999999999512, 0.7600000000000000089, 0.7624999999999999556, 0.7650000000000000133, 0.7674999999999999600, 0.7700000000000000178, 0.7724999999999999645, 0.7750000000000000222, 0.7774999999999999689, 0.7800000000000000266, 0.7824999999999999734, 0.7850000000000000311, 0.7874999999999999778, 0.7900000000000000355, 0.7924999999999999822, 0.7950000000000000400, 0.7974999999999999867, 0.8000000000000000444, 0.8024999999999999911, 0.8050000000000000488, 0.8074999999999999956, 0.8100000000000000533, 0.8125000000000000000, 0.8149999999999999467, 0.8175000000000000044, 0.8199999999999999512, 0.8225000000000000089, 0.8249999999999999556, 0.8275000000000000133, 0.8299999999999999600, 0.8325000000000000178, 0.8349999999999999645, 0.8375000000000000222, 0.8399999999999999689, 0.8425000000000000266, 0.8449999999999999734, 0.8475000000000000311, 0.8499999999999999778, 0.8525000000000000355, 0.8549999999999999822, 0.8575000000000000400, 0.8599999999999999867, 0.8625000000000000444, 0.8649999999999999911, 0.8675000000000000488, 0.8699999999999999956, 0.8725000000000000533, 0.8750000000000000000, 0.8774999999999999467, 0.8800000000000000044, 0.8824999999999999512, 0.8850000000000000089, 0.8874999999999999556, 0.8900000000000000133, 0.8924999999999999600, 0.8950000000000000178, 0.8974999999999999645, 0.9000000000000000222, 0.9024999999999999689, 0.9050000000000000266, 0.9074999999999999734, 0.9100000000000000311, 0.9124999999999999778, 0.9150000000000000355, 0.9174999999999999822, 0.9200000000000000400, 0.9224999999999999867, 0.9250000000000000444, 0.9274999999999999911, 0.9300000000000000488, 0.9324999999999999956, 0.9350000000000000533, 0.9375000000000000000, 0.9399999999999999467, 0.9425000000000000044, 0.9449999999999999512, 0.9475000000000000089, 0.9499999999999999556, 0.9525000000000000133, 0.9549999999999999600, 0.9575000000000000178, 0.9599999999999999645, 0.9625000000000000222, 0.9649999999999999689, 0.9675000000000000266, 0.9699999999999999734, 0.9725000000000000311, 0.9749999999999999778, 0.9775000000000000355, 0.9799999999999999822, 0.9825000000000000400, 0.9849999999999999867, 0.9875000000000000444, 0.9899999999999999911, 0.9925000000000000488, 0.9949999999999999956, 0.9975000000000000533, 1.000000000000000000 ),
 .UNSPECIFIED. ) 
 GEOMETRIC_REPRESENTATION_ITEM ( )  RATIONAL_B_SPLINE_SURFACE ( (
 ( 1.000000000000000000, 0.9238795325112869605, 1.000000000000000000, 0.9238795325112869605, 1.000000000000000000, 0.9238795325112869605, 1.000000000000000000, 0.9238795325112869605, 1.000000000000000000, 0.9238795325112869605, 1.000000000000000000, 0.9238795325112869605, 1.000000000000000000, 0.9238795325112869605, 1.000000000000000000, 0.9238795325112869605, 1.000000000000000000, 0.9238795325112869605, 1.000000000000000000, 0.9238795325112869605, 1.000000000000000000, 0.9238795325112869605, 1.000000000000000000, 0.9238795325112869605, 1.000000000000000000, 0.9238795325112869605, 1.000000000000000000, 0.9238795325112869605, 1.000000000000000000, 0.9238795325112869605, 1.000000000000000000, 0.9238795325112869605, 1.000000000000000000, 0.9238795325112869605, 1.000000000000000000, 0.9238795325112869605, 1.000000000000000000, 0.9238795325112869605, 1.000000000000000000, 0.9238795325112869605, 1.000000000000000000, 0.9238795325112869605, 1.000000000000000000, 0.9238795325112869605, 1.000000000000000000, 0.9238795325112869605, 1.000000000000000000, 0.9238795325112869605, 1.000000000000000000, 0.9238795325112869605, 1.000000000000000000, 0.9238795325112869605, 1.000000000000000000, 0.9238795325112869605, 1.000000000000000000, 0.9238795325112869605, 1.000000000000000000, 0.9238795325112869605, 1.000000000000000000, 0.9238795325112869605, 1.000000000000000000, 0.9238795325112869605, 1.000000000000000000, 0.9238795325112869605, 1.000000000000000000, 0.9238795325112869605, 1.000000000000000000, 0.9238795325112869605, 1.000000000000000000, 0.9238795325112869605, 1.000000000000000000, 0.9238795325112869605, 1.000000000000000000, 0.9238795325112869605, 1.000000000000000000, 0.9238795325112869605, 1.000000000000000000, 0.9238795325112869605, 1.000000000000000000, 0.9238795325112869605, 1.000000000000000000, 0.9238795325112869605, 1.000000000000000000, 0.9238795325112869605, 1.000000000000000000, 0.9238795325112869605, 1.000000000000000000, 0.9238795325112869605, 1.000000000000000000, 0.9238795325112869605, 1.000000000000000000, 0.9238795325112869605, 1.000000000000000000, 0.9238795325112869605, 1.000000000000000000, 0.9238795325112869605, 1.000000000000000000, 0.9238795325112869605, 1.000000000000000000, 0.9238795325112869605, 1.000000000000000000, 0.9238795325112869605, 1.000000000000000000, 0.9238795325112869605, 1.000000000000000000, 0.9238795325112869605, 1.000000000000000000, 0.9238795325112869605, 1.000000000000000000, 0.9238795325112869605, 1.000000000000000000, 0.9238795325112869605, 1.000000000000000000, 0.9238795325112869605, 1.000000000000000000, 0.9238795325112869605, 1.000000000000000000, 0.9238795325112869605, 1.000000000000000000, 0.9238795325112869605, 1.000000000000000000, 0.9238795325112869605, 1.000000000000000000, 0.9238795325112869605, 1.000000000000000000, 0.9238795325112869605, 1.000000000000000000, 0.9238795325112869605, 1.000000000000000000, 0.9238795325112869605, 1.000000000000000000, 0.9238795325112869605, 1.000000000000000000, 0.9238795325112869605, 1.000000000000000000, 0.9238795325112869605, 1.000000000000000000, 0.9238795325112869605, 1.000000000000000000, 0.9238795325112869605, 1.000000000000000000, 0.9238795325112869605, 1.000000000000000000, 0.9238795325112869605, 1.000000000000000000, 0.9238795325112869605, 1.000000000000000000, 0.9238795325112869605, 1.000000000000000000, 0.9238795325112869605, 1.000000000000000000, 0.9238795325112869605, 1.000000000000000000, 0.9238795325112869605, 1.000000000000000000, 0.9238795325112869605, 1.000000000000000000, 0.9238795325112869605, 1.000000000000000000, 0.9238795325112869605, 1.000000000000000000, 0.9238795325112869605, 1.000000000000000000, 0.9238795325112869605, 1.000000000000000000, 0.9238795325112869605, 1.000000000000000000, 0.9238795325112869605, 1.000000000000000000, 0.9238795325112869605, 1.000000000000000000, 0.9238795325112869605, 1.000000000000000000, 0.9238795325112869605, 1.000000000000000000, 0.9238795325112869605, 1.000000000000000000, 0.9238795325112869605, 1.000000000000000000, 0.9238795325112869605, 1.000000000000000000, 0.9238795325112869605, 1.000000000000000000, 0.9238795325112869605, 1.000000000000000000, 0.9238795325112869605, 1.000000000000000000, 0.9238795325112869605, 1.000000000000000000, 0.9238795325112869605, 1.000000000000000000, 0.9238795325112869605, 1.000000000000000000, 0.9238795325112869605, 1.000000000000000000, 0.9238795325112869605, 1.000000000000000000, 0.9238795325112869605, 1.000000000000000000, 0.9238795325112869605, 1.000000000000000000, 0.9238795325112869605, 1.000000000000000000, 0.9238795325112869605, 1.000000000000000000, 0.9238795325112869605, 1.000000000000000000, 0.9238795325112869605, 1.000000000000000000, 0.9238795325112869605, 1.000000000000000000, 0.9238795325112869605, 1.000000000000000000, 0.9238795325112869605, 1.000000000000000000, 0.9238795325112869605, 1.000000000000000000, 0.9238795325112869605, 1.000000000000000000, 0.9238795325112869605, 1.000000000000000000, 0.9238795325112869605, 1.000000000000000000, 0.9238795325112869605, 1.000000000000000000, 0.9238795325112869605, 1.000000000000000000, 0.9238795325112869605, 1.000000000000000000, 0.9238795325112869605, 1.000000000000000000, 0.9238795325112869605, 1.000000000000000000, 0.9238795325112869605, 1.000000000000000000, 0.9238795325112869605, 1.000000000000000000, 0.9238795325112869605, 1.000000000000000000, 0.9238795325112869605, 1.000000000000000000, 0.9238795325112869605, 1.000000000000000000, 0.9238795325112869605, 1.000000000000000000, 0.9238795325112869605, 1.000000000000000000, 0.9238795325112869605, 1.000000000000000000, 0.9238795325112869605, 1.000000000000000000, 0.9238795325112869605, 1.000000000000000000, 0.9238795325112869605, 1.000000000000000000, 0.9238795325112869605, 1.000000000000000000, 0.9238795325112869605, 1.000000000000000000, 0.9238795325112869605, 1.000000000000000000, 0.9238795325112869605, 1.000000000000000000, 0.9238795325112869605, 1.000000000000000000, 0.9238795325112869605, 1.000000000000000000, 0.9238795325112869605, 1.000000000000000000, 0.9238795325112869605, 1.000000000000000000, 0.9238795325112869605, 1.000000000000000000, 0.9238795325112869605, 1.000000000000000000, 0.9238795325112869605, 1.000000000000000000, 0.9238795325112869605, 1.000000000000000000, 0.9238795325112869605, 1.000000000000000000, 0.9238795325112869605, 1.000000000000000000, 0.9238795325112869605, 1.000000000000000000, 0.9238795325112869605, 1.000000000000000000, 0.9238795325112869605, 1.000000000000000000, 0.9238795325112869605, 1.000000000000000000, 0.9238795325112869605, 1.000000000000000000, 0.9238795325112869605, 1.000000000000000000, 0.9238795325112869605, 1.000000000000000000, 0.9238795325112869605, 1.000000000000000000, 0.9238795325112869605, 1.000000000000000000, 0.9238795325112869605, 1.000000000000000000, 0.9238795325112869605, 1.000000000000000000, 0.9238795325112869605, 1.000000000000000000, 0.9238795325112869605, 1.000000000000000000, 0.9238795325112869605, 1.000000000000000000, 0.9238795325112869605, 1.000000000000000000, 0.9238795325112869605, 1.000000000000000000, 0.9238795325112869605, 1.000000000000000000, 0.9238795325112869605, 1.000000000000000000, 0.9238795325112869605, 1.000000000000000000, 0.9238795325112869605, 1.000000000000000000, 0.9238795325112869605, 1.000000000000000000, 0.9238795325112869605, 1.000000000000000000, 0.9238795325112869605, 1.000000000000000000, 0.9238795325112869605, 1.000000000000000000, 0.9238795325112869605, 1.000000000000000000, 0.9238795325112869605, 1.000000000000000000, 0.9238795325112869605, 1.000000000000000000, 0.9238795325112869605, 1.000000000000000000, 0.9238795325112869605, 1.000000000000000000, 0.9238795325112869605, 1.000000000000000000, 0.9238795325112869605, 1.000000000000000000, 0.9238795325112869605, 1.000000000000000000, 0.9238795325112869605, 1.000000000000000000, 0.9238795325112869605, 1.000000000000000000, 0.9238795325112869605, 1.000000000000000000, 0.9238795325112869605, 1.000000000000000000, 0.9238795325112869605, 1.000000000000000000, 0.9238795325112869605, 1.000000000000000000, 0.9238795325112869605, 1.000000000000000000, 0.9238795325112869605, 1.000000000000000000, 0.9238795325112869605, 1.000000000000000000, 0.9238795325112869605, 1.000000000000000000, 0.9238795325112869605, 1.000000000000000000, 0.9238795325112869605, 1.000000000000000000, 0.9238795325112869605, 1.000000000000000000, 0.9238795325112869605, 1.000000000000000000, 0.9238795325112869605, 1.000000000000000000, 0.9238795325112869605, 1.000000000000000000, 0.9238795325112869605, 1.000000000000000000, 0.9238795325112869605, 1.000000000000000000, 0.9238795325112869605, 1.000000000000000000, 0.9238795325112869605, 1.000000000000000000, 0.9238795325112869605, 1.000000000000000000, 0.9238795325112869605, 1.000000000000000000, 0.9238795325112869605, 1.000000000000000000, 0.9238795325112869605, 1.000000000000000000, 0.9238795325112869605, 1.000000000000000000, 0.9238795325112869605, 1.000000000000000000, 0.9238795325112869605, 1.000000000000000000, 0.9238795325112869605, 1.000000000000000000, 0.9238795325112869605, 1.000000000000000000, 0.9238795325112869605, 1.000000000000000000, 0.9238795325112869605, 1.000000000000000000, 0.9238795325112869605, 1.000000000000000000, 0.9238795325112869605, 1.000000000000000000, 0.9238795325112869605, 1.000000000000000000, 0.9238795325112869605, 1.000000000000000000, 0.9238795325112869605, 1.000000000000000000, 0.9238795325112869605, 1.000000000000000000, 0.9238795325112869605, 1.000000000000000000, 0.9238795325112869605, 1.000000000000000000, 0.9238795325112869605, 1.000000000000000000, 0.9238795325112869605, 1.000000000000000000, 0.9238795325112869605, 1.000000000000000000, 0.9238795325112869605, 1.000000000000000000, 0.9238795325112869605, 1.000000000000000000, 0.9238795325112869605, 1.000000000000000000, 0.9238795325112869605, 1.000000000000000000, 0.9238795325112869605, 1.000000000000000000, 0.9238795325112869605, 1.000000000000000000, 0.9238795325112869605, 1.000000000000000000, 0.9238795325112869605, 1.000000000000000000, 0.9238795325112869605, 1.000000000000000000, 0.9238795325112869605, 1.000000000000000000, 0.9238795325112869605, 1.000000000000000000, 0.9238795325112869605, 1.000000000000000000, 0.9238795325112869605, 1.000000000000000000, 0.9238795325112869605, 1.000000000000000000, 0.9238795325112869605, 1.000000000000000000, 0.9238795325112869605, 1.000000000000000000, 0.9238795325112869605, 1.000000000000000000, 0.9238795325112869605, 1.000000000000000000, 0.9238795325112869605, 1.000000000000000000, 0.9238795325112869605, 1.000000000000000000, 0.9238795325112869605, 1.000000000000000000, 0.9238795325112869605, 1.000000000000000000, 0.9238795325112869605, 1.000000000000000000, 0.9238795325112869605, 1.000000000000000000, 0.9238795325112869605, 1.000000000000000000, 0.9238795325112869605, 1.000000000000000000, 0.9238795325112869605, 1.000000000000000000, 0.9238795325112869605, 1.000000000000000000, 0.9238795325112869605, 1.000000000000000000, 0.9238795325112869605, 1.000000000000000000, 0.9238795325112869605, 1.000000000000000000, 0.9238795325112869605, 1.000000000000000000, 0.9238795325112869605, 1.000000000000000000, 0.9238795325112869605, 1.000000000000000000, 0.9238795325112869605, 1.000000000000000000, 0.9238795325112869605, 1.000000000000000000, 0.9238795325112869605, 1.000000000000000000, 0.9238795325112869605, 1.000000000000000000, 0.9238795325112869605, 1.000000000000000000, 0.9238795325112869605, 1.000000000000000000, 0.9238795325112869605, 1.000000000000000000, 0.9238795325112869605, 1.000000000000000000, 0.9238795325112869605, 1.000000000000000000, 0.9238795325112869605, 1.000000000000000000, 0.9238795325112869605, 1.000000000000000000, 0.9238795325112869605, 1.000000000000000000, 0.9238795325112869605, 1.000000000000000000, 0.9238795325112869605, 1.000000000000000000, 0.9238795325112869605, 1.000000000000000000, 0.9238795325112869605, 1.000000000000000000, 0.9238795325112869605, 1.000000000000000000, 0.9238795325112869605, 1.000000000000000000, 0.9238795325112869605, 1.000000000000000000, 0.9238795325112869605, 1.000000000000000000, 0.9238795325112869605, 1.000000000000000000, 0.9238795325112869605, 1.000000000000000000, 0.9238795325112869605, 1.000000000000000000, 0.9238795325112869605, 1.000000000000000000, 0.9238795325112869605, 1.000000000000000000, 0.9238795325112869605, 1.000000000000000000, 0.9238795325112869605, 1.000000000000000000, 0.9238795325112869605, 1.000000000000000000, 0.9238795325112869605, 1.000000000000000000, 0.9238795325112869605, 1.000000000000000000, 0.9238795325112869605, 1.000000000000000000, 0.9238795325112869605, 1.000000000000000000, 0.9238795325112869605, 1.000000000000000000, 0.9238795325112869605, 1.000000000000000000, 0.9238795325112869605, 1.000000000000000000, 0.9238795325112869605, 1.000000000000000000, 0.9238795325112869605, 1.000000000000000000, 0.9238795325112869605, 1.000000000000000000, 0.9238795325112869605, 1.000000000000000000, 0.9238795325112869605, 1.000000000000000000, 0.9238795325112869605, 1.000000000000000000, 0.9238795325112869605, 1.000000000000000000, 0.9238795325112869605, 1.000000000000000000, 0.9238795325112869605, 1.000000000000000000, 0.9238795325112869605, 1.000000000000000000, 0.9238795325112869605, 1.000000000000000000, 0.9238795325112869605, 1.000000000000000000, 0.9238795325112869605, 1.000000000000000000, 0.9238795325112869605, 1.000000000000000000, 0.9238795325112869605, 1.000000000000000000, 0.9238795325112869605, 1.000000000000000000, 0.9238795325112869605, 1.000000000000000000, 0.9238795325112869605, 1.000000000000000000, 0.9238795325112869605, 1.000000000000000000, 0.9238795325112869605, 1.000000000000000000, 0.9238795325112869605, 1.000000000000000000, 0.9238795325112869605, 1.000000000000000000, 0.9238795325112869605, 1.000000000000000000, 0.9238795325112869605, 1.000000000000000000, 0.9238795325112869605, 1.000000000000000000, 0.9238795325112869605, 1.000000000000000000, 0.9238795325112869605, 1.000000000000000000, 0.9238795325112869605, 1.000000000000000000, 0.9238795325112869605, 1.000000000000000000, 0.9238795325112869605, 1.000000000000000000, 0.9238795325112869605, 1.000000000000000000, 0.9238795325112869605, 1.000000000000000000, 0.9238795325112869605, 1.000000000000000000, 0.9238795325112869605, 1.000000000000000000, 0.9238795325112869605, 1.000000000000000000, 0.9238795325112869605, 1.000000000000000000, 0.9238795325112869605, 1.000000000000000000, 0.9238795325112869605, 1.000000000000000000, 0.9238795325112869605, 1.000000000000000000, 0.9238795325112869605, 1.000000000000000000, 0.9238795325112869605, 1.000000000000000000, 0.9238795325112869605, 1.000000000000000000, 0.9238795325112869605, 1.000000000000000000, 0.9238795325112869605, 1.000000000000000000, 0.9238795325112869605, 1.000000000000000000, 0.9238795325112869605, 1.000000000000000000, 0.9238795325112869605, 1.000000000000000000, 0.9238795325112869605, 1.000000000000000000, 0.9238795325112869605, 1.000000000000000000, 0.9238795325112869605, 1.000000000000000000, 0.9238795325112869605, 1.000000000000000000, 0.9238795325112869605, 1.000000000000000000, 0.9238795325112869605, 1.000000000000000000, 0.9238795325112869605, 1.000000000000000000, 0.9238795325112869605, 1.000000000000000000, 0.9238795325112869605, 1.000000000000000000, 0.9238795325112869605, 1.000000000000000000, 0.9238795325112869605, 1.000000000000000000, 0.9238795325112869605, 1.000000000000000000, 0.9238795325112869605, 1.000000000000000000, 0.9238795325112869605, 1.000000000000000000, 0.9238795325112869605, 1.000000000000000000, 0.9238795325112869605, 1.000000000000000000, 0.9238795325112869605, 1.000000000000000000, 0.9238795325112869605, 1.000000000000000000, 0.9238795325112869605, 1.000000000000000000, 0.9238795325112869605, 1.000000000000000000, 0.9238795325112869605, 1.000000000000000000, 0.9238795325112869605, 1.000000000000000000, 0.9238795325112869605, 1.000000000000000000, 0.9238795325112869605, 1.000000000000000000, 0.9238795325112869605, 1.000000000000000000, 0.9238795325112869605, 1.000000000000000000, 0.9238795325112869605, 1.000000000000000000, 0.9238795325112869605, 1.000000000000000000, 0.9238795325112869605, 1.000000000000000000, 0.9238795325112869605, 1.000000000000000000, 0.9238795325112869605, 1.000000000000000000, 0.9238795325112869605, 1.000000000000000000, 0.9238795325112869605, 1.000000000000000000, 0.9238795325112869605, 1.000000000000000000, 0.9238795325112869605, 1.000000000000000000, 0.9238795325112869605, 1.000000000000000000, 0.9238795325112869605, 1.000000000000000000, 0.9238795325112869605, 1.000000000000000000, 0.9238795325112869605, 1.000000000000000000, 0.9238795325112869605, 1.000000000000000000, 0.9238795325112869605, 1.000000000000000000, 0.9238795325112869605, 1.000000000000000000, 0.9238795325112869605, 1.000000000000000000, 0.9238795325112869605, 1.000000000000000000, 0.9238795325112869605, 1.000000000000000000, 0.9238795325112869605, 1.000000000000000000, 0.9238795325112869605, 1.000000000000000000, 0.9238795325112869605, 1.000000000000000000, 0.9238795325112869605, 1.000000000000000000, 0.9238795325112869605, 1.000000000000000000, 0.9238795325112869605, 1.000000000000000000, 0.9238795325112869605, 1.000000000000000000, 0.9238795325112869605, 1.000000000000000000, 0.9238795325112869605, 1.000000000000000000, 0.9238795325112869605, 1.000000000000000000, 0.9238795325112869605, 1.000000000000000000, 0.9238795325112869605, 1.000000000000000000, 0.9238795325112869605, 1.000000000000000000, 0.9238795325112869605, 1.000000000000000000, 0.9238795325112869605, 1.000000000000000000, 0.9238795325112869605, 1.000000000000000000, 0.9238795325112869605, 1.000000000000000000, 0.9238795325112869605, 1.000000000000000000, 0.9238795325112869605, 1.000000000000000000, 0.9238795325112869605, 1.000000000000000000, 0.9238795325112869605, 1.000000000000000000, 0.9238795325112869605, 1.000000000000000000, 0.9238795325112869605, 1.000000000000000000, 0.9238795325112869605, 1.000000000000000000),
 ( 1.000000000000000000, 0.9238795325112869605, 1.000000000000000000, 0.9238795325112869605, 1.000000000000000000, 0.9238795325112869605, 1.000000000000000000, 0.9238795325112869605, 1.000000000000000000, 0.9238795325112869605, 1.000000000000000000, 0.9238795325112869605, 1.000000000000000000, 0.9238795325112869605, 1.000000000000000000, 0.9238795325112869605, 1.000000000000000000, 0.9238795325112869605, 1.000000000000000000, 0.9238795325112869605, 1.000000000000000000, 0.9238795325112869605, 1.000000000000000000, 0.9238795325112869605, 1.000000000000000000, 0.9238795325112869605, 1.000000000000000000, 0.9238795325112869605, 1.000000000000000000, 0.9238795325112869605, 1.000000000000000000, 0.9238795325112869605, 1.000000000000000000, 0.9238795325112869605, 1.000000000000000000, 0.9238795325112869605, 1.000000000000000000, 0.9238795325112869605, 1.000000000000000000, 0.9238795325112869605, 1.000000000000000000, 0.9238795325112869605, 1.000000000000000000, 0.9238795325112869605, 1.000000000000000000, 0.9238795325112869605, 1.000000000000000000, 0.9238795325112869605, 1.000000000000000000, 0.9238795325112869605, 1.000000000000000000, 0.9238795325112869605, 1.000000000000000000, 0.9238795325112869605, 1.000000000000000000, 0.9238795325112869605, 1.000000000000000000, 0.9238795325112869605, 1.000000000000000000, 0.9238795325112869605, 1.000000000000000000, 0.9238795325112869605, 1.000000000000000000, 0.9238795325112869605, 1.000000000000000000, 0.9238795325112869605, 1.000000000000000000, 0.9238795325112869605, 1.000000000000000000, 0.9238795325112869605, 1.000000000000000000, 0.9238795325112869605, 1.000000000000000000, 0.9238795325112869605, 1.000000000000000000, 0.9238795325112869605, 1.000000000000000000, 0.9238795325112869605, 1.000000000000000000, 0.9238795325112869605, 1.000000000000000000, 0.9238795325112869605, 1.000000000000000000, 0.9238795325112869605, 1.000000000000000000, 0.9238795325112869605, 1.000000000000000000, 0.9238795325112869605, 1.000000000000000000, 0.9238795325112869605, 1.000000000000000000, 0.9238795325112869605, 1.000000000000000000, 0.9238795325112869605, 1.000000000000000000, 0.9238795325112869605, 1.000000000000000000, 0.9238795325112869605, 1.000000000000000000, 0.9238795325112869605, 1.000000000000000000, 0.9238795325112869605, 1.000000000000000000, 0.9238795325112869605, 1.000000000000000000, 0.9238795325112869605, 1.000000000000000000, 0.9238795325112869605, 1.000000000000000000, 0.9238795325112869605, 1.000000000000000000, 0.9238795325112869605, 1.000000000000000000, 0.9238795325112869605, 1.000000000000000000, 0.9238795325112869605, 1.000000000000000000, 0.9238795325112869605, 1.000000000000000000, 0.9238795325112869605, 1.000000000000000000, 0.9238795325112869605, 1.000000000000000000, 0.9238795325112869605, 1.000000000000000000, 0.9238795325112869605, 1.000000000000000000, 0.9238795325112869605, 1.000000000000000000, 0.9238795325112869605, 1.000000000000000000, 0.9238795325112869605, 1.000000000000000000, 0.9238795325112869605, 1.000000000000000000, 0.9238795325112869605, 1.000000000000000000, 0.9238795325112869605, 1.000000000000000000, 0.9238795325112869605, 1.000000000000000000, 0.9238795325112869605, 1.000000000000000000, 0.9238795325112869605, 1.000000000000000000, 0.9238795325112869605, 1.000000000000000000, 0.9238795325112869605, 1.000000000000000000, 0.9238795325112869605, 1.000000000000000000, 0.9238795325112869605, 1.000000000000000000, 0.9238795325112869605, 1.000000000000000000, 0.9238795325112869605, 1.000000000000000000, 0.9238795325112869605, 1.000000000000000000, 0.9238795325112869605, 1.000000000000000000, 0.9238795325112869605, 1.000000000000000000, 0.9238795325112869605, 1.000000000000000000, 0.9238795325112869605, 1.000000000000000000, 0.9238795325112869605, 1.000000000000000000, 0.9238795325112869605, 1.000000000000000000, 0.9238795325112869605, 1.000000000000000000, 0.9238795325112869605, 1.000000000000000000, 0.9238795325112869605, 1.000000000000000000, 0.9238795325112869605, 1.000000000000000000, 0.9238795325112869605, 1.000000000000000000, 0.9238795325112869605, 1.000000000000000000, 0.9238795325112869605, 1.000000000000000000, 0.9238795325112869605, 1.000000000000000000, 0.9238795325112869605, 1.000000000000000000, 0.9238795325112869605, 1.000000000000000000, 0.9238795325112869605, 1.000000000000000000, 0.9238795325112869605, 1.000000000000000000, 0.9238795325112869605, 1.000000000000000000, 0.9238795325112869605, 1.000000000000000000, 0.9238795325112869605, 1.000000000000000000, 0.9238795325112869605, 1.000000000000000000, 0.9238795325112869605, 1.000000000000000000, 0.9238795325112869605, 1.000000000000000000, 0.9238795325112869605, 1.000000000000000000, 0.9238795325112869605, 1.000000000000000000, 0.9238795325112869605, 1.000000000000000000, 0.9238795325112869605, 1.000000000000000000, 0.9238795325112869605, 1.000000000000000000, 0.9238795325112869605, 1.000000000000000000, 0.9238795325112869605, 1.000000000000000000, 0.9238795325112869605, 1.000000000000000000, 0.9238795325112869605, 1.000000000000000000, 0.9238795325112869605, 1.000000000000000000, 0.9238795325112869605, 1.000000000000000000, 0.9238795325112869605, 1.000000000000000000, 0.9238795325112869605, 1.000000000000000000, 0.9238795325112869605, 1.000000000000000000, 0.9238795325112869605, 1.000000000000000000, 0.9238795325112869605, 1.000000000000000000, 0.9238795325112869605, 1.000000000000000000, 0.9238795325112869605, 1.000000000000000000, 0.9238795325112869605, 1.000000000000000000, 0.9238795325112869605, 1.000000000000000000, 0.9238795325112869605, 1.000000000000000000, 0.9238795325112869605, 1.000000000000000000, 0.9238795325112869605, 1.000000000000000000, 0.9238795325112869605, 1.000000000000000000, 0.9238795325112869605, 1.000000000000000000, 0.9238795325112869605, 1.000000000000000000, 0.9238795325112869605, 1.000000000000000000, 0.9238795325112869605, 1.000000000000000000, 0.9238795325112869605, 1.000000000000000000, 0.9238795325112869605, 1.000000000000000000, 0.9238795325112869605, 1.000000000000000000, 0.9238795325112869605, 1.000000000000000000, 0.9238795325112869605, 1.000000000000000000, 0.9238795325112869605, 1.000000000000000000, 0.9238795325112869605, 1.000000000000000000, 0.9238795325112869605, 1.000000000000000000, 0.9238795325112869605, 1.000000000000000000, 0.9238795325112869605, 1.000000000000000000, 0.9238795325112869605, 1.000000000000000000, 0.9238795325112869605, 1.000000000000000000, 0.9238795325112869605, 1.000000000000000000, 0.9238795325112869605, 1.000000000000000000, 0.9238795325112869605, 1.000000000000000000, 0.9238795325112869605, 1.000000000000000000, 0.9238795325112869605, 1.000000000000000000, 0.9238795325112869605, 1.000000000000000000, 0.9238795325112869605, 1.000000000000000000, 0.9238795325112869605, 1.000000000000000000, 0.9238795325112869605, 1.000000000000000000, 0.9238795325112869605, 1.000000000000000000, 0.9238795325112869605, 1.000000000000000000, 0.9238795325112869605, 1.000000000000000000, 0.9238795325112869605, 1.000000000000000000, 0.9238795325112869605, 1.000000000000000000, 0.9238795325112869605, 1.000000000000000000, 0.9238795325112869605, 1.000000000000000000, 0.9238795325112869605, 1.000000000000000000, 0.9238795325112869605, 1.000000000000000000, 0.9238795325112869605, 1.000000000000000000, 0.9238795325112869605, 1.000000000000000000, 0.9238795325112869605, 1.000000000000000000, 0.9238795325112869605, 1.000000000000000000, 0.9238795325112869605, 1.000000000000000000, 0.9238795325112869605, 1.000000000000000000, 0.9238795325112869605, 1.000000000000000000, 0.9238795325112869605, 1.000000000000000000, 0.9238795325112869605, 1.000000000000000000, 0.9238795325112869605, 1.000000000000000000, 0.9238795325112869605, 1.000000000000000000, 0.9238795325112869605, 1.000000000000000000, 0.9238795325112869605, 1.000000000000000000, 0.9238795325112869605, 1.000000000000000000, 0.9238795325112869605, 1.000000000000000000, 0.9238795325112869605, 1.000000000000000000, 0.9238795325112869605, 1.000000000000000000, 0.9238795325112869605, 1.000000000000000000, 0.9238795325112869605, 1.000000000000000000, 0.9238795325112869605, 1.000000000000000000, 0.9238795325112869605, 1.000000000000000000, 0.9238795325112869605, 1.000000000000000000, 0.9238795325112869605, 1.000000000000000000, 0.9238795325112869605, 1.000000000000000000, 0.9238795325112869605, 1.000000000000000000, 0.9238795325112869605, 1.000000000000000000, 0.9238795325112869605, 1.000000000000000000, 0.9238795325112869605, 1.000000000000000000, 0.9238795325112869605, 1.000000000000000000, 0.9238795325112869605, 1.000000000000000000, 0.9238795325112869605, 1.000000000000000000, 0.9238795325112869605, 1.000000000000000000, 0.9238795325112869605, 1.000000000000000000, 0.9238795325112869605, 1.000000000000000000, 0.9238795325112869605, 1.000000000000000000, 0.9238795325112869605, 1.000000000000000000, 0.9238795325112869605, 1.000000000000000000, 0.9238795325112869605, 1.000000000000000000, 0.9238795325112869605, 1.000000000000000000, 0.9238795325112869605, 1.000000000000000000, 0.9238795325112869605, 1.000000000000000000, 0.9238795325112869605, 1.000000000000000000, 0.9238795325112869605, 1.000000000000000000, 0.9238795325112869605, 1.000000000000000000, 0.9238795325112869605, 1.000000000000000000, 0.9238795325112869605, 1.000000000000000000, 0.9238795325112869605, 1.000000000000000000, 0.9238795325112869605, 1.000000000000000000, 0.9238795325112869605, 1.000000000000000000, 0.9238795325112869605, 1.000000000000000000, 0.9238795325112869605, 1.000000000000000000, 0.9238795325112869605, 1.000000000000000000, 0.9238795325112869605, 1.000000000000000000, 0.9238795325112869605, 1.000000000000000000, 0.9238795325112869605, 1.000000000000000000, 0.9238795325112869605, 1.000000000000000000, 0.9238795325112869605, 1.000000000000000000, 0.9238795325112869605, 1.000000000000000000, 0.9238795325112869605, 1.000000000000000000, 0.9238795325112869605, 1.000000000000000000, 0.9238795325112869605, 1.000000000000000000, 0.9238795325112869605, 1.000000000000000000, 0.9238795325112869605, 1.000000000000000000, 0.9238795325112869605, 1.000000000000000000, 0.9238795325112869605, 1.000000000000000000, 0.9238795325112869605, 1.000000000000000000, 0.9238795325112869605, 1.000000000000000000, 0.9238795325112869605, 1.000000000000000000, 0.9238795325112869605, 1.000000000000000000, 0.9238795325112869605, 1.000000000000000000, 0.9238795325112869605, 1.000000000000000000, 0.9238795325112869605, 1.000000000000000000, 0.9238795325112869605, 1.000000000000000000, 0.9238795325112869605, 1.000000000000000000, 0.9238795325112869605, 1.000000000000000000, 0.9238795325112869605, 1.000000000000000000, 0.9238795325112869605, 1.000000000000000000, 0.9238795325112869605, 1.000000000000000000, 0.9238795325112869605, 1.000000000000000000, 0.9238795325112869605, 1.000000000000000000, 0.9238795325112869605, 1.000000000000000000, 0.9238795325112869605, 1.000000000000000000, 0.9238795325112869605, 1.000000000000000000, 0.9238795325112869605, 1.000000000000000000, 0.9238795325112869605, 1.000000000000000000, 0.9238795325112869605, 1.000000000000000000, 0.9238795325112869605, 1.000000000000000000, 0.9238795325112869605, 1.000000000000000000, 0.9238795325112869605, 1.000000000000000000, 0.9238795325112869605, 1.000000000000000000, 0.9238795325112869605, 1.000000000000000000, 0.9238795325112869605, 1.000000000000000000, 0.9238795325112869605, 1.000000000000000000, 0.9238795325112869605, 1.000000000000000000, 0.9238795325112869605, 1.000000000000000000, 0.9238795325112869605, 1.000000000000000000, 0.9238795325112869605, 1.000000000000000000, 0.9238795325112869605, 1.000000000000000000, 0.9238795325112869605, 1.000000000000000000, 0.9238795325112869605, 1.000000000000000000, 0.9238795325112869605, 1.000000000000000000, 0.9238795325112869605, 1.000000000000000000, 0.9238795325112869605, 1.000000000000000000, 0.9238795325112869605, 1.000000000000000000, 0.9238795325112869605, 1.000000000000000000, 0.9238795325112869605, 1.000000000000000000, 0.9238795325112869605, 1.000000000000000000, 0.9238795325112869605, 1.000000000000000000, 0.9238795325112869605, 1.000000000000000000, 0.9238795325112869605, 1.000000000000000000, 0.9238795325112869605, 1.000000000000000000, 0.9238795325112869605, 1.000000000000000000, 0.9238795325112869605, 1.000000000000000000, 0.9238795325112869605, 1.000000000000000000, 0.9238795325112869605, 1.000000000000000000, 0.9238795325112869605, 1.000000000000000000, 0.9238795325112869605, 1.000000000000000000, 0.9238795325112869605, 1.000000000000000000, 0.9238795325112869605, 1.000000000000000000, 0.9238795325112869605, 1.000000000000000000, 0.9238795325112869605, 1.000000000000000000, 0.9238795325112869605, 1.000000000000000000, 0.9238795325112869605, 1.000000000000000000, 0.9238795325112869605, 1.000000000000000000, 0.9238795325112869605, 1.000000000000000000, 0.9238795325112869605, 1.000000000000000000, 0.9238795325112869605, 1.000000000000000000, 0.9238795325112869605, 1.000000000000000000, 0.9238795325112869605, 1.000000000000000000, 0.9238795325112869605, 1.000000000000000000, 0.9238795325112869605, 1.000000000000000000, 0.9238795325112869605, 1.000000000000000000, 0.9238795325112869605, 1.000000000000000000, 0.9238795325112869605, 1.000000000000000000, 0.9238795325112869605, 1.000000000000000000, 0.9238795325112869605, 1.000000000000000000, 0.9238795325112869605, 1.000000000000000000, 0.9238795325112869605, 1.000000000000000000, 0.9238795325112869605, 1.000000000000000000, 0.9238795325112869605, 1.000000000000000000, 0.9238795325112869605, 1.000000000000000000, 0.9238795325112869605, 1.000000000000000000, 0.9238795325112869605, 1.000000000000000000, 0.9238795325112869605, 1.000000000000000000, 0.9238795325112869605, 1.000000000000000000, 0.9238795325112869605, 1.000000000000000000, 0.9238795325112869605, 1.000000000000000000, 0.9238795325112869605, 1.000000000000000000, 0.9238795325112869605, 1.000000000000000000, 0.9238795325112869605, 1.000000000000000000, 0.9238795325112869605, 1.000000000000000000, 0.9238795325112869605, 1.000000000000000000, 0.9238795325112869605, 1.000000000000000000, 0.9238795325112869605, 1.000000000000000000, 0.9238795325112869605, 1.000000000000000000, 0.9238795325112869605, 1.000000000000000000, 0.9238795325112869605, 1.000000000000000000, 0.9238795325112869605, 1.000000000000000000, 0.9238795325112869605, 1.000000000000000000, 0.9238795325112869605, 1.000000000000000000, 0.9238795325112869605, 1.000000000000000000, 0.9238795325112869605, 1.000000000000000000, 0.9238795325112869605, 1.000000000000000000, 0.9238795325112869605, 1.000000000000000000, 0.9238795325112869605, 1.000000000000000000, 0.9238795325112869605, 1.000000000000000000, 0.9238795325112869605, 1.000000000000000000, 0.9238795325112869605, 1.000000000000000000, 0.9238795325112869605, 1.000000000000000000, 0.9238795325112869605, 1.000000000000000000, 0.9238795325112869605, 1.000000000000000000, 0.9238795325112869605, 1.000000000000000000, 0.9238795325112869605, 1.000000000000000000, 0.9238795325112869605, 1.000000000000000000, 0.9238795325112869605, 1.000000000000000000, 0.9238795325112869605, 1.000000000000000000, 0.9238795325112869605, 1.000000000000000000, 0.9238795325112869605, 1.000000000000000000, 0.9238795325112869605, 1.000000000000000000, 0.9238795325112869605, 1.000000000000000000, 0.9238795325112869605, 1.000000000000000000, 0.9238795325112869605, 1.000000000000000000, 0.9238795325112869605, 1.000000000000000000, 0.9238795325112869605, 1.000000000000000000, 0.9238795325112869605, 1.000000000000000000, 0.9238795325112869605, 1.000000000000000000, 0.9238795325112869605, 1.000000000000000000, 0.9238795325112869605, 1.000000000000000000, 0.9238795325112869605, 1.000000000000000000, 0.9238795325112869605, 1.000000000000000000, 0.9238795325112869605, 1.000000000000000000, 0.9238795325112869605, 1.000000000000000000, 0.9238795325112869605, 1.000000000000000000, 0.9238795325112869605, 1.000000000000000000, 0.9238795325112869605, 1.000000000000000000, 0.9238795325112869605, 1.000000000000000000, 0.9238795325112869605, 1.000000000000000000, 0.9238795325112869605, 1.000000000000000000, 0.9238795325112869605, 1.000000000000000000, 0.9238795325112869605, 1.000000000000000000, 0.9238795325112869605, 1.000000000000000000, 0.9238795325112869605, 1.000000000000000000, 0.9238795325112869605, 1.000000000000000000, 0.9238795325112869605, 1.000000000000000000, 0.9238795325112869605, 1.000000000000000000, 0.9238795325112869605, 1.000000000000000000, 0.9238795325112869605, 1.000000000000000000, 0.9238795325112869605, 1.000000000000000000, 0.9238795325112869605, 1.000000000000000000, 0.9238795325112869605, 1.000000000000000000, 0.9238795325112869605, 1.000000000000000000, 0.9238795325112869605, 1.000000000000000000, 0.9238795325112869605, 1.000000000000000000, 0.9238795325112869605, 1.000000000000000000, 0.9238795325112869605, 1.000000000000000000, 0.9238795325112869605, 1.000000000000000000, 0.9238795325112869605, 1.000000000000000000, 0.9238795325112869605, 1.000000000000000000, 0.9238795325112869605, 1.000000000000000000, 0.9238795325112869605, 1.000000000000000000, 0.9238795325112869605, 1.000000000000000000, 0.9238795325112869605, 1.000000000000000000, 0.9238795325112869605, 1.000000000000000000, 0.9238795325112869605, 1.000000000000000000, 0.9238795325112869605, 1.000000000000000000, 0.9238795325112869605, 1.000000000000000000, 0.9238795325112869605, 1.000000000000000000, 0.9238795325112869605, 1.000000000000000000, 0.9238795325112869605, 1.000000000000000000, 0.9238795325112869605, 1.000000000000000000, 0.9238795325112869605, 1.000000000000000000, 0.9238795325112869605, 1.000000000000000000, 0.9238795325112869605, 1.000000000000000000, 0.9238795325112869605, 1.000000000000000000, 0.9238795325112869605, 1.000000000000000000, 0.9238795325112869605, 1.000000000000000000, 0.9238795325112869605, 1.000000000000000000, 0.9238795325112869605, 1.000000000000000000, 0.9238795325112869605, 1.000000000000000000) ) ) 
 REPRESENTATION_ITEM ( '' )  SURFACE ( )  ) ;
#34255 = CARTESIAN_POINT ( 'NONE',  ( 0.7646288533564489232, -0.1113553986120547346, 0.5757874014672763607 ) ) ;
#34256 = CARTESIAN_POINT ( 'NONE',  ( -0.1377952755905509363, 0.000000000000000000, -0.1045766232635885612 ) ) ;
#34257 = B_SPLINE_CURVE_WITH_KNOTS ( 'NONE', 3,
 ( #18761, #29839, #11359, #44382, #11593, #26217, #8208, #10897, #22600, #43932, #4359, #40088, #23554, #20176, #5565, #26690, #4845, #45334, #15670, #41959, #12779, #8930, #30996, #41242, #13009, #27415, #9166, #45559, #27173, #1728, #31226, #38395, #24028, #19709, #5087, #34350, #9410, #37692 ),
 .UNSPECIFIED., .F., .F.,
 ( 4, 2, 2, 2, 2, 2, 2, 2, 2, 2, 2, 2, 2, 2, 2, 2, 2, 2, 4 ),
 ( 0.000000000000000000, 0.0008476847199669325589, 0.001695369439933865118, 0.002543054159900797785, 0.003390738879867730236, 0.004238423599834662686, 0.005086108319801595570, 0.005933793039768528454, 0.006781477759735462206, 0.007205320119718934720, 0.007629162479702406366, 0.008476847199669360067, 0.009324531919636313768, 0.01017221663960326747, 0.01101990135957022117, 0.01186758607953717487, 0.01229142843952065259, 0.01271527079950412857, 0.01356295551947108401 ),
 .UNSPECIFIED. ) ;
#34258 = CARTESIAN_POINT ( 'NONE',  ( -0.1563239858028344920, -0.08956157449492478662, 0.05512560382421622523 ) ) ;
#34259 = CARTESIAN_POINT ( 'NONE',  ( -1.094772975963752103E-17, -0.4827755904974173617, -0.1787899950787401882 ) ) ;
#34260 = ORIENTED_EDGE ( 'NONE', *, *, #26036, .F. ) ;
#34261 = CARTESIAN_POINT ( 'NONE',  ( -0.2066929133858267931, -0.4410959923581754816, -0.9673892061308019263 ) ) ;
#34262 = CARTESIAN_POINT ( 'NONE',  ( 0.7646288533564489232, -0.1113553986120547346, 0.8612204724409449064 ) ) ;
#34263 = EDGE_CURVE ( 'NONE', #12053, #8209, #3988, .T. ) ;
#34264 = ORIENTED_EDGE ( 'NONE', *, *, #623, .F. ) ;
#34265 = CARTESIAN_POINT ( 'NONE',  ( 0.3161444924769535869, 1.205832402325950792, -1.129708666049259902 ) ) ;
#34266 = CARTESIAN_POINT ( 'NONE',  ( -0.8107537697050254399, 0.1574803149606300301, 0.4453740156405042727 ) ) ;
#34267 = CARTESIAN_POINT ( 'NONE',  ( -1.094772975963752103E-17, -1.663877952702141672, -0.1787899950787401882 ) ) ;
#34268 = CARTESIAN_POINT ( 'NONE',  ( 0.1264236179284866091, -0.9355314960092283583, 0.1264236179284866091 ) ) ;
#34269 = CARTESIAN_POINT ( 'NONE',  ( 0.1113553986120547346, -1.272637795275590511, 0.1113553986120547346 ) ) ;
#34270 = CARTESIAN_POINT ( 'NONE',  ( 0.8107537697050253289, -0.1574803149606297803, 1.050688976270426567 ) ) ;
#34271 = ADVANCED_FACE ( 'NONE', ( #9319, #26599 ), #41872, .F. ) ;
#34272 = DIRECTION ( 'NONE',  ( 0.000000000000000000, -1.000000000000000000, 0.000000000000000000 ) ) ;
#34273 = CARTESIAN_POINT ( 'NONE',  ( -0.7495606340400177148, 0.1264236179284866091, 0.4699803149068661479 ) ) ;
#34274 = ORIENTED_EDGE ( 'NONE', *, *, #8162, .T. ) ;
#34275 = EDGE_LOOP ( 'NONE', ( #10301, #33245, #42749, #14596 ) ) ;
#34276 = CARTESIAN_POINT ( 'NONE',  ( -0.9500414927467378812, 0.1787899950787401604, 1.687992125930489307 ) ) ;
#34277 = ORIENTED_EDGE ( 'NONE', *, *, #28957, .F. ) ;
#34278 = EDGE_CURVE ( 'NONE', #44204, #33479, #20328, .T. ) ;
#34279 = CARTESIAN_POINT ( 'NONE',  ( 1.002407869896990045, -0.1264236179284866091, 1.833169291284818758 ) ) ;
#34280 = ORIENTED_EDGE ( 'NONE', *, *, #8325, .T. ) ;
#34281 = CARTESIAN_POINT ( 'NONE',  ( -0.6971942568897626646, -0.07405724077823297447, 0.9153543306548987957 ) ) ;
#34282 = CARTESIAN_POINT ( 'NONE',  ( 1.033464566929133799, 0.000000000000000000, 0.5610236220472440971 ) ) ;
#34283 = CARTESIAN_POINT ( 'NONE',  ( 1.054774247047244540, 0.07405724077823318263, 0.4232283464029293896 ) ) ;
#34284 = CARTESIAN_POINT ( 'NONE',  ( -0.6971942568897648851, 0.07405724077823318263, 1.377952755851748146 ) ) ;
#34285 = ADVANCED_FACE ( 'NONE', ( #16282, #45711, #37841 ), #45954, .T. ) ;
#34286 = CARTESIAN_POINT ( 'NONE',  ( 0.03734157890109738448, 0.2739282660277746473, -0.3031249188863235355 ) ) ;
#34287 = CARTESIAN_POINT ( 'NONE',  ( -1.054774247047244540, -0.07405724077823318263, 1.397637795221827517 ) ) ;
#34288 = AXIS2_PLACEMENT_3D ( 'NONE', #33216, #43242, #340 ) ;
#34289 = CARTESIAN_POINT ( 'NONE',  ( -1.054774247047244540, -0.07405724077823318263, 0.1427165353793072855 ) ) ;
#34290 = ( BOUNDED_CURVE ( )  B_SPLINE_CURVE ( 2, ( #44601, #34108, #29607, #12289, #18748, #26205, #11349, #33640, #15414 ),
 .UNSPECIFIED., .F., .T. ) 
 B_SPLINE_CURVE_WITH_KNOTS ( ( 3, 2, 2, 2, 3 ),
 ( 0.6800000000000000488, 0.6824999999999999956, 0.6850000000000000533, 0.6875000000000000000, 0.6899999999999999467 ),
 .UNSPECIFIED. ) 
 CURVE ( )  GEOMETRIC_REPRESENTATION_ITEM ( )  RATIONAL_B_SPLINE_CURVE ( ( 1.000000000000000000, 0.9238795325112869605, 1.000000000000000000, 0.9238795325112869605, 1.000000000000000000, 0.9238795325112869605, 1.000000000000000000, 0.9238795325112829637, 1.000000000000000000 ) ) 
 REPRESENTATION_ITEM ( '' )  ) ;
#34291 = DIRECTION ( 'NONE',  ( -1.000000000000000000, -0.000000000000000000, -0.000000000000000000 ) ) ;
#34292 = CARTESIAN_POINT ( 'NONE',  ( -0.7495606340400177148, -0.1264236179284866091, 1.705216535379307174 ) ) ;
#34293 = CARTESIAN_POINT ( 'NONE',  ( -0.8759842519685039353, -0.1787899950787401882, 0.09596456687537047170 ) ) ;
#34294 = CARTESIAN_POINT ( 'NONE',  ( -0.9873396505805591694, 0.1113553986120547346, 1.825787401574803237 ) ) ;
#34295 = CARTESIAN_POINT ( 'NONE',  ( 0.03901279071809810040, 0.3740157480314960647, 1.713085361781127913 ) ) ;
#34296 = CARTESIAN_POINT ( 'NONE',  ( 1.002407869896990045, 0.1264236179284866091, 1.567421259788755794 ) ) ;
#34297 = CARTESIAN_POINT ( 'NONE',  ( -0.2190824202996543291, -0.09842519685039370636, 0.09088772691789900882 ) ) ;
#34298 = CARTESIAN_POINT ( 'NONE',  ( 0.8759842519685039353, 0.000000000000000000, 0.03937007874015747977 ) ) ;
#34299 = EDGE_LOOP ( 'NONE', ( #33102, #38079, #32088, #9385 ) ) ;
#34300 = ORIENTED_EDGE ( 'NONE', *, *, #20175, .F. ) ;
#34301 = CARTESIAN_POINT ( 'NONE',  ( -0.1787899950787401604, -0.9527559054580476694, -0.07405724077823318263 ) ) ;
#34302 = CARTESIAN_POINT ( 'NONE',  ( 0.1787899950787401604, -1.006889763725763220, 0.07405724077823318263 ) ) ;
#34303 = AXIS2_PLACEMENT_3D ( 'NONE', #34366, #34851, #1996 ) ;
#34304 = DIRECTION ( 'NONE',  ( -1.000000000000000000, 0.000000000000000000, 0.000000000000000000 ) ) ;
#34305 = CARTESIAN_POINT ( 'NONE',  ( 0.8019270111902717657, 0.1787899950787401604, 1.845472440891119392 ) ) ;
#34306 = CARTESIAN_POINT ( 'NONE',  ( 0.1797182628040039087, -0.4119532584019430788, -0.07444174185955065859 ) ) ;
#34307 = CARTESIAN_POINT ( 'NONE',  ( 0.06523048226347956391, -1.816437007766488421, 0.1574803149606297803 ) ) ;
#34308 = CARTESIAN_POINT ( 'NONE',  ( -0.06523048226347956391, 0.09793307086614169710, 0.1574803149606297803 ) ) ;
#34309 = CARTESIAN_POINT ( 'NONE',  ( 1.054774247047244096, 0.000000000000000000, 0.8489173227808819444 ) ) ;
#34310 = VECTOR ( 'NONE', #43669, 39.37007874015748143 ) ;
#34312 = CARTESIAN_POINT ( 'NONE',  ( 0.1578913225048159952, -0.03378178545795391258, 0.1404269458896959810 ) ) ;
#34311 = ( NAMED_UNIT ( * ) SI_UNIT ( $, .STERADIAN. ) SOLID_ANGLE_UNIT ( ) ) ;
#34313 = DIRECTION ( 'NONE',  ( -1.000000000000000000, 0.000000000000000000, 0.000000000000000000 ) ) ;
#34314 = CARTESIAN_POINT ( 'NONE',  ( 1.002407869896990045, 0.1264236179284866091, 1.961122047190330786 ) ) ;
#34315 = CARTESIAN_POINT ( 'NONE',  ( 0.4028871391076110364, 4.616380251121755931E-17, 0.000000000000000000 ) ) ;
#34316 = CARTESIAN_POINT ( 'NONE',  ( -0.07405724077823318263, -0.4311023621509605386, 0.1787899950787401604 ) ) ;
#34317 = CARTESIAN_POINT ( 'NONE',  ( 1.033464566929133799, 0.000000000000000000, 0.1279527559055118058 ) ) ;
#34318 = CARTESIAN_POINT ( 'NONE',  ( -0.1787899950787401604, -1.218503936954111300, 0.07405724077823318263 ) ) ;
#34319 = EDGE_CURVE ( 'NONE', #41713, #45855, #23695, .T. ) ;
#34320 = DIRECTION ( 'NONE',  ( 0.000000000000000000, -0.9771240687918510970, -0.2126700594528006527 ) ) ;
#34321 = CARTESIAN_POINT ( 'NONE',  ( -0.9500414927467378812, -0.1787899950787401604, 1.747047244040724312 ) ) ;
#34322 = ORIENTED_EDGE ( 'NONE', *, *, #24833, .F. ) ;
#34323 = CARTESIAN_POINT ( 'NONE',  ( -0.9500414927467378812, 0.1787899950787401604, 1.373031496009229135 ) ) ;
#34324 = CARTESIAN_POINT ( 'NONE',  ( 0.1476377952755906220, 0.3743908788525358022, -3.616772362661642592 ) ) ;
#34325 = CARTESIAN_POINT ( 'NONE',  ( 0.6971942568897637749, 2.189545951927499583E-17, 1.345964566875370139 ) ) ;
#34326 = CARTESIAN_POINT ( 'NONE',  ( -0.6971942568897648851, 0.07405724077823318263, 1.141732283410804349 ) ) ;
#34327 = DIRECTION ( 'NONE',  ( 3.074932031758790220E-16, -1.000000000000000000, -7.235709728040729085E-17 ) ) ;
#34328 = ADVANCED_FACE ( 'NONE', ( #9077 ), #5476, .T. ) ;
#34329 = CARTESIAN_POINT ( 'NONE',  ( -0.1281275874986674834, -0.09843444007757132241, -0.1247355789481490590 ) ) ;
#34330 = DIRECTION ( 'NONE',  ( 1.822029033848725028E-16, 0.000000000000000000, 1.000000000000000000 ) ) ;
#34331 = CARTESIAN_POINT ( 'NONE',  ( 0.8759842519685039353, 0.1787899950787401882, 0.5093503936470236138 ) ) ;
#34332 = CARTESIAN_POINT ( 'NONE',  ( -0.9500414927467377701, 0.1787899950787401604, 0.3444881889226146243 ) ) ;
#34333 = ( CONVERSION_BASED_UNIT ( 'INCH', #19040 ) LENGTH_UNIT ( ) NAMED_UNIT ( #13025 ) ) ;
#34334 = CARTESIAN_POINT ( 'NONE',  ( -0.1213179770789060835, -0.08931471071071625523, -0.1315292587780671485 ) ) ;
#34335 = ORIENTED_EDGE ( 'NONE', *, *, #34425, .T. ) ;
#34336 = CARTESIAN_POINT ( 'NONE',  ( -0.8107537697050253289, 0.1574803149606300301, 0.3371062992125987146 ) ) ;
#34337 = CARTESIAN_POINT ( 'NONE',  ( 0.8019270111902716547, -0.1787899950787401604, 1.235236220418678199 ) ) ;
#34338 = CARTESIAN_POINT ( 'NONE',  ( 0.8759842519685039353, 0.1574803149606299191, 1.938976377845228249 ) ) ;
#34339 = CARTESIAN_POINT ( 'NONE',  ( -0.7185039370078739607, 1.928577636452523993E-17, 1.958661417322834719 ) ) ;
#34340 = ORIENTED_EDGE ( 'NONE', *, *, #30395, .T. ) ;
#34341 = DIRECTION ( 'NONE',  ( 1.000000000000000000, -0.000000000000000000, -0.000000000000000000 ) ) ;
#34342 = CARTESIAN_POINT ( 'NONE',  ( -1.054774247047244096, 0.000000000000000000, 1.011318897584031484 ) ) ;
#34343 = AXIS2_PLACEMENT_3D ( 'NONE', #20111, #46211, #34759 ) ;
#34344 = CARTESIAN_POINT ( 'NONE',  ( -0.7185039370078739607, 1.928577636452523993E-17, 1.476377952648377789 ) ) ;
#34345 = CARTESIAN_POINT ( 'NONE',  ( -0.8019270111902717657, 0.1787899950787401604, 0.03444881884387430981 ) ) ;
#34346 = CARTESIAN_POINT ( 'NONE',  ( -1.094772975963752103E-17, -1.522269637520576868, -0.1787899950787401882 ) ) ;
#34347 = ORIENTED_EDGE ( 'NONE', *, *, #3519, .F. ) ;
#34348 = CARTESIAN_POINT ( 'NONE',  ( -0.9873396505805591694, 0.1113553986120547346, 0.1624015746956226358 ) ) ;
#34349 = CARTESIAN_POINT ( 'NONE',  ( -0.1264236179284866091, -0.3892716534895436786, 0.1264236179284866091 ) ) ;
#34350 = CARTESIAN_POINT ( 'NONE',  ( -0.3094378032379022647, -0.02221465895966917917, 1.042200290985264344 ) ) ;
#34351 = CARTESIAN_POINT ( 'NONE',  ( 0.6971942568897648851, 0.07405724077823318263, 1.338582677111590069 ) ) ;
#34352 = CARTESIAN_POINT ( 'NONE',  ( 0.9412147342319837628, 0.1574803149606300301, 1.464074803042079376 ) ) ;
#34353 = DIRECTION ( 'NONE',  ( 0.000000000000000000, 1.000000000000000000, 0.000000000000000000 ) ) ;
#34354 = CARTESIAN_POINT ( 'NONE',  ( 0.6971942568897637749, 2.189545951927499583E-17, 1.616633858213952779 ) ) ;
#34355 = CARTESIAN_POINT ( 'NONE',  ( -0.1787899950787401882, -1.777066929080094670, 0.000000000000000000 ) ) ;
#34356 = ITEM_DEFINED_TRANSFORMATION ( 'NONE', 'NONE', #30894,  #20860 ) ;
#34357 = DIRECTION ( 'NONE',  ( 0.000000000000000000, 0.000000000000000000, -1.000000000000000000 ) ) ;
#34358 = CARTESIAN_POINT ( 'NONE',  ( -1.054774247047244540, 0.07405724077823318263, 0.5807086613635594752 ) ) ;
#34359 = CARTESIAN_POINT ( 'NONE',  ( 0.1574803149606300301, -0.7977362204724408601, 0.06523048226347956391 ) ) ;
#34360 = CARTESIAN_POINT ( 'NONE',  ( 0.1797182628040039087, -1.637346959189346141, 0.07444174185955046430 ) ) ;
#34361 = CARTESIAN_POINT ( 'NONE',  ( 0.8070866141732283561, -0.0009842519685049383633, -0.8559055118110230342 ) ) ;
#34362 = LINE ( 'NONE', #33670, #13134 ) ;
#34363 = CARTESIAN_POINT ( 'NONE',  ( 0.7495606340400177148, 0.1264236179284866091, 1.537893700733637736 ) ) ;
#34364 = CARTESIAN_POINT ( 'NONE',  ( 0.7495606340400177148, 0.1264236179284866091, 1.847933070812378009 ) ) ;
#34365 = FACE_OUTER_BOUND ( 'NONE', #10021, .T. ) ;
#34366 = CARTESIAN_POINT ( 'NONE',  ( -0.5314960629921260393, 0.000000000000000000, 4.842519685039370358 ) ) ;
#34367 = CARTESIAN_POINT ( 'NONE',  ( 0.2343326035694769383, -0.1601959449155855308, -0.2989494884450356049 ) ) ;
#34369 = CARTESIAN_POINT ( 'NONE',  ( 0.1787899950787401604, 0.05610236225848794223, -0.07405724077823318263 ) ) ;
#34368 = CARTESIAN_POINT ( 'NONE',  ( 0.1574803149606299191, -0.8641732282389291697, -1.928577636452523993E-17 ) ) ;
#34370 = AXIS2_PLACEMENT_3D ( 'NONE', #27045, #8320, #16481 ) ;
#34371 = CARTESIAN_POINT ( 'NONE',  ( 0.7495606340400177148, -0.1264236179284866091, 0.4404527558517480901 ) ) ;
#34372 = EDGE_CURVE ( 'NONE', #18734, #9939, #37591, .T. ) ;
#34373 = DIRECTION ( 'NONE',  ( 1.000000000000000000, 0.000000000000000000, -1.822029033848725275E-16 ) ) ;
#34374 = LINE ( 'NONE', #26245, #42638 ) ;
#34375 = CARTESIAN_POINT ( 'NONE',  ( 0.7646288533564489232, 0.1113553986120547346, 0.2214566929133858220 ) ) ;
#34376 = CARTESIAN_POINT ( 'NONE',  ( -0.7495606340400177148, 0.1264236179284866091, 1.296751968450173154 ) ) ;
#34377 = CARTESIAN_POINT ( 'NONE',  ( 1.033464566929133799, 0.000000000000000000, 0.7874015746956221085 ) ) ;
#34378 = ORIENTED_EDGE ( 'NONE', *, *, #41188, .T. ) ;
#34379 = PLANE ( 'NONE',  #2324 ) ;
#34380 = CARTESIAN_POINT ( 'NONE',  ( 1.002407869896990045, 0.1264236179284866091, 1.016240157426551161 ) ) ;
#34381 = ORIENTED_EDGE ( 'NONE', *, *, #32539, .F. ) ;
#34382 = CARTESIAN_POINT ( 'NONE',  ( 0.07405724077823318263, -1.331692913332063855, 0.1787899950787401604 ) ) ;
#34383 = CARTESIAN_POINT ( 'NONE',  ( -0.9873396505805591694, -0.1113553986120547346, 0.5856299211523157133 ) ) ;
#34384 = DIRECTION ( 'NONE',  ( 0.000000000000000000, 0.000000000000000000, 1.000000000000000000 ) ) ;
#34385 = CARTESIAN_POINT ( 'NONE',  ( 0.6971942568897648851, -0.07405724077823297447, 1.697834645615527771 ) ) ;
#34386 = CARTESIAN_POINT ( 'NONE',  ( -0.8107537697050253289, -0.1574803149606297803, 1.296751968503936370 ) ) ;
#34387 = EDGE_CURVE ( 'NONE', #41647, #35449, #35888, .T. ) ;
#34388 = CARTESIAN_POINT ( 'NONE',  ( 0.1711860128073784404, 0.1966586703794935831, -0.3122165016188708231 ) ) ;
#34389 = CARTESIAN_POINT ( 'NONE',  ( 0.8075642843603819676, 0.1651804176431314886, 0.03937007863263043694 ) ) ;
#34390 = CARTESIAN_POINT ( 'NONE',  ( 0.9873396505805591694, 0.1113553986120547346, 1.343503936900346529 ) ) ;
#34391 = ORIENTED_EDGE ( 'NONE', *, *, #28769, .F. ) ;
#34392 = ORIENTED_EDGE ( 'NONE', *, *, #33362, .F. ) ;
#34393 = ( BOUNDED_CURVE ( )  B_SPLINE_CURVE ( 2, ( #7937, #40741, #8165, #8641, #22793, #27134, #37399, #19190, #41684 ),
 .UNSPECIFIED., .F., .T. ) 
 B_SPLINE_CURVE_WITH_KNOTS ( ( 3, 2, 2, 2, 3 ),
 ( 0.7700000000000000178, 0.7724999999999999645, 0.7750000000000000222, 0.7774999999999999689, 0.7800000000000000266 ),
 .UNSPECIFIED. ) 
 CURVE ( )  GEOMETRIC_REPRESENTATION_ITEM ( )  RATIONAL_B_SPLINE_CURVE ( ( 1.000000000000000000, 0.9238795325112899581, 1.000000000000000000, 0.9238795325112869605, 1.000000000000000000, 0.9238795325112869605, 1.000000000000000000, 0.9238795325112869605, 1.000000000000000000 ) ) 
 REPRESENTATION_ITEM ( '' )  ) ;
#34394 = ORIENTED_EDGE ( 'NONE', *, *, #5348, .F. ) ;
#34395 = CARTESIAN_POINT ( 'NONE',  ( 0.8759842519685039353, -0.1787899950787401882, 0.9621062991588346103 ) ) ;
#34396 = CARTESIAN_POINT ( 'NONE',  ( -0.6971942568897648851, 0.07405724077823318263, 1.535433070812378675 ) ) ;
#34397 = CARTESIAN_POINT ( 'NONE',  ( -0.06523048226347956391, 0.02903543317839319890, 0.1574803149606297803 ) ) ;
#34398 = CARTESIAN_POINT ( 'NONE',  ( -0.8019270111902717657, -0.1787899950787401604, 1.471456692859622217 ) ) ;
#34399 = CARTESIAN_POINT ( 'NONE',  ( 0.000000000000000000, -0.09842519685039370636, 0.2471922904502826812 ) ) ;
#34400 = CARTESIAN_POINT ( 'NONE',  ( 0.7185039370078739607, 1.928577636452523993E-17, 0.8858267715460158565 ) ) ;
#34401 = CARTESIAN_POINT ( 'NONE',  ( -0.1787899950787401604, -1.042446802874906986, -0.07405724077823318263 ) ) ;
#34402 = ORIENTED_EDGE ( 'NONE', *, *, #47268, .F. ) ;
#34403 = CARTESIAN_POINT ( 'NONE',  ( -0.07405724077823318263, 0.07086614178604697112, -0.1787899950787401604 ) ) ;
#34404 = VERTEX_POINT ( 'NONE', #42364 ) ;
#34405 = ORIENTED_EDGE ( 'NONE', *, *, #14723, .T. ) ;
#34406 = CARTESIAN_POINT ( 'NONE',  ( -1.033464566929136907, -0.06523048226347749612, 1.414862204616882835 ) ) ;
#34407 = VECTOR ( 'NONE', #3306, 39.37007874015748143 ) ;
#34408 = EDGE_CURVE ( 'NONE', #1638, #10984, #31610, .T. ) ;
#34409 = CARTESIAN_POINT ( 'NONE',  ( 0.9412147342319837628, -0.1574803149606297803, 0.1107283463491657988 ) ) ;
#34410 = AXIS2_PLACEMENT_3D ( 'NONE', #41114, #44479, #22215 ) ;
#34411 = CARTESIAN_POINT ( 'NONE',  ( -0.1787899950787401882, -0.5565944881352126172, 0.000000000000000000 ) ) ;
#34412 = CARTESIAN_POINT ( 'NONE',  ( -0.7495606340400177148, 0.1264236179284866091, 0.1599409448281264023 ) ) ;
#34413 = CARTESIAN_POINT ( 'NONE',  ( -0.7646288533564489232, 0.1113553986120547346, 1.087598425196850460 ) ) ;
#34414 = CARTESIAN_POINT ( 'NONE',  ( -0.3697796008031323245, 0.000000000000000000, 0.3049950039803606128 ) ) ;
#34415 = CARTESIAN_POINT ( 'NONE',  ( -0.1797182628040039087, -1.145220974937376734, -0.07444174185955065859 ) ) ;
#34416 = CARTESIAN_POINT ( 'NONE',  ( -1.033464566929133799, 0.000000000000000000, 1.929133858160188897 ) ) ;
#34417 = CARTESIAN_POINT ( 'NONE',  ( 1.002407869896990045, -0.1264236179284866091, 0.9276574802611967652 ) ) ;
#34418 = FACE_OUTER_BOUND ( 'NONE', #39055, .T. ) ;
#34419 = CARTESIAN_POINT ( 'NONE',  ( 0.9873396505805591694, -0.1113553986120547346, 1.579724409448818978 ) ) ;
#34421 = LINE ( 'NONE', #1567, #33879 ) ;
#34420 = CARTESIAN_POINT ( 'NONE',  ( 0.9412147342319837628, -0.1574803149606297803, 1.419783464566930054 ) ) ;
#34422 = CYLINDRICAL_SURFACE ( 'NONE', #43505, 0.1574803149606299191 ) ;
#34423 = CARTESIAN_POINT ( 'NONE',  ( 0.1787899950787401604, 0.09547244099864542199, 0.07405724077823318263 ) ) ;
#34424 = DIRECTION ( 'NONE',  ( -3.364312195833787750E-15, -1.000000000000000000, 0.000000000000000000 ) ) ;
#34425 = EDGE_CURVE ( 'NONE', #13566, #14779, #10904, .T. ) ;
#34426 = CARTESIAN_POINT ( 'NONE',  ( 0.9500414927467377701, -0.1787899950787401604, 0.9202755904974182499 ) ) ;
#34427 = CARTESIAN_POINT ( 'NONE',  ( 0.7495606340400177148, -0.1264236179284866091, 1.862696850339937038 ) ) ;
#34428 = CARTESIAN_POINT ( 'NONE',  ( 0.9873396505805591694, -0.1113553986120547346, 0.3494094487113705294 ) ) ;
#34429 = ORIENTED_EDGE ( 'NONE', *, *, #10628, .F. ) ;
#34430 = CARTESIAN_POINT ( 'NONE',  ( 0.7185039370078766252, -0.06523048226348168721, 1.242618110128693276 ) ) ;
#34431 = CARTESIAN_POINT ( 'NONE',  ( -0.06523048226347956391, -1.663877952648379788, 0.1574803149606297803 ) ) ;
#34432 = CARTESIAN_POINT ( 'NONE',  ( -1.033464566929133799, 0.000000000000000000, 0.2362204723334177248 ) ) ;
#34433 = LINE ( 'NONE', #19571, #3778 ) ;
#34434 = CARTESIAN_POINT ( 'NONE',  ( 0.9500414927467378812, -0.1787899950787401604, 1.195866141678520345 ) ) ;
#34435 = EDGE_CURVE ( 'NONE', #19285, #34008, #30364, .T. ) ;
#34436 = CARTESIAN_POINT ( 'NONE',  ( 0.09072478486330262659, -0.09340956239926194449, 0.2330530577653585345 ) ) ;
#34438 = TOROIDAL_SURFACE ( 'NONE', #13762, 0.3814023619577306956, 0.009842519685039369942 ) ;
#34437 = CARTESIAN_POINT ( 'NONE',  ( -0.07405724077823318263, 0.1496062992663619862, -0.1787899950787401604 ) ) ;
#34439 = CARTESIAN_POINT ( 'NONE',  ( 1.033464566929133799, 1.928577636452524610E-17, 4.498031496062992574 ) ) ;
#34440 = CARTESIAN_POINT ( 'NONE',  ( -0.6971942568897626646, -0.07405724077823297447, 0.5954724408911187261 ) ) ;
#34441 = DIRECTION ( 'NONE',  ( 0.000000000000000000, 1.000000000000000000, 0.000000000000000000 ) ) ;
#34442 = CARTESIAN_POINT ( 'NONE',  ( 0.07405724077823318263, -1.513779527505292322, -0.1787899950787401604 ) ) ;
#34443 = CARTESIAN_POINT ( 'NONE',  ( -1.002407869896990045, -0.1264236179284866091, 1.828248031442299082 ) ) ;
#34444 = ORIENTED_EDGE ( 'NONE', *, *, #29768, .T. ) ;
#34445 = CARTESIAN_POINT ( 'NONE',  ( -0.6971942568897637749, 2.189545951927499583E-17, 0.9867125983714331028 ) ) ;
#34446 = CARTESIAN_POINT ( 'NONE',  ( -0.6971942568897626646, 0.07405724077823318263, 0.5954724408911187261 ) ) ;
#34447 = VERTEX_POINT ( 'NONE', #27800 ) ;
#34448 = CARTESIAN_POINT ( 'NONE',  ( 0.3727034120734909473, 0.08090551181102362266, 9.908067607274841931E-18 ) ) ;
#34449 = CARTESIAN_POINT ( 'NONE',  ( 0.1512627532823037080, 0.1257768396322719584, -0.06122819718290384294 ) ) ;
#34450 = LINE ( 'NONE', #30186, #22865 ) ;
#34451 = CARTESIAN_POINT ( 'NONE',  ( 0.07405724077823318263, -0.5552420784654592545, 0.1787899950787401604 ) ) ;
#34452 = CARTESIAN_POINT ( 'NONE',  ( 0.1244665901409340580, -0.08956009715716832520, 0.1738892908116259906 ) ) ;
#34453 = CARTESIAN_POINT ( 'NONE',  ( 0.8759842519685039353, 0.000000000000000000, 4.498031496062992574 ) ) ;
#34454 = DIRECTION ( 'NONE',  ( 1.000000000000000000, -0.000000000000000000, -0.000000000000000000 ) ) ;
#34455 = CARTESIAN_POINT ( 'NONE',  ( -0.8019270111902717657, 0.1787899950787401604, 0.4281496062454490659 ) ) ;
#34456 = CARTESIAN_POINT ( 'NONE',  ( 0.1787899950787401604, -1.810163338307978265, 0.07405724077823318263 ) ) ;
#34458 = EDGE_LOOP ( 'NONE', ( #46715, #19271, #39897, #33705 ) ) ;
#34457 = AXIS2_PLACEMENT_3D ( 'NONE', #43070, #29241, #25115 ) ;
#34459 = DIRECTION ( 'NONE',  ( 0.000000000000000000, 1.000000000000000000, 0.000000000000000000 ) ) ;
#34460 = CARTESIAN_POINT ( 'NONE',  ( -1.002407869896990045, -0.1264236179284866091, 1.478838582623401399 ) ) ;
#34461 = CIRCLE ( 'NONE', #37603, 0.09842519685039370636 ) ;
#34462 = CARTESIAN_POINT ( 'NONE',  ( 0.1264236179284866091, -1.447342519631275692, 0.1264236179284866091 ) ) ;
#34463 = DIRECTION ( 'NONE',  ( -1.000000000000000000, 0.000000000000000000, 0.000000000000000000 ) ) ;
#34464 = CARTESIAN_POINT ( 'NONE',  ( 1.033464566929133799, 0.000000000000000000, 1.023622047136567126 ) ) ;
#34465 = DIRECTION ( 'NONE',  ( 0.000000000000000000, 0.000000000000000000, 1.000000000000000000 ) ) ;
#34466 = CARTESIAN_POINT ( 'NONE',  ( 0.7185039370078746268, 0.06523048226347956391, 0.4601377952755902889 ) ) ;
#34467 = CARTESIAN_POINT ( 'NONE',  ( -0.1270800023317771588, -0.7441382977720216729, 0.1270800023317771588 ) ) ;
#34468 = CARTESIAN_POINT ( 'NONE',  ( 1.229559056033039366E-16, -0.3937007874015746034, 0.4921259842519680183 ) ) ;
#34469 = CARTESIAN_POINT ( 'NONE',  ( -0.8107537697050253289, -0.1574803149606297803, 1.208169291231056430 ) ) ;
#34470 = EDGE_CURVE ( 'NONE', #36104, #40667, #39003, .T. ) ;
#34471 = CARTESIAN_POINT ( 'NONE',  ( 1.054774247047244540, 0.07405724077823318263, 0.5807086613635594752 ) ) ;
#34472 = CARTESIAN_POINT ( 'NONE',  ( -0.1113553986120547346, -0.3769685039370078705, 0.1113553986120547346 ) ) ;
#34473 = CARTESIAN_POINT ( 'NONE',  ( -1.033464566929133799, 0.000000000000000000, 1.181102362097196989 ) ) ;
#34474 = ORIENTED_EDGE ( 'NONE', *, *, #15044, .F. ) ;
#34475 = DIRECTION ( 'NONE',  ( 0.000000000000000000, 0.000000000000000000, -1.000000000000000000 ) ) ;
#34476 = CARTESIAN_POINT ( 'NONE',  ( -1.054774247047244096, 0.000000000000000000, 1.129429133804503937 ) ) ;
#34477 = CARTESIAN_POINT ( 'NONE',  ( 0.7646288533564489232, -0.1113553986120547346, 1.176181102362204633 ) ) ;
#34478 = DIRECTION ( 'NONE',  ( -1.000000000000000000, 0.000000000000000000, 0.000000000000000000 ) ) ;
#34479 = CARTESIAN_POINT ( 'NONE',  ( 0.3980944881889773024, 0.2597269656108940894, 0.7480314960629921295 ) ) ;
#34481 = CARTESIAN_POINT ( 'NONE',  ( 0.000000000000000000, 0.000000000000000000, -0.1183602362204724257 ) ) ;
#34480 = LINE ( 'NONE', #23693, #44449 ) ;
#34482 = CARTESIAN_POINT ( 'NONE',  ( -1.033464566929134687, -0.06523048226347956391, 1.267224409448818978 ) ) ;
#34483 = CARTESIAN_POINT ( 'NONE',  ( 0.1602931993194442739, 0.07955613945526338049, 0.1377952755905511861 ) ) ;
#34484 = CARTESIAN_POINT ( 'NONE',  ( 0.1787899950787401882, -0.6107283464029291675, -2.189545951927503898E-17 ) ) ;
#34485 = VERTEX_POINT ( 'NONE', #20792 ) ;
#34486 = CARTESIAN_POINT ( 'NONE',  ( -1.054774247047244540, 0.07405724077823318263, 1.053149606245450176 ) ) ;
#34487 = CARTESIAN_POINT ( 'NONE',  ( -0.7646288533564489232, 0.1113553986120547346, 1.126968503937007871 ) ) ;
#34488 = VERTEX_POINT ( 'NONE', #24635 ) ;
#34489 = EDGE_CURVE ( 'NONE', #24250, #47218, #2571, .T. ) ;
#34490 = CARTESIAN_POINT ( 'NONE',  ( -1.033464566929133799, 0.000000000000000000, 1.771653543199558811 ) ) ;
#34491 = CARTESIAN_POINT ( 'NONE',  ( 0.07405724077823318263, -1.666338582623402953, -0.1787899950787401604 ) ) ;
#34492 = CARTESIAN_POINT ( 'NONE',  ( 0.1787899950787401882, -0.9699803149068660924, -2.189545951927503898E-17 ) ) ;
#34493 = CARTESIAN_POINT ( 'NONE',  ( -0.1113553986120547346, -1.331692913385826849, -0.1113553986120547346 ) ) ;
#34494 = CARTESIAN_POINT ( 'NONE',  ( 1.033464566929133799, 0.000000000000000000, 1.062992125876724314 ) ) ;
#34495 = CARTESIAN_POINT ( 'NONE',  ( 0.2642359194686346169, -0.09842519685039370636, 1.205361022782828805E-17 ) ) ;
#34496 = CONICAL_SURFACE ( 'NONE', #2319, 0.08090551181102362266, 0.9599310885968742602 ) ;
#34497 = ORIENTED_EDGE ( 'NONE', *, *, #41444, .F. ) ;
#34498 = VERTEX_POINT ( 'NONE', #6408 ) ;
#34499 = CARTESIAN_POINT ( 'NONE',  ( -1.054774247047244540, 0.07405724077823318263, 1.761811023568284007 ) ) ;
#34500 = CARTESIAN_POINT ( 'NONE',  ( 0.8019270111902717657, -0.1787899950787401604, 1.786417322780882388 ) ) ;
#34501 = ORIENTED_EDGE ( 'NONE', *, *, #45091, .F. ) ;
#34502 = CARTESIAN_POINT ( 'NONE',  ( 0.7185039370078739607, 1.928577636452523993E-17, 0.5413385826771653919 ) ) ;
#34503 = CARTESIAN_POINT ( 'NONE',  ( 0.7495606340400177148, -0.1264236179284866091, 0.4060039369541102450 ) ) ;
#34504 = VECTOR ( 'NONE', #1393, 39.37007874015748143 ) ;
#34505 = CARTESIAN_POINT ( 'NONE',  ( -1.054774247047244540, -0.07405724077823318263, 1.318897637741511364 ) ) ;
#34506 = FACE_OUTER_BOUND ( 'NONE', #40914, .T. ) ;
#34507 = CIRCLE ( 'NONE', #40593, 0.09842519685039370636 ) ;
#34508 = CARTESIAN_POINT ( 'NONE',  ( -0.8019270111902717657, -0.1787899950787401604, 0.09350393695411057804 ) ) ;
#34509 = LINE ( 'NONE', #23496, #2294 ) ;
#34510 = CARTESIAN_POINT ( 'NONE',  ( -0.6971942568897648851, -0.07405724077823297447, 1.781496062938362934 ) ) ;
#34511 = CARTESIAN_POINT ( 'NONE',  ( -0.8107537697050253289, 0.1574803149606300301, 1.980807086506644943 ) ) ;
#34512 = CARTESIAN_POINT ( 'NONE',  ( 0.9873396505805591694, -0.1113553986120547346, 1.412401574695621997 ) ) ;
#34513 = CARTESIAN_POINT ( 'NONE',  ( -0.7185039370078746268, -0.06523048226347956391, 1.764271653543307838 ) ) ;
#34514 = DIRECTION ( 'NONE',  ( -1.000000000000000000, 0.000000000000000000, 0.000000000000000000 ) ) ;
#34515 = CARTESIAN_POINT ( 'NONE',  ( 0.1947348203212858064, -0.09842519685039370636, -0.06116798660091043310 ) ) ;
#34516 = CARTESIAN_POINT ( 'NONE',  ( 1.033464566929134687, -0.06523048226347956391, 1.021161417215306955 ) ) ;
#34517 = CARTESIAN_POINT ( 'NONE',  ( -1.033464566929134687, 0.06523048226347956391, 1.783956692913386544 ) ) ;
#34518 = EDGE_LOOP ( 'NONE', ( #27714, #29124, #31178, #29812 ) ) ;
#34519 = ADVANCED_FACE ( 'NONE', ( #2805 ), #12437, .F. ) ;
#34520 = CARTESIAN_POINT ( 'NONE',  ( 0.1787899950787401604, -0.9724409448281265966, 0.07405724077823318263 ) ) ;
#34521 = EDGE_CURVE ( 'NONE', #23610, #8711, #5534, .T. ) ;
#34522 = CARTESIAN_POINT ( 'NONE',  ( -0.1787899950787401604, -1.105314960576158301, -0.07405724077823318263 ) ) ;
#34523 = VECTOR ( 'NONE', #3475, 39.37007874015748143 ) ;
#34524 = CARTESIAN_POINT ( 'NONE',  ( -0.8107537697050254399, -0.1574803149606297803, 0.5880905511811019837 ) ) ;
#34525 = CARTESIAN_POINT ( 'NONE',  ( 0.8019270111902717657, -0.1787899950787401604, 0.4035433070328508509 ) ) ;
#34526 = CARTESIAN_POINT ( 'NONE',  ( 0.1797182628040039365, -0.3750438095830456731, -2.200913952912460540E-17 ) ) ;
#34527 = CARTESIAN_POINT ( 'NONE',  ( -0.7185039370078746268, -0.06523048226347956391, 0.8489173227271192834 ) ) ;
#34528 = ADVANCED_FACE ( 'NONE', ( #39417 ), #39648, .T. ) ;
#34529 = CARTESIAN_POINT ( 'NONE',  ( -9.642888182262618425E-18, 0.08070866141732284393, -0.1574803149606299191 ) ) ;
#34530 = PRESENTATION_LAYER_ASSIGNMENT (  '', '', ( #7733 ) ) ;
#34531 = CARTESIAN_POINT ( 'NONE',  ( 1.002407869896990045, -0.1264236179284866091, 0.9227362204186770889 ) ) ;
#34532 = CIRCLE ( 'NONE', #10811, 0.8366141732283465249 ) ;
#34534 = FACE_OUTER_BOUND ( 'NONE', #45717, .T. ) ;
#34533 = CARTESIAN_POINT ( 'NONE',  ( 0.8107537697050254399, 0.1574803149606300301, 0.6126968503937006982 ) ) ;
#34535 = CARTESIAN_POINT ( 'NONE',  ( 1.054774247047244540, -0.07405724077823318263, 1.993110236166711013 ) ) ;
#34536 = VECTOR ( 'NONE', #18560, 39.37007874015748143 ) ;
#34537 = ORIENTED_EDGE ( 'NONE', *, *, #34186, .T. ) ;
#34538 = CARTESIAN_POINT ( 'NONE',  ( 0.7185039370078746268, 0.06523048226347956391, 0.2239173228346459099 ) ) ;
#34539 = CARTESIAN_POINT ( 'NONE',  ( -0.5555748031496061667, 0.1864803149606359678, 0.7480314960629921295 ) ) ;
#34540 = CARTESIAN_POINT ( 'NONE',  ( 0.07405724077823318263, -0.4901574802611972093, -0.1787899950787401604 ) ) ;
#34541 = DIRECTION ( 'NONE',  ( 0.000000000000000000, 0.000000000000000000, -1.000000000000000000 ) ) ;
#34542 = CARTESIAN_POINT ( 'NONE',  ( 0.1264236179284866091, -1.432578740103716664, -0.1264236179284866091 ) ) ;
#34543 = ( BOUNDED_CURVE ( )  B_SPLINE_CURVE ( 2, ( #34015, #19836, #27061, #1615, #34717, #23211, #45217, #22966, #901 ),
 .UNSPECIFIED., .F., .T. ) 
 B_SPLINE_CURVE_WITH_KNOTS ( ( 3, 2, 2, 2, 3 ),
 ( 0.08999999999999999667, 0.09249999999999999889, 0.09500000000000000111, 0.09750000000000000333, 0.1000000000000000056 ),
 .UNSPECIFIED. ) 
 CURVE ( )  GEOMETRIC_REPRESENTATION_ITEM ( )  RATIONAL_B_SPLINE_CURVE ( ( 1.000000000000000000, 0.9238795325112869605, 1.000000000000000000, 0.9238795325112869605, 1.000000000000000000, 0.9238795325112869605, 1.000000000000000000, 0.9238795325112869605, 1.000000000000000000 ) ) 
 REPRESENTATION_ITEM ( '' )  ) ;
#34544 = CARTESIAN_POINT ( 'NONE',  ( -1.054774247047244540, -0.07405724077823318263, 1.712598425143087688 ) ) ;
#34545 = EDGE_LOOP ( 'NONE', ( #4899, #46936, #5803, #1675, #46750, #4478, #27858 ) ) ;
#34546 = CARTESIAN_POINT ( 'NONE',  ( -0.8019270111902717657, 0.1787899950787401604, 1.299212598371432215 ) ) ;
#34547 = CARTESIAN_POINT ( 'NONE',  ( 0.3906197235759846786, -0.09842519685039370636, 0.000000000000000000 ) ) ;
#34548 = CARTESIAN_POINT ( 'NONE',  ( 0.6971942568897648851, -0.07405724077823297447, 1.427165354276944687 ) ) ;
#34549 = CARTESIAN_POINT ( 'NONE',  ( -1.054774247047244540, 0.07405724077823318263, 0.5019685038832442103 ) ) ;
#34550 = CARTESIAN_POINT ( 'NONE',  ( 0.8759842519685039353, 0.1787899950787401882, 0.07627952750529173875 ) ) ;
#34551 = CARTESIAN_POINT ( 'NONE',  ( -0.8019270111902717657, -0.1787899950787401604, 1.230314960576156746 ) ) ;
#34552 = CARTESIAN_POINT ( 'NONE',  ( 0.03929603434986066873, -0.09842483377092413332, -0.1744181471411035411 ) ) ;
#34553 = CARTESIAN_POINT ( 'NONE',  ( -0.9873396505805591694, 0.1113553986120547346, 1.343503936900346529 ) ) ;
#34554 = CARTESIAN_POINT ( 'NONE',  ( 0.7495606340400177148, 0.1264236179284866091, 0.5930118109698583329 ) ) ;
#34555 = CARTESIAN_POINT ( 'NONE',  ( -1.054774247047244096, 0.000000000000000000, 0.4552165353793071745 ) ) ;
#34556 = CARTESIAN_POINT ( 'NONE',  ( -0.6971942568897637749, 2.189545951927499583E-17, 0.8292322834108031282 ) ) ;
#34557 = ( LENGTH_UNIT ( ) NAMED_UNIT ( * ) SI_UNIT ( $, .METRE. ) ) ;
#34558 = AXIS2_PLACEMENT_3D ( 'NONE', #20081, #16504, #23685 ) ;
#34559 = DIRECTION ( 'NONE',  ( 0.6018150231520413840, -0.000000000000000000, -0.7986355100472980473 ) ) ;
#34560 = VERTEX_POINT ( 'NONE', #10454 ) ;
#34561 = LINE ( 'NONE', #20400, #14181 ) ;
#34562 = CARTESIAN_POINT ( 'NONE',  ( -0.9412147342319837628, 0.1574803149606300301, 0.3321850393700786497 ) ) ;
#34563 = CARTESIAN_POINT ( 'NONE',  ( 1.054774247047244540, -0.07405724077823318263, 1.166338582623402731 ) ) ;
#34564 = CARTESIAN_POINT ( 'NONE',  ( -0.09381437428497224618, -0.09851384883702854478, 0.2089447948460571025 ) ) ;
#34565 = CARTESIAN_POINT ( 'NONE',  ( -0.2559055118110236671, -0.04461241169208605278, -0.03567375012348084767 ) ) ;
#34566 = ORIENTED_EDGE ( 'NONE', *, *, #14071, .T. ) ;
#34567 = VECTOR ( 'NONE', #37235, 39.37007874015748143 ) ;
#34568 = CARTESIAN_POINT ( 'NONE',  ( -0.8759842519685039353, -0.1787899950787401882, 0.9621062991588346103 ) ) ;
#34569 = CARTESIAN_POINT ( 'NONE',  ( -0.7495606340400177148, 0.1264236179284866091, 0.1943897637257641919 ) ) ;
#34570 = CARTESIAN_POINT ( 'NONE',  ( 3.284318927891251994E-17, -1.620694834370970616, 0.1787899950787401882 ) ) ;
#34571 = VERTEX_POINT ( 'NONE', #25054 ) ;
#34572 = CARTESIAN_POINT ( 'NONE',  ( -0.1968503937007874127, 0.06245656531175255294, -0.1492449156640650032 ) ) ;
#34573 = CARTESIAN_POINT ( 'NONE',  ( -0.1264236179284866091, -0.5467519684501732646, 0.1264236179284866091 ) ) ;
#34574 = DIRECTION ( 'NONE',  ( -6.938893903907234689E-15, 0.000000000000000000, 1.000000000000000000 ) ) ;
#34575 = CARTESIAN_POINT ( 'NONE',  ( 0.8019270111902717657, -0.1787899950787401604, 1.348425196796630976 ) ) ;
#34576 = EDGE_CURVE ( 'NONE', #32303, #21217, #23888, .T. ) ;
#34577 = CARTESIAN_POINT ( 'NONE',  ( 0.005401850751814351800, 0.1458776762658619275, 0.02292264490054247289 ) ) ;
#34578 = CARTESIAN_POINT ( 'NONE',  ( 0.7185039370078739607, 1.928577636452523993E-17, 1.919291338582677309 ) ) ;
#34579 = CARTESIAN_POINT ( 'NONE',  ( 0.07405724077823318263, -0.2539370078202523584, -0.1787899950787401604 ) ) ;
#34580 = EDGE_CURVE ( 'NONE', #46098, #34120, #23919, .T. ) ;
#34581 = DIRECTION ( 'NONE',  ( 1.822029033848725028E-16, 0.000000000000000000, 1.000000000000000000 ) ) ;
#34582 = CARTESIAN_POINT ( 'NONE',  ( 0.7495606340400177148, 0.1264236179284866091, 1.572342519631275692 ) ) ;
#34583 = ADVANCED_FACE ( 'NONE', ( #17156 ), #2991, .T. ) ;
#34584 = CARTESIAN_POINT ( 'NONE',  ( 3.284318927891251994E-17, 0.1115886301959580773, 0.1787899950787401882 ) ) ;
#34585 = CARTESIAN_POINT ( 'NONE',  ( -0.1787899950787401604, 0.1496062992663619862, -0.07405724077823318263 ) ) ;
#34586 = CONTEXT_DEPENDENT_SHAPE_REPRESENTATION ( #28491, #7693 ) ;
#34587 = CARTESIAN_POINT ( 'NONE',  ( 1.284448818897637956, 0.000000000000000000, -1.181102362204724310 ) ) ;
#34588 = EDGE_CURVE ( 'NONE', #19760, #22180, #39802, .T. ) ;
#34589 = CIRCLE ( 'NONE', #13921, 0.08090551181102362266 ) ;
#34590 = AXIS2_PLACEMENT_3D ( 'NONE', #28846, #29575, #43889 ) ;
#34591 = CARTESIAN_POINT ( 'NONE',  ( -1.002407869896990045, -0.1264236179284866091, 0.7308070865604093802 ) ) ;
#34593 = CARTESIAN_POINT ( 'NONE',  ( 0.2759478392031617933, -0.09842519685039370636, 1.713085361781127913 ) ) ;
#34592 = CARTESIAN_POINT ( 'NONE',  ( -0.1574803149606297803, -0.8125000000000006661, 0.06523048226347956391 ) ) ;
#34595 = CARTESIAN_POINT ( 'NONE',  ( -0.7765702477540072923, -0.1393169151461616795, 1.986236931248386517 ) ) ;
#34594 = CARTESIAN_POINT ( 'NONE',  ( 0.07444174185955065859, -1.563528061551551218, 0.1797182628040039087 ) ) ;
#34596 = CARTESIAN_POINT ( 'NONE',  ( -0.1574803149606300301, -0.05954724398696107507, -0.06523048226347956391 ) ) ;
#34597 = CARTESIAN_POINT ( 'NONE',  ( 0.1113553986120547346, -0.4360236219397173318, 0.1113553986120547346 ) ) ;
#34598 = CARTESIAN_POINT ( 'NONE',  ( 0.1787899950787401882, -0.4138779527021417826, -2.189545951927503898E-17 ) ) ;
#34599 = CARTESIAN_POINT ( 'NONE',  ( 0.000000000000000000, 0.000000000000000000, -0.1966003937007873570 ) ) ;
#34600 = CARTESIAN_POINT ( 'NONE',  ( 0.8019270111902717657, 0.1787899950787401604, 1.574803149552536530 ) ) ;
#34601 = CARTESIAN_POINT ( 'NONE',  ( 0.6971942568897648851, 0.07405724077823318263, 1.850393700733638624 ) ) ;
#34602 = CARTESIAN_POINT ( 'NONE',  ( 1.002407869896990045, 0.1264236179284866091, 0.4601377952218267953 ) ) ;
#34603 = EDGE_LOOP ( 'NONE', ( #9407, #14629, #13497, #11049 ) ) ;
#34604 = CIRCLE ( 'NONE', #13934, 0.1968503937007874405 ) ;
#34605 = CARTESIAN_POINT ( 'NONE',  ( 1.614954907737318939E-16, 0.1564960629921311464, 0.3937007874015748254 ) ) ;
#34606 = CARTESIAN_POINT ( 'NONE',  ( -0.8759842519685039353, 0.000000000000000000, 1.995570866087968520 ) ) ;
#34607 = DIRECTION ( 'NONE',  ( 8.659560562353580701E-17, 0.7071067811866579289, -0.7071067811864371055 ) ) ;
#34608 = CARTESIAN_POINT ( 'NONE',  ( 3.284318927891251994E-17, 0.004429133912031243958, 0.1787899950787401882 ) ) ;
#34609 = CARTESIAN_POINT ( 'NONE',  ( 0.7185039370078732945, -0.06523048226347899492, 0.4945866140657012577 ) ) ;
#34610 = CARTESIAN_POINT ( 'NONE',  ( 0.8759842519685039353, -0.1787899950787401882, 0.4453740156942677664 ) ) ;
#34611 = CARTESIAN_POINT ( 'NONE',  ( 0.7598281768898816901, -0.1184571006790323261, 0.03937028442103207571 ) ) ;
#34612 = CARTESIAN_POINT ( 'NONE',  ( 1.350095158311321523E-16, -0.0009842519685041700977, 0.2952755905511816326 ) ) ;
#34613 = LINE ( 'NONE', #16167, #8784 ) ;
#34614 = CARTESIAN_POINT ( 'NONE',  ( -0.9500414927467378812, 0.1787899950787401604, 1.368110236166710125 ) ) ;
#34615 = CARTESIAN_POINT ( 'NONE',  ( 0.8107537697050253289, -0.1574803149606297803, 0.8144685038294804391 ) ) ;
#34616 = ORIENTED_EDGE ( 'NONE', *, *, #41599, .T. ) ;
#34617 = CARTESIAN_POINT ( 'NONE',  ( 0.6971942568897648851, 0.07405724077823318263, 1.067913385773007651 ) ) ;
#34618 = VERTEX_POINT ( 'NONE', #35616 ) ;
#34619 = CARTESIAN_POINT ( 'NONE',  ( -1.094772975963752103E-17, -1.314468503883243988, -0.1787899950787401882 ) ) ;
#34620 = CARTESIAN_POINT ( 'NONE',  ( -0.9412147342319837628, 0.1574803149606300301, 0.5979330707586145710 ) ) ;
#34621 = DIRECTION ( 'NONE',  ( 0.000000000000000000, -1.000000000000000000, -0.000000000000000000 ) ) ;
#34622 = CARTESIAN_POINT ( 'NONE',  ( 0.8759842519685039353, -0.1787899950787401882, 1.744586614119464807 ) ) ;
#34623 = CARTESIAN_POINT ( 'NONE',  ( -0.9412147342319837628, -0.1574803149606297803, 1.262303149606299746 ) ) ;
#34624 = DIRECTION ( 'NONE',  ( 1.000000000000000000, 0.000000000000000000, 0.000000000000000000 ) ) ;
#34626 = LINE ( 'NONE', #45610, #42271 ) ;
#34625 = PLANE ( 'NONE',  #1243 ) ;
#34627 = CARTESIAN_POINT ( 'NONE',  ( 0.7495606340400177148, -0.1264236179284866091, 0.09104330703285078152 ) ) ;
#34628 = CARTESIAN_POINT ( 'NONE',  ( 0.7646288533564489232, 0.1113553986120547346, 1.353346456585388102 ) ) ;
#34629 = ORIENTED_EDGE ( 'NONE', *, *, #483, .F. ) ;
#34630 = ORIENTED_EDGE ( 'NONE', *, *, #6163, .F. ) ;
#34631 = CARTESIAN_POINT ( 'NONE',  ( -0.09932472909908414416, -0.09575019180978999733, -0.2280862973330396448 ) ) ;
#34632 = ORIENTED_EDGE ( 'NONE', *, *, #37493, .T. ) ;
#34633 = CARTESIAN_POINT ( 'NONE',  ( -0.6971942568897637749, 2.189545951927499583E-17, 1.616633858213952779 ) ) ;
#34634 = CARTESIAN_POINT ( 'NONE',  ( 0.1574803149606299191, -0.03740157469562260112, -1.928577636452523993E-17 ) ) ;
#34635 = ORIENTED_EDGE ( 'NONE', *, *, #31259, .F. ) ;
#34636 = COLOUR_RGB ( '', 0.08235294, 0.09019608, 0.10196078) ;
#34637 = ORIENTED_EDGE ( 'NONE', *, *, #14309, .T. ) ;
#34638 = CIRCLE ( 'NONE', #38453, 0.3937007874015747699 ) ;
#34639 = CARTESIAN_POINT ( 'NONE',  ( 0.1574803149606319730, 0.4667239666988196034, -0.7023826619074858835 ) ) ;
#34640 = CARTESIAN_POINT ( 'NONE',  ( 0.1264236179284866091, -1.133490109961521775, -0.1264236179284866091 ) ) ;
#34641 = ORIENTED_EDGE ( 'NONE', *, *, #5235, .T. ) ;
#34642 = CARTESIAN_POINT ( 'NONE',  ( -0.1264236179284866091, -0.03494094482812625663, 0.1264236179284866091 ) ) ;
#34643 = ORIENTED_EDGE ( 'NONE', *, *, #37823, .F. ) ;
#34644 = ORIENTED_EDGE ( 'NONE', *, *, #38052, .T. ) ;
#34645 = CONICAL_SURFACE ( 'NONE', #21597, 0.1003937007874010356, 0.7853981633978559529 ) ;
#34646 = VECTOR ( 'NONE', #42694, 39.37007874015748143 ) ;
#34647 = CARTESIAN_POINT ( 'NONE',  ( -0.8107537697050254399, -0.1574803149606297803, 1.208169291231056430 ) ) ;
#34648 = FACE_OUTER_BOUND ( 'NONE', #30553, .T. ) ;
#34649 = EDGE_CURVE ( 'NONE', #5875, #39913, #6356, .T. ) ;
#34650 = CARTESIAN_POINT ( 'NONE',  ( 0.7185039370078746268, -0.06523048226347956391, 1.882381889763779181 ) ) ;
#34651 = VECTOR ( 'NONE', #31081, 39.37007874015748143 ) ;
#34652 = EDGE_CURVE ( 'NONE', #32565, #7704, #34638, .T. ) ;
#34653 = CARTESIAN_POINT ( 'NONE',  ( -1.054774247047244540, -0.07405724077823318263, 0.2214566928596221063 ) ) ;
#34654 = CARTESIAN_POINT ( 'NONE',  ( -0.7646288533564489232, -0.1113553986120547346, 1.097440944881889813 ) ) ;
#34655 = CARTESIAN_POINT ( 'NONE',  ( 0.1797182628040039365, -1.201815463126352457, -2.200913952912460540E-17 ) ) ;
#34656 = CARTESIAN_POINT ( 'NONE',  ( 0.9412147342319837628, -0.1574803149606297803, 1.104822834645669882 ) ) ;
#34657 = B_SPLINE_CURVE_WITH_KNOTS ( 'NONE', 3,
 ( #44423, #15004, #4894, #15235, #4177, #26260, #15473, #18802, #1294, #40822, #40354, #37253, #19278, #44197, #11396, #11872, #26012, #29655, #4405, #40591, #7546, #19034 ),
 .UNSPECIFIED., .F., .F.,
 ( 4, 2, 2, 2, 2, 2, 2, 2, 2, 2, 4 ),
 ( 0.000000000000000000, 0.1250000000000007494, 0.1875000000000009714, 0.2187500000000011102, 0.2500000000000012212, 0.5000000000000013323, 0.6250000000000015543, 0.6875000000000015543, 0.7187500000000014433, 0.7500000000000012212, 1.000000000000000000 ),
 .UNSPECIFIED. ) ;
#34658 = CARTESIAN_POINT ( 'NONE',  ( 0.7495606340400177148, -0.1264236179284866091, 1.075295275536787276 ) ) ;
#34659 = CARTESIAN_POINT ( 'NONE',  ( 0.8019270111902716547, -0.1787899950787401604, 1.387795275536786610 ) ) ;
#34660 = CARTESIAN_POINT ( 'NONE',  ( 1.002407869896990045, 0.1264236179284866091, 0.1451771653005673179 ) ) ;
#34661 = LINE ( 'NONE', #24111, #3930 ) ;
#34662 = CARTESIAN_POINT ( 'NONE',  ( 0.8759842519685039353, 0.1574803149606299191, 1.594488188976378007 ) ) ;
#34664 = CARTESIAN_POINT ( 'NONE',  ( -0.2133350748062230740, -0.1723249637081083474, -0.3049284531890984473 ) ) ;
#34663 = LINE ( 'NONE', #20259, #2960 ) ;
#34665 = CARTESIAN_POINT ( 'NONE',  ( -0.8759842519685039353, 0.000000000000000000, 0.000000000000000000 ) ) ;
#34666 = ( BOUNDED_CURVE ( )  B_SPLINE_CURVE ( 2, ( #45136, #42260, #19985, #20462, #24077, #16181, #12353, #38443, #8973 ),
 .UNSPECIFIED., .F., .T. ) 
 B_SPLINE_CURVE_WITH_KNOTS ( ( 3, 2, 2, 2, 3 ),
 ( 0.3599999999999999867, 0.3624999999999999889, 0.3649999999999999911, 0.3674999999999999933, 0.3699999999999999956 ),
 .UNSPECIFIED. ) 
 CURVE ( )  GEOMETRIC_REPRESENTATION_ITEM ( )  RATIONAL_B_SPLINE_CURVE ( ( 1.000000000000000000, 0.9238795325112869605, 1.000000000000000000, 0.9238795325112869605, 1.000000000000000000, 0.9238795325112869605, 1.000000000000000000, 0.9238795325112869605, 1.000000000000000000 ) ) 
 REPRESENTATION_ITEM ( '' )  ) ;
#34667 = AXIS2_PLACEMENT_3D ( 'NONE', #15805, #1623, #16272 ) ;
#34668 = CARTESIAN_POINT ( 'NONE',  ( -0.7185039370078746268, 0.06523048226347956391, 1.562500000000000000 ) ) ;
#34669 = CARTESIAN_POINT ( 'NONE',  ( 1.054774247047244540, 0.07405724077823318263, 0.9301181101824563813 ) ) ;
#34670 = CARTESIAN_POINT ( 'NONE',  ( 0.6971942568897648851, 0.07405724077823318263, 1.855314960576157635 ) ) ;
#34671 = CARTESIAN_POINT ( 'NONE',  ( 0.8759842519685039353, 0.1574803149606299191, 0.3641732282389295583 ) ) ;
#34672 = ORIENTED_EDGE ( 'NONE', *, *, #36848, .T. ) ;
#34673 = DIRECTION ( 'NONE',  ( 1.000000000000000000, -3.469446951953614189E-15, 6.938893903907228378E-16 ) ) ;
#34674 = LINE ( 'NONE', #34212, #33643 ) ;
#34675 = CARTESIAN_POINT ( 'NONE',  ( 0.1574803149606300301, -1.688484251860975949, -0.06523048226347956391 ) ) ;
#34676 = CARTESIAN_POINT ( 'NONE',  ( -0.7185039370078746268, 0.06523048226347956391, 0.2140748030420794590 ) ) ;
#34677 = DIRECTION ( 'NONE',  ( 0.000000000000000000, 1.000000000000000000, 0.000000000000000000 ) ) ;
#34678 = CARTESIAN_POINT ( 'NONE',  ( 1.054774247047244540, 0.07405724077823318263, 1.323818897584032817 ) ) ;
#34679 = EDGE_LOOP ( 'NONE', ( #9091, #5410, #18299 ) ) ;
#34680 = CARTESIAN_POINT ( 'NONE',  ( 0.05730322896416124856, -0.07836638817768049048, 0.2523490388730026401 ) ) ;
#34681 = CARTESIAN_POINT ( 'NONE',  ( 0.1113553986120547346, -1.784448818897637734, 0.1113553986120547346 ) ) ;
#34682 = EDGE_CURVE ( 'NONE', #34404, #13881, #10458, .T. ) ;
#34683 = LINE ( 'NONE', #27753, #29885 ) ;
#34684 = CARTESIAN_POINT ( 'NONE',  ( -0.7495606340400177148, -0.1264236179284866091, 0.5191929133320630774 ) ) ;
#34685 = CARTESIAN_POINT ( 'NONE',  ( 0.8107537697050254399, 0.1574803149606300301, 0.2583661417322834497 ) ) ;
#34686 = CARTESIAN_POINT ( 'NONE',  ( -0.4620708661417322616, 0.9842519685039375910, -0.5511811023622041894 ) ) ;
#34687 = AXIS2_PLACEMENT_3D ( 'NONE', #24038, #1079, #35057 ) ;
#34688 = ORIENTED_EDGE ( 'NONE', *, *, #19997, .T. ) ;
#34690 = CARTESIAN_POINT ( 'NONE',  ( 0.1787899950787401604, -1.484251968450174930, 0.07405724077823318263 ) ) ;
#34689 = CARTESIAN_POINT ( 'NONE',  ( 0.06523048226347956391, -0.3843503935932603421, -0.1574803149606300301 ) ) ;
#34691 = CARTESIAN_POINT ( 'NONE',  ( -1.002407869896990045, 0.1264236179284866091, 1.055610236166708793 ) ) ;
#34692 = CARTESIAN_POINT ( 'NONE',  ( -0.8759842519685039353, -0.1787899950787401882, 1.862696850339937038 ) ) ;
#34693 = CARTESIAN_POINT ( 'NONE',  ( -0.9500414927467377701, -0.1787899950787401604, 0.9990157479777320715 ) ) ;
#34694 = CARTESIAN_POINT ( 'NONE',  ( -1.054774247047244540, 0.07405724077823318263, 0.7381889763241898939 ) ) ;
#34695 = ( BOUNDED_CURVE ( )  B_SPLINE_CURVE ( 2, ( #23100, #16622, #20198, #41504, #45829, #8954, #42237, #8710, #27199 ),
 .UNSPECIFIED., .F., .F. ) 
 B_SPLINE_CURVE_WITH_KNOTS ( ( 3, 2, 2, 2, 3 ),
 ( 0.05000000000000000278, 0.05249999999999999806, 0.05500000000000000028, 0.05750000000000000250, 0.05999999999999999778 ),
 .UNSPECIFIED. ) 
 CURVE ( )  GEOMETRIC_REPRESENTATION_ITEM ( )  RATIONAL_B_SPLINE_CURVE ( ( 1.000000000000000000, 0.9238795325112859613, 1.000000000000000000, 0.9238795325112869605, 1.000000000000000000, 0.9238795325112869605, 1.000000000000000000, 0.9238795325112869605, 1.000000000000000000 ) ) 
 REPRESENTATION_ITEM ( '' )  ) ;
#34696 = ORIENTED_EDGE ( 'NONE', *, *, #9710, .F. ) ;
#34697 = LINE ( 'NONE', #41836, #3839 ) ;
#34698 = CARTESIAN_POINT ( 'NONE',  ( 0.7185039370078746268, -0.06523048226347956391, 1.803641732283465471 ) ) ;
#34699 = DIRECTION ( 'NONE',  ( -0.000000000000000000, 0.9771240687918548717, 0.2126700594527834720 ) ) ;
#34700 = CARTESIAN_POINT ( 'NONE',  ( -0.1787899950787401604, -0.6438247556308137609, 0.07405724077823318263 ) ) ;
#34701 = CARTESIAN_POINT ( 'NONE',  ( 0.1329235558887131852, -0.08956032744261475942, -0.1422831879104033415 ) ) ;
#34702 = FACE_OUTER_BOUND ( 'NONE', #6138, .T. ) ;
#34703 = ORIENTED_EDGE ( 'NONE', *, *, #18714, .F. ) ;
#34704 = VECTOR ( 'NONE', #31662, 39.37007874015748854 ) ;
#34705 = CYLINDRICAL_SURFACE ( 'NONE', #35558, 0.1574803149606299191 ) ;
#34706 = CARTESIAN_POINT ( 'NONE',  ( -1.054774247047244540, -0.07405724077823318263, 0.5314960629383620461 ) ) ;
#34707 = CARTESIAN_POINT ( 'NONE',  ( -0.7185039370078739607, 0.000000000000000000, -2.869337061179095023E-17 ) ) ;
#34708 = CIRCLE ( 'NONE', #36977, 0.1787899950787401049 ) ;
#34709 = EDGE_CURVE ( 'NONE', #1718, #2020, #8018, .T. ) ;
#34710 = DIRECTION ( 'NONE',  ( 0.5735764363510447161, -0.8191520442889925757, 1.003171929053525486E-16 ) ) ;
#34711 = CARTESIAN_POINT ( 'NONE',  ( -0.7495606340400177148, 0.1264236179284866091, 1.498523621993480326 ) ) ;
#34712 = PRODUCT_DEFINITION_FORMATION_WITH_SPECIFIED_SOURCE ( 'ANY', '', #18798, .NOT_KNOWN. ) ;
#34713 = CONICAL_SURFACE ( 'NONE', #16339, 0.2471922904502826812, 0.5235987755982992597 ) ;
#34714 = EDGE_CURVE ( 'NONE', #27780, #36671, #39186, .T. ) ;
#34715 = CARTESIAN_POINT ( 'NONE',  ( 0.07405724077823318263, -1.489173228292693718, 0.1787899950787401604 ) ) ;
#34716 = DIRECTION ( 'NONE',  ( 0.000000000000000000, 0.000000000000000000, -1.000000000000000000 ) ) ;
#34717 = CARTESIAN_POINT ( 'NONE',  ( 0.8759842519685039353, -0.1574803149606299191, 0.1968503937007874127 ) ) ;
#34718 = DIRECTION ( 'NONE',  ( 0.000000000000000000, 0.000000000000000000, 1.000000000000000000 ) ) ;
#34719 = CARTESIAN_POINT ( 'NONE',  ( 0.9873396505805591694, -0.1113553986120547346, 0.5561023622047244208 ) ) ;
#34720 = CARTESIAN_POINT ( 'NONE',  ( -0.1797182628040039087, -0.6727800300554868107, -0.07444174185955065859 ) ) ;
#34721 = LINE ( 'NONE', #4985, #40816 ) ;
#34722 = CARTESIAN_POINT ( 'NONE',  ( -0.7185039370078746268, -0.06523048226347956391, 1.242618110128693276 ) ) ;
#34723 = CARTESIAN_POINT ( 'NONE',  ( 1.054774247047244540, -0.07405724077823318263, 0.6545275590013545086 ) ) ;
#34724 = FACE_OUTER_BOUND ( 'NONE', #7966, .T. ) ;
#34726 = CARTESIAN_POINT ( 'NONE',  ( 0.7646288533564489232, -0.1113553986120547346, 0.3494094488188976277 ) ) ;
#34725 = CARTESIAN_POINT ( 'NONE',  ( 0.1574803149606300301, -0.4434055118110233340, 0.06523048226347956391 ) ) ;
#34727 = CARTESIAN_POINT ( 'NONE',  ( 1.284448818897637956, 0.000000000000000000, 1.181102362204724310 ) ) ;
#34728 = EDGE_LOOP ( 'NONE', ( #16476, #8510 ) ) ;
#34729 = CARTESIAN_POINT ( 'NONE',  ( 0.2395294000716134131, 0.000000000000000000, 0.8759842519685039353 ) ) ;
#34730 = CARTESIAN_POINT ( 'NONE',  ( -1.054774247047244540, -0.07405724077823318263, 1.126968503883244654 ) ) ;
#34731 = CARTESIAN_POINT ( 'NONE',  ( 0.7646288533564489232, 0.1113553986120547346, 1.087598425196850460 ) ) ;
#34733 = CARTESIAN_POINT ( 'NONE',  ( 0.000000000000000000, 0.000000000000000000, -0.0004999999999998990712 ) ) ;
#34732 = DIRECTION ( 'NONE',  ( 0.000000000000000000, -1.000000000000000000, 0.000000000000000000 ) ) ;
#34734 = CARTESIAN_POINT ( 'NONE',  ( -1.033464566929134687, 0.06523048226347956391, 0.7111220471365682361 ) ) ;
#34736 = CARTESIAN_POINT ( 'NONE',  ( -0.7646288533564489232, -0.1113553986120547346, 1.953740157372787500 ) ) ;
#34735 = CARTESIAN_POINT ( 'NONE',  ( 1.033464566929134687, 0.06523048226347956391, 0.1697834645669291653 ) ) ;
#34737 = DIRECTION ( 'NONE',  ( 0.000000000000000000, 0.000000000000000000, -1.000000000000000000 ) ) ;
#34738 = CARTESIAN_POINT ( 'NONE',  ( 0.1498753904841986506, 5.122214988120487988E-17, 0.1377952755905511861 ) ) ;
#34739 = CARTESIAN_POINT ( 'NONE',  ( 0.07405724077823318263, -0.5787401574265509385, 0.1787899950787401604 ) ) ;
#34740 = ORIENTED_EDGE ( 'NONE', *, *, #7573, .T. ) ;
#34741 = CARTESIAN_POINT ( 'NONE',  ( 1.033464566929133799, 0.000000000000000000, 0.2854330708661417804 ) ) ;
#34742 = CARTESIAN_POINT ( 'NONE',  ( 0.6971942568897626646, -0.07405724077823297447, 0.7529527558517473684 ) ) ;
#34743 = ORIENTED_EDGE ( 'NONE', *, *, #38098, .T. ) ;
#34744 = CYLINDRICAL_SURFACE ( 'NONE', #7354, 0.1574803149606299191 ) ;
#34745 = DIRECTION ( 'NONE',  ( 1.822029033848725028E-16, 0.000000000000000000, 1.000000000000000000 ) ) ;
#34746 = CARTESIAN_POINT ( 'NONE',  ( 0.1264236179284866091, -1.668799212544661348, -0.1264236179284866091 ) ) ;
#34747 = CARTESIAN_POINT ( 'NONE',  ( 0.1787899950787401604, -0.9724409448281265966, 0.07405724077823318263 ) ) ;
#34748 = CARTESIAN_POINT ( 'NONE',  ( -0.1113553986120547346, -1.439960629921259949, 0.1113553986120547346 ) ) ;
#34749 = CARTESIAN_POINT ( 'NONE',  ( -0.7185039370078739607, 1.928577636452523993E-17, 1.407480314960629864 ) ) ;
#34750 = ORIENTED_EDGE ( 'NONE', *, *, #15820, .F. ) ;
#34751 = EDGE_LOOP ( 'NONE', ( #37548, #47421, #19658, #33838 ) ) ;
#34752 = CARTESIAN_POINT ( 'NONE',  ( -0.9500414927467378812, 0.1787899950787401604, 1.884842519631275026 ) ) ;
#34753 = VERTEX_POINT ( 'NONE', #21940 ) ;
#34754 = CARTESIAN_POINT ( 'NONE',  ( -0.06523048226347956391, -1.363681102254677313, -0.1574803149606300301 ) ) ;
#34756 = CARTESIAN_POINT ( 'NONE',  ( 0.1377952755905511861, 0.000000000000000000, -0.2103840066576717072 ) ) ;
#34755 = CIRCLE ( 'NONE', #41557, 0.09842519685039370636 ) ;
#34757 = CARTESIAN_POINT ( 'NONE',  ( 1.054774247047244540, 0.07405724077823318263, 0.5019685038832442103 ) ) ;
#34758 = CARTESIAN_POINT ( 'NONE',  ( -1.002407869896990045, 0.1264236179284866091, 1.405019684985606476 ) ) ;
#34759 = DIRECTION ( 'NONE',  ( 0.000000000000000000, -0.9699617890481172511, -0.2432573283306705969 ) ) ;
#34760 = CARTESIAN_POINT ( 'NONE',  ( -0.8759842519685039353, -0.1787899950787401882, 0.1747047243556852092 ) ) ;
#34761 = CARTESIAN_POINT ( 'NONE',  ( -0.8759842519685039353, 0.1574803149606299191, 0.5708661417322835607 ) ) ;
#34762 = CARTESIAN_POINT ( 'NONE',  ( -0.6971942568897648851, 0.07405724077823318263, 1.737204724355685848 ) ) ;
#34763 = CARTESIAN_POINT ( 'NONE',  ( -1.054774247047244540, 0.07405724077823318263, 0.1082677164816695514 ) ) ;
#34764 = CARTESIAN_POINT ( 'NONE',  ( 0.03342428880116892626, -0.06208088008896735233, -0.2661310841544295425 ) ) ;
#34765 = CARTESIAN_POINT ( 'NONE',  ( -0.7185039370078739607, 1.928577636452523993E-17, 1.801181102362204633 ) ) ;
#34766 = CARTESIAN_POINT ( 'NONE',  ( -0.4338976377952755703, -0.1574803149606299191, 0.000000000000000000 ) ) ;
#34767 = EDGE_CURVE ( 'NONE', #20854, #46310, #30081, .T. ) ;
#34768 = CARTESIAN_POINT ( 'NONE',  ( 0.7495606340400177148, -0.1264236179284866091, 1.744586614119464807 ) ) ;
#34769 = CARTESIAN_POINT ( 'NONE',  ( 0.1466781083505074856, -0.09842519685039370636, 0.1600438778087322766 ) ) ;
#34770 = CARTESIAN_POINT ( 'NONE',  ( -0.2362204724409467105, 0.1574803149606323616, -1.186023622047243986 ) ) ;
#34771 = EDGE_CURVE ( 'NONE', #28431, #46488, #898, .T. ) ;
#34772 = DIMENSIONAL_EXPONENTS ( 1.000000000000000000, 0.000000000000000000, 0.000000000000000000, 0.000000000000000000, 0.000000000000000000, 0.000000000000000000, 0.000000000000000000 ) ;
#34773 = EDGE_CURVE ( 'NONE', #28143, #3083, #29423, .T. ) ;
#34774 = VERTEX_POINT ( 'NONE', #40355 ) ;
#34775 = ORIENTED_EDGE ( 'NONE', *, *, #20169, .F. ) ;
#34776 = AXIS2_PLACEMENT_3D ( 'NONE', #47203, #43830, #43591 ) ;
#34777 = CARTESIAN_POINT ( 'NONE',  ( 0.1787899950787401604, -1.085629921206079374, -0.07405724077823318263 ) ) ;
#34778 = CARTESIAN_POINT ( 'NONE',  ( -0.1787899950787401604, -1.218503936954111300, 0.07405724077823318263 ) ) ;
#34779 = EDGE_CURVE ( 'NONE', #10690, #24840, #5821, .T. ) ;
#34780 = SHAPE_REPRESENTATION_RELATIONSHIP ( 'NONE' , 'NONE' ,  #14237, #2147 ) ;
#34781 = CARTESIAN_POINT ( 'NONE',  ( 0.1797182628040039087, -0.5349847544649350972, 0.07444174185955046430 ) ) ;
#34782 = CARTESIAN_POINT ( 'NONE',  ( -1.033464566929134687, -0.06523048226347956391, 0.7455708660342049710 ) ) ;
#34783 = CARTESIAN_POINT ( 'NONE',  ( -0.06523048226347956391, 0.004429133858267709535, -0.1574803149606300301 ) ) ;
#34784 = CONICAL_SURFACE ( 'NONE', #27165, 0.09842519685039310962, 0.7853981633972314524 ) ;
#34785 = CARTESIAN_POINT ( 'NONE',  ( 0.8759842519685039353, -0.1787899950787401882, 0.9178149605761574126 ) ) ;
#34786 = DIRECTION ( 'NONE',  ( -1.000000000000000000, 0.000000000000000000, 0.000000000000000000 ) ) ;
#34787 = AXIS2_PLACEMENT_3D ( 'NONE', #28062, #45997, #46464 ) ;
#34788 = CARTESIAN_POINT ( 'NONE',  ( 0.6971942568897637749, 2.189545951927499583E-17, 1.975885826717889815 ) ) ;
#34789 = ORIENTED_EDGE ( 'NONE', *, *, #11426, .F. ) ;
#34790 = CARTESIAN_POINT ( 'NONE',  ( 0.7646288533564489232, -0.1113553986120547346, 0.3789370077664886427 ) ) ;
#34791 = CARTESIAN_POINT ( 'NONE',  ( 0.07405724077823318263, -0.3868110235682837295, 0.1787899950787401604 ) ) ;
#34792 = LINE ( 'NONE', #45530, #15521 ) ;
#34793 = CARTESIAN_POINT ( 'NONE',  ( 0.1264236179284866091, -1.363681102308440973, 0.1264236179284866091 ) ) ;
#34794 = CARTESIAN_POINT ( 'NONE',  ( 0.7495606340400177148, 0.1264236179284866091, 0.3567913385289137596 ) ) ;
#34795 = CARTESIAN_POINT ( 'NONE',  ( 0.2642359194686346169, 0.09842519685039370636, 0.000000000000000000 ) ) ;
#34796 = CARTESIAN_POINT ( 'NONE',  ( -0.7495606340400177148, 0.1264236179284866091, 1.926673228292693052 ) ) ;
#34797 = VERTEX_POINT ( 'NONE', #4406 ) ;
#34798 = CARTESIAN_POINT ( 'NONE',  ( -0.8759842519685039353, -0.1787899950787401882, 1.513287401521039355 ) ) ;
#34799 = DIRECTION ( 'NONE',  ( -1.000000000000000000, 0.000000000000000000, 0.000000000000000000 ) ) ;
#34800 = CARTESIAN_POINT ( 'NONE',  ( 0.8019270111902717657, -0.1787899950787401604, 1.471456692859622217 ) ) ;
#34801 = LINE ( 'NONE', #31678, #9915 ) ;
#34802 = CARTESIAN_POINT ( 'NONE',  ( -0.9500414927467378812, -0.1787899950787401604, 0.5314960629383620461 ) ) ;
#34803 = CARTESIAN_POINT ( 'NONE',  ( 1.054774247047244096, 0.000000000000000000, 0.1058070865604096300 ) ) ;
#34804 = CARTESIAN_POINT ( 'NONE',  ( -0.8019270111902717657, 0.1787899950787401604, 1.254921259788757348 ) ) ;
#34805 = ADVANCED_FACE ( 'NONE', ( #7076 ), #21702, .T. ) ;
#34806 = CARTESIAN_POINT ( 'NONE',  ( 0.08940444365453828479, -0.09842526949101637612, -0.1548350272596675514 ) ) ;
#34807 = SURFACE_STYLE_FILL_AREA ( #24472 ) ;
#34808 = CARTESIAN_POINT ( 'NONE',  ( 0.6971942568897637749, 2.189545951927499583E-17, 0.6766732282926929409 ) ) ;
#34809 = CARTESIAN_POINT ( 'NONE',  ( -0.8759842519685039353, -0.1787899950787401882, 0.5241141731745827537 ) ) ;
#34810 = ( NAMED_UNIT ( * ) SI_UNIT ( $, .STERADIAN. ) SOLID_ANGLE_UNIT ( ) ) ;
#34811 = CARTESIAN_POINT ( 'NONE',  ( 0.4142125984251969206, -1.512724881123248161E-16, 0.000000000000000000 ) ) ;
#34812 = ORIENTED_EDGE ( 'NONE', *, *, #24843, .F. ) ;
#34813 = AXIS2_PLACEMENT_3D ( 'NONE', #28465, #24610, #14312 ) ;
#34814 = CARTESIAN_POINT ( 'NONE',  ( -0.8759842519685039353, -0.1574803149606299191, 0.3149606299212598381 ) ) ;
#34815 = EDGE_CURVE ( 'NONE', #29787, #11192, #40093, .T. ) ;
#34816 = CARTESIAN_POINT ( 'NONE',  ( 0.7495606340400177148, -0.1264236179284866091, 1.272145669237574772 ) ) ;
#34817 = CARTESIAN_POINT ( 'NONE',  ( 0.1141376464151068887, -0.09851384742766575164, 0.1860460344805917599 ) ) ;
#34818 = AXIS2_PLACEMENT_3D ( 'NONE', #6019, #2426, #34821 ) ;
#34819 = CONICAL_SURFACE ( 'NONE', #32531, 0.08090551181102362266, 0.9599310885968742602 ) ;
#34820 = ORIENTED_EDGE ( 'NONE', *, *, #39731, .T. ) ;
#34821 = DIRECTION ( 'NONE',  ( 1.000000000000000000, -9.297927578135879519E-16, 0.000000000000000000 ) ) ;
#34822 = CARTESIAN_POINT ( 'NONE',  ( -0.7495606340400177148, -0.1264236179284866091, 0.9965551180564724554 ) ) ;
#34823 = CARTESIAN_POINT ( 'NONE',  ( -0.9500414927467378812, -0.1787899950787401604, 0.2116141731745827814 ) ) ;
#34824 = ORIENTED_EDGE ( 'NONE', *, *, #45495, .T. ) ;
#34825 = CARTESIAN_POINT ( 'NONE',  ( -0.07405724077823318263, -0.6624015747493856576, 0.1787899950787401604 ) ) ;
#34826 = CARTESIAN_POINT ( 'NONE',  ( -0.3100393700787401619, -2.714815113292586694E-26, -0.7086614173228351632 ) ) ;
#34827 = ORIENTED_EDGE ( 'NONE', *, *, #17045, .F. ) ;
#34828 = CARTESIAN_POINT ( 'NONE',  ( 1.054774247047244540, 0.07405724077823318263, 1.363188976324188895 ) ) ;
#34829 = CARTESIAN_POINT ( 'NONE',  ( 0.002094777259500726820, 0.1352690037935440348, 0.04129845016539761271 ) ) ;
#34830 = CARTESIAN_POINT ( 'NONE',  ( 0.07405724077823318263, -0.7214566928596228834, -0.1787899950787401604 ) ) ;
#34831 = LINE ( 'NONE', #20652, #11136 ) ;
#34832 = CARTESIAN_POINT ( 'NONE',  ( 1.054774247047244096, 0.000000000000000000, 1.636318897584031484 ) ) ;
#34833 = CARTESIAN_POINT ( 'NONE',  ( -0.1787899950787401604, -0.05819483437097103251, -0.07405724077823318263 ) ) ;
#34834 = CARTESIAN_POINT ( 'NONE',  ( 0.1264236179284866091, 0.1373031496600628232, -0.1264236179284866091 ) ) ;
#34835 = SHAPE_DEFINITION_REPRESENTATION ( #43248, #17291 ) ;
#34836 = CARTESIAN_POINT ( 'NONE',  ( -0.9873396505805591694, 0.1113553986120547346, 1.737204724301921299 ) ) ;
#34837 = CARTESIAN_POINT ( 'NONE',  ( 1.054774247047244540, -0.07405724077823318263, 0.4921259841982048577 ) ) ;
#34838 = ( BOUNDED_CURVE ( )  B_SPLINE_CURVE ( 2, ( #13001, #42198, #46274, #24019, #46035, #38621, #5798, #20404, #35044 ),
 .UNSPECIFIED., .F., .T. ) 
 B_SPLINE_CURVE_WITH_KNOTS ( ( 3, 2, 2, 2, 3 ),
 ( 0.9100000000000000311, 0.9124999999999999778, 0.9150000000000000355, 0.9174999999999999822, 0.9200000000000000400 ),
 .UNSPECIFIED. ) 
 CURVE ( )  GEOMETRIC_REPRESENTATION_ITEM ( )  RATIONAL_B_SPLINE_CURVE ( ( 1.000000000000000000, 0.9238795325112899581, 1.000000000000000000, 0.9238795325112869605, 1.000000000000000000, 0.9238795325112869605, 1.000000000000000000, 0.9238795325112869605, 1.000000000000000000 ) ) 
 REPRESENTATION_ITEM ( '' )  ) ;
#34839 = CARTESIAN_POINT ( 'NONE',  ( -1.054774247047244096, 0.000000000000000000, 0.8538385826234016207 ) ) ;
#34841 = CARTESIAN_POINT ( 'NONE',  ( 0.7185039370078746268, 0.06523048226347956391, 0.09596456682160686702 ) ) ;
#34840 = CARTESIAN_POINT ( 'NONE',  ( 2.892866454678787531E-17, -0.8444881889763780070, 0.1574803149606299191 ) ) ;
#34842 = CARTESIAN_POINT ( 'NONE',  ( -0.1797182628040039087, -1.578291841079108471, -0.07444174185955065859 ) ) ;
#34843 = VECTOR ( 'NONE', #40602, 39.37007874015748143 ) ;
#34844 = CARTESIAN_POINT ( 'NONE',  ( 0.8759842519685039353, -0.1787899950787401882, 1.473917322780881722 ) ) ;
#34845 = CARTESIAN_POINT ( 'NONE',  ( 1.054774247047244540, -0.07405724077823318263, 1.909448818843873186 ) ) ;
#34846 = CARTESIAN_POINT ( 'NONE',  ( 1.002407869896990045, -0.1264236179284866091, 0.3321850393163153226 ) ) ;
#34847 = AXIS2_PLACEMENT_3D ( 'NONE', #19116, #33782, #34459 ) ;
#34848 = MECHANICAL_DESIGN_GEOMETRIC_PRESENTATION_REPRESENTATION (  '', ( #25641 ), #4953 ) ;
#34849 = ORIENTED_EDGE ( 'NONE', *, *, #44195, .T. ) ;
#34850 = CARTESIAN_POINT ( 'NONE',  ( -1.033464566929133799, 0.000000000000000000, 1.023622047136567126 ) ) ;
#34851 = DIRECTION ( 'NONE',  ( 1.000000000000000000, 0.000000000000000000, 0.000000000000000000 ) ) ;
#34852 = DIRECTION ( 'NONE',  ( 1.000000000000000000, 3.662381193212024518E-16, -7.324762386424049233E-15 ) ) ;
#34854 = CARTESIAN_POINT ( 'NONE',  ( -0.07405724077823318263, 0.001968503990771400605, 0.1787899950787401604 ) ) ;
#34853 = CARTESIAN_POINT ( 'NONE',  ( -0.1113553986120547346, -0.8494094487113701408, -0.1113553986120547346 ) ) ;
#34855 = CARTESIAN_POINT ( 'NONE',  ( 0.8759842519685039353, -0.1787899950787401882, 0.5241141731745827537 ) ) ;
#34856 = DIRECTION ( 'NONE',  ( -1.000000000000000000, 0.000000000000000000, 0.000000000000000000 ) ) ;
#34857 = CARTESIAN_POINT ( 'NONE',  ( 0.2362204724409448231, 0.000000000000000000, -1.186023622047243986 ) ) ;
#34858 = CARTESIAN_POINT ( 'NONE',  ( -0.8759842519685039353, -0.1787899950787401882, 1.508366141678519678 ) ) ;
#34859 = CARTESIAN_POINT ( 'NONE',  ( 0.8759842519685039353, -0.1574803149606299191, 0.7381889762704251234 ) ) ;
#34860 = ORIENTED_EDGE ( 'NONE', *, *, #45320, .F. ) ;
#34861 = CARTESIAN_POINT ( 'NONE',  ( -1.033464566929133799, 1.928577636452524610E-17, 2.869337061179095023E-17 ) ) ;
#34862 = CARTESIAN_POINT ( 'NONE',  ( 0.7495606340400177148, 0.1264236179284866091, 1.065452755851747924 ) ) ;
#34863 = ORIENTED_EDGE ( 'NONE', *, *, #24215, .T. ) ;
#34864 = CARTESIAN_POINT ( 'NONE',  ( -1.033464566929133799, 0.000000000000000000, 0.5905511809948347235 ) ) ;
#34865 = CARTESIAN_POINT ( 'NONE',  ( -0.8759842519685039353, -0.1574803149606299191, 1.377952755905512028 ) ) ;
#34866 = EDGE_CURVE ( 'NONE', #30859, #36338, #5613, .T. ) ;
#34867 = CARTESIAN_POINT ( 'NONE',  ( 1.033464566929133799, 0.000000000000000000, 1.820866141732283561 ) ) ;
#34869 = CARTESIAN_POINT ( 'NONE',  ( -0.1574803149606299191, 0.5419727308409664213, -0.7545416139885205986 ) ) ;
#34868 = CARTESIAN_POINT ( 'NONE',  ( 0.1792139591738777793, 0.1920237930726759468, -0.3110703821948122005 ) ) ;
#34870 = CARTESIAN_POINT ( 'NONE',  ( 1.002407869896990045, 0.1264236179284866091, 0.1500984251430867999 ) ) ;
#34871 = CARTESIAN_POINT ( 'NONE',  ( -0.6971942568897626646, -0.07405724077823297447, 0.08366141726907130871 ) ) ;
#34872 = CARTESIAN_POINT ( 'NONE',  ( 1.033464566929133799, 0.000000000000000000, 1.456692913278299084 ) ) ;
#34873 = ORIENTED_EDGE ( 'NONE', *, *, #17211, .F. ) ;
#34874 = ORIENTED_EDGE ( 'NONE', *, *, #27486, .F. ) ;
#34875 = EDGE_CURVE ( 'NONE', #2629, #21809, #34626, .T. ) ;
#34876 = CARTESIAN_POINT ( 'NONE',  ( 0.7185039370078739607, 1.928577636452523993E-17, 0.5807086614173228023 ) ) ;
#34877 = B_SPLINE_CURVE_WITH_KNOTS ( 'NONE', 3,
 ( #9670, #21380, #43173, #31481, #6758, #17790, #32437, #28126, #20906, #32188, #46068, #17316, #24985, #6998, #47014, #24286, #31718 ),
 .UNSPECIFIED., .F., .F.,
 ( 4, 2, 2, 2, 2, 1, 2, 2, 4 ),
 ( 0.000000000000000000, 0.2499999999999797384, 0.3749999999999609201, 0.4999999999999420464, 0.6249999999999232836, 0.6874999999999268363, 0.7187499999999351630, 0.7499999999999434896, 1.000000000000000000 ),
 .UNSPECIFIED. ) ;
#34878 = EDGE_CURVE ( 'NONE', #873, #3606, #21617, .T. ) ;
#34879 = CARTESIAN_POINT ( 'NONE',  ( -1.002407869896990045, -0.1264236179284866091, 1.631397637741511808 ) ) ;
#34880 = CARTESIAN_POINT ( 'NONE',  ( 0.06523048226347956391, -0.2022637794200320971, 0.1574803149606297803 ) ) ;
#34881 = EDGE_CURVE ( 'NONE', #7898, #32014, #12003, .T. ) ;
#34882 = CARTESIAN_POINT ( 'NONE',  ( -0.7185039370078739607, 1.928577636452523993E-17, 0.2559055117034968463 ) ) ;
#34883 = FACE_OUTER_BOUND ( 'NONE', #16623, .T. ) ;
#34884 = CIRCLE ( 'NONE', #40172, 0.09940944881889700324 ) ;
#34885 = DIRECTION ( 'NONE',  ( -1.000000000000000000, 0.000000000000000000, 0.000000000000000000 ) ) ;
#34886 = CARTESIAN_POINT ( 'NONE',  ( 0.1264236179284866091, -1.172860188701678963, -0.1264236179284866091 ) ) ;
#34887 = ORIENTED_EDGE ( 'NONE', *, *, #11343, .F. ) ;
#34888 = CARTESIAN_POINT ( 'NONE',  ( -0.1264236179284866091, -0.04478346451316559534, -0.1264236179284866091 ) ) ;
#34889 = VERTEX_POINT ( 'NONE', #8258 ) ;
#34890 = VECTOR ( 'NONE', #34947, 39.37007874015748143 ) ;
#34891 = AXIS2_PLACEMENT_3D ( 'NONE', #37086, #44261, #33292 ) ;
#34892 = VERTEX_POINT ( 'NONE', #15717 ) ;
#34893 = CARTESIAN_POINT ( 'NONE',  ( -0.8107537697050254399, -0.1574803149606297803, 1.405019684931842816 ) ) ;
#34894 = CARTESIAN_POINT ( 'NONE',  ( -0.1184675242425147906, -0.09842519685039370636, 1.870565676741754668 ) ) ;
#34895 = CARTESIAN_POINT ( 'NONE',  ( 0.7185039370078746268, -0.06523048226347956391, 1.764271653543307838 ) ) ;
#34896 = CARTESIAN_POINT ( 'NONE',  ( 0.07405724077823318263, -0.6870078739619840391, -0.1787899950787401604 ) ) ;
#34897 = CARTESIAN_POINT ( 'NONE',  ( -0.8759842519685039353, 0.1787899950787401882, 0.3518700786863940833 ) ) ;
#34898 = CARTESIAN_POINT ( 'NONE',  ( -0.7185039370078739607, 1.928577636452523993E-17, 1.013779527559055094 ) ) ;
#34900 = CARTESIAN_POINT ( 'NONE',  ( -0.7366659922730268706, 0.08466132560603677193, 1.981546310870151428 ) ) ;
#34899 = CARTESIAN_POINT ( 'NONE',  ( -0.07444174185955065859, -1.214118612732652425, 0.1797182628040039087 ) ) ;
#34901 = CARTESIAN_POINT ( 'NONE',  ( -0.1657445988168630702, 0.1998015435187649458, -0.03531881253560850004 ) ) ;
#34902 = CARTESIAN_POINT ( 'NONE',  ( 0.7495606340400177148, 0.1264236179284866091, 1.065452755851747924 ) ) ;
#34903 = AXIS2_PLACEMENT_3D ( 'NONE', #46666, #7380, #29239 ) ;
#34904 = CARTESIAN_POINT ( 'NONE',  ( -0.8107537697050254399, 0.1574803149606300301, 0.6422244093412927679 ) ) ;
#34905 = CARTESIAN_POINT ( 'NONE',  ( 0.7646288533564489232, -0.1113553986120547346, 1.491141732283464583 ) ) ;
#34907 = LINE ( 'NONE', #27733, #43026 ) ;
#34906 = DIRECTION ( 'NONE',  ( 0.5735764363510447161, 0.8191520442889925757, 0.000000000000000000 ) ) ;
#34908 = DIRECTION ( 'NONE',  ( 1.822029033848725028E-16, 0.000000000000000000, 1.000000000000000000 ) ) ;
#34909 = CARTESIAN_POINT ( 'NONE',  ( 0.1113553986120547346, -0.7509842518609763928, 0.1113553986120547346 ) ) ;
#34910 = DIRECTION ( 'NONE',  ( 0.000000000000000000, 0.000000000000000000, 1.000000000000000000 ) ) ;
#34911 = CARTESIAN_POINT ( 'NONE',  ( 0.7495606340400177148, 0.1264236179284866091, 0.9424212597887559051 ) ) ;
#34912 = CARTESIAN_POINT ( 'NONE',  ( 0.8019270111902716547, 0.1787899950787401604, 1.929133858213952557 ) ) ;
#34913 = CARTESIAN_POINT ( 'NONE',  ( 0.9412147342319837628, -0.1574803149606297803, 0.3469488187901108023 ) ) ;
#34914 = VERTEX_POINT ( 'NONE', #41771 ) ;
#34915 = CARTESIAN_POINT ( 'NONE',  ( -0.8070866141732283561, -0.3937007874015746034, 0.7574803149606299524 ) ) ;
#34916 = TOROIDAL_SURFACE ( 'NONE', #10421, 0.7775590551181102983, 0.009842519685039369942 ) ;
#34917 = CARTESIAN_POINT ( 'NONE',  ( -9.642888182262618425E-18, -1.681102362097196767, -0.1574803149606299191 ) ) ;
#34918 = CARTESIAN_POINT ( 'NONE',  ( -1.033464566929134687, -0.06523048226347956391, 0.1943897636720004762 ) ) ;
#34919 = DIRECTION ( 'NONE',  ( 0.000000000000000000, 0.000000000000000000, -1.000000000000000000 ) ) ;
#34920 = CARTESIAN_POINT ( 'NONE',  ( 0.7495606340400177148, 0.1264236179284866091, 1.257381889710015743 ) ) ;
#34921 = DIRECTION ( 'NONE',  ( 0.000000000000000000, 1.000000000000000000, 0.000000000000000000 ) ) ;
#34922 = CARTESIAN_POINT ( 'NONE',  ( 3.284318927891251994E-17, 0.1274606299750234428, 0.1787899950787401882 ) ) ;
#34923 = LINE ( 'NONE', #42318, #43603 ) ;
#34924 = EDGE_CURVE ( 'NONE', #12211, #14871, #11873, .T. ) ;
#34925 = CARTESIAN_POINT ( 'NONE',  ( -0.6971942568897626646, 0.07405724077823318263, 0.5905511810485987167 ) ) ;
#34926 = DIRECTION ( 'NONE',  ( -0.000000000000000000, 1.000000000000000000, 1.020425574104001164E-16 ) ) ;
#34927 = CARTESIAN_POINT ( 'NONE',  ( -0.1787899950787401604, -1.617125984198204414, 0.07405724077823318263 ) ) ;
#34928 = CARTESIAN_POINT ( 'NONE',  ( -0.8759842519685039353, -0.1787899950787401882, 1.040846456639149764 ) ) ;
#34929 = CARTESIAN_POINT ( 'NONE',  ( -0.6971942568897648851, -0.07405724077823297447, 1.934055118056471567 ) ) ;
#34930 = VERTEX_POINT ( 'NONE', #26500 ) ;
#34931 = EDGE_CURVE ( 'NONE', #8568, #8310, #46530, .T. ) ;
#34932 = CARTESIAN_POINT ( 'NONE',  ( -0.7495606340400177148, 0.1264236179284866091, 0.7504921259304880854 ) ) ;
#34933 = ORIENTED_EDGE ( 'NONE', *, *, #45147, .F. ) ;
#34934 = CARTESIAN_POINT ( 'NONE',  ( -0.7185039370078746268, 0.06523048226347956391, 0.09596456682160686702 ) ) ;
#34935 = CARTESIAN_POINT ( 'NONE',  ( -1.094772975963752103E-17, -0.6561279052371122855, -0.1787899950787401882 ) ) ;
#34936 = VERTEX_POINT ( 'NONE', #37739 ) ;
#34937 = CARTESIAN_POINT ( 'NONE',  ( 0.1168315015349214586, -0.08956051179396516682, -0.1546330483755491980 ) ) ;
#34938 = FACE_OUTER_BOUND ( 'NONE', #1549, .T. ) ;
#34939 = DIRECTION ( 'NONE',  ( 0.000000000000000000, 0.000000000000000000, -1.000000000000000000 ) ) ;
#34940 = CARTESIAN_POINT ( 'NONE',  ( -0.7646288533564489232, -0.1113553986120547346, 1.756889763671999782 ) ) ;
#34941 = CARTESIAN_POINT ( 'NONE',  ( -1.054774247047244540, -0.07405724077823318263, 0.4921259841982048577 ) ) ;
#34942 = CARTESIAN_POINT ( 'NONE',  ( -1.181162989532618060E-16, -0.0009842519685041700977, -0.2952755905511816326 ) ) ;
#34943 = VERTEX_POINT ( 'NONE', #5367 ) ;
#34944 = CARTESIAN_POINT ( 'NONE',  ( -0.8019270111902716547, -0.1787899950787401604, 1.668307086560410157 ) ) ;
#34945 = CARTESIAN_POINT ( 'NONE',  ( -0.1787899950787401604, -1.543307086560409713, -0.07405724077823318263 ) ) ;
#34946 = ADVANCED_FACE ( 'NONE', ( #30352 ), #33897, .T. ) ;
#34947 = DIRECTION ( 'NONE',  ( 0.000000000000000000, 0.000000000000000000, -1.000000000000000000 ) ) ;
#34948 = ( BOUNDED_CURVE ( )  B_SPLINE_CURVE ( 2, ( #46130, #13779, #28426, #20503, #6107, #27500, #42050, #16686, #17141 ),
 .UNSPECIFIED., .F., .T. ) 
 B_SPLINE_CURVE_WITH_KNOTS ( ( 3, 2, 2, 2, 3 ),
 ( 0.8299999999999999600, 0.8325000000000000178, 0.8349999999999999645, 0.8375000000000000222, 0.8399999999999999689 ),
 .UNSPECIFIED. ) 
 CURVE ( )  GEOMETRIC_REPRESENTATION_ITEM ( )  RATIONAL_B_SPLINE_CURVE ( ( 1.000000000000000000, 0.9238795325112899581, 1.000000000000000000, 0.9238795325112869605, 1.000000000000000000, 0.9238795325112869605, 1.000000000000000000, 0.9238795325112869605, 1.000000000000000000 ) ) 
 REPRESENTATION_ITEM ( '' )  ) ;
#34949 = CARTESIAN_POINT ( 'NONE',  ( -0.7646288533564489232, 0.1113553986120547346, 0.4970472440944882497 ) ) ;
#34950 = CARTESIAN_POINT ( 'NONE',  ( 0.7185039370078746268, 0.06523048226347956391, 0.5388779527559054427 ) ) ;
#34951 = CARTESIAN_POINT ( 'NONE',  ( -0.07444174185955065859, -0.6777012898980057098, -0.1797182628040039087 ) ) ;
#34952 = DIRECTION ( 'NONE',  ( 0.000000000000000000, 1.000000000000000000, 0.000000000000000000 ) ) ;
#34953 = CARTESIAN_POINT ( 'NONE',  ( -0.7185039370078746268, -0.06523048226347956391, 1.163877952648379344 ) ) ;
#34955 = CARTESIAN_POINT ( 'NONE',  ( -0.1604642934754345052, -0.09842519685039373412, -0.07810648738970782379 ) ) ;
#34954 = CARTESIAN_POINT ( 'NONE',  ( -0.1574803149606297803, -0.3794291338582678752, 0.06523048226347956391 ) ) ;
#34956 = PLANE ( 'NONE',  #43701 ) ;
#34957 = ORIENTED_EDGE ( 'NONE', *, *, #11424, .T. ) ;
#34958 = DIRECTION ( 'NONE',  ( -1.000000000000000000, 0.000000000000000000, 7.051687499798870116E-15 ) ) ;
#34959 = CARTESIAN_POINT ( 'NONE',  ( -0.6971942568897648851, 0.07405724077823318263, 1.146653543253323582 ) ) ;
#34960 = CARTESIAN_POINT ( 'NONE',  ( 0.9873396505805591694, -0.1113553986120547346, 1.028543307086614123 ) ) ;
#34961 = DIRECTION ( 'NONE',  ( 0.000000000000000000, -1.000000000000000000, 0.000000000000000000 ) ) ;
#34963 = CARTESIAN_POINT ( 'NONE',  ( -0.9410460383272908347, -0.1644621043414253858, 1.989368141162188186 ) ) ;
#34962 = FACE_OUTER_BOUND ( 'NONE', #25249, .T. ) ;
#34964 = CARTESIAN_POINT ( 'NONE',  ( 0.1574803149606300301, -0.5910433069790869132, 0.06523048226347956391 ) ) ;
#34966 = FACE_OUTER_BOUND ( 'NONE', #23310, .T. ) ;
#34965 = CYLINDRICAL_SURFACE ( 'NONE', #21476, 0.2952755905511806334 ) ;
#34967 = CARTESIAN_POINT ( 'NONE',  ( 0.000000000000000000, 0.000000000000000000, 0.000000000000000000 ) ) ;
#34968 = CARTESIAN_POINT ( 'NONE',  ( 0.1264236179284866091, -0.5369094487651339120, 0.1264236179284866091 ) ) ;
#34969 = ORIENTED_EDGE ( 'NONE', *, *, #9556, .T. ) ;
#34970 = CARTESIAN_POINT ( 'NONE',  ( -0.3094147346904633777, 0.02254976514608433499, 0.7098108543537183790 ) ) ;
#34971 = AXIS2_PLACEMENT_3D ( 'NONE', #7465, #40278, #4097 ) ;
#34972 = CARTESIAN_POINT ( 'NONE',  ( 0.8759842519685039353, 0.1787899950787401882, 0.8193897637257637756 ) ) ;
#34973 = ORIENTED_EDGE ( 'NONE', *, *, #29729, .T. ) ;
#34974 = CARTESIAN_POINT ( 'NONE',  ( -0.06655125492326575964, 0.08353766247255413335, -0.2470096859212868312 ) ) ;
#34975 = CARTESIAN_POINT ( 'NONE',  ( 0.000000000000000000, 0.000000000000000000, 0.000000000000000000 ) ) ;
#34976 = CARTESIAN_POINT ( 'NONE',  ( 0.1264236179284866091, -1.757381889710015965, 0.1264236179284866091 ) ) ;
#34977 = CARTESIAN_POINT ( 'NONE',  ( -0.07405724077823318263, -1.115157480261196987, -0.1787899950787401604 ) ) ;
#34978 = CARTESIAN_POINT ( 'NONE',  ( -0.06523048226347956391, -1.358759842519685845, 0.1574803149606297803 ) ) ;
#34980 = ( BOUNDED_SURFACE ( )  B_SPLINE_SURFACE ( 1, 2, ( 
 ( #23723, #8863, #37619, #16307, #38097, #37370, #33582, #23255, #12002, #8377, #19165, #15843, #12722, #695, #4525, #11766, #19645, #16074, #9102, #4777, #34056, #30699, #26386, #26860, #15601, #45264, #5259, #34508, #27110, #12483, #41419, #41657, #1183, #5024, #26623, #8140, #30466, #22764, #19879, #23495, #12235, #15353, #30935, #942, #37870, #45496, #27351, #34289, #1661, #1415, #23007, #41894, #18923, #30004, #44548, #40945, #20582, #16996, #1901, #10044, #34760, #24661, #6193, #43083, #45976, #42830, #31636, #21047, #46447, #20816, #39254, #13413, #38570, #31867, #28045, #35454, #17457, #6430, #10287, #35227, #2136, #38803, #24895, #23965, #16763, #2598, #13629, #9346, #35689, #24200, #5500, #39024, #2824, #5737, #28267, #32091, #46678, #13187, #13870, #28511, #12948, #9582, #20112, #42604, #5963, #16539, #31166, #46213, #45739, #9818, #24424, #20353, #27584, #42136, #34991, #31402, #27821, #42383, #18629, #21999, #14819, #25842, #33289, #7388, #32582, #413, #44258, #47169, #36856, #3560, #10999, #29253, #44029, #3065, #21523, #29485, #36625, #17695, #39493, #14352, #36160, #14113, #32344, #46924, #11232, #28757, #40424, #43558, #29000, #10769, #11458, #43326, #21772, #6667, #32813, #10528, #15064, #33051, #25125, #3315, #25381, #39957, #7148, #36402, #3785, #18173, #47407, #14579, #40192, #18403, #15290, #22705, #7848, #30182, #11942, #37083, #37310, #30411, #41590, #18861, #34228, #44726, #5193, #40649, #635, #26328, #878, #30638, #29941, #23190, #44487, #8557, #37804, #4459, #4957, #15781, #19584, #23429, #26564, #40889, #45200, #41122, #11702, #4232, #30878, #45439, #8796, #8082, #19343, #44959, #16013, #26075, #8317, #12422, #19101, #33767, #1357, #15539, #22946, #37556, #4717, #22463, #33519, #27042, #33995, #38035, #19818, #1122, #12172, #26795, #41352, #34446, #1593, #9521, #6373, #41834, #31108, #5434, #13356, #9755, #2775, #45917, #27767, #24368, #20052, #20529, #9279, #38968, #31810, #28208, #20755, #6133, #35164, #35402, #13131, #46160, #38507, #1838, #42327, #16478, #13573, #2543, #24146, #27286, #24598, #45671, #31578, #9988, #39197, #2307, #46396, #38749, #16705, #20287, #17398, #32037, #12661, #5914, #16936, #27984, #9037, #17172, #23660, #42773, #42552, #38269, #5678, #20985, #35634, #34694, #12889, #27524, #42077, #23900, #34932, #6616, #47110, #28453, #3962, #40370, #43022, #3006, #3505, #32287, #39906, #10228, #21952, #7339, #14052, #18355, #28943, #14770, #28700, #14300, #35854, #25798, #43503, #43980, #21229, #6844, #32998, #21720, #11187, #10472, #25070, #14532, #46866, #3735, #17640, #22171, #43271, #36351, #24835, #46628, #7558, #18118, #32762, #29197, #43744, #10948, #36574, #121, #33885, #4133, #19463, #22594, #29834, #7973, #18985, #759, #15421, #30069, #22827, #37442, #4592, #1006, #41953, #24259, #38152, #5316, #27647, #27167, #41718, #31453, #9160, #30761, #37927, #31696, #46279, #42436, #45327, #20168, #45797, #16815, #26922, #23774, #13246, #8922, #19931, #9405, #34568, #1720, #38389, #12544, #41473, #8678, #9640, #5558, #38855, #6020, #16366, #23312, #31220, #30990, #34822, #1963, #16595, #20642, #19701, #42203, #34342, #24022, #38626, #17055, #5801, #20408, #35047, #1474, #2193, #35287, #2427, #16131, #40201, #33297, #2985, #17617, #3226, #34486, #1882, #27565, #47335, #8009, #21933, #36553, #20210, #19742, #26487, #33924, #26727, #45371, #26964, #8965, #28373, #10393, #28140, #42480, #25493, #40759, #3174, #32453, #21881, #18278, #14688, #47030, #7715, #28864, #22331, #18508, #25234, #43664, #40525, #29362, #18736, #25946, #33164, #36725, #29111, #39823, #32920, #7012, #4115, #33394, #43903, #21639, #15168, #36272, #22099, #511, #29813, #40294, #44358, #40, #7259, #40059, #3424, #18039, #47274, #36501, #11103, #25725, #14453, #11566, #3656, #26191, #284, #7479, #14930, #29594, #1223, #5297, #30737, #5064, #41700, #40995, #12758, #30046, #8419, #4332, #41932, #30968, #18966, #8181, #41455, #22806, #15877, #33626, #12525, #45306, #4573, #8901, #19443, #19915, #19207, #23046, #26429, #16347, #34095, #34546, #44592, #44832, #23533, #37665, #45535, #984, #15643, #37907, #37415, #33866, #38135, #4820, #12043, #741, #9140, #37188, #27389, #26665, #30502, #8656, #27147, #15402, #45064, #11808, #41214, #12278, #19681, #26897, #23292, #34323, #1454, #16112, #28558, #13669, #42417, #21092, #42874, #42176, #38365, #28081, #2174, #46017, #24005, #20622, #17503, #5539, #9386, #16573, #24464, #20855, #13913, #9621, #38836, #35498, #31203, #31675, #20385, #2638, #10085, #39297, #31907, #17271, #46254, #46490, #24239, #35026, #28306, #24697, #6471, #35730, #2868, #13451, #32134, #6002, #9853, #31436, #12985, #35269, #27625, #46725, #43127, #2404, #20151, #23756, #38603, #42643, #34798, #1939, #6231, #45775, #17037, #27860, #13226, #5779, #29761, #10331, #29048, #25430, #21821, #6713, #14873, #39538, #29532, #11052, #462, #3366, #224, #36449, #25892, #3832, #25664, #44083, #14161, #33338, #3115, #43607, #24942, #15114, #4064, #21327, #28804, #14630, #43367, #3603, #35960, #33101, #18453, #25177, #11280, #40005, #40474, #39761, #10817, #46971, #36910, #7198, #7658, #17742, #17976, #22274, #18223, #18678, #21574, #36214, #7429, #10578, #6953, #32391, #32863, #32630, #47217, #14400, #47459, #29300, #43848, #22048, #36674, #34276, #1653, #15591, #1405, #11756, #26378, #26851, #40937, #44540, #41168, #15343, #16298, #44308, #30691, #30229, #41650, #45255, #29996, #11511, #1172, #22757, #19152, #8133, #8371, #38089, #26133, #37362, #37132, #45013, #41409, #34499, #44777, #11993, #8607, #4283, #4769, #34048, #23246, #8852, #26615, #19396, #4514, #37860, #15832, #5014, #23488, #12475, #40702, #37610, #33817, #30456, #22517, #933, #12225, #19634, #27098, #690, #5248, #19873, #18914, #33572, #20808, #16530, #28036, #17225, #9808, #38564, #42595, #35447, #38320, #34985, #30926, #20575, #31396, #13407, #6184, #2128, #23713, #45966, #16757, #34752, #13180, #13620, #10034, #1894, #27817, #31860, #42821, #24416, #2587, #46439, #24653, #46206, #23958, #39247, #35681, #5729, #28259, #42376, #2354, #35217, #6420, #41885, #31158, #21038, #39018, #9092, #45488, #20345, #12943, #5493, #27341, #20106, #2818, #45727, #12715, #9575, #24193, #9339, #27575, #42125, #38795, #5955, #16988, #31629, #3777 ),
 ( #10276, #25609, #36150, #44022, #32084, #39483, #17684, #39708, #21993, #6660, #14573, #21279, #47400, #29245, #14104, #43794, #47160, #21513, #25117, #22216, #36846, #17450, #3305, #32576, #28990, #13860, #36618, #46672, #18398, #18164, #28505, #10519, #7384, #43549, #33042, #10993, #32804, #168, #35902, #40416, #24886, #17922, #43071, #3056, #11224, #32336, #46915, #21763, #28750, #10763, #43315, #40184, #14815, #6893, #29478, #14344, #25837, #25370, #39950, #7142, #36398, #3552, #19578, #44251, #11695, #23182, #37303, #1350, #15285, #29935, #4708, #4227, #18856, #8549, #19091, #7842, #15058, #8790, #23425, #34223, #22454, #44715, #22938, #41347, #4002, #22698, #37798, #33513, #627, #33988, #44480, #26321, #871, #37075, #18624, #33284, #4950, #4453, #16007, #30631, #40879, #409, #8308, #8076, #33761, #15530, #30174, #45194, #29706, #11936, #11454, #19337, #1114, #41588, #26558, #41115, #15773, #26069, #37547, #30405, #44954, #12416, #27037, #12165, #26790, #40640, #40239, #36210, #3599, #28801, #39535, #47214, #6711, #18449, #7426, #14396, #17500, #44079, #21325, #18219, #11276, #40470, #40002, #22045, #7654, #47457, #36670, #17738, #14628, #22270, #29297, #10574, #43845, #2864, #10328, #6950, #32132, #7194, #3362, #11047, #46723, #21571, #43124, #29045, #43604, #32388, #10814, #13910, #28556, #46968, #25427, #24940, #14157, #43365, #25174, #39758, #27095, #12223, #40934, #41646, #8849, #8131, #34273, #19631, #29758, #44304, #7897, #4279, #33569, #687, #15340, #22754, #4512, #19088, #33758, #18621, #40413, #30171, #19576, #44711, #26555, #41112, #34684, #9026, #36027, #8788, #12880, #45192, #23890, #5187, #17574, #24135, #12414, #2937, #13987, #28637, #23650, #1829, #27756, #27035, #45662, #21162, #3188, #46801, #19808, #27276, #41586, #16465, #31101, #38027, #41825, #34925, #43195, #34440, #38738, #27514, #10406, #1585, #16239, #30870, #5425, #35794, #45432, #42319, #38261, #13122, #9511, #42066, #6550, #20276, #32215, #25008, #9270, #38497, #5669, #39606, #2070, #6783, #21402, #30629, #31328, #45906, #14463, #3666, #7964, #36284, #29122, #14941, #29603, #21651, #4122, #36511, #21890, #7272, #43674, #22583, #43434, #14699, #32464, #11116, #39835, #18746, #11344, #47042, #36969, #521, #15179, #10884, #18290, #44145, #14234, #32931, #7725, #17817, #33404, #7026, #25504, #28876, #29374, #43913, #10642, #40072, #22109, #29822, #25247, #40535, #25735, #44368, #3436, #18049, #32695, #40307, #22341, #47285, #11575, #7489, #26202, #40768, #36736, #3894, #18521, #33173, #1708, #23057, #8666, #37429, #30745, #12536, #34556, #16355, #27398, #33636, #15888, #996, #30512, #750, #33877, #30291, #15411, #8191, #44843, #45073, #30237, #1660, #41418, #1414, #44547, #8616, #8862, #19644, #19163, #23254, #30698, #18921, #44788, #40709, #1182, #12001, #5258, #19878, #26621, #4290, #41176, #8376, #15351, #23006, #16306, #30934, #30003, #37618, #7909, #22525, #37141, #33580, #11765, #26385, #40944, #15842, #37369, #30465, #5736, #42829, #9581, #16995, #35226, #2597, #9101, #45737, #17231, #42603, #23722, #27349, #2134, #27583, #1899, #41892, #9345, #6191, #23964, #46446, #28265, #20815, #31866, #20581, #10042, #2361, #31635, #46212, #28044, #9815, #24660, #6429, #21046, #35688, #17455, #44028, #32343, #3559, #22222, #4008, #36401, #3784, #25379, #36159, #39716, #32090, #28510, #43082, #3314, #47168, #39956, #10285, #36623, #24894, #39492, #10998, #21283, #6900, #21998, #7147, #14112, #25616, #40191, #28756, #10527, #32581, #18172, #44725, #633, #22704, #37555, #1121, #35375, #43243, #2519, #25043, #13108, #6821, #16689, #17145, #27739, #31789, #42305, #18091, #21930, #39881, #15220, #18334, #4168, #28914, #43719, #22387, #36550, #33448, #47332, #14503, #36782, #36325, #3479, #40580, #3711, #7065, #14275, #40810, #36068, #564, #21693, #43958, #7537, #37014, #43477, #7311, #44410, #32737, #29165, #18561, #10924, #32972, #14743, #11157, #10685, #22149, #11628, #3938, #26247, #33218, #342, #14991, #29643, #44184, #12100, #22871, #34153, #45597, #4392, #4636, #15462, #37965, #34376, #27449, #8479, #37727, #1515, #30112, #26961, #1046, #16168, #41759, #19975, #15703, #26724, #30802, #41279, #4881, #8962, #1281, #15937, #33686, #41992, #22635, #5352, #41514, #8719, #45368, #12583, #19022, #23582, #34614, #1763, #797, #11860, #24064, #9450, #6057, #27684, #13974, #28625, #46549, #27913, #6536, #28371, #42246, #23814, #13506, #16854, #31497, #38673, #20685, #17562, #38433, #5841, #2004, #9912, #6295, #46786, #42478, #24297, #20917, #16630, #17091, #20449, #35556, #42941, #39354, #17328, #31964, #31729, #13732, #9682, #42696, #46080, #45839, #38896, #13048, #10150, #21150, #35325, #5600, #35785, #13282, #28138, #32200, #9196, #46322, #34858, #2464, #24522, #39123, #31261, #15166, #43182, #14451, #10871, #7256, #39592, #282, #24996, #14927, #43901, #33392, #36270, #33161, #21879, #11333, #36723, #11100, #29592, #47027, #18733, #36014, #29109, #10391, #508, #36958, #6773, #14221, #38, #28862, #36499, #21389, #18506, #3885, #10630, #44135, #25490, #25944, #25232, #43662, #32451, #22329, #40057, #40523, #3172, #3421, #7713, #3654, #17801, #39821, #14686, #4113, #43421, #7010, #18276, #21636, #18037, #32683, #47272, #32918, #29359, #40292, #7477, #22097, #12276, #41453, #26426, #26895, #19441, #8654, #27145, #982, #37663, #15400, #23290, #4818, #37904, #41697, #16110, #34544, #44830, #40993, #15641, #19913, #739, #8179, #5062, #19679, #33624, #30735, #30276, #1696, #15875, #34321, #30044, #1452, #45304, #12523, #37413, #8899, #23531, #37186, #33864, #29811, #34092, #12041, #38133, #5295, #26663, #22571, #41212, #8416, #44589, #23044, #44356, #11564, #11806, #1221, #26189, #40756, #7953, #4330, #18964, #22804, #45062, #4571, #19205, #30500, #24003, #28304, #27856, #35267, #6000, #2636, #27386, #16571, #6229, #13449, #41930, #16345, #38601, #45773, #38363, #12756, #23754, #24462, #9138, #17269, #20382, #5776, #42174, #21089, #5537, #46015, #30966, #9618, #20149, #31905, #9850, #45533, #46487, #42872, #10083, #9383, #35024, #28078, #34796, #31434, #24695, #35728, #39295, #1936, #12983, #31201, #2172, #16795, #6469, #42414, #27622, #13223, #24237, #2402, #38834, #20620, #17035, #31672, #46251, #42640, #39061, #33028, #14805, #42804, #14090 ) ),
 .UNSPECIFIED., .F., .F., .T. ) 
 B_SPLINE_SURFACE_WITH_KNOTS ( ( 2, 2 ),
 ( 3, 2, 2, 2, 2, 2, 2, 2, 2, 2, 2, 2, 2, 2, 2, 2, 2, 2, 2, 2, 2, 2, 2, 2, 2, 2, 2, 2, 2, 2, 2, 2, 2, 2, 2, 2, 2, 2, 2, 2, 2, 2, 2, 2, 2, 2, 2, 2, 2, 2, 2, 2, 2, 2, 2, 2, 2, 2, 2, 2, 2, 2, 2, 2, 2, 2, 2, 2, 2, 2, 2, 2, 2, 2, 2, 2, 2, 2, 2, 2, 2, 2, 2, 2, 2, 2, 2, 2, 2, 2, 2, 2, 2, 2, 2, 2, 2, 2, 2, 2, 2, 2, 2, 2, 2, 2, 2, 2, 2, 2, 2, 2, 2, 2, 2, 2, 2, 2, 2, 2, 2, 2, 2, 2, 2, 2, 2, 2, 2, 2, 2, 2, 2, 2, 2, 2, 2, 2, 2, 2, 2, 2, 2, 2, 2, 2, 2, 2, 2, 2, 2, 2, 2, 2, 2, 2, 2, 2, 2, 2, 2, 2, 2, 2, 2, 2, 2, 2, 2, 2, 2, 2, 2, 2, 2, 2, 2, 2, 2, 2, 2, 2, 2, 2, 2, 2, 2, 2, 2, 2, 2, 2, 2, 2, 2, 2, 2, 2, 2, 2, 2, 2, 2, 2, 2, 2, 2, 2, 2, 2, 2, 2, 2, 2, 2, 2, 2, 2, 2, 2, 2, 2, 2, 2, 2, 2, 2, 2, 2, 2, 2, 2, 2, 2, 2, 2, 2, 2, 2, 2, 2, 2, 2, 2, 2, 2, 2, 2, 2, 2, 2, 2, 2, 2, 2, 2, 2, 2, 2, 2, 2, 2, 2, 2, 2, 2, 2, 2, 2, 2, 2, 2, 2, 2, 2, 2, 2, 2, 2, 2, 2, 2, 2, 2, 2, 2, 2, 2, 2, 2, 2, 2, 2, 2, 2, 2, 2, 2, 2, 2, 2, 2, 2, 2, 2, 2, 2, 2, 2, 2, 2, 2, 2, 2, 2, 2, 2, 2, 2, 2, 2, 2, 2, 2, 2, 2, 2, 2, 2, 2, 2, 2, 2, 2, 2, 2, 2, 2, 2, 2, 2, 2, 2, 2, 2, 2, 2, 2, 2, 2, 2, 2, 2, 2, 2, 2, 2, 2, 2, 2, 2, 2, 2, 2, 2, 2, 2, 2, 2, 2, 2, 2, 2, 2, 2, 2, 2, 2, 2, 2, 2, 2, 2, 2, 2, 2, 2, 2, 2, 2, 2, 2, 2, 2, 2, 2, 2, 2, 2, 2, 3 ),
 ( 0.000000000000000000, 1.000000000000000000 ),
 ( 0.000000000000000000, 0.002500000000000000052, 0.005000000000000000104, 0.007499999999999999722, 0.01000000000000000021, 0.01250000000000000069, 0.01499999999999999944, 0.01750000000000000167, 0.02000000000000000042, 0.02249999999999999917, 0.02500000000000000139, 0.02750000000000000014, 0.02999999999999999889, 0.03250000000000000111, 0.03500000000000000333, 0.03749999999999999861, 0.04000000000000000083, 0.04250000000000000305, 0.04499999999999999833, 0.04750000000000000056, 0.05000000000000000278, 0.05249999999999999806, 0.05500000000000000028, 0.05750000000000000250, 0.05999999999999999778, 0.06250000000000000000, 0.06500000000000000222, 0.06750000000000000444, 0.07000000000000000666, 0.07249999999999999500, 0.07499999999999999722, 0.07749999999999999944, 0.08000000000000000167, 0.08250000000000000389, 0.08500000000000000611, 0.08749999999999999445, 0.08999999999999999667, 0.09249999999999999889, 0.09500000000000000111, 0.09750000000000000333, 0.1000000000000000056, 0.1024999999999999939, 0.1049999999999999961, 0.1074999999999999983, 0.1100000000000000006, 0.1125000000000000028, 0.1150000000000000050, 0.1174999999999999933, 0.1199999999999999956, 0.1224999999999999978, 0.1250000000000000000, 0.1275000000000000022, 0.1300000000000000044, 0.1325000000000000067, 0.1350000000000000089, 0.1375000000000000111, 0.1400000000000000133, 0.1424999999999999878, 0.1449999999999999900, 0.1474999999999999922, 0.1499999999999999944, 0.1524999999999999967, 0.1549999999999999989, 0.1575000000000000011, 0.1600000000000000033, 0.1625000000000000056, 0.1650000000000000078, 0.1675000000000000100, 0.1700000000000000122, 0.1724999999999999867, 0.1749999999999999889, 0.1774999999999999911, 0.1799999999999999933, 0.1824999999999999956, 0.1849999999999999978, 0.1875000000000000000, 0.1900000000000000022, 0.1925000000000000044, 0.1950000000000000067, 0.1975000000000000089, 0.2000000000000000111, 0.2025000000000000133, 0.2049999999999999878, 0.2074999999999999900, 0.2099999999999999922, 0.2124999999999999944, 0.2149999999999999967, 0.2174999999999999989, 0.2200000000000000011, 0.2225000000000000033, 0.2250000000000000056, 0.2275000000000000078, 0.2300000000000000100, 0.2325000000000000122, 0.2349999999999999867, 0.2374999999999999889, 0.2399999999999999911, 0.2424999999999999933, 0.2449999999999999956, 0.2474999999999999978, 0.2500000000000000000, 0.2525000000000000022, 0.2550000000000000044, 0.2575000000000000067, 0.2600000000000000089, 0.2625000000000000111, 0.2650000000000000133, 0.2675000000000000155, 0.2700000000000000178, 0.2725000000000000200, 0.2750000000000000222, 0.2775000000000000244, 0.2800000000000000266, 0.2824999999999999734, 0.2849999999999999756, 0.2874999999999999778, 0.2899999999999999800, 0.2924999999999999822, 0.2949999999999999845, 0.2974999999999999867, 0.2999999999999999889, 0.3024999999999999911, 0.3049999999999999933, 0.3074999999999999956, 0.3099999999999999978, 0.3125000000000000000, 0.3150000000000000022, 0.3175000000000000044, 0.3200000000000000067, 0.3225000000000000089, 0.3250000000000000111, 0.3275000000000000133, 0.3300000000000000155, 0.3325000000000000178, 0.3350000000000000200, 0.3375000000000000222, 0.3400000000000000244, 0.3425000000000000266, 0.3449999999999999734, 0.3474999999999999756, 0.3499999999999999778, 0.3524999999999999800, 0.3549999999999999822, 0.3574999999999999845, 0.3599999999999999867, 0.3624999999999999889, 0.3649999999999999911, 0.3674999999999999933, 0.3699999999999999956, 0.3724999999999999978, 0.3750000000000000000, 0.3775000000000000022, 0.3800000000000000044, 0.3825000000000000067, 0.3850000000000000089, 0.3875000000000000111, 0.3900000000000000133, 0.3925000000000000155, 0.3950000000000000178, 0.3975000000000000200, 0.4000000000000000222, 0.4025000000000000244, 0.4050000000000000266, 0.4074999999999999734, 0.4099999999999999756, 0.4124999999999999778, 0.4149999999999999800, 0.4174999999999999822, 0.4199999999999999845, 0.4224999999999999867, 0.4249999999999999889, 0.4274999999999999911, 0.4299999999999999933, 0.4324999999999999956, 0.4349999999999999978, 0.4375000000000000000, 0.4400000000000000022, 0.4425000000000000044, 0.4450000000000000067, 0.4475000000000000089, 0.4500000000000000111, 0.4525000000000000133, 0.4550000000000000155, 0.4575000000000000178, 0.4600000000000000200, 0.4625000000000000222, 0.4650000000000000244, 0.4675000000000000266, 0.4699999999999999734, 0.4724999999999999756, 0.4749999999999999778, 0.4774999999999999800, 0.4799999999999999822, 0.4824999999999999845, 0.4849999999999999867, 0.4874999999999999889, 0.4899999999999999911, 0.4924999999999999933, 0.4949999999999999956, 0.4974999999999999978, 0.5000000000000000000, 0.5024999999999999467, 0.5050000000000000044, 0.5074999999999999512, 0.5100000000000000089, 0.5124999999999999556, 0.5150000000000000133, 0.5174999999999999600, 0.5200000000000000178, 0.5224999999999999645, 0.5250000000000000222, 0.5274999999999999689, 0.5300000000000000266, 0.5324999999999999734, 0.5350000000000000311, 0.5374999999999999778, 0.5400000000000000355, 0.5424999999999999822, 0.5450000000000000400, 0.5474999999999999867, 0.5500000000000000444, 0.5524999999999999911, 0.5550000000000000488, 0.5574999999999999956, 0.5600000000000000533, 0.5625000000000000000, 0.5649999999999999467, 0.5675000000000000044, 0.5699999999999999512, 0.5725000000000000089, 0.5749999999999999556, 0.5775000000000000133, 0.5799999999999999600, 0.5825000000000000178, 0.5849999999999999645, 0.5875000000000000222, 0.5899999999999999689, 0.5925000000000000266, 0.5949999999999999734, 0.5975000000000000311, 0.5999999999999999778, 0.6025000000000000355, 0.6049999999999999822, 0.6075000000000000400, 0.6099999999999999867, 0.6125000000000000444, 0.6149999999999999911, 0.6175000000000000488, 0.6199999999999999956, 0.6225000000000000533, 0.6250000000000000000, 0.6274999999999999467, 0.6300000000000000044, 0.6324999999999999512, 0.6350000000000000089, 0.6374999999999999556, 0.6400000000000000133, 0.6424999999999999600, 0.6450000000000000178, 0.6474999999999999645, 0.6500000000000000222, 0.6524999999999999689, 0.6550000000000000266, 0.6574999999999999734, 0.6600000000000000311, 0.6624999999999999778, 0.6650000000000000355, 0.6674999999999999822, 0.6700000000000000400, 0.6724999999999999867, 0.6750000000000000444, 0.6774999999999999911, 0.6800000000000000488, 0.6824999999999999956, 0.6850000000000000533, 0.6875000000000000000, 0.6899999999999999467, 0.6925000000000000044, 0.6949999999999999512, 0.6975000000000000089, 0.6999999999999999556, 0.7025000000000000133, 0.7049999999999999600, 0.7075000000000000178, 0.7099999999999999645, 0.7125000000000000222, 0.7149999999999999689, 0.7175000000000000266, 0.7199999999999999734, 0.7225000000000000311, 0.7249999999999999778, 0.7275000000000000355, 0.7299999999999999822, 0.7325000000000000400, 0.7349999999999999867, 0.7375000000000000444, 0.7399999999999999911, 0.7425000000000000488, 0.7449999999999999956, 0.7475000000000000533, 0.7500000000000000000, 0.7524999999999999467, 0.7550000000000000044, 0.7574999999999999512, 0.7600000000000000089, 0.7624999999999999556, 0.7650000000000000133, 0.7674999999999999600, 0.7700000000000000178, 0.7724999999999999645, 0.7750000000000000222, 0.7774999999999999689, 0.7800000000000000266, 0.7824999999999999734, 0.7850000000000000311, 0.7874999999999999778, 0.7900000000000000355, 0.7924999999999999822, 0.7950000000000000400, 0.7974999999999999867, 0.8000000000000000444, 0.8024999999999999911, 0.8050000000000000488, 0.8074999999999999956, 0.8100000000000000533, 0.8125000000000000000, 0.8149999999999999467, 0.8175000000000000044, 0.8199999999999999512, 0.8225000000000000089, 0.8249999999999999556, 0.8275000000000000133, 0.8299999999999999600, 0.8325000000000000178, 0.8349999999999999645, 0.8375000000000000222, 0.8399999999999999689, 0.8425000000000000266, 0.8449999999999999734, 0.8475000000000000311, 0.8499999999999999778, 0.8525000000000000355, 0.8549999999999999822, 0.8575000000000000400, 0.8599999999999999867, 0.8625000000000000444, 0.8649999999999999911, 0.8675000000000000488, 0.8699999999999999956, 0.8725000000000000533, 0.8750000000000000000, 0.8774999999999999467, 0.8800000000000000044, 0.8824999999999999512, 0.8850000000000000089, 0.8874999999999999556, 0.8900000000000000133, 0.8924999999999999600, 0.8950000000000000178, 0.8974999999999999645, 0.9000000000000000222, 0.9024999999999999689, 0.9050000000000000266, 0.9074999999999999734, 0.9100000000000000311, 0.9124999999999999778, 0.9150000000000000355, 0.9174999999999999822, 0.9200000000000000400, 0.9224999999999999867, 0.9250000000000000444, 0.9274999999999999911, 0.9300000000000000488, 0.9324999999999999956, 0.9350000000000000533, 0.9375000000000000000, 0.9399999999999999467, 0.9425000000000000044, 0.9449999999999999512, 0.9475000000000000089, 0.9499999999999999556, 0.9525000000000000133, 0.9549999999999999600, 0.9575000000000000178, 0.9599999999999999645, 0.9625000000000000222, 0.9649999999999999689, 0.9675000000000000266, 0.9699999999999999734, 0.9725000000000000311, 0.9749999999999999778, 0.9775000000000000355, 0.9799999999999999822, 0.9825000000000000400, 0.9849999999999999867, 0.9875000000000000444, 0.9899999999999999911, 0.9925000000000000488, 0.9949999999999999956, 0.9975000000000000533, 1.000000000000000000 ),
 .UNSPECIFIED. ) 
 GEOMETRIC_REPRESENTATION_ITEM ( )  RATIONAL_B_SPLINE_SURFACE ( (
 ( 1.000000000000000000, 0.9238795325112869605, 1.000000000000000000, 0.9238795325112869605, 1.000000000000000000, 0.9238795325112869605, 1.000000000000000000, 0.9238795325112869605, 1.000000000000000000, 0.9238795325112869605, 1.000000000000000000, 0.9238795325112869605, 1.000000000000000000, 0.9238795325112869605, 1.000000000000000000, 0.9238795325112869605, 1.000000000000000000, 0.9238795325112869605, 1.000000000000000000, 0.9238795325112869605, 1.000000000000000000, 0.9238795325112869605, 1.000000000000000000, 0.9238795325112869605, 1.000000000000000000, 0.9238795325112869605, 1.000000000000000000, 0.9238795325112869605, 1.000000000000000000, 0.9238795325112869605, 1.000000000000000000, 0.9238795325112869605, 1.000000000000000000, 0.9238795325112869605, 1.000000000000000000, 0.9238795325112869605, 1.000000000000000000, 0.9238795325112869605, 1.000000000000000000, 0.9238795325112869605, 1.000000000000000000, 0.9238795325112869605, 1.000000000000000000, 0.9238795325112869605, 1.000000000000000000, 0.9238795325112869605, 1.000000000000000000, 0.9238795325112869605, 1.000000000000000000, 0.9238795325112869605, 1.000000000000000000, 0.9238795325112869605, 1.000000000000000000, 0.9238795325112869605, 1.000000000000000000, 0.9238795325112869605, 1.000000000000000000, 0.9238795325112869605, 1.000000000000000000, 0.9238795325112869605, 1.000000000000000000, 0.9238795325112869605, 1.000000000000000000, 0.9238795325112869605, 1.000000000000000000, 0.9238795325112869605, 1.000000000000000000, 0.9238795325112869605, 1.000000000000000000, 0.9238795325112869605, 1.000000000000000000, 0.9238795325112869605, 1.000000000000000000, 0.9238795325112869605, 1.000000000000000000, 0.9238795325112869605, 1.000000000000000000, 0.9238795325112869605, 1.000000000000000000, 0.9238795325112869605, 1.000000000000000000, 0.9238795325112869605, 1.000000000000000000, 0.9238795325112869605, 1.000000000000000000, 0.9238795325112869605, 1.000000000000000000, 0.9238795325112869605, 1.000000000000000000, 0.9238795325112869605, 1.000000000000000000, 0.9238795325112869605, 1.000000000000000000, 0.9238795325112869605, 1.000000000000000000, 0.9238795325112869605, 1.000000000000000000, 0.9238795325112869605, 1.000000000000000000, 0.9238795325112869605, 1.000000000000000000, 0.9238795325112869605, 1.000000000000000000, 0.9238795325112869605, 1.000000000000000000, 0.9238795325112869605, 1.000000000000000000, 0.9238795325112869605, 1.000000000000000000, 0.9238795325112869605, 1.000000000000000000, 0.9238795325112869605, 1.000000000000000000, 0.9238795325112869605, 1.000000000000000000, 0.9238795325112869605, 1.000000000000000000, 0.9238795325112869605, 1.000000000000000000, 0.9238795325112869605, 1.000000000000000000, 0.9238795325112869605, 1.000000000000000000, 0.9238795325112869605, 1.000000000000000000, 0.9238795325112869605, 1.000000000000000000, 0.9238795325112869605, 1.000000000000000000, 0.9238795325112869605, 1.000000000000000000, 0.9238795325112869605, 1.000000000000000000, 0.9238795325112869605, 1.000000000000000000, 0.9238795325112869605, 1.000000000000000000, 0.9238795325112869605, 1.000000000000000000, 0.9238795325112869605, 1.000000000000000000, 0.9238795325112869605, 1.000000000000000000, 0.9238795325112869605, 1.000000000000000000, 0.9238795325112869605, 1.000000000000000000, 0.9238795325112869605, 1.000000000000000000, 0.9238795325112869605, 1.000000000000000000, 0.9238795325112869605, 1.000000000000000000, 0.9238795325112869605, 1.000000000000000000, 0.9238795325112869605, 1.000000000000000000, 0.9238795325112869605, 1.000000000000000000, 0.9238795325112869605, 1.000000000000000000, 0.9238795325112869605, 1.000000000000000000, 0.9238795325112869605, 1.000000000000000000, 0.9238795325112869605, 1.000000000000000000, 0.9238795325112869605, 1.000000000000000000, 0.9238795325112869605, 1.000000000000000000, 0.9238795325112869605, 1.000000000000000000, 0.9238795325112869605, 1.000000000000000000, 0.9238795325112869605, 1.000000000000000000, 0.9238795325112869605, 1.000000000000000000, 0.9238795325112869605, 1.000000000000000000, 0.9238795325112869605, 1.000000000000000000, 0.9238795325112869605, 1.000000000000000000, 0.9238795325112869605, 1.000000000000000000, 0.9238795325112869605, 1.000000000000000000, 0.9238795325112869605, 1.000000000000000000, 0.9238795325112869605, 1.000000000000000000, 0.9238795325112869605, 1.000000000000000000, 0.9238795325112869605, 1.000000000000000000, 0.9238795325112869605, 1.000000000000000000, 0.9238795325112869605, 1.000000000000000000, 0.9238795325112869605, 1.000000000000000000, 0.9238795325112869605, 1.000000000000000000, 0.9238795325112869605, 1.000000000000000000, 0.9238795325112869605, 1.000000000000000000, 0.9238795325112869605, 1.000000000000000000, 0.9238795325112869605, 1.000000000000000000, 0.9238795325112869605, 1.000000000000000000, 0.9238795325112869605, 1.000000000000000000, 0.9238795325112869605, 1.000000000000000000, 0.9238795325112869605, 1.000000000000000000, 0.9238795325112869605, 1.000000000000000000, 0.9238795325112869605, 1.000000000000000000, 0.9238795325112869605, 1.000000000000000000, 0.9238795325112869605, 1.000000000000000000, 0.9238795325112869605, 1.000000000000000000, 0.9238795325112869605, 1.000000000000000000, 0.9238795325112869605, 1.000000000000000000, 0.9238795325112869605, 1.000000000000000000, 0.9238795325112869605, 1.000000000000000000, 0.9238795325112869605, 1.000000000000000000, 0.9238795325112869605, 1.000000000000000000, 0.9238795325112869605, 1.000000000000000000, 0.9238795325112869605, 1.000000000000000000, 0.9238795325112869605, 1.000000000000000000, 0.9238795325112869605, 1.000000000000000000, 0.9238795325112869605, 1.000000000000000000, 0.9238795325112869605, 1.000000000000000000, 0.9238795325112869605, 1.000000000000000000, 0.9238795325112869605, 1.000000000000000000, 0.9238795325112869605, 1.000000000000000000, 0.9238795325112869605, 1.000000000000000000, 0.9238795325112869605, 1.000000000000000000, 0.9238795325112869605, 1.000000000000000000, 0.9238795325112869605, 1.000000000000000000, 0.9238795325112869605, 1.000000000000000000, 0.9238795325112869605, 1.000000000000000000, 0.9238795325112869605, 1.000000000000000000, 0.9238795325112869605, 1.000000000000000000, 0.9238795325112869605, 1.000000000000000000, 0.9238795325112869605, 1.000000000000000000, 0.9238795325112869605, 1.000000000000000000, 0.9238795325112869605, 1.000000000000000000, 0.9238795325112869605, 1.000000000000000000, 0.9238795325112869605, 1.000000000000000000, 0.9238795325112869605, 1.000000000000000000, 0.9238795325112869605, 1.000000000000000000, 0.9238795325112869605, 1.000000000000000000, 0.9238795325112869605, 1.000000000000000000, 0.9238795325112869605, 1.000000000000000000, 0.9238795325112869605, 1.000000000000000000, 0.9238795325112869605, 1.000000000000000000, 0.9238795325112869605, 1.000000000000000000, 0.9238795325112869605, 1.000000000000000000, 0.9238795325112869605, 1.000000000000000000, 0.9238795325112869605, 1.000000000000000000, 0.9238795325112869605, 1.000000000000000000, 0.9238795325112869605, 1.000000000000000000, 0.9238795325112869605, 1.000000000000000000, 0.9238795325112869605, 1.000000000000000000, 0.9238795325112869605, 1.000000000000000000, 0.9238795325112869605, 1.000000000000000000, 0.9238795325112869605, 1.000000000000000000, 0.9238795325112869605, 1.000000000000000000, 0.9238795325112869605, 1.000000000000000000, 0.9238795325112869605, 1.000000000000000000, 0.9238795325112869605, 1.000000000000000000, 0.9238795325112869605, 1.000000000000000000, 0.9238795325112869605, 1.000000000000000000, 0.9238795325112869605, 1.000000000000000000, 0.9238795325112869605, 1.000000000000000000, 0.9238795325112869605, 1.000000000000000000, 0.9238795325112869605, 1.000000000000000000, 0.9238795325112869605, 1.000000000000000000, 0.9238795325112869605, 1.000000000000000000, 0.9238795325112869605, 1.000000000000000000, 0.9238795325112869605, 1.000000000000000000, 0.9238795325112869605, 1.000000000000000000, 0.9238795325112869605, 1.000000000000000000, 0.9238795325112869605, 1.000000000000000000, 0.9238795325112869605, 1.000000000000000000, 0.9238795325112869605, 1.000000000000000000, 0.9238795325112869605, 1.000000000000000000, 0.9238795325112869605, 1.000000000000000000, 0.9238795325112869605, 1.000000000000000000, 0.9238795325112869605, 1.000000000000000000, 0.9238795325112869605, 1.000000000000000000, 0.9238795325112869605, 1.000000000000000000, 0.9238795325112869605, 1.000000000000000000, 0.9238795325112869605, 1.000000000000000000, 0.9238795325112869605, 1.000000000000000000, 0.9238795325112869605, 1.000000000000000000, 0.9238795325112869605, 1.000000000000000000, 0.9238795325112869605, 1.000000000000000000, 0.9238795325112869605, 1.000000000000000000, 0.9238795325112869605, 1.000000000000000000, 0.9238795325112869605, 1.000000000000000000, 0.9238795325112869605, 1.000000000000000000, 0.9238795325112869605, 1.000000000000000000, 0.9238795325112869605, 1.000000000000000000, 0.9238795325112869605, 1.000000000000000000, 0.9238795325112869605, 1.000000000000000000, 0.9238795325112869605, 1.000000000000000000, 0.9238795325112869605, 1.000000000000000000, 0.9238795325112869605, 1.000000000000000000, 0.9238795325112869605, 1.000000000000000000, 0.9238795325112869605, 1.000000000000000000, 0.9238795325112869605, 1.000000000000000000, 0.9238795325112869605, 1.000000000000000000, 0.9238795325112869605, 1.000000000000000000, 0.9238795325112869605, 1.000000000000000000, 0.9238795325112869605, 1.000000000000000000, 0.9238795325112869605, 1.000000000000000000, 0.9238795325112869605, 1.000000000000000000, 0.9238795325112869605, 1.000000000000000000, 0.9238795325112869605, 1.000000000000000000, 0.9238795325112869605, 1.000000000000000000, 0.9238795325112869605, 1.000000000000000000, 0.9238795325112869605, 1.000000000000000000, 0.9238795325112869605, 1.000000000000000000, 0.9238795325112869605, 1.000000000000000000, 0.9238795325112869605, 1.000000000000000000, 0.9238795325112869605, 1.000000000000000000, 0.9238795325112869605, 1.000000000000000000, 0.9238795325112869605, 1.000000000000000000, 0.9238795325112869605, 1.000000000000000000, 0.9238795325112869605, 1.000000000000000000, 0.9238795325112869605, 1.000000000000000000, 0.9238795325112869605, 1.000000000000000000, 0.9238795325112869605, 1.000000000000000000, 0.9238795325112869605, 1.000000000000000000, 0.9238795325112869605, 1.000000000000000000, 0.9238795325112869605, 1.000000000000000000, 0.9238795325112869605, 1.000000000000000000, 0.9238795325112869605, 1.000000000000000000, 0.9238795325112869605, 1.000000000000000000, 0.9238795325112869605, 1.000000000000000000, 0.9238795325112869605, 1.000000000000000000, 0.9238795325112869605, 1.000000000000000000, 0.9238795325112869605, 1.000000000000000000, 0.9238795325112869605, 1.000000000000000000, 0.9238795325112869605, 1.000000000000000000, 0.9238795325112869605, 1.000000000000000000, 0.9238795325112869605, 1.000000000000000000, 0.9238795325112869605, 1.000000000000000000, 0.9238795325112869605, 1.000000000000000000, 0.9238795325112869605, 1.000000000000000000, 0.9238795325112869605, 1.000000000000000000, 0.9238795325112869605, 1.000000000000000000, 0.9238795325112869605, 1.000000000000000000, 0.9238795325112869605, 1.000000000000000000, 0.9238795325112869605, 1.000000000000000000, 0.9238795325112869605, 1.000000000000000000, 0.9238795325112869605, 1.000000000000000000, 0.9238795325112869605, 1.000000000000000000, 0.9238795325112869605, 1.000000000000000000, 0.9238795325112869605, 1.000000000000000000, 0.9238795325112869605, 1.000000000000000000, 0.9238795325112869605, 1.000000000000000000, 0.9238795325112869605, 1.000000000000000000, 0.9238795325112869605, 1.000000000000000000, 0.9238795325112869605, 1.000000000000000000, 0.9238795325112869605, 1.000000000000000000, 0.9238795325112869605, 1.000000000000000000, 0.9238795325112869605, 1.000000000000000000, 0.9238795325112869605, 1.000000000000000000, 0.9238795325112869605, 1.000000000000000000, 0.9238795325112869605, 1.000000000000000000, 0.9238795325112869605, 1.000000000000000000, 0.9238795325112869605, 1.000000000000000000, 0.9238795325112869605, 1.000000000000000000, 0.9238795325112869605, 1.000000000000000000, 0.9238795325112869605, 1.000000000000000000, 0.9238795325112869605, 1.000000000000000000, 0.9238795325112869605, 1.000000000000000000, 0.9238795325112869605, 1.000000000000000000, 0.9238795325112869605, 1.000000000000000000, 0.9238795325112869605, 1.000000000000000000, 0.9238795325112869605, 1.000000000000000000, 0.9238795325112869605, 1.000000000000000000, 0.9238795325112869605, 1.000000000000000000, 0.9238795325112869605, 1.000000000000000000, 0.9238795325112869605, 1.000000000000000000, 0.9238795325112869605, 1.000000000000000000, 0.9238795325112869605, 1.000000000000000000, 0.9238795325112869605, 1.000000000000000000, 0.9238795325112869605, 1.000000000000000000, 0.9238795325112869605, 1.000000000000000000, 0.9238795325112869605, 1.000000000000000000, 0.9238795325112869605, 1.000000000000000000, 0.9238795325112869605, 1.000000000000000000, 0.9238795325112869605, 1.000000000000000000, 0.9238795325112869605, 1.000000000000000000, 0.9238795325112869605, 1.000000000000000000, 0.9238795325112869605, 1.000000000000000000, 0.9238795325112869605, 1.000000000000000000, 0.9238795325112869605, 1.000000000000000000, 0.9238795325112869605, 1.000000000000000000, 0.9238795325112869605, 1.000000000000000000, 0.9238795325112869605, 1.000000000000000000, 0.9238795325112869605, 1.000000000000000000, 0.9238795325112869605, 1.000000000000000000, 0.9238795325112869605, 1.000000000000000000, 0.9238795325112869605, 1.000000000000000000, 0.9238795325112869605, 1.000000000000000000, 0.9238795325112869605, 1.000000000000000000, 0.9238795325112869605, 1.000000000000000000, 0.9238795325112869605, 1.000000000000000000, 0.9238795325112869605, 1.000000000000000000, 0.9238795325112869605, 1.000000000000000000, 0.9238795325112869605, 1.000000000000000000, 0.9238795325112869605, 1.000000000000000000, 0.9238795325112869605, 1.000000000000000000, 0.9238795325112869605, 1.000000000000000000, 0.9238795325112869605, 1.000000000000000000, 0.9238795325112869605, 1.000000000000000000, 0.9238795325112869605, 1.000000000000000000, 0.9238795325112869605, 1.000000000000000000, 0.9238795325112869605, 1.000000000000000000, 0.9238795325112869605, 1.000000000000000000, 0.9238795325112869605, 1.000000000000000000, 0.9238795325112869605, 1.000000000000000000, 0.9238795325112869605, 1.000000000000000000, 0.9238795325112869605, 1.000000000000000000, 0.9238795325112869605, 1.000000000000000000, 0.9238795325112869605, 1.000000000000000000, 0.9238795325112869605, 1.000000000000000000, 0.9238795325112869605, 1.000000000000000000, 0.9238795325112869605, 1.000000000000000000, 0.9238795325112869605, 1.000000000000000000, 0.9238795325112869605, 1.000000000000000000, 0.9238795325112869605, 1.000000000000000000, 0.9238795325112869605, 1.000000000000000000, 0.9238795325112869605, 1.000000000000000000, 0.9238795325112869605, 1.000000000000000000, 0.9238795325112869605, 1.000000000000000000, 0.9238795325112869605, 1.000000000000000000, 0.9238795325112869605, 1.000000000000000000, 0.9238795325112869605, 1.000000000000000000, 0.9238795325112869605, 1.000000000000000000, 0.9238795325112869605, 1.000000000000000000, 0.9238795325112869605, 1.000000000000000000, 0.9238795325112869605, 1.000000000000000000, 0.9238795325112869605, 1.000000000000000000, 0.9238795325112869605, 1.000000000000000000, 0.9238795325112869605, 1.000000000000000000, 0.9238795325112869605, 1.000000000000000000, 0.9238795325112869605, 1.000000000000000000, 0.9238795325112869605, 1.000000000000000000, 0.9238795325112869605, 1.000000000000000000, 0.9238795325112869605, 1.000000000000000000, 0.9238795325112869605, 1.000000000000000000, 0.9238795325112869605, 1.000000000000000000, 0.9238795325112869605, 1.000000000000000000, 0.9238795325112869605, 1.000000000000000000, 0.9238795325112869605, 1.000000000000000000, 0.9238795325112869605, 1.000000000000000000, 0.9238795325112869605, 1.000000000000000000, 0.9238795325112869605, 1.000000000000000000, 0.9238795325112869605, 1.000000000000000000, 0.9238795325112869605, 1.000000000000000000, 0.9238795325112869605, 1.000000000000000000, 0.9238795325112869605, 1.000000000000000000, 0.9238795325112869605, 1.000000000000000000, 0.9238795325112869605, 1.000000000000000000, 0.9238795325112869605, 1.000000000000000000, 0.9238795325112869605, 1.000000000000000000, 0.9238795325112869605, 1.000000000000000000, 0.9238795325112869605, 1.000000000000000000, 0.9238795325112869605, 1.000000000000000000, 0.9238795325112869605, 1.000000000000000000, 0.9238795325112869605, 1.000000000000000000, 0.9238795325112869605, 1.000000000000000000, 0.9238795325112869605, 1.000000000000000000, 0.9238795325112869605, 1.000000000000000000, 0.9238795325112869605, 1.000000000000000000, 0.9238795325112869605, 1.000000000000000000, 0.9238795325112869605, 1.000000000000000000, 0.9238795325112869605, 1.000000000000000000, 0.9238795325112869605, 1.000000000000000000, 0.9238795325112869605, 1.000000000000000000, 0.9238795325112869605, 1.000000000000000000, 0.9238795325112869605, 1.000000000000000000, 0.9238795325112869605, 1.000000000000000000, 0.9238795325112869605, 1.000000000000000000, 0.9238795325112869605, 1.000000000000000000, 0.9238795325112869605, 1.000000000000000000, 0.9238795325112869605, 1.000000000000000000, 0.9238795325112869605, 1.000000000000000000, 0.9238795325112869605, 1.000000000000000000, 0.9238795325112869605, 1.000000000000000000, 0.9238795325112869605, 1.000000000000000000, 0.9238795325112869605, 1.000000000000000000, 0.9238795325112869605, 1.000000000000000000, 0.9238795325112869605, 1.000000000000000000, 0.9238795325112869605, 1.000000000000000000, 0.9238795325112869605, 1.000000000000000000, 0.9238795325112869605, 1.000000000000000000, 0.9238795325112869605, 1.000000000000000000, 0.9238795325112869605, 1.000000000000000000, 0.9238795325112869605, 1.000000000000000000),
 ( 1.000000000000000000, 0.9238795325112869605, 1.000000000000000000, 0.9238795325112869605, 1.000000000000000000, 0.9238795325112869605, 1.000000000000000000, 0.9238795325112869605, 1.000000000000000000, 0.9238795325112869605, 1.000000000000000000, 0.9238795325112869605, 1.000000000000000000, 0.9238795325112869605, 1.000000000000000000, 0.9238795325112869605, 1.000000000000000000, 0.9238795325112869605, 1.000000000000000000, 0.9238795325112869605, 1.000000000000000000, 0.9238795325112869605, 1.000000000000000000, 0.9238795325112869605, 1.000000000000000000, 0.9238795325112869605, 1.000000000000000000, 0.9238795325112869605, 1.000000000000000000, 0.9238795325112869605, 1.000000000000000000, 0.9238795325112869605, 1.000000000000000000, 0.9238795325112869605, 1.000000000000000000, 0.9238795325112869605, 1.000000000000000000, 0.9238795325112869605, 1.000000000000000000, 0.9238795325112869605, 1.000000000000000000, 0.9238795325112869605, 1.000000000000000000, 0.9238795325112869605, 1.000000000000000000, 0.9238795325112869605, 1.000000000000000000, 0.9238795325112869605, 1.000000000000000000, 0.9238795325112869605, 1.000000000000000000, 0.9238795325112869605, 1.000000000000000000, 0.9238795325112869605, 1.000000000000000000, 0.9238795325112869605, 1.000000000000000000, 0.9238795325112869605, 1.000000000000000000, 0.9238795325112869605, 1.000000000000000000, 0.9238795325112869605, 1.000000000000000000, 0.9238795325112869605, 1.000000000000000000, 0.9238795325112869605, 1.000000000000000000, 0.9238795325112869605, 1.000000000000000000, 0.9238795325112869605, 1.000000000000000000, 0.9238795325112869605, 1.000000000000000000, 0.9238795325112869605, 1.000000000000000000, 0.9238795325112869605, 1.000000000000000000, 0.9238795325112869605, 1.000000000000000000, 0.9238795325112869605, 1.000000000000000000, 0.9238795325112869605, 1.000000000000000000, 0.9238795325112869605, 1.000000000000000000, 0.9238795325112869605, 1.000000000000000000, 0.9238795325112869605, 1.000000000000000000, 0.9238795325112869605, 1.000000000000000000, 0.9238795325112869605, 1.000000000000000000, 0.9238795325112869605, 1.000000000000000000, 0.9238795325112869605, 1.000000000000000000, 0.9238795325112869605, 1.000000000000000000, 0.9238795325112869605, 1.000000000000000000, 0.9238795325112869605, 1.000000000000000000, 0.9238795325112869605, 1.000000000000000000, 0.9238795325112869605, 1.000000000000000000, 0.9238795325112869605, 1.000000000000000000, 0.9238795325112869605, 1.000000000000000000, 0.9238795325112869605, 1.000000000000000000, 0.9238795325112869605, 1.000000000000000000, 0.9238795325112869605, 1.000000000000000000, 0.9238795325112869605, 1.000000000000000000, 0.9238795325112869605, 1.000000000000000000, 0.9238795325112869605, 1.000000000000000000, 0.9238795325112869605, 1.000000000000000000, 0.9238795325112869605, 1.000000000000000000, 0.9238795325112869605, 1.000000000000000000, 0.9238795325112869605, 1.000000000000000000, 0.9238795325112869605, 1.000000000000000000, 0.9238795325112869605, 1.000000000000000000, 0.9238795325112869605, 1.000000000000000000, 0.9238795325112869605, 1.000000000000000000, 0.9238795325112869605, 1.000000000000000000, 0.9238795325112869605, 1.000000000000000000, 0.9238795325112869605, 1.000000000000000000, 0.9238795325112869605, 1.000000000000000000, 0.9238795325112869605, 1.000000000000000000, 0.9238795325112869605, 1.000000000000000000, 0.9238795325112869605, 1.000000000000000000, 0.9238795325112869605, 1.000000000000000000, 0.9238795325112869605, 1.000000000000000000, 0.9238795325112869605, 1.000000000000000000, 0.9238795325112869605, 1.000000000000000000, 0.9238795325112869605, 1.000000000000000000, 0.9238795325112869605, 1.000000000000000000, 0.9238795325112869605, 1.000000000000000000, 0.9238795325112869605, 1.000000000000000000, 0.9238795325112869605, 1.000000000000000000, 0.9238795325112869605, 1.000000000000000000, 0.9238795325112869605, 1.000000000000000000, 0.9238795325112869605, 1.000000000000000000, 0.9238795325112869605, 1.000000000000000000, 0.9238795325112869605, 1.000000000000000000, 0.9238795325112869605, 1.000000000000000000, 0.9238795325112869605, 1.000000000000000000, 0.9238795325112869605, 1.000000000000000000, 0.9238795325112869605, 1.000000000000000000, 0.9238795325112869605, 1.000000000000000000, 0.9238795325112869605, 1.000000000000000000, 0.9238795325112869605, 1.000000000000000000, 0.9238795325112869605, 1.000000000000000000, 0.9238795325112869605, 1.000000000000000000, 0.9238795325112869605, 1.000000000000000000, 0.9238795325112869605, 1.000000000000000000, 0.9238795325112869605, 1.000000000000000000, 0.9238795325112869605, 1.000000000000000000, 0.9238795325112869605, 1.000000000000000000, 0.9238795325112869605, 1.000000000000000000, 0.9238795325112869605, 1.000000000000000000, 0.9238795325112869605, 1.000000000000000000, 0.9238795325112869605, 1.000000000000000000, 0.9238795325112869605, 1.000000000000000000, 0.9238795325112869605, 1.000000000000000000, 0.9238795325112869605, 1.000000000000000000, 0.9238795325112869605, 1.000000000000000000, 0.9238795325112869605, 1.000000000000000000, 0.9238795325112869605, 1.000000000000000000, 0.9238795325112869605, 1.000000000000000000, 0.9238795325112869605, 1.000000000000000000, 0.9238795325112869605, 1.000000000000000000, 0.9238795325112869605, 1.000000000000000000, 0.9238795325112869605, 1.000000000000000000, 0.9238795325112869605, 1.000000000000000000, 0.9238795325112869605, 1.000000000000000000, 0.9238795325112869605, 1.000000000000000000, 0.9238795325112869605, 1.000000000000000000, 0.9238795325112869605, 1.000000000000000000, 0.9238795325112869605, 1.000000000000000000, 0.9238795325112869605, 1.000000000000000000, 0.9238795325112869605, 1.000000000000000000, 0.9238795325112869605, 1.000000000000000000, 0.9238795325112869605, 1.000000000000000000, 0.9238795325112869605, 1.000000000000000000, 0.9238795325112869605, 1.000000000000000000, 0.9238795325112869605, 1.000000000000000000, 0.9238795325112869605, 1.000000000000000000, 0.9238795325112869605, 1.000000000000000000, 0.9238795325112869605, 1.000000000000000000, 0.9238795325112869605, 1.000000000000000000, 0.9238795325112869605, 1.000000000000000000, 0.9238795325112869605, 1.000000000000000000, 0.9238795325112869605, 1.000000000000000000, 0.9238795325112869605, 1.000000000000000000, 0.9238795325112869605, 1.000000000000000000, 0.9238795325112869605, 1.000000000000000000, 0.9238795325112869605, 1.000000000000000000, 0.9238795325112869605, 1.000000000000000000, 0.9238795325112869605, 1.000000000000000000, 0.9238795325112869605, 1.000000000000000000, 0.9238795325112869605, 1.000000000000000000, 0.9238795325112869605, 1.000000000000000000, 0.9238795325112869605, 1.000000000000000000, 0.9238795325112869605, 1.000000000000000000, 0.9238795325112869605, 1.000000000000000000, 0.9238795325112869605, 1.000000000000000000, 0.9238795325112869605, 1.000000000000000000, 0.9238795325112869605, 1.000000000000000000, 0.9238795325112869605, 1.000000000000000000, 0.9238795325112869605, 1.000000000000000000, 0.9238795325112869605, 1.000000000000000000, 0.9238795325112869605, 1.000000000000000000, 0.9238795325112869605, 1.000000000000000000, 0.9238795325112869605, 1.000000000000000000, 0.9238795325112869605, 1.000000000000000000, 0.9238795325112869605, 1.000000000000000000, 0.9238795325112869605, 1.000000000000000000, 0.9238795325112869605, 1.000000000000000000, 0.9238795325112869605, 1.000000000000000000, 0.9238795325112869605, 1.000000000000000000, 0.9238795325112869605, 1.000000000000000000, 0.9238795325112869605, 1.000000000000000000, 0.9238795325112869605, 1.000000000000000000, 0.9238795325112869605, 1.000000000000000000, 0.9238795325112869605, 1.000000000000000000, 0.9238795325112869605, 1.000000000000000000, 0.9238795325112869605, 1.000000000000000000, 0.9238795325112869605, 1.000000000000000000, 0.9238795325112869605, 1.000000000000000000, 0.9238795325112869605, 1.000000000000000000, 0.9238795325112869605, 1.000000000000000000, 0.9238795325112869605, 1.000000000000000000, 0.9238795325112869605, 1.000000000000000000, 0.9238795325112869605, 1.000000000000000000, 0.9238795325112869605, 1.000000000000000000, 0.9238795325112869605, 1.000000000000000000, 0.9238795325112869605, 1.000000000000000000, 0.9238795325112869605, 1.000000000000000000, 0.9238795325112869605, 1.000000000000000000, 0.9238795325112869605, 1.000000000000000000, 0.9238795325112869605, 1.000000000000000000, 0.9238795325112869605, 1.000000000000000000, 0.9238795325112869605, 1.000000000000000000, 0.9238795325112869605, 1.000000000000000000, 0.9238795325112869605, 1.000000000000000000, 0.9238795325112869605, 1.000000000000000000, 0.9238795325112869605, 1.000000000000000000, 0.9238795325112869605, 1.000000000000000000, 0.9238795325112869605, 1.000000000000000000, 0.9238795325112869605, 1.000000000000000000, 0.9238795325112869605, 1.000000000000000000, 0.9238795325112869605, 1.000000000000000000, 0.9238795325112869605, 1.000000000000000000, 0.9238795325112869605, 1.000000000000000000, 0.9238795325112869605, 1.000000000000000000, 0.9238795325112869605, 1.000000000000000000, 0.9238795325112869605, 1.000000000000000000, 0.9238795325112869605, 1.000000000000000000, 0.9238795325112869605, 1.000000000000000000, 0.9238795325112869605, 1.000000000000000000, 0.9238795325112869605, 1.000000000000000000, 0.9238795325112869605, 1.000000000000000000, 0.9238795325112869605, 1.000000000000000000, 0.9238795325112869605, 1.000000000000000000, 0.9238795325112869605, 1.000000000000000000, 0.9238795325112869605, 1.000000000000000000, 0.9238795325112869605, 1.000000000000000000, 0.9238795325112869605, 1.000000000000000000, 0.9238795325112869605, 1.000000000000000000, 0.9238795325112869605, 1.000000000000000000, 0.9238795325112869605, 1.000000000000000000, 0.9238795325112869605, 1.000000000000000000, 0.9238795325112869605, 1.000000000000000000, 0.9238795325112869605, 1.000000000000000000, 0.9238795325112869605, 1.000000000000000000, 0.9238795325112869605, 1.000000000000000000, 0.9238795325112869605, 1.000000000000000000, 0.9238795325112869605, 1.000000000000000000, 0.9238795325112869605, 1.000000000000000000, 0.9238795325112869605, 1.000000000000000000, 0.9238795325112869605, 1.000000000000000000, 0.9238795325112869605, 1.000000000000000000, 0.9238795325112869605, 1.000000000000000000, 0.9238795325112869605, 1.000000000000000000, 0.9238795325112869605, 1.000000000000000000, 0.9238795325112869605, 1.000000000000000000, 0.9238795325112869605, 1.000000000000000000, 0.9238795325112869605, 1.000000000000000000, 0.9238795325112869605, 1.000000000000000000, 0.9238795325112869605, 1.000000000000000000, 0.9238795325112869605, 1.000000000000000000, 0.9238795325112869605, 1.000000000000000000, 0.9238795325112869605, 1.000000000000000000, 0.9238795325112869605, 1.000000000000000000, 0.9238795325112869605, 1.000000000000000000, 0.9238795325112869605, 1.000000000000000000, 0.9238795325112869605, 1.000000000000000000, 0.9238795325112869605, 1.000000000000000000, 0.9238795325112869605, 1.000000000000000000, 0.9238795325112869605, 1.000000000000000000, 0.9238795325112869605, 1.000000000000000000, 0.9238795325112869605, 1.000000000000000000, 0.9238795325112869605, 1.000000000000000000, 0.9238795325112869605, 1.000000000000000000, 0.9238795325112869605, 1.000000000000000000, 0.9238795325112869605, 1.000000000000000000, 0.9238795325112869605, 1.000000000000000000, 0.9238795325112869605, 1.000000000000000000, 0.9238795325112869605, 1.000000000000000000, 0.9238795325112869605, 1.000000000000000000, 0.9238795325112869605, 1.000000000000000000, 0.9238795325112869605, 1.000000000000000000, 0.9238795325112869605, 1.000000000000000000, 0.9238795325112869605, 1.000000000000000000, 0.9238795325112869605, 1.000000000000000000, 0.9238795325112869605, 1.000000000000000000, 0.9238795325112869605, 1.000000000000000000, 0.9238795325112869605, 1.000000000000000000, 0.9238795325112869605, 1.000000000000000000, 0.9238795325112869605, 1.000000000000000000, 0.9238795325112869605, 1.000000000000000000, 0.9238795325112869605, 1.000000000000000000, 0.9238795325112869605, 1.000000000000000000, 0.9238795325112869605, 1.000000000000000000, 0.9238795325112869605, 1.000000000000000000, 0.9238795325112869605, 1.000000000000000000, 0.9238795325112869605, 1.000000000000000000, 0.9238795325112869605, 1.000000000000000000, 0.9238795325112869605, 1.000000000000000000, 0.9238795325112869605, 1.000000000000000000, 0.9238795325112869605, 1.000000000000000000, 0.9238795325112869605, 1.000000000000000000, 0.9238795325112869605, 1.000000000000000000, 0.9238795325112869605, 1.000000000000000000, 0.9238795325112869605, 1.000000000000000000, 0.9238795325112869605, 1.000000000000000000, 0.9238795325112869605, 1.000000000000000000, 0.9238795325112869605, 1.000000000000000000, 0.9238795325112869605, 1.000000000000000000, 0.9238795325112869605, 1.000000000000000000, 0.9238795325112869605, 1.000000000000000000, 0.9238795325112869605, 1.000000000000000000, 0.9238795325112869605, 1.000000000000000000, 0.9238795325112869605, 1.000000000000000000, 0.9238795325112869605, 1.000000000000000000, 0.9238795325112869605, 1.000000000000000000, 0.9238795325112869605, 1.000000000000000000, 0.9238795325112869605, 1.000000000000000000, 0.9238795325112869605, 1.000000000000000000, 0.9238795325112869605, 1.000000000000000000, 0.9238795325112869605, 1.000000000000000000, 0.9238795325112869605, 1.000000000000000000, 0.9238795325112869605, 1.000000000000000000, 0.9238795325112869605, 1.000000000000000000, 0.9238795325112869605, 1.000000000000000000, 0.9238795325112869605, 1.000000000000000000, 0.9238795325112869605, 1.000000000000000000, 0.9238795325112869605, 1.000000000000000000, 0.9238795325112869605, 1.000000000000000000, 0.9238795325112869605, 1.000000000000000000, 0.9238795325112869605, 1.000000000000000000, 0.9238795325112869605, 1.000000000000000000, 0.9238795325112869605, 1.000000000000000000, 0.9238795325112869605, 1.000000000000000000, 0.9238795325112869605, 1.000000000000000000, 0.9238795325112869605, 1.000000000000000000, 0.9238795325112869605, 1.000000000000000000, 0.9238795325112869605, 1.000000000000000000, 0.9238795325112869605, 1.000000000000000000, 0.9238795325112869605, 1.000000000000000000, 0.9238795325112869605, 1.000000000000000000, 0.9238795325112869605, 1.000000000000000000, 0.9238795325112869605, 1.000000000000000000, 0.9238795325112869605, 1.000000000000000000, 0.9238795325112869605, 1.000000000000000000, 0.9238795325112869605, 1.000000000000000000, 0.9238795325112869605, 1.000000000000000000, 0.9238795325112869605, 1.000000000000000000, 0.9238795325112869605, 1.000000000000000000, 0.9238795325112869605, 1.000000000000000000, 0.9238795325112869605, 1.000000000000000000, 0.9238795325112869605, 1.000000000000000000, 0.9238795325112869605, 1.000000000000000000, 0.9238795325112869605, 1.000000000000000000, 0.9238795325112869605, 1.000000000000000000, 0.9238795325112869605, 1.000000000000000000, 0.9238795325112869605, 1.000000000000000000, 0.9238795325112869605, 1.000000000000000000, 0.9238795325112869605, 1.000000000000000000, 0.9238795325112869605, 1.000000000000000000, 0.9238795325112869605, 1.000000000000000000, 0.9238795325112869605, 1.000000000000000000, 0.9238795325112869605, 1.000000000000000000, 0.9238795325112869605, 1.000000000000000000, 0.9238795325112869605, 1.000000000000000000, 0.9238795325112869605, 1.000000000000000000, 0.9238795325112869605, 1.000000000000000000, 0.9238795325112869605, 1.000000000000000000, 0.9238795325112869605, 1.000000000000000000, 0.9238795325112869605, 1.000000000000000000, 0.9238795325112869605, 1.000000000000000000, 0.9238795325112869605, 1.000000000000000000, 0.9238795325112869605, 1.000000000000000000, 0.9238795325112869605, 1.000000000000000000, 0.9238795325112869605, 1.000000000000000000, 0.9238795325112869605, 1.000000000000000000, 0.9238795325112869605, 1.000000000000000000, 0.9238795325112869605, 1.000000000000000000, 0.9238795325112869605, 1.000000000000000000, 0.9238795325112869605, 1.000000000000000000, 0.9238795325112869605, 1.000000000000000000, 0.9238795325112869605, 1.000000000000000000, 0.9238795325112869605, 1.000000000000000000, 0.9238795325112869605, 1.000000000000000000, 0.9238795325112869605, 1.000000000000000000, 0.9238795325112869605, 1.000000000000000000, 0.9238795325112869605, 1.000000000000000000, 0.9238795325112869605, 1.000000000000000000, 0.9238795325112869605, 1.000000000000000000, 0.9238795325112869605, 1.000000000000000000, 0.9238795325112869605, 1.000000000000000000, 0.9238795325112869605, 1.000000000000000000, 0.9238795325112869605, 1.000000000000000000, 0.9238795325112869605, 1.000000000000000000, 0.9238795325112869605, 1.000000000000000000, 0.9238795325112869605, 1.000000000000000000, 0.9238795325112869605, 1.000000000000000000, 0.9238795325112869605, 1.000000000000000000, 0.9238795325112869605, 1.000000000000000000, 0.9238795325112869605, 1.000000000000000000, 0.9238795325112869605, 1.000000000000000000, 0.9238795325112869605, 1.000000000000000000, 0.9238795325112869605, 1.000000000000000000, 0.9238795325112869605, 1.000000000000000000, 0.9238795325112869605, 1.000000000000000000, 0.9238795325112869605, 1.000000000000000000, 0.9238795325112869605, 1.000000000000000000, 0.9238795325112869605, 1.000000000000000000, 0.9238795325112869605, 1.000000000000000000, 0.9238795325112869605, 1.000000000000000000, 0.9238795325112869605, 1.000000000000000000, 0.9238795325112869605, 1.000000000000000000, 0.9238795325112869605, 1.000000000000000000, 0.9238795325112869605, 1.000000000000000000, 0.9238795325112869605, 1.000000000000000000, 0.9238795325112869605, 1.000000000000000000, 0.9238795325112869605, 1.000000000000000000, 0.9238795325112869605, 1.000000000000000000, 0.9238795325112869605, 1.000000000000000000, 0.9238795325112869605, 1.000000000000000000, 0.9238795325112869605, 1.000000000000000000, 0.9238795325112869605, 1.000000000000000000, 0.9238795325112869605, 1.000000000000000000, 0.9238795325112869605, 1.000000000000000000) ) ) 
 REPRESENTATION_ITEM ( '' )  SURFACE ( )  ) ;
#34979 = CARTESIAN_POINT ( 'NONE',  ( 0.9412147342319837628, 0.1574803149606300301, 1.227854330601135580 ) ) ;
#34981 = CARTESIAN_POINT ( 'NONE',  ( 0.1588150004738602128, 0.1472798737662930069, -0.02049432688553750465 ) ) ;
#34982 = EDGE_CURVE ( 'NONE', #12359, #20645, #7082, .T. ) ;
#34983 = ORIENTED_EDGE ( 'NONE', *, *, #44187, .T. ) ;
#34984 = VERTEX_POINT ( 'NONE', #16182 ) ;
#34985 = CARTESIAN_POINT ( 'NONE',  ( -0.6971942568897648851, -0.07405724077823297447, 1.860236220418677089 ) ) ;
#34986 = ORIENTED_EDGE ( 'NONE', *, *, #4041, .T. ) ;
#34987 = DIRECTION ( 'NONE',  ( -0.000000000000000000, 1.000000000000000000, -0.000000000000000000 ) ) ;
#34988 = CARTESIAN_POINT ( 'NONE',  ( -0.8019270111902717657, -0.1787899950787401604, 1.466535433017102763 ) ) ;
#34989 = CARTESIAN_POINT ( 'NONE',  ( 0.5113546317124669782, -3.032960542342102697E-32, 0.09842519685039370636 ) ) ;
#34990 = EDGE_CURVE ( 'NONE', #31526, #46098, #30813, .T. ) ;
#34991 = CARTESIAN_POINT ( 'NONE',  ( -1.002407869896990045, 0.1264236179284866091, 0.3075787401037169411 ) ) ;
#34992 = CARTESIAN_POINT ( 'NONE',  ( 0.8107537697050254399, -0.1574803149606297803, 1.572342519685040907 ) ) ;
#34993 = CARTESIAN_POINT ( 'NONE',  ( -1.054774247047244540, -0.07405724077823318263, 1.756889763725764553 ) ) ;
#34994 = CARTESIAN_POINT ( 'NONE',  ( -0.1292751490962173455, 0.09842519685039369248, 0.2107960287359116613 ) ) ;
#34995 = CARTESIAN_POINT ( 'NONE',  ( -0.8107537697050253289, 0.1574803149606300301, 1.715059055118110631 ) ) ;
#34996 = CYLINDRICAL_SURFACE ( 'NONE', #29784, 0.1574803149606292529 ) ;
#34997 = CARTESIAN_POINT ( 'NONE',  ( -0.07405724077823318263, -0.2058326296465617378, 0.1787899950787401604 ) ) ;
#34998 = CARTESIAN_POINT ( 'NONE',  ( 0.7495606340400177148, 0.1264236179284866091, 1.695374015694267822 ) ) ;
#34999 = CARTESIAN_POINT ( 'NONE',  ( -0.02490719980953610274, -0.09842519685039370636, -0.1871115436693586709 ) ) ;
#35000 = LINE ( 'NONE', #5747, #42462 ) ;
#35001 = AXIS2_PLACEMENT_3D ( 'NONE', #15105, #39353, #36900 ) ;
#35002 = ORIENTED_EDGE ( 'NONE', *, *, #38271, .F. ) ;
#35003 = CARTESIAN_POINT ( 'NONE',  ( -0.9500414927467377701, 0.1787899950787401604, 1.294291338528913204 ) ) ;
#35004 = CARTESIAN_POINT ( 'NONE',  ( -0.07405724077823318263, -1.075787401521038689, -0.1787899950787401604 ) ) ;
#35005 = CARTESIAN_POINT ( 'NONE',  ( -0.1264236179284866091, -1.255413385773007873, 0.1264236179284866091 ) ) ;
#35006 = CARTESIAN_POINT ( 'NONE',  ( -1.033464566929134687, 0.06523048226347956391, 1.272145669291338432 ) ) ;
#35007 = CARTESIAN_POINT ( 'NONE',  ( 0.1797182628040039087, -0.5300634946224150879, -0.07444174185955065859 ) ) ;
#35008 = CARTESIAN_POINT ( 'NONE',  ( 2.892866454678787531E-17, -1.779527558947590515, 0.1574803149606299191 ) ) ;
#35009 = CARTESIAN_POINT ( 'NONE',  ( -0.9412147342319837628, 0.1574803149606300301, 0.7947834644594014009 ) ) ;
#35010 = CARTESIAN_POINT ( 'NONE',  ( -1.033464566929134687, 0.06523048226347956391, 0.7997047244094482865 ) ) ;
#35011 = CARTESIAN_POINT ( 'NONE',  ( -0.1574803149606299191, 0.05118110236220472370, 0.000000000000000000 ) ) ;
#35012 = CARTESIAN_POINT ( 'NONE',  ( 0.6971942568897626646, 0.07405724077823318263, 0.9448818897100165204 ) ) ;
#35013 = CARTESIAN_POINT ( 'NONE',  ( 0.1982027233128390575, 0.1810618366036217119, -0.05428606100831530334 ) ) ;
#35014 = CARTESIAN_POINT ( 'NONE',  ( 1.054774247047244096, 0.000000000000000000, 1.956200787347811110 ) ) ;
#35015 = EDGE_CURVE ( 'NONE', #18113, #6083, #46799, .T. ) ;
#35016 = CARTESIAN_POINT ( 'NONE',  ( -0.8107537697050254399, -0.1574803149606297803, 1.178641732283464583 ) ) ;
#35017 = CARTESIAN_POINT ( 'NONE',  ( 0.1787899950787401604, -0.6181102361667089040, 0.07405724077823318263 ) ) ;
#35018 = DIRECTION ( 'NONE',  ( 0.000000000000000000, 0.7071067811862530306, 0.7071067811868418929 ) ) ;
#35019 = ADVANCED_FACE ( 'NONE', ( #35097 ), #40001, .F. ) ;
#35021 = AXIS2_PLACEMENT_3D ( 'NONE', #6654, #24409, #36079 ) ;
#35020 = CARTESIAN_POINT ( 'NONE',  ( 0.1264236179284866091, -1.403051181048598384, 0.1264236179284866091 ) ) ;
#35022 = CARTESIAN_POINT ( 'NONE',  ( 0.7495606340400177148, -0.1264236179284866091, 0.3272637794737956463 ) ) ;
#35023 = ADVANCED_FACE ( 'NONE', ( #9692 ), #17339, .T. ) ;
#35024 = CARTESIAN_POINT ( 'NONE',  ( -0.8759842519685039353, 0.1787899950787401882, 1.921751968450173376 ) ) ;
#35025 = ORIENTED_EDGE ( 'NONE', *, *, #45633, .F. ) ;
#35026 = CARTESIAN_POINT ( 'NONE',  ( -0.6971942568897648851, 0.07405724077823318263, 1.461614173174583753 ) ) ;
#35027 = CARTESIAN_POINT ( 'NONE',  ( 0.6971942568897648851, 0.07405724077823318263, 1.382874015694268044 ) ) ;
#35028 = CARTESIAN_POINT ( 'NONE',  ( -0.7646288533564489232, -0.1113553986120547346, 0.9005905511811023167 ) ) ;
#35029 = CARTESIAN_POINT ( 'NONE',  ( -0.6971942568897626646, 0.07405724077823318263, 0.7135826771115916234 ) ) ;
#35030 = CARTESIAN_POINT ( 'NONE',  ( -0.7495606340400177148, -0.1264236179284866091, 1.149114173174582643 ) ) ;
#35031 = DIRECTION ( 'NONE',  ( 1.000000000000000000, 0.000000000000000000, -1.822029033848725275E-16 ) ) ;
#35032 = DIRECTION ( 'NONE',  ( -1.000000000000000000, 0.000000000000000000, -7.051687499798870116E-15 ) ) ;
#35033 = CARTESIAN_POINT ( 'NONE',  ( 0.6971942568897637749, 2.189545951927499583E-17, 0.5585629920722204877 ) ) ;
#35034 = EDGE_CURVE ( 'NONE', #35490, #22163, #16644, .T. ) ;
#35035 = CARTESIAN_POINT ( 'NONE',  ( -0.3980944881889731390, 1.061695335278756147, -0.02376411959061705201 ) ) ;
#35036 = EDGE_CURVE ( 'NONE', #34797, #799, #42261, .T. ) ;
#35037 = DIRECTION ( 'NONE',  ( 0.000000000000000000, 0.000000000000000000, 1.000000000000000000 ) ) ;
#35038 = ORIENTED_EDGE ( 'NONE', *, *, #45869, .T. ) ;
#35039 = ORIENTED_EDGE ( 'NONE', *, *, #12090, .T. ) ;
#35040 = DIRECTION ( 'NONE',  ( 0.000000000000000000, 0.000000000000000000, 1.000000000000000000 ) ) ;
#35041 = CARTESIAN_POINT ( 'NONE',  ( -0.9412147342319837628, -0.1574803149606297803, 0.2386811023622048278 ) ) ;
#35042 = CARTESIAN_POINT ( 'NONE',  ( 1.002407869896990045, -0.1264236179284866091, 1.360728346402929168 ) ) ;
#35043 = CARTESIAN_POINT ( 'NONE',  ( 0.05863737992348047601, -0.09851384783664468570, 0.2134933313796791299 ) ) ;
#35044 = CARTESIAN_POINT ( 'NONE',  ( -1.033464566929133799, 0.000000000000000000, 1.850393700679873854 ) ) ;
#35045 = ORIENTED_EDGE ( 'NONE', *, *, #7746, .F. ) ;
#35046 = CARTESIAN_POINT ( 'NONE',  ( -1.033464566929133799, 0.000000000000000000, 0.6397637795275591399 ) ) ;
#35047 = CARTESIAN_POINT ( 'NONE',  ( -0.7495606340400177148, 0.1264236179284866091, 1.026082677111590513 ) ) ;
#35048 = ORIENTED_EDGE ( 'NONE', *, *, #16236, .T. ) ;
#35049 = CARTESIAN_POINT ( 'NONE',  ( 0.4736248074375850603, 1.357244529069700612, -1.397888825503269761 ) ) ;
#35050 = CARTESIAN_POINT ( 'NONE',  ( 3.284318927891251994E-17, -0.6205708660879685201, 0.1787899950787401882 ) ) ;
#35051 = DIRECTION ( 'NONE',  ( 0.000000000000000000, -0.6156614753256598460, -0.7880107536067206819 ) ) ;
#35052 = ORIENTED_EDGE ( 'NONE', *, *, #43050, .T. ) ;
#35053 = CARTESIAN_POINT ( 'NONE',  ( 0.7495606340400177148, 0.1264236179284866091, 1.414862204670645829 ) ) ;
#35054 = VECTOR ( 'NONE', #9627, 39.37007874015748143 ) ;
#35055 = CARTESIAN_POINT ( 'NONE',  ( 0.1787899950787401604, -0.7657480314423001921, -0.07405724077823318263 ) ) ;
#35056 = CARTESIAN_POINT ( 'NONE',  ( 0.5966535433070866423, 0.000000000000000000, 0.09842519685039370636 ) ) ;
#35057 = DIRECTION ( 'NONE',  ( -1.000000000000000000, 3.469446951953613794E-15, 0.000000000000000000 ) ) ;
#35058 = CARTESIAN_POINT ( 'NONE',  ( 0.07405724077823318263, 0.03530910263690301143, 0.1787899950787401604 ) ) ;
#35059 = CARTESIAN_POINT ( 'NONE',  ( 3.284318927891251994E-17, 0.08316929139234625901, 0.1787899950787401882 ) ) ;
#35060 = APPLICATION_PROTOCOL_DEFINITION ( 'draft international standard', 'automotive_design', 1998, #26947 ) ;
#35061 = CARTESIAN_POINT ( 'NONE',  ( -0.01002589960738839783, -0.09842519685039363697, 0.1604807810695956793 ) ) ;
#35062 = CARTESIAN_POINT ( 'NONE',  ( 0.7495606340400177148, 0.1264236179284866091, 0.5093503936470236138 ) ) ;
#35063 = CARTESIAN_POINT ( 'NONE',  ( -0.8019270111902716547, 0.1787899950787401604, 0.8661417322297002563 ) ) ;
#35064 = EDGE_CURVE ( 'NONE', #10382, #40254, #21662, .T. ) ;
#35066 = CARTESIAN_POINT ( 'NONE',  ( 0.7185039370078739607, 1.928577636452523993E-17, 0.09842519674286673292 ) ) ;
#35065 = CARTESIAN_POINT ( 'NONE',  ( -0.1574803149606299191, -0.9330708661417322913, 0.000000000000000000 ) ) ;
#35068 = CARTESIAN_POINT ( 'NONE',  ( -0.8490223526853721836, -0.1715985158898769847, 1.987713034038145477 ) ) ;
#35067 = CARTESIAN_POINT ( 'NONE',  ( -0.1797182628040039365, -1.575831211157848299, 0.000000000000000000 ) ) ;
#35069 = CARTESIAN_POINT ( 'NONE',  ( -0.7185039370078739607, 1.928577636452523993E-17, 1.240157480207432883 ) ) ;
#35070 = CARTESIAN_POINT ( 'NONE',  ( 0.6971942568897648851, -0.07405724077823297447, 1.584645669237574994 ) ) ;
#35072 = CARTESIAN_POINT ( 'NONE',  ( -0.7185039370078746268, -0.06523048226347956391, 1.803641732283465471 ) ) ;
#35071 = CARTESIAN_POINT ( 'NONE',  ( 0.1235961452251413406, 0.09842519685039370636, -0.2140748031496062798 ) ) ;
#35073 = CARTESIAN_POINT ( 'NONE',  ( 0.7495606340400177148, 0.1264236179284866091, 0.3912401574265515491 ) ) ;
#35074 = EDGE_CURVE ( 'NONE', #5428, #13158, #3270, .T. ) ;
#35076 = ORIENTED_EDGE ( 'NONE', *, *, #5387, .T. ) ;
#35075 = DIRECTION ( 'NONE',  ( -0.000000000000000000, 0.7880107536067174623, -0.6156614753256640649 ) ) ;
#35077 = CARTESIAN_POINT ( 'NONE',  ( 1.033464566929134687, -0.06523048226347956391, 0.8636811022546768690 ) ) ;
#35078 = DIRECTION ( 'NONE',  ( 0.000000000000000000, 0.000000000000000000, -1.000000000000000000 ) ) ;
#35080 = CARTESIAN_POINT ( 'NONE',  ( 0.07405724077823318263, -0.03248031490686641154, 0.1787899950787401604 ) ) ;
#35079 = CARTESIAN_POINT ( 'NONE',  ( 2.892866454678787531E-17, -0.8740157479239685223, 0.1574803149606299191 ) ) ;
#35081 = CARTESIAN_POINT ( 'NONE',  ( 0.9412147342319837628, -0.1574803149606297803, 0.5044291337507409434 ) ) ;
#35082 = CARTESIAN_POINT ( 'NONE',  ( -0.1787899950787401882, -0.03986220467064590517, 0.000000000000000000 ) ) ;
#35083 = CARTESIAN_POINT ( 'NONE',  ( 0.8019270111902717657, -0.1787899950787401604, 0.4429133857730075952 ) ) ;
#35084 = CARTESIAN_POINT ( 'NONE',  ( 0.1264236179284866091, -0.9995078739619842612, -0.1264236179284866091 ) ) ;
#35085 = CARTESIAN_POINT ( 'NONE',  ( 0.7925511340933090176, -0.1404228911275084979, 0.03937002898646041471 ) ) ;
#35086 = CYLINDRICAL_SURFACE ( 'NONE', #20831, 0.1574803149606299191 ) ;
#35087 = EDGE_LOOP ( 'NONE', ( #5205, #21834, #7494, #31483 ) ) ;
#35088 = DIRECTION ( 'NONE',  ( 0.000000000000000000, 0.2432573283306645462, -0.9699617890481188054 ) ) ;
#35089 = CARTESIAN_POINT ( 'NONE',  ( 0.7495606340400177148, -0.1264236179284866091, 1.035925196796629866 ) ) ;
#35090 = ORIENTED_EDGE ( 'NONE', *, *, #8384, .F. ) ;
#35091 = CARTESIAN_POINT ( 'NONE',  ( -0.06523048226347956391, -1.088090551073574996, -0.1574803149606300301 ) ) ;
#35092 = CARTESIAN_POINT ( 'NONE',  ( -0.8759842519685039353, -0.1574803149606299191, 0.5019685038294811052 ) ) ;
#35093 = CARTESIAN_POINT ( 'NONE',  ( 0.8759842519685039353, 0.1787899950787401882, 1.724901574749385880 ) ) ;
#35094 = CARTESIAN_POINT ( 'NONE',  ( -0.7185039370078739607, 1.928577636452523993E-17, 1.407480314960629864 ) ) ;
#35095 = DIRECTION ( 'NONE',  ( -1.000000000000000000, 0.000000000000000000, 0.000000000000000000 ) ) ;
#35097 = FACE_OUTER_BOUND ( 'NONE', #2191, .T. ) ;
#35096 = DIRECTION ( 'NONE',  ( 1.267059173938974432E-30, 3.652049423109077687E-16, -1.000000000000000000 ) ) ;
#35098 = CARTESIAN_POINT ( 'NONE',  ( 0.9500414927467377701, -0.1787899950787401604, 0.2165354330171024577 ) ) ;
#35099 = CARTESIAN_POINT ( 'NONE',  ( -0.7495606340400177148, -0.1264236179284866091, 0.1254921259304885850 ) ) ;
#35100 = CARTESIAN_POINT ( 'NONE',  ( 0.7185039370078739607, 1.928577636452523993E-17, 1.358267716427907779 ) ) ;
#35101 = EDGE_LOOP ( 'NONE', ( #27225, #19394, #3775, #35108, #35626 ) ) ;
#35102 = ORIENTED_EDGE ( 'NONE', *, *, #8645, .T. ) ;
#35103 = CONICAL_SURFACE ( 'NONE', #18986, 0.2471922904502826812, 0.5235987755982992597 ) ;
#35104 = CARTESIAN_POINT ( 'NONE',  ( 0.1787899950787401882, 0.09301181107738563936, -2.189545951927503898E-17 ) ) ;
#35105 = CARTESIAN_POINT ( 'NONE',  ( 0.1993772601175047565, -0.1803837174632775264, -0.05517042925146220522 ) ) ;
#35106 = ORIENTED_EDGE ( 'NONE', *, *, #9368, .T. ) ;
#35107 = CARTESIAN_POINT ( 'NONE',  ( -1.054774247047244096, 0.000000000000000000, 1.636318897584031484 ) ) ;
#35108 = ORIENTED_EDGE ( 'NONE', *, *, #9960, .F. ) ;
#35109 = ORIENTED_EDGE ( 'NONE', *, *, #10990, .T. ) ;
#35110 = DIRECTION ( 'NONE',  ( 1.000000000000000000, 0.000000000000000000, 0.000000000000000000 ) ) ;
#35111 = CARTESIAN_POINT ( 'NONE',  ( -7.957671378281915615E-17, 0.1564960629921311464, -0.3937007874015748254 ) ) ;
#35112 = CARTESIAN_POINT ( 'NONE',  ( 0.7185039370078766252, -0.06523048226348168721, 1.596948818790109970 ) ) ;
#35113 = CARTESIAN_POINT ( 'NONE',  ( -0.1264236179284866091, -1.153175149331600480, 0.1264236179284866091 ) ) ;
#35114 = ORIENTED_EDGE ( 'NONE', *, *, #6147, .F. ) ;
#35115 = CARTESIAN_POINT ( 'NONE',  ( -0.1787899950787401882, -0.1973425196312759700, 0.000000000000000000 ) ) ;
#35116 = ORIENTED_EDGE ( 'NONE', *, *, #35064, .T. ) ;
#35117 = EDGE_LOOP ( 'NONE', ( #24182, #283, #16195, #26791 ) ) ;
#35118 = CARTESIAN_POINT ( 'NONE',  ( -0.9412147342319837628, -0.1574803149606297803, 1.409940944774363603 ) ) ;
#35119 = FACE_OUTER_BOUND ( 'NONE', #30343, .T. ) ;
#35120 = CARTESIAN_POINT ( 'NONE',  ( 0.7185039370078746268, 0.06523048226347956391, 1.877460629921260393 ) ) ;
#35121 = CARTESIAN_POINT ( 'NONE',  ( -0.1264236179284866091, -0.6304133857730078727, 0.1264236179284866091 ) ) ;
#35122 = EDGE_CURVE ( 'NONE', #40732, #46518, #1995, .T. ) ;
#35123 = EDGE_LOOP ( 'NONE', ( #41789, #4513, #13583, #2416 ) ) ;
#35124 = EDGE_CURVE ( 'NONE', #3019, #44530, #39366, .T. ) ;
#35125 = CARTESIAN_POINT ( 'NONE',  ( -1.002407869896990045, -0.1264236179284866091, 0.3764763778989925203 ) ) ;
#35126 = CARTESIAN_POINT ( 'NONE',  ( -0.7185039370078746268, -0.06523048226347956391, 1.016240157480315487 ) ) ;
#35127 = CARTESIAN_POINT ( 'NONE',  ( -0.3161444924769509779, 2.559880088878760951, -3.648497683167374550 ) ) ;
#35128 = CARTESIAN_POINT ( 'NONE',  ( -1.100456976456230270E-17, -1.231343022181470293, -0.1797182628040039365 ) ) ;
#35129 = DIRECTION ( 'NONE',  ( -1.000000000000000000, 0.000000000000000000, 0.000000000000000000 ) ) ;
#35130 = CARTESIAN_POINT ( 'NONE',  ( 0.9500414927467378812, -0.1787899950787401604, 1.122047244040725644 ) ) ;
#35131 = CARTESIAN_POINT ( 'NONE',  ( 1.054774247047244540, -0.07405724077823318263, 1.594488188922615457 ) ) ;
#35132 = CARTESIAN_POINT ( 'NONE',  ( 0.8019270111902716547, 0.1787899950787401604, 0.1919291338045042705 ) ) ;
#35133 = EDGE_CURVE ( 'NONE', #19079, #19636, #40740, .T. ) ;
#35134 = EDGE_CURVE ( 'NONE', #34936, #30980, #4870, .T. ) ;
#35135 = CARTESIAN_POINT ( 'NONE',  ( 0.7646288533564489232, -0.1113553986120547346, 0.2312992125984252023 ) ) ;
#35136 = CARTESIAN_POINT ( 'NONE',  ( 0.7185039370078746268, -0.06523048226347956391, 1.646161417322835385 ) ) ;
#35138 = DIRECTION ( 'NONE',  ( -1.000000000000000000, -0.000000000000000000, -0.000000000000000000 ) ) ;
#35137 = CARTESIAN_POINT ( 'NONE',  ( 0.7717440911643036472, 0.1232935613849624051, 1.980556353253522861 ) ) ;
#35139 = CARTESIAN_POINT ( 'NONE',  ( 0.000000000000000000, 0.09842519685039370636, 0.2471922904502826812 ) ) ;
#35140 = CYLINDRICAL_SURFACE ( 'NONE', #46746, 0.09842519685039317900 ) ;
#35141 = CARTESIAN_POINT ( 'NONE',  ( 0.8759842519685039353, 0.1787899950787401882, 1.016240157426551161 ) ) ;
#35142 = CARTESIAN_POINT ( 'NONE',  ( 0.7495606340400177148, -0.1264236179284866091, 1.980807086560409491 ) ) ;
#35143 = CARTESIAN_POINT ( 'NONE',  ( 1.033464566929133799, 0.000000000000000000, 0.3543307085538902057 ) ) ;
#35144 = ORIENTED_EDGE ( 'NONE', *, *, #15157, .T. ) ;
#35145 = PLANE ( 'NONE',  #6188 ) ;
#35146 = CARTESIAN_POINT ( 'NONE',  ( -0.9873396505805591694, 0.1113553986120547346, 0.2017716534357799352 ) ) ;
#35147 = CARTESIAN_POINT ( 'NONE',  ( -0.07405724077823318263, -0.08661417317458304510, -0.1787899950787401604 ) ) ;
#35148 = CARTESIAN_POINT ( 'NONE',  ( 1.002407869896990045, -0.1264236179284866091, 1.355807086560409491 ) ) ;
#35150 = CARTESIAN_POINT ( 'NONE',  ( 0.9873396505805591694, -0.1113553986120547346, 0.07381889753026830980 ) ) ;
#35149 = DIRECTION ( 'NONE',  ( 0.000000000000000000, -1.000000000000000000, 0.000000000000000000 ) ) ;
#35151 = CARTESIAN_POINT ( 'NONE',  ( 0.06523048226347956391, -1.772145669291338654, -0.1574803149606300301 ) ) ;
#35152 = LINE ( 'NONE', #30627, #21410 ) ;
#35153 = AXIS2_PLACEMENT_3D ( 'NONE', #45528, #30730, #12035 ) ;
#35154 = DIRECTION ( 'NONE',  ( -1.000000000000000000, 0.000000000000000000, 0.000000000000000000 ) ) ;
#35155 = DIRECTION ( 'NONE',  ( -1.267059173938974432E-30, -3.652049423109077687E-16, 1.000000000000000000 ) ) ;
#35156 = CIRCLE ( 'NONE', #14484, 0.09842519685039370636 ) ;
#35157 = ORIENTED_EDGE ( 'NONE', *, *, #14833, .T. ) ;
#35158 = CARTESIAN_POINT ( 'NONE',  ( -0.9500414927467377701, 0.1787899950787401604, 1.328740157426552049 ) ) ;
#35159 = CARTESIAN_POINT ( 'NONE',  ( -0.1787899950787401604, -1.656496062938362268, 0.07405724077823318263 ) ) ;
#35160 = CARTESIAN_POINT ( 'NONE',  ( -1.054774247047244096, 0.000000000000000000, 1.011318897584031484 ) ) ;
#35161 = CARTESIAN_POINT ( 'NONE',  ( -1.054774247047244540, -0.07405724077823318263, 1.909448818843873186 ) ) ;
#35162 = ORIENTED_EDGE ( 'NONE', *, *, #25825, .T. ) ;
#35163 = AXIS2_PLACEMENT_3D ( 'NONE', #8442, #11588, #19704 ) ;
#35164 = CARTESIAN_POINT ( 'NONE',  ( -0.8759842519685039353, -0.1787899950787401882, 0.6471456692375747721 ) ) ;
#35165 = DIRECTION ( 'NONE',  ( 0.000000000000000000, 0.000000000000000000, 1.000000000000000000 ) ) ;
#35166 = CARTESIAN_POINT ( 'NONE',  ( 0.0002862075950689860768, 0.01346164328476122732, -0.1377991285521767972 ) ) ;
#35167 = ORIENTED_EDGE ( 'NONE', *, *, #9368, .F. ) ;
#35168 = CARTESIAN_POINT ( 'NONE',  ( 0.1405684605170431090, -0.08956022275308050951, -0.1355147671057568837 ) ) ;
#35169 = CIRCLE ( 'NONE', #22116, 0.1968503937007874405 ) ;
#35170 = DIRECTION ( 'NONE',  ( 0.000000000000000000, -0.000000000000000000, 1.000000000000000000 ) ) ;
#35171 = ORIENTED_EDGE ( 'NONE', *, *, #25617, .T. ) ;
#35172 = DIRECTION ( 'NONE',  ( -1.000000000000000000, 0.000000000000000000, 0.000000000000000000 ) ) ;
#35173 = CARTESIAN_POINT ( 'NONE',  ( -0.6971942568897626646, -0.07405724077823297447, 0.6742125983714335469 ) ) ;
#35174 = CARTESIAN_POINT ( 'NONE',  ( -1.033464566929133799, 0.000000000000000000, 0.9153543307086614567 ) ) ;
#35175 = VERTEX_POINT ( 'NONE', #22338 ) ;
#35176 = CARTESIAN_POINT ( 'NONE',  ( -0.9500414927467377701, -0.1787899950787401604, 1.673228346402929834 ) ) ;
#35177 = CARTESIAN_POINT ( 'NONE',  ( -0.2066929133858267931, -0.5221178280460080368, -0.9040880104747088808 ) ) ;
#35178 = EDGE_CURVE ( 'NONE', #20867, #39669, #13222, .T. ) ;
#35179 = CIRCLE ( 'NONE', #44318, 0.04921259842519686012 ) ;
#35180 = SURFACE_STYLE_FILL_AREA ( #17189 ) ;
#35181 = CARTESIAN_POINT ( 'NONE',  ( 0.9873396505805591694, 0.1113553986120547346, 0.6446850393700788162 ) ) ;
#35182 = ORIENTED_EDGE ( 'NONE', *, *, #30403, .T. ) ;
#35183 = CARTESIAN_POINT ( 'NONE',  ( -0.1270800023317771588, -0.7047682190318641515, 0.1270800023317771588 ) ) ;
#35184 = DIRECTION ( 'NONE',  ( 1.000000000000000000, 0.000000000000000000, 0.000000000000000000 ) ) ;
#35185 = EDGE_CURVE ( 'NONE', #17524, #42489, #10171, .T. ) ;
#35187 = CARTESIAN_POINT ( 'NONE',  ( -0.1683020774058382463, -0.09842519685039370636, 0.03867328716997087829 ) ) ;
#35186 = CARTESIAN_POINT ( 'NONE',  ( 0.1574803149606299191, -0.3622047244094488416, -1.928577636452523993E-17 ) ) ;
#35188 = CARTESIAN_POINT ( 'NONE',  ( -0.8107537697050254399, 0.1574803149606300301, 1.193405511703496957 ) ) ;
#35189 = ORIENTED_EDGE ( 'NONE', *, *, #16146, .T. ) ;
#35190 = EDGE_CURVE ( 'NONE', #17345, #38222, #7961, .T. ) ;
#35191 = CARTESIAN_POINT ( 'NONE',  ( 0.06523048226347956391, 0.02411417322834644855, 0.1574803149606297803 ) ) ;
#35192 = B_SPLINE_CURVE_WITH_KNOTS ( 'NONE', 3,
 ( #35988, #21609, #10364, #47244, #17300, #46997, #21124, #3393, #3149, #24970, #14191, #13481, #29078, #17063, #10118, #24271 ),
 .UNSPECIFIED., .F., .F.,
 ( 4, 2, 2, 2, 2, 2, 2, 4 ),
 ( 0.000000000000000000, 0.1249999999999663325, 0.1874999999999494849, 0.2187499999999465983, 0.2499999999999437117, 0.3749999999999585332, 0.4999999999999734657, 1.000000000000000000 ),
 .UNSPECIFIED. ) ;
#35193 = CARTESIAN_POINT ( 'NONE',  ( 0.9873396505805591694, -0.1113553986120547346, 1.146653543307086798 ) ) ;
#35195 = SURFACE_SIDE_STYLE ('',( #9554 ) ) ;
#35194 = CARTESIAN_POINT ( 'NONE',  ( -0.7185039370078739607, 1.928577636452523993E-17, 1.279527558947590515 ) ) ;
#35196 = VECTOR ( 'NONE', #4228, 39.37007874015748143 ) ;
#35197 = CARTESIAN_POINT ( 'NONE',  ( 1.033464566929133799, 0.000000000000000000, 1.978346456692913646 ) ) ;
#35199 = CARTESIAN_POINT ( 'NONE',  ( -0.3980944881889736386, 0.9100161909011718064, 0.01858545845903165558 ) ) ;
#35198 = CARTESIAN_POINT ( 'NONE',  ( 0.7185039370078739607, 1.928577636452523993E-17, 0.1870078740157480324 ) ) ;
#35200 = DIRECTION ( 'NONE',  ( 1.000000000000000000, 0.000000000000000000, -4.336808689942015271E-16 ) ) ;
#35201 = CARTESIAN_POINT ( 'NONE',  ( -0.1239754358329518830, -0.08954324691734161235, -0.1284353226271238435 ) ) ;
#35202 = CARTESIAN_POINT ( 'NONE',  ( -0.07405724077823318263, -0.5590551180564723444, -0.1787899950787401604 ) ) ;
#35203 = DIRECTION ( 'NONE',  ( 0.000000000000000000, 0.000000000000000000, -1.000000000000000000 ) ) ;
#35204 = ORIENTED_EDGE ( 'NONE', *, *, #46184, .F. ) ;
#35205 = VECTOR ( 'NONE', #37797, 39.37007874015748143 ) ;
#35206 = ( REPRESENTATION_RELATIONSHIP ('NONE','NONE', #9609, #11151 ) REPRESENTATION_RELATIONSHIP_WITH_TRANSFORMATION ( #6033 )SHAPE_REPRESENTATION_RELATIONSHIP( ) ) ;
#35207 = CARTESIAN_POINT ( 'NONE',  ( 0.1377952755905509363, 0.000000000000000000, -0.1436967020037460685 ) ) ;
#35208 = CARTESIAN_POINT ( 'NONE',  ( 0.8019270111902717657, -0.1787899950787401604, 0.7972440944344250102 ) ) ;
#35209 = CARTESIAN_POINT ( 'NONE',  ( -0.07600661141688493105, 0.08819060268786639567, -0.2415506333044120379 ) ) ;
#35210 = DIRECTION ( 'NONE',  ( 1.000000000000000000, 0.000000000000000000, 0.000000000000000000 ) ) ;
#35211 = CARTESIAN_POINT ( 'NONE',  ( 0.1270800023317771588, 0.1416884738815214761, -0.1270800023317771588 ) ) ;
#35212 = CARTESIAN_POINT ( 'NONE',  ( 0.1264236179284866091, -1.132381889710015743, 0.1264236179284866091 ) ) ;
#35213 = CARTESIAN_POINT ( 'NONE',  ( 0.06523048226347956391, -1.299704724409448398, -0.1574803149606300301 ) ) ;
#35214 = CARTESIAN_POINT ( 'NONE',  ( 0.9873396505805591694, -0.1113553986120547346, 1.215551180994834723 ) ) ;
#35215 = CARTESIAN_POINT ( 'NONE',  ( 0.1559665883013252041, 0.1473510212940076780, -0.02037109575271764048 ) ) ;
#35216 = EDGE_LOOP ( 'NONE', ( #38965, #8431, #21661, #39189 ) ) ;
#35217 = CARTESIAN_POINT ( 'NONE',  ( -0.6971942568897648851, 0.07405724077823318263, 1.934055118056471567 ) ) ;
#35218 = CARTESIAN_POINT ( 'NONE',  ( 1.054774247047244096, 0.000000000000000000, 1.995570866087968520 ) ) ;
#35219 = ORIENTED_EDGE ( 'NONE', *, *, #26865, .F. ) ;
#35220 = CARTESIAN_POINT ( 'NONE',  ( -0.1113553986120547346, -1.439960629813732185, -0.1113553986120547346 ) ) ;
#35221 = CARTESIAN_POINT ( 'NONE',  ( 0.8070866141732283561, 0.000000000000000000, 0.6590551181102368705 ) ) ;
#35222 = B_SPLINE_CURVE_WITH_KNOTS ( 'NONE', 3,
 ( #44262, #40893, #8086, #15068, #15293, #22226, #11235, #29489, #4464, #33770, #18176, #7611, #36859, #18633, #14584, #29945, #29258, #44490, #26079, #19105 ),
 .UNSPECIFIED., .F., .F.,
 ( 4, 1, 1, 1, 1, 1, 2, 2, 1, 1, 1, 2, 2, 4 ),
 ( 0.000000000000000000, 0.2499999999999991118, 0.3749999999999987232, 0.4374999999999983347, 0.4687499999999982792, 0.4843749999999981681, 0.4921874999999980016, 0.4999999999999977796, 0.6249999999999977796, 0.6874999999999978906, 0.7187499999999981126, 0.7343749999999981126, 0.7499999999999982236, 1.000000000000000000 ),
 .UNSPECIFIED. ) ;
#35223 = CARTESIAN_POINT ( 'NONE',  ( -0.8759842519685039353, 0.1787899950787401882, 1.528051181048598384 ) ) ;
#35224 = CARTESIAN_POINT ( 'NONE',  ( 0.08476992594623591892, 0.2465534299916050109, -0.3121915932859317122 ) ) ;
#35225 = ADVANCED_FACE ( 'NONE', ( #14696 ), #518, .T. ) ;
#35226 = CARTESIAN_POINT ( 'NONE',  ( -1.054774247047244096, 0.000000000000000000, 0.9670275590013542866 ) ) ;
#35227 = CARTESIAN_POINT ( 'NONE',  ( -1.054774247047244540, -0.07405724077823318263, 0.2214566928596220785 ) ) ;
#35228 = AXIS2_PLACEMENT_3D ( 'NONE', #22935, #1110, #23180 ) ;
#35229 = CARTESIAN_POINT ( 'NONE',  ( -0.7646288533564489232, 0.1113553986120547346, 0.5757874015748032370 ) ) ;
#35230 = CARTESIAN_POINT ( 'NONE',  ( -0.9500414927467378812, 0.1787899950787401604, 1.924212598371433325 ) ) ;
#35231 = CARTESIAN_POINT ( 'NONE',  ( -0.8019270111902717657, -0.1787899950787401604, 0.1328740156942679607 ) ) ;
#35232 = CARTESIAN_POINT ( 'NONE',  ( 0.05467468201772719694, -0.07678538764759434976, -0.2538665577330192491 ) ) ;
#35233 = CARTESIAN_POINT ( 'NONE',  ( -0.9412147342319837628, 0.1574803149606300301, 1.788877952755905332 ) ) ;
#35234 = FACE_OUTER_BOUND ( 'NONE', #40240, .T. ) ;
#35235 = CARTESIAN_POINT ( 'NONE',  ( 3.284318927891251994E-17, -0.2821121572056168869, 0.1787899950787401882 ) ) ;
#35236 = CARTESIAN_POINT ( 'NONE',  ( 0.1908586082815771912, -0.09842519685039370636, -0.07077711205430314845 ) ) ;
#35237 = CARTESIAN_POINT ( 'NONE',  ( 0.4451448144122268080, 1.417321315443419438, -0.2957149730314338476 ) ) ;
#35238 = PLANE ( 'NONE',  #31831 ) ;
#35239 = VECTOR ( 'NONE', #34291, 39.37007874015748143 ) ;
#35240 = ( BOUNDED_CURVE ( )  B_SPLINE_CURVE ( 2, ( #18971, #27153, #4338, #8908, #37915, #12764, #23054, #37674, #4826 ),
 .UNSPECIFIED., .F., .T. ) 
 B_SPLINE_CURVE_WITH_KNOTS ( ( 3, 2, 2, 2, 3 ),
 ( 0.000000000000000000, 0.002500000000000000052, 0.005000000000000000104, 0.007499999999999998855, 0.01000000000000000021 ),
 .UNSPECIFIED. ) 
 CURVE ( )  GEOMETRIC_REPRESENTATION_ITEM ( )  RATIONAL_B_SPLINE_CURVE ( ( 1.000000000000000000, 0.9238795325112869605, 1.000000000000000000, 0.9238795325112869605, 1.000000000000000000, 0.9238795325112869605, 1.000000000000000000, 0.9238795325112869605, 1.000000000000000000 ) ) 
 REPRESENTATION_ITEM ( '' )  ) ;
#35241 = VERTEX_POINT ( 'NONE', #15176 ) ;
#35242 = EDGE_LOOP ( 'NONE', ( #16519, #2836, #27837, #30917 ) ) ;
#35243 = CARTESIAN_POINT ( 'NONE',  ( 0.1787899950787401604, -1.046259842465921297, -0.07405724077823318263 ) ) ;
#35244 = CARTESIAN_POINT ( 'NONE',  ( 0.1787899950787401604, -1.198818897584032150, -0.07405724077823318263 ) ) ;
#35245 = EDGE_CURVE ( 'NONE', #13881, #33816, #29819, .T. ) ;
#35246 = DIRECTION ( 'NONE',  ( -0.000000000000000000, 0.7880107536067207930, -0.6156614753256598460 ) ) ;
#35247 = CARTESIAN_POINT ( 'NONE',  ( -0.1797182628040039365, -0.5522091639137544083, 0.000000000000000000 ) ) ;
#35248 = DIRECTION ( 'NONE',  ( 1.000000000000000000, 0.000000000000000000, 0.000000000000000000 ) ) ;
#35249 = CARTESIAN_POINT ( 'NONE',  ( -0.7185039370078739607, 1.928577636452523993E-17, 0.7677165353255432922 ) ) ;
#35250 = CARTESIAN_POINT ( 'NONE',  ( -0.7185039370078739607, 1.928577636452523993E-17, 0.6594488188976378451 ) ) ;
#35251 = CARTESIAN_POINT ( 'NONE',  ( 0.1574803149606299191, 0.07086614173228346358, -1.928577636452523993E-17 ) ) ;
#35252 = ADVANCED_FACE ( 'NONE', ( #11572 ), #46882, .T. ) ;
#35253 = CARTESIAN_POINT ( 'NONE',  ( 0.8019270111902717657, -0.1787899950787401604, 0.9153543306548987957 ) ) ;
#35254 = CARTESIAN_POINT ( 'NONE',  ( 0.1849324350982721465, -0.1887234410765286363, -0.04495255068440705964 ) ) ;
#35255 = ( BOUNDED_CURVE ( )  B_SPLINE_CURVE ( 2, ( #47330, #14501, #39638, #36323, #32259, #6587, #10202, #40115, #21928 ),
 .UNSPECIFIED., .F., .T. ) 
 B_SPLINE_CURVE_WITH_KNOTS ( ( 3, 2, 2, 2, 3 ),
 ( 0.2500000000000000000, 0.2525000000000000022, 0.2550000000000000044, 0.2575000000000000067, 0.2600000000000000089 ),
 .UNSPECIFIED. ) 
 CURVE ( )  GEOMETRIC_REPRESENTATION_ITEM ( )  RATIONAL_B_SPLINE_CURVE ( ( 1.000000000000000000, 0.9238795325112869605, 1.000000000000000000, 0.9238795325112869605, 1.000000000000000000, 0.9238795325112869605, 1.000000000000000000, 0.9238795325112869605, 1.000000000000000000 ) ) 
 REPRESENTATION_ITEM ( '' )  ) ;
#35256 = CONICAL_SURFACE ( 'NONE', #8440, 0.1574803149606299191, 0.9599310885968735940 ) ;
#35258 = CARTESIAN_POINT ( 'NONE',  ( 0.1631207519397703531, -0.1587913448376755687, -0.006047451551306580811 ) ) ;
#35257 = CARTESIAN_POINT ( 'NONE',  ( 0.9412147342319837628, 0.1574803149606300301, 0.6077755905511815770 ) ) ;
#35259 = CARTESIAN_POINT ( 'NONE',  ( 0.9412147342319837628, -0.1574803149606297803, 1.094980314853103653 ) ) ;
#35260 = CARTESIAN_POINT ( 'NONE',  ( 1.033464566929133799, 0.000000000000000000, 0.03937007863263043694 ) ) ;
#35261 = CONICAL_SURFACE ( 'NONE', #1562, 0.2559055118110236116, 1.047197551196597409 ) ;
#35262 = ORIENTED_EDGE ( 'NONE', *, *, #38476, .F. ) ;
#35263 = FACE_OUTER_BOUND ( 'NONE', #30693, .T. ) ;
#35264 = CARTESIAN_POINT ( 'NONE',  ( 0.07405724077823318263, -0.6624015747493856576, 0.1787899950787401604 ) ) ;
#35265 = CIRCLE ( 'NONE', #4604, 0.09842519685039370636 ) ;
#35266 = CARTESIAN_POINT ( 'NONE',  ( 0.1264236179284866091, -1.353838582623401621, -0.1264236179284866091 ) ) ;
#35267 = CARTESIAN_POINT ( 'NONE',  ( -0.9500414927467378812, 0.1787899950787401604, 1.840551181048599938 ) ) ;
#35268 = VERTEX_POINT ( 'NONE', #25244 ) ;
#35269 = CARTESIAN_POINT ( 'NONE',  ( -0.9500414927467378812, 0.1787899950787401604, 1.491141732229701367 ) ) ;
#35270 = CARTESIAN_POINT ( 'NONE',  ( 0.8019270111902717657, -0.1787899950787401604, 1.432086614119464141 ) ) ;
#35271 = CARTESIAN_POINT ( 'NONE',  ( -0.7185039370078746268, -0.06523048226347956391, 0.8981299212598432558 ) ) ;
#35272 = CARTESIAN_POINT ( 'NONE',  ( -0.6971942568897626646, -0.07405724077823297447, 0.7185039369541108556 ) ) ;
#35273 = CARTESIAN_POINT ( 'NONE',  ( 0.1574803149606300023, -0.4075443641102559078, -0.9311509272141712534 ) ) ;
#35274 = CARTESIAN_POINT ( 'NONE',  ( -0.9873396505805591694, 0.1113553986120547346, 1.619094488081448846 ) ) ;
#35275 = CARTESIAN_POINT ( 'NONE',  ( -0.9500414927467377701, -0.1787899950787401604, 0.6053149605761580787 ) ) ;
#35276 = EDGE_CURVE ( 'NONE', #47215, #16187, #18687, .T. ) ;
#35277 = CARTESIAN_POINT ( 'NONE',  ( 0.1235961452251413406, -0.09842519685039370636, 0.2140748031496062798 ) ) ;
#35278 = CARTESIAN_POINT ( 'NONE',  ( -1.033464566929133799, 0.000000000000000000, 0.3248031496062992463 ) ) ;
#35279 = VERTEX_POINT ( 'NONE', #22580 ) ;
#35280 = CARTESIAN_POINT ( 'NONE',  ( -0.8759842519685039353, 0.1787899950787401882, 1.493602362150960650 ) ) ;
#35281 = VERTEX_POINT ( 'NONE', #19449 ) ;
#35282 = CARTESIAN_POINT ( 'NONE',  ( -0.9412147342319837628, -0.1574803149606297803, 0.5142716535433068392 ) ) ;
#35283 = CARTESIAN_POINT ( 'NONE',  ( 0.8019270111902716547, 0.1787899950787401604, 1.259842519631276359 ) ) ;
#35284 = CARTESIAN_POINT ( 'NONE',  ( 0.1643129700501710921, -0.09851384408417600269, -0.1153281366345470377 ) ) ;
#35285 = ORIENTED_EDGE ( 'NONE', *, *, #19482, .T. ) ;
#35286 = FACE_OUTER_BOUND ( 'NONE', #33116, .T. ) ;
#35287 = CARTESIAN_POINT ( 'NONE',  ( -0.6971942568897648851, -0.07405724077823297447, 1.033464566875371027 ) ) ;
#35288 = ORIENTED_EDGE ( 'NONE', *, *, #23784, .T. ) ;
#35289 = CARTESIAN_POINT ( 'NONE',  ( -0.1787899950787401604, -1.554257826496955097, -0.07405724077823318263 ) ) ;
#35290 = VERTEX_POINT ( 'NONE', #41000 ) ;
#35291 = CARTESIAN_POINT ( 'NONE',  ( -0.07405724077823318263, -0.6377952755367874982, -0.1787899950787401604 ) ) ;
#35292 = LINE ( 'NONE', #21115, #37669 ) ;
#35293 = CIRCLE ( 'NONE', #30719, 0.09842519685039370636 ) ;
#35294 = VECTOR ( 'NONE', #12507, 39.37007874015748854 ) ;
#35295 = CARTESIAN_POINT ( 'NONE',  ( -0.1264236179284866091, -0.2760826771115909573, 0.1264236179284866091 ) ) ;
#35296 = CARTESIAN_POINT ( 'NONE',  ( 0.07405724077823318263, -0.7608267715997808489, -0.1787899950787401604 ) ) ;
#35297 = EDGE_CURVE ( 'NONE', #34488, #28708, #43039, .T. ) ;
#35298 = DIRECTION ( 'NONE',  ( 0.000000000000000000, 0.000000000000000000, -1.000000000000000000 ) ) ;
#35299 = DIRECTION ( 'NONE',  ( 1.000000000000000000, -5.464378949326940770E-15, 4.275490733183370330E-15 ) ) ;
#35300 = CARTESIAN_POINT ( 'NONE',  ( 0.1787899950787401604, 0.0008602837392652073079, 0.07405724077823318263 ) ) ;
#35301 = CARTESIAN_POINT ( 'NONE',  ( -0.07405724077823318263, 0.02657480320336980464, -0.1787899950787401604 ) ) ;
#35302 = CONTEXT_DEPENDENT_SHAPE_REPRESENTATION ( #16242, #29568 ) ;
#35303 = CARTESIAN_POINT ( 'NONE',  ( 0.1033725344634994631, -0.09842519685039372024, 0.1327416431847782963 ) ) ;
#35304 = ADVANCED_FACE ( 'NONE', ( #15885 ), #8662, .T. ) ;
#35305 = CARTESIAN_POINT ( 'NONE',  ( 1.002407869896990045, -0.1264236179284866091, 0.5290354330171024300 ) ) ;
#35306 = CARTESIAN_POINT ( 'NONE',  ( -0.8759842519685039353, -0.1787899950787401882, 0.8439960629383622681 ) ) ;
#35308 = DIRECTION ( 'NONE',  ( 1.822029033848725028E-16, 0.000000000000000000, 1.000000000000000000 ) ) ;
#35307 = CARTESIAN_POINT ( 'NONE',  ( -9.642888182262618425E-18, -0.9429133858267716439, -0.1574803149606299191 ) ) ;
#35310 = CARTESIAN_POINT ( 'NONE',  ( -0.7244611917879343332, -0.07363402883329660253, 1.984689699691266851 ) ) ;
#35309 = CARTESIAN_POINT ( 'NONE',  ( 0.1270800023317771588, -1.718547746590919356, 0.1270800023317771588 ) ) ;
#35311 = CARTESIAN_POINT ( 'NONE',  ( 1.054774247047244540, 0.07405724077823318263, 1.446850393647023614 ) ) ;
#35313 = DIRECTION ( 'NONE',  ( 1.822029033848725028E-16, 0.000000000000000000, 1.000000000000000000 ) ) ;
#35312 = DIRECTION ( 'NONE',  ( 0.6018150231520412730, 0.000000000000000000, -0.7986355100472980473 ) ) ;
#35314 = CARTESIAN_POINT ( 'NONE',  ( 0.7495606340400177148, -0.1264236179284866091, 0.3223425196312759144 ) ) ;
#35315 = ORIENTED_EDGE ( 'NONE', *, *, #33207, .T. ) ;
#35317 = ORIENTED_EDGE ( 'NONE', *, *, #24044, .F. ) ;
#35316 = CARTESIAN_POINT ( 'NONE',  ( -0.1588219152425539016, -0.09266989036297289262, -0.1937372027062211621 ) ) ;
#35318 = CARTESIAN_POINT ( 'NONE',  ( 0.8759842519685039353, -0.1574803149606299191, 0.8562992124908976876 ) ) ;
#35319 = CARTESIAN_POINT ( 'NONE',  ( 0.1264236179284866091, -0.1481299212060789294, 0.1264236179284866091 ) ) ;
#35320 = CARTESIAN_POINT ( 'NONE',  ( 0.8759842519685039353, -0.1787899950787401882, 0.6028543306548976854 ) ) ;
#35321 = CARTESIAN_POINT ( 'NONE',  ( 0.07405724077823318263, -0.8937007873478103326, 0.1787899950787401604 ) ) ;
#35322 = CARTESIAN_POINT ( 'NONE',  ( 0.7606907602897685639, -0.1191966515041183866, 0.03937009332876739015 ) ) ;
#35323 = CARTESIAN_POINT ( 'NONE',  ( -1.033464566929133799, 0.000000000000000000, 0.9448818896562519720 ) ) ;
#35324 = AXIS2_PLACEMENT_3D ( 'NONE', #41745, #1500, #27192 ) ;
#35325 = CARTESIAN_POINT ( 'NONE',  ( -0.8759842519685039353, 0.1787899950787401882, 1.488681102308440751 ) ) ;
#35326 = EDGE_LOOP ( 'NONE', ( #45547, #20857, #19632, #27380 ) ) ;
#35327 = CARTESIAN_POINT ( 'NONE',  ( -0.2896766839110012648, -0.1108097609387615201, -0.7501563460709702591 ) ) ;
#35328 = CARTESIAN_POINT ( 'NONE',  ( 1.002407869896990045, 0.1264236179284866091, 0.9768700786863937502 ) ) ;
#35329 = ORIENTED_EDGE ( 'NONE', *, *, #16209, .F. ) ;
#35330 = AXIS2_PLACEMENT_3D ( 'NONE', #4673, #19302, #5388 ) ;
#35331 = AXIS2_PLACEMENT_3D ( 'NONE', #4073, #15123, #29769 ) ;
#35332 = CARTESIAN_POINT ( 'NONE',  ( -0.9500414927467378812, 0.1787899950787401604, 0.8956692912848198684 ) ) ;
#35333 = CARTESIAN_POINT ( 'NONE',  ( 0.1574803149606299746, 1.174718201258053485, -3.430321324600322352 ) ) ;
#35334 = DIRECTION ( 'NONE',  ( -3.469446951953614189E-15, -1.000000000000000000, 0.000000000000000000 ) ) ;
#35335 = CARTESIAN_POINT ( 'NONE',  ( 0.7495606340400177148, 0.1264236179284866091, 0.08120078734781142893 ) ) ;
#35336 = CARTESIAN_POINT ( 'NONE',  ( -0.8759842519685039353, 0.1787899950787401882, 0.1107283464029295283 ) ) ;
#35337 = CIRCLE ( 'NONE', #26159, 0.1864803149606298893 ) ;
#35338 = CARTESIAN_POINT ( 'NONE',  ( 0.8759842519685039353, 0.1574803149606299191, 1.348425196742866206 ) ) ;
#35339 = ORIENTED_EDGE ( 'NONE', *, *, #22221, .F. ) ;
#35340 = DIRECTION ( 'NONE',  ( -1.000000000000000000, 0.000000000000000000, 0.000000000000000000 ) ) ;
#35341 = CARTESIAN_POINT ( 'NONE',  ( -1.002407869896990045, -0.1264236179284866091, 1.749507873961984483 ) ) ;
#35342 = B_SPLINE_CURVE_WITH_KNOTS ( 'NONE', 3,
 ( #44141, #36507, #3662, #40531, #18517, #18285, #32927, #48, #29369, #11111, #25731, #40302, #33169, #7720, #33400, #517, #33873, #22811, #1704, #22579, #26671, #41707 ),
 .UNSPECIFIED., .F., .F.,
 ( 4, 2, 2, 2, 2, 2, 2, 2, 2, 2, 4 ),
 ( 0.000000000000000000, 0.1250000000000000555, 0.1875000000000000833, 0.2187500000000001943, 0.2500000000000002776, 0.5000000000000004441, 0.6250000000000005551, 0.6875000000000006661, 0.7187500000000006661, 0.7500000000000006661, 1.000000000000000000 ),
 .UNSPECIFIED. ) ;
#35343 = CARTESIAN_POINT ( 'NONE',  ( -0.2471922904502826257, 0.08811029028640915417, -0.05516800237527129391 ) ) ;
#35344 = CARTESIAN_POINT ( 'NONE',  ( -0.9412147342319837628, -0.1574803149606297803, 0.7898622047244097111 ) ) ;
#35345 = CARTESIAN_POINT ( 'NONE',  ( 0.07405724077823318263, -1.170399558780419680, -0.1787899950787401604 ) ) ;
#35346 = ORIENTED_EDGE ( 'NONE', *, *, #47454, .T. ) ;
#35347 = CARTESIAN_POINT ( 'NONE',  ( -0.1787899950787401604, -0.1604330708123782034, -0.07405724077823318263 ) ) ;
#35348 = ORIENTED_EDGE ( 'NONE', *, *, #34709, .F. ) ;
#35349 = EDGE_CURVE ( 'NONE', #2870, #36693, #8898, .T. ) ;
#35350 = ORIENTED_EDGE ( 'NONE', *, *, #32490, .F. ) ;
#35351 = CARTESIAN_POINT ( 'NONE',  ( -0.1574803149606299191, 1.126631386849004990, -3.440787370833234604 ) ) ;
#35352 = VECTOR ( 'NONE', #26543, 39.37007874015748143 ) ;
#35353 = EDGE_CURVE ( 'NONE', #41157, #39149, #19322, .T. ) ;
#35354 = CARTESIAN_POINT ( 'NONE',  ( 0.7185039370078739607, 1.928577636452523993E-17, 1.801181102362204633 ) ) ;
#35355 = CARTESIAN_POINT ( 'NONE',  ( -0.1797182628040039365, -0.1978784552523369933, 0.000000000000000000 ) ) ;
#35356 = AXIS2_PLACEMENT_3D ( 'NONE', #26932, #1485, #4364 ) ;
#35357 = CIRCLE ( 'NONE', #20797, 0.1003937007874010356 ) ;
#35358 = CARTESIAN_POINT ( 'NONE',  ( -0.07405724077823318263, -0.8001968503399367050, -0.1787899950787401604 ) ) ;
#35359 = CARTESIAN_POINT ( 'NONE',  ( -0.6971942568897637749, 2.189545951927499583E-17, 0.2829724408911185041 ) ) ;
#35360 = CARTESIAN_POINT ( 'NONE',  ( -0.8107537697050253289, 0.1574803149606300301, 1.085137795275590955 ) ) ;
#35361 = CARTESIAN_POINT ( 'NONE',  ( -0.1797182628040039087, -1.140299715094857502, 0.07444174185955065859 ) ) ;
#35362 = CARTESIAN_POINT ( 'NONE',  ( -0.1667418150844807434, 0.1992258004382155001, -0.03573910814353464110 ) ) ;
#35363 = CARTESIAN_POINT ( 'NONE',  ( 1.002407869896990045, -0.1264236179284866091, 1.045767716481669440 ) ) ;
#35364 = CARTESIAN_POINT ( 'NONE',  ( 0.6971942568897648851, 0.07405724077823318263, 1.535433070812378675 ) ) ;
#35365 = CARTESIAN_POINT ( 'NONE',  ( 1.054774247047244540, -0.07405724077823318263, 0.1771653542769450751 ) ) ;
#35366 = DIRECTION ( 'NONE',  ( 0.000000000000000000, 1.000000000000000000, 0.000000000000000000 ) ) ;
#35367 = CARTESIAN_POINT ( 'NONE',  ( 0.7185039370078746268, -0.06523048226347956391, 1.685531496062990797 ) ) ;
#35369 = DIRECTION ( 'NONE',  ( 0.000000000000000000, 0.000000000000000000, 1.000000000000000000 ) ) ;
#35368 = CARTESIAN_POINT ( 'NONE',  ( -0.1574803149606299191, 0.3743908788525360798, -3.616772362661643925 ) ) ;
#35370 = FACE_OUTER_BOUND ( 'NONE', #20399, .T. ) ;
#35371 = CARTESIAN_POINT ( 'NONE',  ( -0.7185039370078746268, 0.06523048226347956391, 1.670767716427906002 ) ) ;
#35372 = PLANE ( 'NONE',  #4633 ) ;
#35373 = CARTESIAN_POINT ( 'NONE',  ( 1.054774247047244540, -0.07405724077823318263, 1.161417322780881278 ) ) ;
#35374 = FACE_OUTER_BOUND ( 'NONE', #41931, .T. ) ;
#35375 = CARTESIAN_POINT ( 'NONE',  ( -0.8759842519685039353, 0.1787899950787401882, 1.134350393647023614 ) ) ;
#35376 = CARTESIAN_POINT ( 'NONE',  ( 0.8759842519685039353, -0.1574803149606299191, 0.4232283463491653963 ) ) ;
#35377 = ORIENTED_EDGE ( 'NONE', *, *, #33363, .F. ) ;
#35378 = DIRECTION ( 'NONE',  ( -1.000000000000000000, 0.000000000000000000, 0.000000000000000000 ) ) ;
#35379 = CARTESIAN_POINT ( 'NONE',  ( 0.9412147342319837628, 0.1574803149606300301, 0.2534448818897637734 ) ) ;
#35380 = CARTESIAN_POINT ( 'NONE',  ( 0.1113553986120547346, -1.016732283357039357, -0.1113553986120547346 ) ) ;
#35381 = CARTESIAN_POINT ( 'NONE',  ( -0.7646288533564489232, 0.1113553986120547346, 0.2903543306011346359 ) ) ;
#35382 = EDGE_LOOP ( 'NONE', ( #24592, #16471, #42017, #1171 ) ) ;
#35383 = CARTESIAN_POINT ( 'NONE',  ( 0.6971942568897648851, -0.07405724077823297447, 1.225393700733637514 ) ) ;
#35385 = CARTESIAN_POINT ( 'NONE',  ( 0.7185039370078746268, -0.06523048226347956391, 0.06151574792396910518 ) ) ;
#35384 = DIRECTION ( 'NONE',  ( 1.000000000000000000, 0.000000000000000000, -4.336808689942015271E-16 ) ) ;
#35386 = DIMENSIONAL_EXPONENTS ( 1.000000000000000000, 0.000000000000000000, 0.000000000000000000, 0.000000000000000000, 0.000000000000000000, 0.000000000000000000, 0.000000000000000000 ) ;
#35387 = CARTESIAN_POINT ( 'NONE',  ( 3.284318927891251994E-17, -0.03001968498560657339, 0.1787899950787401882 ) ) ;
#35388 = CARTESIAN_POINT ( 'NONE',  ( 1.033464566929133799, 0.000000000000000000, 0.7185039370078739607 ) ) ;
#35389 = ORIENTED_EDGE ( 'NONE', *, *, #23328, .F. ) ;
#35390 = LINE ( 'NONE', #25061, #5311 ) ;
#35391 = DIRECTION ( 'NONE',  ( 0.000000000000000000, 0.000000000000000000, -1.000000000000000000 ) ) ;
#35392 = ORIENTED_EDGE ( 'NONE', *, *, #17851, .F. ) ;
#35393 = CARTESIAN_POINT ( 'NONE',  ( -1.054774247047244540, 0.07405724077823318263, 1.323818897584032594 ) ) ;
#35394 = CARTESIAN_POINT ( 'NONE',  ( -0.07405724077823318263, -1.730314960576156968, 0.1787899950787401604 ) ) ;
#35395 = CARTESIAN_POINT ( 'NONE',  ( -0.8019270111902717657, -0.1787899950787401604, 0.9990157479777320715 ) ) ;
#35396 = AXIS2_PLACEMENT_3D ( 'NONE', #6500, #21120, #35754 ) ;
#35397 = CIRCLE ( 'NONE', #36179, 0.09842519685039317900 ) ;
#35398 = CARTESIAN_POINT ( 'NONE',  ( -0.9500414927467378812, -0.1787899950787401604, 1.983267716481667886 ) ) ;
#35399 = ORIENTED_EDGE ( 'NONE', *, *, #7041, .T. ) ;
#35400 = EDGE_CURVE ( 'NONE', #43655, #2549, #5572, .T. ) ;
#35401 = CARTESIAN_POINT ( 'NONE',  ( -1.054774247047244096, 0.000000000000000000, 1.006397637741511808 ) ) ;
#35402 = CARTESIAN_POINT ( 'NONE',  ( -0.9500414927467378812, -0.1787899950787401604, 0.6496062991588353874 ) ) ;
#35403 = CARTESIAN_POINT ( 'NONE',  ( 0.9873396505805591694, -0.1113553986120547346, 1.815944881889763884 ) ) ;
#35404 = DIRECTION ( 'NONE',  ( 1.000000000000000000, 0.000000000000000000, -1.822029033848725275E-16 ) ) ;
#35405 = CARTESIAN_POINT ( 'NONE',  ( -0.07405724077823318263, -0.6536672753158522253, -0.1787899950787401604 ) ) ;
#35406 = TOROIDAL_SURFACE ( 'NONE', #30840, 0.1870078740157480324, 0.04921259842519685318 ) ;
#35407 = EDGE_LOOP ( 'NONE', ( #6730, #22535, #29956, #17439 ) ) ;
#35408 = CARTESIAN_POINT ( 'NONE',  ( -0.1639377702882210686, -0.08956143926285886625, 0.03448135181225767815 ) ) ;
#35409 = EDGE_CURVE ( 'NONE', #17977, #16297, #25468, .T. ) ;
#35410 = VERTEX_POINT ( 'NONE', #26904 ) ;
#35411 = FACE_OUTER_BOUND ( 'NONE', #44047, .T. ) ;
#35412 = CARTESIAN_POINT ( 'NONE',  ( -1.002407869896990045, -0.1264236179284866091, 0.6077755904974173617 ) ) ;
#35413 = CARTESIAN_POINT ( 'NONE',  ( 0.1113553986120547346, -0.01279527559055118092, 0.1113553986120547346 ) ) ;
#35414 = DIRECTION ( 'NONE',  ( 1.000000000000000000, 0.000000000000000000, 0.000000000000000000 ) ) ;
#35415 = VECTOR ( 'NONE', #35032, 39.37007874015748143 ) ;
#35416 = DIRECTION ( 'NONE',  ( 0.000000000000000000, -1.756682000989171636E-15, 1.000000000000000000 ) ) ;
#35417 = EDGE_LOOP ( 'NONE', ( #11071, #24914, #28948, #42809 ) ) ;
#35418 = CARTESIAN_POINT ( 'NONE',  ( 0.7646288533564489232, -0.1113553986120547346, 0.5462598425196850682 ) ) ;
#35419 = CARTESIAN_POINT ( 'NONE',  ( 0.1797182628040039087, -0.6530949906854075504, 0.07444174185955046430 ) ) ;
#35420 = DIRECTION ( 'NONE',  ( 0.000000000000000000, -0.7907053606985338101, 0.6121968903568536513 ) ) ;
#35421 = CARTESIAN_POINT ( 'NONE',  ( -1.033464566929134687, -0.06523048226347956391, 1.375492125876724980 ) ) ;
#35423 = CARTESIAN_POINT ( 'NONE',  ( -0.1509072091341974453, -0.09842519685039369248, 0.07426438480369451645 ) ) ;
#35422 = CARTESIAN_POINT ( 'NONE',  ( -0.1574803149606297803, -0.5369094488188979053, 0.06523048226347956391 ) ) ;
#35424 = AXIS2_PLACEMENT_3D ( 'NONE', #30040, #44583, #40288 ) ;
#35425 = CARTESIAN_POINT ( 'NONE',  ( 1.033464566929133799, 1.928577636452524610E-17, 4.498031496062992574 ) ) ;
#35426 = ORIENTED_EDGE ( 'NONE', *, *, #21966, .T. ) ;
#35427 = CARTESIAN_POINT ( 'NONE',  ( 0.4620708661417355922, 0.9842519685039370358, -1.186023622047243986 ) ) ;
#35428 = CARTESIAN_POINT ( 'NONE',  ( 0.8107537697050253289, -0.1574803149606297803, 1.218011811023622437 ) ) ;
#35429 = CARTESIAN_POINT ( 'NONE',  ( 0.06523048226347956391, 0.07332677176107038619, 0.1574803149606297803 ) ) ;
#35431 = DIRECTION ( 'NONE',  ( 0.000000000000000000, 0.6156614753256575145, 0.7880107536067224583 ) ) ;
#35430 = DIRECTION ( 'NONE',  ( -1.000000000000000000, 0.000000000000000000, 0.000000000000000000 ) ) ;
#35432 = CARTESIAN_POINT ( 'NONE',  ( 1.033464566929136907, -0.06523048226347749612, 1.857775590551182798 ) ) ;
#35433 = VERTEX_POINT ( 'NONE', #12533 ) ;
#35435 = CARTESIAN_POINT ( 'NONE',  ( -0.3161444924769541420, 0.8918838478058933594, -1.034309214090480822 ) ) ;
#35434 = CARTESIAN_POINT ( 'NONE',  ( 0.8759842519685039353, -0.1787899950787401882, 0.6815944881352126172 ) ) ;
#35436 = DIRECTION ( 'NONE',  ( -1.000000000000000000, 0.000000000000000000, 0.000000000000000000 ) ) ;
#35437 = ORIENTED_EDGE ( 'NONE', *, *, #46459, .F. ) ;
#35438 = CIRCLE ( 'NONE', #20871, 0.1567662409572586624 ) ;
#35439 = CARTESIAN_POINT ( 'NONE',  ( 0.002794899976010023664, 0.1008940036866861484, -0.1008370195738217678 ) ) ;
#35440 = CARTESIAN_POINT ( 'NONE',  ( 1.002407869896990045, 0.1264236179284866091, 0.8932086613635591421 ) ) ;
#35441 = DIRECTION ( 'NONE',  ( 0.000000000000000000, -1.000000000000000000, 0.000000000000000000 ) ) ;
#35442 = DIRECTION ( 'NONE',  ( 0.000000000000000000, 0.000000000000000000, -1.000000000000000000 ) ) ;
#35443 = CARTESIAN_POINT ( 'NONE',  ( 3.284318927891251994E-17, -1.801673228292693052, 0.1787899950787401882 ) ) ;
#35444 = CARTESIAN_POINT ( 'NONE',  ( 0.07405724077823318263, -1.016732283410803905, 0.1787899950787401604 ) ) ;
#35445 = CARTESIAN_POINT ( 'NONE',  ( -0.1574803149606300301, -1.407972440944881942, -0.06523048226347956391 ) ) ;
#35446 = CARTESIAN_POINT ( 'NONE',  ( 0.1586955767088463476, 0.09170575825942825499, -0.1167515185291642249 ) ) ;
#35447 = CARTESIAN_POINT ( 'NONE',  ( -0.6971942568897648851, 0.07405724077823318263, 1.855314960576157635 ) ) ;
#35448 = CARTESIAN_POINT ( 'NONE',  ( 0.8759842519685039353, -0.1787899950787401882, 1.985728346402929168 ) ) ;
#35449 = VERTEX_POINT ( 'NONE', #16352 ) ;
#35450 = CARTESIAN_POINT ( 'NONE',  ( -1.002407869896990045, -0.1264236179284866091, 1.872539370024976391 ) ) ;
#35451 = CARTESIAN_POINT ( 'NONE',  ( -0.7495606340400177148, -0.1264236179284866091, 1.542814960576157413 ) ) ;
#35452 = CARTESIAN_POINT ( 'NONE',  ( 0.06871726393438436220, 0.2558202476623961386, -0.3098131533094667933 ) ) ;
#35453 = EDGE_CURVE ( 'NONE', #10984, #19760, #35240, .T. ) ;
#35454 = CARTESIAN_POINT ( 'NONE',  ( -0.8019270111902717657, -0.1787899950787401604, 0.2116141731745827814 ) ) ;
#35455 = EDGE_CURVE ( 'NONE', #18349, #8537, #45070, .T. ) ;
#35456 = AXIS2_PLACEMENT_3D ( 'NONE', #13029, #12563, #27188 ) ;
#35457 = CARTESIAN_POINT ( 'NONE',  ( -0.1594274916601879644, 0.09247100924357856688, -0.1933875656399054732 ) ) ;
#35458 = CARTESIAN_POINT ( 'NONE',  ( -1.054774247047244540, -0.07405724077823318263, 1.953740157426552715 ) ) ;
#35459 = CARTESIAN_POINT ( 'NONE',  ( -0.7646288533564489232, 0.1113553986120547346, 1.835629921259842590 ) ) ;
#35460 = CYLINDRICAL_SURFACE ( 'NONE', #16716, 0.1574803149606299191 ) ;
#35461 = CARTESIAN_POINT ( 'NONE',  ( 0.1787899950787401882, -0.2722696375205775898, -2.189545951927503898E-17 ) ) ;
#35462 = CARTESIAN_POINT ( 'NONE',  ( 0.1225656093788251993, -0.09842519685039370636, 0.1799294716465091037 ) ) ;
#35463 = CARTESIAN_POINT ( 'NONE',  ( -0.1113553986120547346, 0.01673228346456692717, 0.1113553986120547346 ) ) ;
#35464 = CARTESIAN_POINT ( 'NONE',  ( 1.033464566929133799, 0.000000000000000000, 1.062992125876724314 ) ) ;
#35465 = ADVANCED_FACE ( 'NONE', ( #5304 ), #36209, .F. ) ;
#35466 = PRODUCT_DEFINITION_FORMATION_WITH_SPECIFIED_SOURCE ( 'ANY', '', #9398, .NOT_KNOWN. ) ;
#35467 = AXIS2_PLACEMENT_3D ( 'NONE', #29713, #44260, #3788 ) ;
#35468 = ADVANCED_FACE ( 'NONE', ( #33633 ), #2486, .F. ) ;
#35469 = CLOSED_SHELL ( 'NONE', ( #3961, #39636, #32226, #9238, #41092, #38899, #22134, #46934, #9282, #34285, #45974, #39375, #35468, #30024 ) ) ;
#35470 = ORIENTED_EDGE ( 'NONE', *, *, #46352, .F. ) ;
#35471 = CARTESIAN_POINT ( 'NONE',  ( -1.002407869896990045, 0.1264236179284866091, 1.213090551127338435 ) ) ;
#35472 = ORIENTED_EDGE ( 'NONE', *, *, #1132, .T. ) ;
#35473 = CARTESIAN_POINT ( 'NONE',  ( 0.07405724077823318263, -1.016732283410803905, 0.1787899950787401604 ) ) ;
#35474 = CARTESIAN_POINT ( 'NONE',  ( 0.1787899950787401604, -1.238188976324190005, -0.07405724077823318263 ) ) ;
#35475 = CARTESIAN_POINT ( 'NONE',  ( -0.7185039370078739607, 0.000000000000000000, -2.869337061179095023E-17 ) ) ;
#35476 = CARTESIAN_POINT ( 'NONE',  ( -0.1270800023317771588, -0.4390201875358015760, -0.1270800023317771588 ) ) ;
#35477 = DIRECTION ( 'NONE',  ( 0.000000000000000000, 6.980778575359379259E-17, -1.000000000000000000 ) ) ;
#35478 = CARTESIAN_POINT ( 'NONE',  ( -0.8759842519685039353, -0.1574803149606299191, 0.7775590550105826448 ) ) ;
#35479 = CARTESIAN_POINT ( 'NONE',  ( -0.7185039370078739607, 1.928577636452523993E-17, 0.7775590551181102983 ) ) ;
#35480 = CARTESIAN_POINT ( 'NONE',  ( 0.1113553986120547346, 0.06594488188976378729, 0.1113553986120547346 ) ) ;
#35481 = ORIENTED_EDGE ( 'NONE', *, *, #44446, .F. ) ;
#35482 = AXIS2_PLACEMENT_3D ( 'NONE', #11030, #28545, #10560 ) ;
#35483 = CARTESIAN_POINT ( 'NONE',  ( 0.7185039370078746268, -0.06523048226347956391, 0.8193897637795271027 ) ) ;
#35484 = CARTESIAN_POINT ( 'NONE',  ( 0.09631076833421682581, -0.2398891842387891882, -0.03294411891277762572 ) ) ;
#35485 = FACE_OUTER_BOUND ( 'NONE', #119, .T. ) ;
#35487 = SURFACE_STYLE_USAGE ( .BOTH. , #28546 ) ;
#35486 = CARTESIAN_POINT ( 'NONE',  ( 0.2559055118110236116, 0.1477471161312045311, -0.1122047244094488277 ) ) ;
#35488 = MANIFOLD_SOLID_BREP ( 'Catch Plate', #35469 ) ;
#35489 = CARTESIAN_POINT ( 'NONE',  ( 1.033464566929134687, 0.06523048226347956391, 0.1205708660342053040 ) ) ;
#35490 = VERTEX_POINT ( 'NONE', #24702 ) ;
#35491 = ORIENTED_EDGE ( 'NONE', *, *, #18190, .T. ) ;
#35492 = DIRECTION ( 'NONE',  ( 0.000000000000000000, -0.000000000000000000, -1.000000000000000000 ) ) ;
#35493 = CARTESIAN_POINT ( 'NONE',  ( -0.1787899950787401604, -0.5590551180564723444, -0.07405724077823318263 ) ) ;
#35494 = LINE ( 'NONE', #42867, #27056 ) ;
#35495 = CARTESIAN_POINT ( 'NONE',  ( -0.1264236179284866091, -1.373523621993480326, 0.1264236179284866091 ) ) ;
#35496 = VERTEX_POINT ( 'NONE', #42186 ) ;
#35497 = CONICAL_SURFACE ( 'NONE', #14077, 0.2471922904502826812, 0.5235987755982992597 ) ;
#35498 = CARTESIAN_POINT ( 'NONE',  ( -0.8019270111902717657, -0.1787899950787401604, 1.432086614119464141 ) ) ;
#35499 = CARTESIAN_POINT ( 'NONE',  ( 1.054774247047244096, 0.000000000000000000, 1.601870078686393750 ) ) ;
#35500 = ORIENTED_EDGE ( 'NONE', *, *, #6553, .T. ) ;
#35501 = CARTESIAN_POINT ( 'NONE',  ( 0.000000000000000000, 0.0004086818895575684884, -0.2204724409448818867 ) ) ;
#35502 = CARTESIAN_POINT ( 'NONE',  ( -0.6971942568897626646, 0.07405724077823318263, 0.5954724408911187261 ) ) ;
#35503 = CARTESIAN_POINT ( 'NONE',  ( 0.9500414927467378812, 0.1787899950787401604, 0.1525590550643468046 ) ) ;
#35504 = CARTESIAN_POINT ( 'NONE',  ( 0.08824861846397512311, -0.09842533983058743274, -0.1554957777122596418 ) ) ;
#35505 = LENGTH_MEASURE_WITH_UNIT ( LENGTH_MEASURE( 0.02539999999999999897 ), #6237 ) ;
#35506 = CARTESIAN_POINT ( 'NONE',  ( 0.9500414927467377701, -0.1787899950787401604, 0.5708661416785200116 ) ) ;
#35507 = CARTESIAN_POINT ( 'NONE',  ( -0.7495606340400177148, -0.1264236179284866091, 0.4798228345919055560 ) ) ;
#35508 = DIRECTION ( 'NONE',  ( 0.000000000000000000, 0.000000000000000000, 1.000000000000000000 ) ) ;
#35509 = ( BOUNDED_CURVE ( )  B_SPLINE_CURVE ( 2, ( #42477, #23110, #41755, #45595, #27446, #19503, #4875, #1278, #23352 ),
 .UNSPECIFIED., .F., .T. ) 
 B_SPLINE_CURVE_WITH_KNOTS ( ( 3, 2, 2, 2, 3 ),
 ( 0.3699999999999999956, 0.3724999999999999978, 0.3750000000000000000, 0.3775000000000000022, 0.3800000000000000044 ),
 .UNSPECIFIED. ) 
 CURVE ( )  GEOMETRIC_REPRESENTATION_ITEM ( )  RATIONAL_B_SPLINE_CURVE ( ( 1.000000000000000000, 0.9238795325112869605, 1.000000000000000000, 0.9238795325112869605, 1.000000000000000000, 0.9238795325112869605, 1.000000000000000000, 0.9238795325112869605, 1.000000000000000000 ) ) 
 REPRESENTATION_ITEM ( '' )  ) ;
#35510 = ADVANCED_FACE ( 'NONE', ( #23764 ), #37426, .F. ) ;
#35511 = DIRECTION ( 'NONE',  ( 1.000000000000000000, 0.000000000000000000, 0.000000000000000000 ) ) ;
#35512 = EDGE_LOOP ( 'NONE', ( #30816, #44428 ) ) ;
#35513 = CARTESIAN_POINT ( 'NONE',  ( -1.054774247047244540, 0.07405724077823318263, 1.407480314906865981 ) ) ;
#35514 = CARTESIAN_POINT ( 'NONE',  ( -0.7185039370078746268, -0.06523048226347956391, 0.3863188976377951445 ) ) ;
#35515 = CARTESIAN_POINT ( 'NONE',  ( 0.6971942568897637749, 2.189545951927499583E-17, 1.267224409395055096 ) ) ;
#35516 = CARTESIAN_POINT ( 'NONE',  ( 0.06845965469993897656, -0.09851384754476909256, 0.2100007770323626122 ) ) ;
#35517 = ORIENTED_EDGE ( 'NONE', *, *, #16236, .F. ) ;
#35518 = EDGE_CURVE ( 'NONE', #10419, #21057, #16582, .T. ) ;
#35519 = CARTESIAN_POINT ( 'NONE',  ( -0.9873396505805591694, -0.1113553986120547346, 0.5561023622047244208 ) ) ;
#35520 = ORIENTED_EDGE ( 'NONE', *, *, #44180, .T. ) ;
#35521 = CARTESIAN_POINT ( 'NONE',  ( 0.07405724077823318263, -1.775714519410341419, 0.1787899950787401604 ) ) ;
#35522 = EDGE_LOOP ( 'NONE', ( #2761, #3572, #7656, #7221, #7672, #36813, #35167, #11660 ) ) ;
#35523 = CARTESIAN_POINT ( 'NONE',  ( 0.1787899950787401604, -0.6525590550643474153, 0.07405724077823318263 ) ) ;
#35524 = CARTESIAN_POINT ( 'NONE',  ( 1.033464566929133799, 0.000000000000000000, 1.624015748031496287 ) ) ;
#35525 = CARTESIAN_POINT ( 'NONE',  ( 0.9412147342319837628, -0.1574803149606297803, 0.3961614173228344415 ) ) ;
#35526 = ORIENTED_EDGE ( 'NONE', *, *, #1789, .F. ) ;
#35527 = CARTESIAN_POINT ( 'NONE',  ( 0.8019270111902717657, -0.1787899950787401604, 1.427165354276944687 ) ) ;
#35528 = CYLINDRICAL_SURFACE ( 'NONE', #23854, 0.1574803149606299191 ) ;
#35529 = ( BOUNDED_CURVE ( )  B_SPLINE_CURVE ( 3, ( #26080, #4236, #3564, #8087 ),
 .UNSPECIFIED., .F., .F. ) 
 B_SPLINE_CURVE_WITH_KNOTS ( ( 4, 4 ),
 ( 3.141592653589813544, 4.712388980384689674 ),
 .UNSPECIFIED. ) 
 CURVE ( )  GEOMETRIC_REPRESENTATION_ITEM ( )  RATIONAL_B_SPLINE_CURVE ( ( 1.000000000000000000, 0.8047378541243698225, 0.8047378541243698225, 1.000000000000000000 ) ) 
 REPRESENTATION_ITEM ( '' )  ) ;
#35530 = CARTESIAN_POINT ( 'NONE',  ( 0.1264236179284866091, -0.6943897637257637756, 0.1264236179284866091 ) ) ;
#35531 = CARTESIAN_POINT ( 'NONE',  ( 1.033464566929134687, -0.06523048226347956391, 0.1943897636720005040 ) ) ;
#35532 = CYLINDRICAL_SURFACE ( 'NONE', #33233, 0.1624015748031507056 ) ;
#35533 = CARTESIAN_POINT ( 'NONE',  ( 0.1264236179284866091, 0.04761225224320220911, -0.1264236179284866091 ) ) ;
#35534 = CARTESIAN_POINT ( 'NONE',  ( -0.07405724077823318263, -0.2687007873478113318, 0.1787899950787401604 ) ) ;
#35535 = CYLINDRICAL_SURFACE ( 'NONE', #16548, 0.1574803149606299191 ) ;
#35536 = CARTESIAN_POINT ( 'NONE',  ( 0.9500414927467378812, -0.1787899950787401604, 0.5265748030958428139 ) ) ;
#35537 = EDGE_CURVE ( 'NONE', #38700, #23237, #41484, .T. ) ;
#35538 = CARTESIAN_POINT ( 'NONE',  ( -1.054774247047244540, -0.07405724077823318263, 0.8120078739619844832 ) ) ;
#35540 = CARTESIAN_POINT ( 'NONE',  ( 1.033464566929134687, 0.06523048226347956391, 0.9867125983176703308 ) ) ;
#35539 = CARTESIAN_POINT ( 'NONE',  ( 2.892866454678787531E-17, -0.9625984251968503491, 0.1574803149606299191 ) ) ;
#35541 = CARTESIAN_POINT ( 'NONE',  ( -0.07444174185955065859, -1.804669793835014469, 0.1797182628040039087 ) ) ;
#35542 = CARTESIAN_POINT ( 'NONE',  ( -0.06523048226347956391, -0.4975393699712130080, -0.1574803149606300301 ) ) ;
#35543 = CARTESIAN_POINT ( 'NONE',  ( 0.1264236179284866091, -0.3695866141194649179, -0.1264236179284866091 ) ) ;
#35544 = CARTESIAN_POINT ( 'NONE',  ( 0.9500414927467378812, 0.1787899950787401604, 1.727362204670645385 ) ) ;
#35546 = CARTESIAN_POINT ( 'NONE',  ( 0.1476377952755906220, 1.126631386849005878, -3.440787370833236380 ) ) ;
#35545 = CARTESIAN_POINT ( 'NONE',  ( 0.9500414927467377701, -0.1787899950787401604, 1.983267716481668108 ) ) ;
#35547 = CARTESIAN_POINT ( 'NONE',  ( 1.054774247047244540, 0.07405724077823318263, 0.3395669290800949480 ) ) ;
#35548 = ORIENTED_EDGE ( 'NONE', *, *, #20354, .F. ) ;
#35549 = APPLICATION_CONTEXT ( 'automotive_design' ) ;
#35550 = DIRECTION ( 'NONE',  ( -1.000000000000000000, 0.000000000000000000, 0.000000000000000000 ) ) ;
#35551 = CARTESIAN_POINT ( 'NONE',  ( 0.1264236179284866091, -0.1874999999462366451, 0.1264236179284866091 ) ) ;
#35552 = CARTESIAN_POINT ( 'NONE',  ( 1.054774247047244540, -0.07405724077823318263, 0.6496062991588353874 ) ) ;
#35553 = CARTESIAN_POINT ( 'NONE',  ( 3.284318927891251994E-17, -0.8961614172690708369, 0.1787899950787401882 ) ) ;
#35554 = CARTESIAN_POINT ( 'NONE',  ( 1.033464566929133799, 0.000000000000000000, 0.08858267716535432601 ) ) ;
#35555 = CARTESIAN_POINT ( 'NONE',  ( -0.8107537697050254399, -0.1574803149606297803, 1.523129921152316379 ) ) ;
#35556 = CARTESIAN_POINT ( 'NONE',  ( -0.8019270111902717657, 0.1787899950787401604, 1.451771653489543290 ) ) ;
#35557 = ORIENTED_EDGE ( 'NONE', *, *, #3461, .F. ) ;
#35558 = AXIS2_PLACEMENT_3D ( 'NONE', #5920, #31817, #1849 ) ;
#35559 = CARTESIAN_POINT ( 'NONE',  ( -0.3100393700787403284, -0.01116717051762143413, -0.7086614173228348301 ) ) ;
#35560 = CARTESIAN_POINT ( 'NONE',  ( 0.9500414927467378812, -0.1787899950787401604, 1.200787401521039355 ) ) ;
#35561 = CIRCLE ( 'NONE', #27943, 0.3912448816427701037 ) ;
#35562 = AXIS2_PLACEMENT_3D ( 'NONE', #44525, #25646, #40687 ) ;
#35563 = CARTESIAN_POINT ( 'NONE',  ( -1.033464566929133799, 0.000000000000000000, 0.7086614172153071767 ) ) ;
#35564 = CARTESIAN_POINT ( 'NONE',  ( 0.7495606340400177148, -0.1264236179284866091, 1.779035433017102319 ) ) ;
#35565 = CARTESIAN_POINT ( 'NONE',  ( -0.9412147342319837628, -0.1574803149606297803, 1.459153543307085688 ) ) ;
#35566 = CARTESIAN_POINT ( 'NONE',  ( -1.002407869896990045, 0.1264236179284866091, 0.9325787401037164415 ) ) ;
#35567 = FACE_OUTER_BOUND ( 'NONE', #39985, .T. ) ;
#35568 = CARTESIAN_POINT ( 'NONE',  ( 0.9500414927467377701, 0.1787899950787401604, 0.07381889758403178958 ) ) ;
#35569 = CARTESIAN_POINT ( 'NONE',  ( 0.9412147342319837628, -0.1574803149606297803, 1.567421259734991690 ) ) ;
#35570 = ORIENTED_EDGE ( 'NONE', *, *, #46516, .T. ) ;
#35571 = EDGE_CURVE ( 'NONE', #36086, #22696, #16877, .T. ) ;
#35572 = DIRECTION ( 'NONE',  ( -1.000000000000000000, 0.000000000000000000, 0.000000000000000000 ) ) ;
#35573 = CARTESIAN_POINT ( 'NONE',  ( 0.2460099227178147996, -0.1534603371579595921, -0.09996720075266711525 ) ) ;
#35574 = CARTESIAN_POINT ( 'NONE',  ( -1.002407869896990045, -0.1264236179284866091, 1.670767716481669440 ) ) ;
#35575 = EDGE_CURVE ( 'NONE', #46991, #44026, #31592, .T. ) ;
#35576 = CARTESIAN_POINT ( 'NONE',  ( -0.2471922904502826812, 0.08342621139836772781, -0.06611980121264428301 ) ) ;
#35577 = CARTESIAN_POINT ( 'NONE',  ( -0.8759842519685039353, 0.000000000000000000, 0.000000000000000000 ) ) ;
#35578 = CARTESIAN_POINT ( 'NONE',  ( -1.094772975963752103E-17, -1.167938928859159509, -0.1787899950787401882 ) ) ;
#35579 = ORIENTED_EDGE ( 'NONE', *, *, #6443, .T. ) ;
#35580 = CARTESIAN_POINT ( 'NONE',  ( -0.07405724077823318263, -0.08661417317458304510, -0.1787899950787401604 ) ) ;
#35581 = ORIENTED_EDGE ( 'NONE', *, *, #24534, .F. ) ;
#35582 = CARTESIAN_POINT ( 'NONE',  ( 0.9500414927467378812, 0.1787899950787401604, 1.092519684985605810 ) ) ;
#35583 = VECTOR ( 'NONE', #34151, 39.37007874015748143 ) ;
#35584 = CARTESIAN_POINT ( 'NONE',  ( -1.033464566929133799, 0.000000000000000000, 1.220472440837354400 ) ) ;
#35585 = CARTESIAN_POINT ( 'NONE',  ( -0.9873396505805591694, 0.1113553986120547346, 0.9104330707586141269 ) ) ;
#35586 = CARTESIAN_POINT ( 'NONE',  ( 0.8107537697050253289, 0.1574803149606300301, 1.754429133858266932 ) ) ;
#35587 = AXIS2_PLACEMENT_3D ( 'NONE', #7158, #37319, #26084 ) ;
#35588 = AXIS2_PLACEMENT_3D ( 'NONE', #5958, #45732, #45258 ) ;
#35589 = CONICAL_SURFACE ( 'NONE', #372, 0.2471922904502826812, 0.5235987755982992597 ) ;
#35590 = VECTOR ( 'NONE', #26585, 39.37007874015748854 ) ;
#35591 = CARTESIAN_POINT ( 'NONE',  ( -0.07405724077823318263, -0.7854330708123791194, 0.1787899950787401604 ) ) ;
#35592 = EDGE_CURVE ( 'NONE', #21809, #752, #182, .T. ) ;
#35594 = CARTESIAN_POINT ( 'NONE',  ( -0.7371950664085656912, 0.08546456393164050813, 1.981527568757507130 ) ) ;
#35593 = CARTESIAN_POINT ( 'NONE',  ( -0.1797182628040039365, -1.300240659976745983, 0.000000000000000000 ) ) ;
#35595 = CARTESIAN_POINT ( 'NONE',  ( -0.9873396505805591694, 0.1113553986120547346, 0.2116141732283464416 ) ) ;
#35596 = CARTESIAN_POINT ( 'NONE',  ( 1.002407869896990045, 0.1264236179284866091, 1.134350393647023614 ) ) ;
#35597 = CARTESIAN_POINT ( 'NONE',  ( 1.054774247047244540, 0.07405724077823318263, 1.599409448765134911 ) ) ;
#35598 = CARTESIAN_POINT ( 'NONE',  ( 1.033464566929133799, 0.000000000000000000, 0.7578740157480314821 ) ) ;
#35600 = CARTESIAN_POINT ( 'NONE',  ( -0.9873396505805591694, -0.1113553986120547346, 1.107283464566929165 ) ) ;
#35599 = CARTESIAN_POINT ( 'NONE',  ( 0.1645760504121570877, -0.08210179070116299660, 0.1405695446656931025 ) ) ;
#35601 = DIRECTION ( 'NONE',  ( 0.000000000000000000, 0.2432573283306646017, -0.9699617890481188054 ) ) ;
#35602 = CARTESIAN_POINT ( 'NONE',  ( -0.8759842519685039353, -0.1574803149606299191, 1.801181102254677091 ) ) ;
#35603 = CARTESIAN_POINT ( 'NONE',  ( -0.07405724077823318263, 0.03149606304588949135, -0.1787899950787401604 ) ) ;
#35604 = CARTESIAN_POINT ( 'NONE',  ( 1.054774247047244096, 0.000000000000000000, 0.1796259841982051075 ) ) ;
#35605 = CARTESIAN_POINT ( 'NONE',  ( -0.7185039370078746268, -0.06523048226347956391, 0.6914370077664891978 ) ) ;
#35607 = LINE ( 'NONE', #25041, #27720 ) ;
#35606 = CARTESIAN_POINT ( 'NONE',  ( 0.8759842519685039353, -0.1787899950787401882, 1.154035433017102319 ) ) ;
#35608 = CARTESIAN_POINT ( 'NONE',  ( 1.054774247047244540, 0.07405724077823318263, 1.958661417269071947 ) ) ;
#35609 = CARTESIAN_POINT ( 'NONE',  ( 1.033464566929134687, 0.06523048226347956391, 0.5142716534357801850 ) ) ;
#35610 = ORIENTED_EDGE ( 'NONE', *, *, #42133, .T. ) ;
#35611 = EDGE_CURVE ( 'NONE', #9090, #36581, #15639, .T. ) ;
#35612 = LINE ( 'NONE', #2752, #27655 ) ;
#35613 = CARTESIAN_POINT ( 'NONE',  ( -0.8107537697050253289, -0.1574803149606297803, 0.4601377951680635792 ) ) ;
#35614 = ORIENTED_EDGE ( 'NONE', *, *, #41235, .F. ) ;
#35615 = CARTESIAN_POINT ( 'NONE',  ( 0.6971942568897648851, -0.07405724077823297447, 1.461614173174583753 ) ) ;
#35616 = CARTESIAN_POINT ( 'NONE',  ( -1.060626887254335780E-16, -0.3937007874015746034, -0.4921259842519680183 ) ) ;
#35617 = CARTESIAN_POINT ( 'NONE',  ( 0.07405724077823318263, -0.06692913380450424277, 0.1787899950787401604 ) ) ;
#35618 = CARTESIAN_POINT ( 'NONE',  ( 0.4620708661417356478, 0.9842519685039370358, -0.7135826771653542844 ) ) ;
#35619 = EDGE_CURVE ( 'NONE', #30060, #22114, #19610, .T. ) ;
#35620 = VERTEX_POINT ( 'NONE', #11971 ) ;
#35621 = AXIS2_PLACEMENT_3D ( 'NONE', #45679, #23435, #5442 ) ;
#35623 = CARTESIAN_POINT ( 'NONE',  ( 0.1674339218906837068, 0.08959396230940555594, 0.1887650509910807906 ) ) ;
#35622 = CIRCLE ( 'NONE', #25681, 0.04921259842519683930 ) ;
#35624 = DIRECTION ( 'NONE',  ( -0.000000000000000000, 0.000000000000000000, 1.000000000000000000 ) ) ;
#35625 = CARTESIAN_POINT ( 'NONE',  ( 1.054774247047244096, 0.000000000000000000, 0.4207677164816693294 ) ) ;
#35626 = ORIENTED_EDGE ( 'NONE', *, *, #42705, .F. ) ;
#35628 = CARTESIAN_POINT ( 'NONE',  ( -0.1787899950787401882, -1.737696850339937038, 0.000000000000000000 ) ) ;
#35627 = CARTESIAN_POINT ( 'NONE',  ( 0.06523048226347956391, -0.4237204723334175305, -0.1574803149606300301 ) ) ;
#35629 = CARTESIAN_POINT ( 'NONE',  ( -0.6971942568897648851, 0.07405724077823318263, 1.028543307032851795 ) ) ;
#35630 = AXIS2_PLACEMENT_3D ( 'NONE', #3148, #35987, #17771 ) ;
#35631 = VECTOR ( 'NONE', #13078, 39.37007874015748143 ) ;
#35632 = CARTESIAN_POINT ( 'NONE',  ( -0.9500414927467378812, -0.1787899950787401604, 1.904527559001354398 ) ) ;
#35633 = CARTESIAN_POINT ( 'NONE',  ( -0.8759842519685039353, -0.1787899950787401882, 1.035925196796629866 ) ) ;
#35634 = CARTESIAN_POINT ( 'NONE',  ( -1.054774247047244096, 0.000000000000000000, 0.7357283464029290565 ) ) ;
#35635 = ADVANCED_FACE ( 'NONE', ( #8824 ), #12484, .F. ) ;
#35636 = B_SPLINE_CURVE_WITH_KNOTS ( 'NONE', 3,
 ( #12975, #38828, #30725, #45295, #20141, #19671, #34312, #23995, #1688, #23279, #42409, #5285 ),
 .UNSPECIFIED., .F., .F.,
 ( 4, 2, 2, 2, 2, 4 ),
 ( 0.000000000000000000, 0.2499999999999993339, 0.3749999999999991118, 0.4374999999999991118, 0.4999999999999991118, 1.000000000000000000 ),
 .UNSPECIFIED. ) ;
#35637 = CARTESIAN_POINT ( 'NONE',  ( -1.033464566929134687, 0.06523048226347956391, 0.08120078729404769935 ) ) ;
#35638 = ORIENTED_EDGE ( 'NONE', *, *, #21846, .T. ) ;
#35639 = CARTESIAN_POINT ( 'NONE',  ( -0.8759842519685039353, 0.1574803149606299191, 0.05905511811023622659 ) ) ;
#35640 = DIRECTION ( 'NONE',  ( 0.000000000000000000, 6.980778575359379259E-17, -1.000000000000000000 ) ) ;
#35641 = ORIENTED_EDGE ( 'NONE', *, *, #36987, .F. ) ;
#35642 = CARTESIAN_POINT ( 'NONE',  ( -0.8107537697050234415, -0.1574803149606297803, 0.3420275589475912370 ) ) ;
#35643 = FACE_OUTER_BOUND ( 'NONE', #2943, .T. ) ;
#35644 = CARTESIAN_POINT ( 'NONE',  ( -0.6971942568897626646, -0.07405724077823297447, 0.5561023621509617598 ) ) ;
#35645 = ( BOUNDED_CURVE ( )  B_SPLINE_CURVE ( 2, ( #5449, #23200, #30421, #37816, #41602, #15793, #20064, #34238, #15549 ),
 .UNSPECIFIED., .F., .T. ) 
 B_SPLINE_CURVE_WITH_KNOTS ( ( 3, 2, 2, 2, 3 ),
 ( 0.5799999999999999600, 0.5825000000000000178, 0.5849999999999999645, 0.5875000000000000222, 0.5899999999999999689 ),
 .UNSPECIFIED. ) 
 CURVE ( )  GEOMETRIC_REPRESENTATION_ITEM ( )  RATIONAL_B_SPLINE_CURVE ( ( 1.000000000000000000, 0.9238795325112869605, 1.000000000000000000, 0.9238795325112869605, 1.000000000000000000, 0.9238795325112869605, 1.000000000000000000, 0.9238795325112869605, 1.000000000000000000 ) ) 
 REPRESENTATION_ITEM ( '' )  ) ;
#35646 = DIRECTION ( 'NONE',  ( 0.000000000000000000, 0.7071067811866824648, 0.7071067811864125696 ) ) ;
#35647 = CARTESIAN_POINT ( 'NONE',  ( -0.8019270111902716547, 0.1787899950787401604, 1.614173228292692386 ) ) ;
#35648 = AXIS2_PLACEMENT_3D ( 'NONE', #16980, #2347, #35441 ) ;
#35649 = CARTESIAN_POINT ( 'NONE',  ( -0.2559055118110236116, 0.1477471161312031434, -0.1122047244094468571 ) ) ;
#35650 = DIRECTION ( 'NONE',  ( -0.5735764363510518216, -0.8191520442889876907, 0.000000000000000000 ) ) ;
#35651 = ORIENTED_EDGE ( 'NONE', *, *, #4417, .T. ) ;
#35652 = CARTESIAN_POINT ( 'NONE',  ( 0.8759842519685039353, 0.1574803149606299191, 0.5708661417322835607 ) ) ;
#35653 = CARTESIAN_POINT ( 'NONE',  ( 0.1797182628040039365, -0.8868548332050926186, -2.200913952912460540E-17 ) ) ;
#35654 = CARTESIAN_POINT ( 'NONE',  ( 0.8759842519685039353, 0.1574803149606299191, 0.6397637794200314865 ) ) ;
#35655 = CARTESIAN_POINT ( 'NONE',  ( -0.7185039370078739607, 1.928577636452523993E-17, 1.437007873908220601 ) ) ;
#35656 = CARTESIAN_POINT ( 'NONE',  ( 0.1574803149606300301, -0.5221456692913385433, 0.06523048226347956391 ) ) ;
#35657 = AXIS2_PLACEMENT_3D ( 'NONE', #25340, #46642, #44392 ) ;
#35658 = VECTOR ( 'NONE', #7286, 39.37007874015748143 ) ;
#35659 = CARTESIAN_POINT ( 'NONE',  ( 0.9873396505805591694, 0.1113553986120547346, 1.619094488081448846 ) ) ;
#35660 = EDGE_CURVE ( 'NONE', #34488, #28305, #22973, .T. ) ;
#35661 = LINE ( 'NONE', #7122, #10840 ) ;
#35662 = CARTESIAN_POINT ( 'NONE',  ( 0.7185039370078746268, -0.06523048226347956391, 1.291830708661417360 ) ) ;
#35664 = CARTESIAN_POINT ( 'NONE',  ( -0.8107537697050254399, -0.1574803149606297803, 1.336122047244094446 ) ) ;
#35663 = FACE_OUTER_BOUND ( 'NONE', #46812, .T. ) ;
#35665 = CARTESIAN_POINT ( 'NONE',  ( 0.7185039370078739607, 1.928577636452523993E-17, 1.722440944881889813 ) ) ;
#35667 = DIRECTION ( 'NONE',  ( -3.469446951953631938E-15, -1.000000000000000000, 0.000000000000000000 ) ) ;
#35666 = CARTESIAN_POINT ( 'NONE',  ( 0.9500414927467377701, -0.1787899950787401604, 0.6840551180564720113 ) ) ;
#35668 = CARTESIAN_POINT ( 'NONE',  ( 1.033464566929133799, 0.000000000000000000, 1.545275590551181244 ) ) ;
#35669 = VERTEX_POINT ( 'NONE', #5216 ) ;
#35670 = ADVANCED_FACE ( 'NONE', ( #45462 ), #45225, .T. ) ;
#35671 = CARTESIAN_POINT ( 'NONE',  ( 0.1634876958472368524, 0.08035653198460006308, 0.1391823568175673820 ) ) ;
#35672 = CARTESIAN_POINT ( 'NONE',  ( 1.033464566929134687, -0.06523048226347956391, 1.739665354330709013 ) ) ;
#35673 = CARTESIAN_POINT ( 'NONE',  ( 0.1598936088129072619, 0.05389714384562859645, -0.1404773021332343941 ) ) ;
#35674 = CARTESIAN_POINT ( 'NONE',  ( 0.8019270111902717657, 0.1787899950787401604, 0.8612204723871809131 ) ) ;
#35675 = DIRECTION ( 'NONE',  ( 0.000000000000000000, 1.000000000000000000, 0.000000000000000000 ) ) ;
#35676 = DIRECTION ( 'NONE',  ( 0.000000000000000000, 0.000000000000000000, 1.000000000000000000 ) ) ;
#35677 = CARTESIAN_POINT ( 'NONE',  ( 0.1797182628040039087, 0.05556642663742687727, 0.07444174185955046430 ) ) ;
#35678 = CARTESIAN_POINT ( 'NONE',  ( 3.284318927891251994E-17, -1.019192913332062966, 0.1787899950787401882 ) ) ;
#35679 = CARTESIAN_POINT ( 'NONE',  ( 0.1574803149606300301, -1.501476377952755570, -0.06523048226347956391 ) ) ;
#35680 = LINE ( 'NONE', #24885, #13782 ) ;
#35681 = CARTESIAN_POINT ( 'NONE',  ( -1.002407869896990045, 0.1264236179284866091, 1.921751968450173376 ) ) ;
#35682 = VERTEX_POINT ( 'NONE', #38295 ) ;
#35683 = CARTESIAN_POINT ( 'NONE',  ( 0.7495606340400177148, 0.1264236179284866091, 1.931594488135212728 ) ) ;
#35684 = ORIENTED_EDGE ( 'NONE', *, *, #26743, .T. ) ;
#35685 = CARTESIAN_POINT ( 'NONE',  ( -0.6971942568897637749, 2.189545951927499583E-17, 1.936515747977732405 ) ) ;
#35686 = CARTESIAN_POINT ( 'NONE',  ( -0.8759842519685039353, 0.1787899950787401882, 1.567421259788755794 ) ) ;
#35687 = CARTESIAN_POINT ( 'NONE',  ( 0.9500414927467377701, 0.1787899950787401604, 0.8612204723871810241 ) ) ;
#35688 = CARTESIAN_POINT ( 'NONE',  ( -0.9500414927467378812, -0.1787899950787401604, 1.038385826717890259 ) ) ;
#35689 = CARTESIAN_POINT ( 'NONE',  ( -0.6971942568897637749, 2.189545951927499583E-17, 0.2436023621509610382 ) ) ;
#35690 = EDGE_CURVE ( 'NONE', #36971, #44905, #9066, .T. ) ;
#35691 = CARTESIAN_POINT ( 'NONE',  ( -0.9500414927467378812, -0.1787899950787401604, 1.948818897584033927 ) ) ;
#35692 = CARTESIAN_POINT ( 'NONE',  ( 0.5660731898098425585, 4.766607801171850497E-17, 0.000000000000000000 ) ) ;
#35693 = CARTESIAN_POINT ( 'NONE',  ( 3.284318927891251994E-17, -0.3214822359457744638, 0.1787899950787401882 ) ) ;
#35694 = CARTESIAN_POINT ( 'NONE',  ( -1.033464566929133799, 0.000000000000000000, 1.505905511811023612 ) ) ;
#35695 = CARTESIAN_POINT ( 'NONE',  ( 1.033464566929134687, -0.06523048226347956391, 1.060531495955465031 ) ) ;
#35696 = DIMENSIONAL_EXPONENTS ( 1.000000000000000000, 0.000000000000000000, 0.000000000000000000, 0.000000000000000000, 0.000000000000000000, 0.000000000000000000, 0.000000000000000000 ) ;
#35697 = CARTESIAN_POINT ( 'NONE',  ( -0.6971942568897626646, -0.07405724077823297447, 0.1230314960092287191 ) ) ;
#35698 = VERTEX_POINT ( 'NONE', #12917 ) ;
#35699 = CARTESIAN_POINT ( 'NONE',  ( -0.8759842519685039353, -0.1787899950787401882, 1.277066929080094448 ) ) ;
#35700 = ORIENTED_EDGE ( 'NONE', *, *, #44681, .F. ) ;
#35701 = CARTESIAN_POINT ( 'NONE',  ( -1.094772975963752103E-17, -1.156988188922614125, -0.1787899950787401882 ) ) ;
#35702 = CARTESIAN_POINT ( 'NONE',  ( 0.1264236179284866091, -1.363681102308440973, 0.1264236179284866091 ) ) ;
#35703 = CARTESIAN_POINT ( 'NONE',  ( -0.7185039370078739607, 1.928577636452523993E-17, 1.358267716427907779 ) ) ;
#35704 = CARTESIAN_POINT ( 'NONE',  ( -0.07444174185955065859, -0.5054571954098173725, 0.1797182628040039087 ) ) ;
#35705 = CARTESIAN_POINT ( 'NONE',  ( 0.4453382816733590377, -0.09842519685039370636, 1.205361022782828805E-17 ) ) ;
#35706 = CARTESIAN_POINT ( 'NONE',  ( -0.9412147342319837628, -0.1574803149606297803, 0.8981299211523156023 ) ) ;
#35707 = CARTESIAN_POINT ( 'NONE',  ( -0.8107537697050253289, 0.1574803149606300301, 0.6914370078740167402 ) ) ;
#35708 = CARTESIAN_POINT ( 'NONE',  ( 0.1574803149606300301, -0.08907480314960623813, 0.06523048226347956391 ) ) ;
#35709 = CARTESIAN_POINT ( 'NONE',  ( 0.9412147342319837628, 0.1574803149606300301, 1.739665354223181470 ) ) ;
#35710 = ADVANCED_FACE ( 'NONE', ( #27547 ), #12197, .F. ) ;
#35711 = DIRECTION ( 'NONE',  ( 1.000000000000000000, 0.000000000000000000, 0.000000000000000000 ) ) ;
#35712 = CARTESIAN_POINT ( 'NONE',  ( 0.9873396505805591694, 0.1113553986120547346, 0.7234251968503936370 ) ) ;
#35713 = CARTESIAN_POINT ( 'NONE',  ( 0.06200172126963626046, -0.2596975217971643213, -0.05114647357132630356 ) ) ;
#35714 = CARTESIAN_POINT ( 'NONE',  ( -1.033464566929133799, 0.000000000000000000, 1.230314960629921295 ) ) ;
#35715 = EDGE_CURVE ( 'NONE', #36104, #34892, #4741, .T. ) ;
#35717 = CARTESIAN_POINT ( 'NONE',  ( 0.1564256176496392203, -0.1180751491311568813, -0.07625914551943928366 ) ) ;
#35716 = LINE ( 'NONE', #25415, #8676 ) ;
#35718 = CARTESIAN_POINT ( 'NONE',  ( 0.9873396505805591694, -0.1113553986120547346, 0.1131889762704257896 ) ) ;
#35719 = EDGE_CURVE ( 'NONE', #40831, #45750, #8347, .T. ) ;
#35720 = EDGE_CURVE ( 'NONE', #6499, #35936, #17061, .T. ) ;
#35721 = ORIENTED_EDGE ( 'NONE', *, *, #46571, .T. ) ;
#35722 = FACE_OUTER_BOUND ( 'NONE', #28706, .T. ) ;
#35723 = DIRECTION ( 'NONE',  ( 1.000000000000000000, 0.000000000000000000, -0.000000000000000000 ) ) ;
#35724 = CARTESIAN_POINT ( 'NONE',  ( -0.07405724077823318263, -0.6427165353793066194, -0.1787899950787401604 ) ) ;
#35725 = CARTESIAN_POINT ( 'NONE',  ( 0.1574803149606300301, -1.107775590551181688, -0.06523048226347956391 ) ) ;
#35726 = CARTESIAN_POINT ( 'NONE',  ( 0.7646288533564489232, -0.1113553986120547346, 0.8513779526483780113 ) ) ;
#35727 = DIRECTION ( 'NONE',  ( 0.000000000000000000, 0.000000000000000000, -1.000000000000000000 ) ) ;
#35728 = CARTESIAN_POINT ( 'NONE',  ( -0.6971942568897648851, -0.07405724077823297447, 1.934055118056471567 ) ) ;
#35729 = ORIENTED_EDGE ( 'NONE', *, *, #38229, .T. ) ;
#35730 = CARTESIAN_POINT ( 'NONE',  ( -0.8019270111902717657, -0.1787899950787401604, 1.471456692859622217 ) ) ;
#35731 = CARTESIAN_POINT ( 'NONE',  ( 0.9500414927467378812, -0.1787899950787401604, 1.515748031442299526 ) ) ;
#35732 = EDGE_LOOP ( 'NONE', ( #2313, #45790, #9230 ) ) ;
#35733 = DIRECTION ( 'NONE',  ( -1.000000000000000000, 0.000000000000000000, 0.000000000000000000 ) ) ;
#35734 = CARTESIAN_POINT ( 'NONE',  ( -1.054774247047244540, -0.07405724077823318263, 0.6151574802611974313 ) ) ;
#35735 = CARTESIAN_POINT ( 'NONE',  ( 1.054774247047244096, 0.000000000000000000, 0.1451771653005673179 ) ) ;
#35736 = CARTESIAN_POINT ( 'NONE',  ( 1.033464566929133799, 1.928577636452524610E-17, 4.498031496062992574 ) ) ;
#35737 = CARTESIAN_POINT ( 'NONE',  ( 1.002407869896990045, 0.1264236179284866091, 0.7012795275052913224 ) ) ;
#35738 = CARTESIAN_POINT ( 'NONE',  ( -1.002407869896990045, 0.1264236179284866091, 0.6569881889226141247 ) ) ;
#35739 = FACE_OUTER_BOUND ( 'NONE', #21091, .T. ) ;
#35740 = CARTESIAN_POINT ( 'NONE',  ( -0.8107537697050254399, -0.1574803149606297803, 0.8636811023622043004 ) ) ;
#35741 = CARTESIAN_POINT ( 'NONE',  ( -9.642888182262618425E-18, -0.1850393699712129802, -0.1574803149606299191 ) ) ;
#35742 = CARTESIAN_POINT ( 'NONE',  ( -1.054774247047244540, -0.07405724077823318263, 1.441929133804504604 ) ) ;
#35743 = ORIENTED_EDGE ( 'NONE', *, *, #28438, .T. ) ;
#35744 = CARTESIAN_POINT ( 'NONE',  ( -0.9412147342319837628, 0.1574803149606300301, 1.473917322834645605 ) ) ;
#35745 = CARTESIAN_POINT ( 'NONE',  ( -0.9412147342319837628, 0.1574803149606300301, 0.4896653543307081802 ) ) ;
#35746 = CARTESIAN_POINT ( 'NONE',  ( 1.002407869896990045, 0.1264236179284866091, 1.252460629867496067 ) ) ;
#35747 = CARTESIAN_POINT ( 'NONE',  ( -0.09636693384614980484, -0.09851383887303406806, -0.1572292210079062891 ) ) ;
#35748 = B_SPLINE_CURVE_WITH_KNOTS ( 'NONE', 3,
 ( #19883, #34994, #31640, #13632, #24427, #27355, #5504, #1665, #45743, #42139, #16312, #20117, #45981, #6196, #41898, #2364, #12952, #17234, #8867 ),
 .UNSPECIFIED., .F., .F.,
 ( 4, 1, 1, 1, 2, 2, 1, 1, 1, 1, 2, 2, 4 ),
 ( 0.000000000000000000, 0.1249999999999964473, 0.1874999999999945599, 0.2187499999999934497, 0.2343749999999929223, 0.2499999999999923950, 0.3749999999999917843, 0.4374999999999915068, 0.4687499999999910627, 0.4843749999999910627, 0.4921874999999908407, 0.4999999999999905631, 1.000000000000000000 ),
 .UNSPECIFIED. ) ;
#35749 = ORIENTED_EDGE ( 'NONE', *, *, #2644, .F. ) ;
#35750 = ORIENTED_EDGE ( 'NONE', *, *, #26876, .F. ) ;
#35751 = CARTESIAN_POINT ( 'NONE',  ( 0.1574803149606299746, -0.09842519685039370636, 2.185526306663016616 ) ) ;
#35752 = ORIENTED_EDGE ( 'NONE', *, *, #3086, .F. ) ;
#35753 = CARTESIAN_POINT ( 'NONE',  ( 0.7495606340400177148, -0.1264236179284866091, 1.385334645615527549 ) ) ;
#35754 = DIRECTION ( 'NONE',  ( -1.000000000000000000, 0.000000000000000000, 0.000000000000000000 ) ) ;
#35755 = CARTESIAN_POINT ( 'NONE',  ( 0.1787899950787401882, -0.8075787401037164415, -2.189545951927503898E-17 ) ) ;
#35756 = LINE ( 'NONE', #2896, #47106 ) ;
#35757 = LINE ( 'NONE', #2897, #43126 ) ;
#35758 = CARTESIAN_POINT ( 'NONE',  ( 1.002407869896990045, 0.1264236179284866091, 0.2632874015210397434 ) ) ;
#35759 = CARTESIAN_POINT ( 'NONE',  ( -0.1787899950787401604, -0.05327357452845130764, 0.07405724077823318263 ) ) ;
#35760 = CARTESIAN_POINT ( 'NONE',  ( -0.1264236179284866091, -0.2416338582139531399, -0.1264236179284866091 ) ) ;
#35761 = CARTESIAN_POINT ( 'NONE',  ( -0.07405724077823318263, 0.001968503990771400605, 0.1787899950787401604 ) ) ;
#35762 = CYLINDRICAL_SURFACE ( 'NONE', #12731, 0.1574803149606299191 ) ;
#35763 = FACE_OUTER_BOUND ( 'NONE', #13315, .T. ) ;
#35764 = CARTESIAN_POINT ( 'NONE',  ( 0.7495606340400177148, 0.1264236179284866091, 0.5880905511273386566 ) ) ;
#35765 = AXIS2_PLACEMENT_3D ( 'NONE', #44657, #30814, #18804 ) ;
#35766 = EDGE_CURVE ( 'NONE', #763, #34774, #3960, .T. ) ;
#35767 = CARTESIAN_POINT ( 'NONE',  ( -0.6971942568897637749, 2.189545951927499583E-17, 0.9128937007336377363 ) ) ;
#35768 = CARTESIAN_POINT ( 'NONE',  ( -0.06523048226347956391, -0.9650590551181117416, 0.1574803149606297803 ) ) ;
#35770 = CARTESIAN_POINT ( 'NONE',  ( -0.8765439795121998667, -0.1745856626756026320, 1.988193917683002132 ) ) ;
#35769 = CARTESIAN_POINT ( 'NONE',  ( -0.1797182628040039087, -1.657031998559424846, -0.07444174185955065859 ) ) ;
#35771 = CARTESIAN_POINT ( 'NONE',  ( 0.8019270111902717657, 0.1787899950787401604, 1.614173228292692386 ) ) ;
#35773 = CARTESIAN_POINT ( 'NONE',  ( -0.2431102362204724532, 0.000000000000000000, 0.000000000000000000 ) ) ;
#35772 = CARTESIAN_POINT ( 'NONE',  ( 0.6971942568897637749, 2.189545951927499583E-17, 1.931594488135212728 ) ) ;
#35774 = ORIENTED_EDGE ( 'NONE', *, *, #25272, .F. ) ;
#35775 = VERTEX_POINT ( 'NONE', #45945 ) ;
#35776 = EDGE_CURVE ( 'NONE', #27412, #30178, #12509, .T. ) ;
#35777 = CARTESIAN_POINT ( 'NONE',  ( 0.08946752424252854552, 0.3740157480314960647, 1.224299699984021661 ) ) ;
#35778 = CARTESIAN_POINT ( 'NONE',  ( 3.284318927891251994E-17, -0.1530511810485986057, 0.1787899950787401882 ) ) ;
#35779 = CARTESIAN_POINT ( 'NONE',  ( 1.054774247047244540, 0.07405724077823318263, 0.6545275590013545086 ) ) ;
#35780 = CARTESIAN_POINT ( 'NONE',  ( 0.1264236179284866091, -0.8813976377415118080, -0.1264236179284866091 ) ) ;
#35781 = CYLINDRICAL_SURFACE ( 'NONE', #33039, 0.1574803149606299191 ) ;
#35782 = ( BOUNDED_CURVE ( )  B_SPLINE_CURVE ( 2, ( #24449, #7180, #17256, #17727, #36430, #20844, #3099, #47202, #24927 ),
 .UNSPECIFIED., .F., .F. ) 
 B_SPLINE_CURVE_WITH_KNOTS ( ( 3, 2, 2, 2, 3 ),
 ( 0.5400000000000000355, 0.5424999999999999822, 0.5450000000000000400, 0.5474999999999999867, 0.5500000000000000444 ),
 .UNSPECIFIED. ) 
 CURVE ( )  GEOMETRIC_REPRESENTATION_ITEM ( )  RATIONAL_B_SPLINE_CURVE ( ( 1.000000000000000000, 0.9238795325112869605, 1.000000000000000000, 0.9238795325112869605, 1.000000000000000000, 0.9238795325112869605, 1.000000000000000000, 0.9238795325112869605, 1.000000000000000000 ) ) 
 REPRESENTATION_ITEM ( '' )  ) ;
#35783 = DIRECTION ( 'NONE',  ( 0.000000000000000000, 0.7880107536067200158, -0.6156614753256608452 ) ) ;
#35784 = CARTESIAN_POINT ( 'NONE',  ( 0.9873396505805591694, 0.1113553986120547346, 1.146653543199559033 ) ) ;
#35785 = CARTESIAN_POINT ( 'NONE',  ( -0.7495606340400177148, 0.1264236179284866091, 1.493602362150960650 ) ) ;
#35786 = ORIENTED_EDGE ( 'NONE', *, *, #38043, .T. ) ;
#35787 = CARTESIAN_POINT ( 'NONE',  ( 0.7646288533564489232, -0.1113553986120547346, 0.1525590551181102428 ) ) ;
#35788 = CARTESIAN_POINT ( 'NONE',  ( 1.002407869896990045, 0.1264236179284866091, 1.094980314906866203 ) ) ;
#35789 = CARTESIAN_POINT ( 'NONE',  ( 1.002407869896990045, 0.1264236179284866091, 1.838090551127338657 ) ) ;
#35790 = CARTESIAN_POINT ( 'NONE',  ( -1.054774247047244540, 0.07405724077823318263, 0.9694881889226144578 ) ) ;
#35791 = CARTESIAN_POINT ( 'NONE',  ( 0.8759842519685039353, 0.000000000000000000, 4.498031496062992574 ) ) ;
#35792 = CARTESIAN_POINT ( 'NONE',  ( -0.7012869015610273538, 0.0004423858256796530677, 0.03937007874015843734 ) ) ;
#35793 = CARTESIAN_POINT ( 'NONE',  ( 0.9500414927467377701, 0.1787899950787401604, 0.3494094487651343006 ) ) ;
#35794 = CARTESIAN_POINT ( 'NONE',  ( -1.054774247047244540, 0.07405724077823318263, 0.6151574802611965431 ) ) ;
#35795 = CARTESIAN_POINT ( 'NONE',  ( 1.033464566929133799, 0.000000000000000000, 1.535433070758614127 ) ) ;
#35796 = VERTEX_POINT ( 'NONE', #38990 ) ;
#35797 = CARTESIAN_POINT ( 'NONE',  ( 0.1787899950787401604, -0.06692913380450424277, 0.07405724077823318263 ) ) ;
#35798 = CARTESIAN_POINT ( 'NONE',  ( 0.7646288533564489232, 0.1113553986120547346, 1.786417322727117840 ) ) ;
#35799 = ORIENTED_EDGE ( 'NONE', *, *, #7901, .T. ) ;
#35800 = CARTESIAN_POINT ( 'NONE',  ( 0.7495606340400177148, -0.1264236179284866091, 0.7997047243556849594 ) ) ;
#35801 = CARTESIAN_POINT ( 'NONE',  ( -0.6971942568897648851, -0.07405724077823297447, 1.737204724355685626 ) ) ;
#35802 = VECTOR ( 'NONE', #40009, 39.37007874015748143 ) ;
#35803 = ( BOUNDED_CURVE ( )  B_SPLINE_CURVE ( 2, ( #4761, #34039, #19865, #1164, #37600, #34266, #8363, #42116, #9330 ),
 .UNSPECIFIED., .F., .F. ) 
 B_SPLINE_CURVE_WITH_KNOTS ( ( 3, 2, 2, 2, 3 ),
 ( 0.2000000000000000111, 0.2025000000000000133, 0.2049999999999999878, 0.2074999999999999900, 0.2099999999999999922 ),
 .UNSPECIFIED. ) 
 CURVE ( )  GEOMETRIC_REPRESENTATION_ITEM ( )  RATIONAL_B_SPLINE_CURVE ( ( 1.000000000000000000, 0.9238795325112869605, 1.000000000000000000, 0.9238795325112869605, 1.000000000000000000, 0.9238795325112869605, 1.000000000000000000, 0.9238795325112869605, 1.000000000000000000 ) ) 
 REPRESENTATION_ITEM ( '' )  ) ;
#35804 = CARTESIAN_POINT ( 'NONE',  ( -0.7185039370078739607, 1.928577636452523993E-17, 0.6594488188976378451 ) ) ;
#35805 = CARTESIAN_POINT ( 'NONE',  ( -7.957671378281915615E-17, -8.878505979408855953E-16, -0.3937007874015748254 ) ) ;
#35806 = CARTESIAN_POINT ( 'NONE',  ( -0.1264236179284866091, -1.310655464292230565, 0.1264236179284866091 ) ) ;
#35807 = ORIENTED_EDGE ( 'NONE', *, *, #37823, .T. ) ;
#35808 = CARTESIAN_POINT ( 'NONE',  ( -0.1787899950787401604, -0.1555118109698585271, 0.07405724077823318263 ) ) ;
#35809 = VERTEX_POINT ( 'NONE', #43942 ) ;
#35810 = CARTESIAN_POINT ( 'NONE',  ( 0.6971942568897637749, 2.189545951927499583E-17, 1.065452755851747924 ) ) ;
#35811 = CARTESIAN_POINT ( 'NONE',  ( 0.003062405574132101051, -0.1386494127070022064, -0.03544276884525298515 ) ) ;
#35812 = CARTESIAN_POINT ( 'NONE',  ( 0.9873396505805591694, -0.1113553986120547346, 1.973425196850393970 ) ) ;
#35813 = CARTESIAN_POINT ( 'NONE',  ( 0.1787899950787401604, -1.479330708607653699, -0.07405724077823318263 ) ) ;
#35814 = CARTESIAN_POINT ( 'NONE',  ( 0.1264236179284866091, -0.7682086613635590311, -0.1264236179284866091 ) ) ;
#35815 = EDGE_CURVE ( 'NONE', #649, #19819, #31600, .T. ) ;
#35816 = CARTESIAN_POINT ( 'NONE',  ( -0.6971942568897648851, 0.07405724077823318263, 0.3592519684501735422 ) ) ;
#35817 = CIRCLE ( 'NONE', #9041, 0.09842519685039370636 ) ;
#35818 = CARTESIAN_POINT ( 'NONE',  ( -0.1270800023317771588, -1.295319400134226306, 0.1270800023317771588 ) ) ;
#35819 = CARTESIAN_POINT ( 'NONE',  ( -0.1017711380106712249, 0.2367366383362116133, -0.03112915705353517387 ) ) ;
#35820 = CARTESIAN_POINT ( 'NONE',  ( 0.6971942568897648851, 0.07405724077823318263, 1.225393700733637514 ) ) ;
#35821 = CARTESIAN_POINT ( 'NONE',  ( 0.8759842519685039353, -0.1787899950787401882, 1.508366141678519678 ) ) ;
#35822 = CARTESIAN_POINT ( 'NONE',  ( 1.054774247047244540, 0.07405724077823318263, 0.1820866141194649179 ) ) ;
#35823 = ADVANCED_FACE ( 'NONE', ( #7294 ), #36536, .T. ) ;
#35824 = CARTESIAN_POINT ( 'NONE',  ( 0.7646288533564489232, -0.1113553986120547346, 1.687992125984252079 ) ) ;
#35825 = CARTESIAN_POINT ( 'NONE',  ( -0.07154104892864131260, 0.1299212598425195930, 0.1541805736627041012 ) ) ;
#35827 = CARTESIAN_POINT ( 'NONE',  ( 1.033464566929133799, 0.000000000000000000, 1.535433070758614127 ) ) ;
#35826 = CARTESIAN_POINT ( 'NONE',  ( -1.033464566929134687, 0.06523048226347956391, 0.9965551181102363376 ) ) ;
#35828 = CARTESIAN_POINT ( 'NONE',  ( 0.5839895013123354017, 0.08090551181102362266, 0.000000000000000000 ) ) ;
#35829 = CARTESIAN_POINT ( 'NONE',  ( -0.9873396505805591694, -0.1113553986120547346, 1.727362204616881947 ) ) ;
#35830 = AXIS2_PLACEMENT_3D ( 'NONE', #45735, #24422, #2133 ) ;
#35831 = CARTESIAN_POINT ( 'NONE',  ( 0.1264236179284866091, 0.01427165359707059308, 0.1264236179284866091 ) ) ;
#35832 = CARTESIAN_POINT ( 'NONE',  ( 1.002407869896990045, -0.1264236179284866091, 0.1747047243556852092 ) ) ;
#35833 = CARTESIAN_POINT ( 'NONE',  ( 0.7302202526404721894, -0.08507351211645501621, 0.03937197694971072970 ) ) ;
#35835 = FACE_OUTER_BOUND ( 'NONE', #19455, .T. ) ;
#35834 = CARTESIAN_POINT ( 'NONE',  ( 1.054774247047244096, 0.000000000000000000, 1.203248031442299304 ) ) ;
#35836 = CARTESIAN_POINT ( 'NONE',  ( 1.002407869896990045, 0.1264236179284866091, 1.921751968450173376 ) ) ;
#35837 = CARTESIAN_POINT ( 'NONE',  ( 0.7646288533564489232, -0.1113553986120547346, 0.4576771652468039631 ) ) ;
#35838 = ORIENTED_EDGE ( 'NONE', *, *, #37129, .T. ) ;
#35839 = CARTESIAN_POINT ( 'NONE',  ( -0.8107537697050253289, -0.1574803149606297803, 0.4207677164279059467 ) ) ;
#35840 = ORIENTED_EDGE ( 'NONE', *, *, #29496, .F. ) ;
#35841 = CARTESIAN_POINT ( 'NONE',  ( 1.054774247047244540, -0.07405724077823318263, 1.515748031442299526 ) ) ;
#35842 = CARTESIAN_POINT ( 'NONE',  ( -0.7646288533564489232, 0.1113553986120547346, 0.2903543306011346359 ) ) ;
#35843 = CARTESIAN_POINT ( 'NONE',  ( 0.1787899950787401604, -0.02263779522182702078, 0.07405724077823318263 ) ) ;
#35844 = ORIENTED_EDGE ( 'NONE', *, *, #4516, .F. ) ;
#35845 = CARTESIAN_POINT ( 'NONE',  ( 0.1594617487093093755, -0.04893254358511540947, -0.1404675734346159666 ) ) ;
#35846 = ORIENTED_EDGE ( 'NONE', *, *, #42294, .F. ) ;
#35847 = DIRECTION ( 'NONE',  ( 1.000000000000000000, 0.000000000000000000, -1.822029033848725275E-16 ) ) ;
#35848 = PLANE ( 'NONE',  #20765 ) ;
#35849 = EDGE_LOOP ( 'NONE', ( #23266, #22987 ) ) ;
#35850 = CARTESIAN_POINT ( 'NONE',  ( -0.07405724077823318263, -1.651574803095843258, 0.1787899950787401604 ) ) ;
#35851 = CARTESIAN_POINT ( 'NONE',  ( -0.6971942568897637749, 2.189545951927499583E-17, 1.970964566875370139 ) ) ;
#35852 = ORIENTED_EDGE ( 'NONE', *, *, #5387, .F. ) ;
#35853 = CARTESIAN_POINT ( 'NONE',  ( -0.6971942568897648851, -0.07405724077823297447, 1.067913385773007651 ) ) ;
#35854 = CARTESIAN_POINT ( 'NONE',  ( -0.7495606340400177148, -0.1264236179284866091, 0.7997047243556849594 ) ) ;
#35855 = EDGE_CURVE ( 'NONE', #10419, #12883, #7896, .T. ) ;
#35856 = CONICAL_SURFACE ( 'NONE', #9865, 0.08090551181102362266, 0.9599310885968742602 ) ;
#35857 = DIRECTION ( 'NONE',  ( 0.000000000000000000, 0.000000000000000000, -1.000000000000000000 ) ) ;
#35858 = CARTESIAN_POINT ( 'NONE',  ( 0.03901279071809810040, -0.09842519685039370636, 1.713085361781125471 ) ) ;
#35859 = CARTESIAN_POINT ( 'NONE',  ( -0.1264236179284866091, -0.8480570390953799942, -0.1264236179284866091 ) ) ;
#35860 = ORIENTED_EDGE ( 'NONE', *, *, #42398, .T. ) ;
#35861 = CARTESIAN_POINT ( 'NONE',  ( -0.06485735496959410540, -0.08956202182541239676, 0.1433340101501935082 ) ) ;
#35862 = LINE ( 'NONE', #17648, #11889 ) ;
#35863 = ORIENTED_EDGE ( 'NONE', *, *, #998, .F. ) ;
#35864 = LINE ( 'NONE', #10723, #24875 ) ;
#35865 = CARTESIAN_POINT ( 'NONE',  ( 0.1822895153388602307, 0.000000000000000000, 0.000000000000000000 ) ) ;
#35866 = VECTOR ( 'NONE', #12175, 39.37007874015748143 ) ;
#35867 = CARTESIAN_POINT ( 'NONE',  ( -1.054774247047244096, 0.000000000000000000, 0.6914370078202519698 ) ) ;
#35868 = CARTESIAN_POINT ( 'NONE',  ( 1.033464566929134687, 0.06523048226347956391, 1.341043306979086358 ) ) ;
#35869 = VERTEX_POINT ( 'NONE', #32722 ) ;
#35870 = CARTESIAN_POINT ( 'NONE',  ( -0.9500414927467377701, -0.1787899950787401604, 1.791338582623401177 ) ) ;
#35871 = CARTESIAN_POINT ( 'NONE',  ( 1.033464566929134687, -0.06523048226347956391, 1.345964566929133133 ) ) ;
#35872 = EDGE_CURVE ( 'NONE', #46575, #30455, #46129, .T. ) ;
#35873 = CARTESIAN_POINT ( 'NONE',  ( -0.9873396505805591694, 0.1113553986120547346, 0.1230314959554651699 ) ) ;
#35874 = DIRECTION ( 'NONE',  ( 0.000000000000000000, 1.000000000000000000, 0.000000000000000000 ) ) ;
#35875 = CARTESIAN_POINT ( 'NONE',  ( 0.1797182628040039087, -0.9237642820239904129, -0.07444174185955065859 ) ) ;
#35876 = CARTESIAN_POINT ( 'NONE',  ( 0.2471922904502826535, 0.09123121687245852596, 0.04590630800384764426 ) ) ;
#35877 = CARTESIAN_POINT ( 'NONE',  ( -0.9873396505805591694, -0.1113553986120547346, 1.333661417215306955 ) ) ;
#35878 = CARTESIAN_POINT ( 'NONE',  ( 0.8019270111902717657, 0.1787899950787401604, 0.7874015747493863238 ) ) ;
#35879 = CARTESIAN_POINT ( 'NONE',  ( -0.06523048226347956391, -0.6107283464566929387, 0.1574803149606297803 ) ) ;
#35880 = CARTESIAN_POINT ( 'NONE',  ( -0.1485133662041858704, 0.1246681010365934816, -0.06542554175153637852 ) ) ;
#35881 = DIRECTION ( 'NONE',  ( 1.822029033848725028E-16, 0.000000000000000000, 1.000000000000000000 ) ) ;
#35882 = EDGE_CURVE ( 'NONE', #37690, #44293, #43084, .T. ) ;
#35883 = CARTESIAN_POINT ( 'NONE',  ( 0.7185039370078746268, 0.06523048226347956391, 1.247539370078740273 ) ) ;
#35885 = CARTESIAN_POINT ( 'NONE',  ( 1.284448818897637956, -0.3937007874015748254, 1.181102362204724310 ) ) ;
#35884 = CARTESIAN_POINT ( 'NONE',  ( 0.7469364138422923682, -0.1104497288306852537, 1.985496003449917390 ) ) ;
#35887 = DIRECTION ( 'NONE',  ( -0.8191520442889861364, 1.003171929053517844E-16, 0.5735764363510541530 ) ) ;
#35886 = CARTESIAN_POINT ( 'NONE',  ( 1.002407869896990045, 0.1264236179284866091, 0.6176181101824566033 ) ) ;
#35888 = LINE ( 'NONE', #24402, #31567 ) ;
#35889 = CARTESIAN_POINT ( 'NONE',  ( -0.7185039370078746268, -0.06523048226347956391, 0.3764763778452288046 ) ) ;
#35890 = ORIENTED_EDGE ( 'NONE', *, *, #21536, .F. ) ;
#35891 = CARTESIAN_POINT ( 'NONE',  ( 0.1642909309750750502, 0.08091905466946164305, 0.1401559438098464727 ) ) ;
#35892 = CARTESIAN_POINT ( 'NONE',  ( 0.9412147342319837628, -0.1574803149606297803, 0.7111220472440957785 ) ) ;
#35893 = CARTESIAN_POINT ( 'NONE',  ( 0.6971942568897648851, 0.07405724077823318263, 1.062992125930488418 ) ) ;
#35894 = VERTEX_POINT ( 'NONE', #25274 ) ;
#35895 = CARTESIAN_POINT ( 'NONE',  ( 0.9412147342319837628, 0.1574803149606300301, 1.473917322834645605 ) ) ;
#35896 = DIRECTION ( 'NONE',  ( -1.000000000000000000, 0.000000000000000000, 0.000000000000000000 ) ) ;
#35897 = CARTESIAN_POINT ( 'NONE',  ( -0.1797182628040039087, 0.1195428045901827108, 0.07444174185955065859 ) ) ;
#35898 = CARTESIAN_POINT ( 'NONE',  ( -0.1787899950787401604, -1.110236220418677533, -0.07405724077823318263 ) ) ;
#35900 = AXIS2_PLACEMENT_3D ( 'NONE', #11412, #10716, #6848 ) ;
#35899 = CARTESIAN_POINT ( 'NONE',  ( -0.06523048226347956391, -1.476870078740157188, 0.1574803149606297803 ) ) ;
#35901 = DIRECTION ( 'NONE',  ( 0.000000000000000000, 0.000000000000000000, 1.000000000000000000 ) ) ;
#35902 = CARTESIAN_POINT ( 'NONE',  ( -0.7495606340400177148, 0.1264236179284866091, 0.1156496062454492185 ) ) ;
#35903 = VERTEX_POINT ( 'NONE', #39862 ) ;
#35904 = CARTESIAN_POINT ( 'NONE',  ( 2.892866454678787531E-17, 0.07086614183981043702, 0.1574803149606299191 ) ) ;
#35905 = ORIENTED_EDGE ( 'NONE', *, *, #13144, .T. ) ;
#35906 = CARTESIAN_POINT ( 'NONE',  ( -0.7495606340400177148, 0.1264236179284866091, 1.931594488135212728 ) ) ;
#35907 = CARTESIAN_POINT ( 'NONE',  ( -1.002407869896990045, 0.1264236179284866091, 1.523129921206078707 ) ) ;
#35908 = CARTESIAN_POINT ( 'NONE',  ( 0.8019270111902716547, -0.1787899950787401604, 0.8415354330171020969 ) ) ;
#35909 = ( BOUNDED_CURVE ( )  B_SPLINE_CURVE ( 2, ( #45294, #38125, #40978 ),
 .UNSPECIFIED., .F., .T. ) 
 B_SPLINE_CURVE_WITH_KNOTS ( ( 3, 3 ),
 ( 0.9975000000000000533, 1.000000000000000000 ),
 .UNSPECIFIED. ) 
 CURVE ( )  GEOMETRIC_REPRESENTATION_ITEM ( )  RATIONAL_B_SPLINE_CURVE ( ( 1.000000000000000000, 0.9238795325112869605, 1.000000000000000000 ) ) 
 REPRESENTATION_ITEM ( '' )  ) ;
#35910 = CARTESIAN_POINT ( 'NONE',  ( -0.2471922904502826535, 0.09660984127287175482, 0.02629157619858309841 ) ) ;
#35911 = CARTESIAN_POINT ( 'NONE',  ( -0.7495606340400177148, -0.1264236179284866091, 1.823326771599779406 ) ) ;
#35912 = CARTESIAN_POINT ( 'NONE',  ( 0.08640460078259740162, -0.09201407021830487754, -0.2355472506762735785 ) ) ;
#35913 = CARTESIAN_POINT ( 'NONE',  ( -0.7185039370078739607, 1.928577636452523993E-17, 0.3051181102362204856 ) ) ;
#35914 = CARTESIAN_POINT ( 'NONE',  ( -0.1264236179284866091, -0.2476633383079787365, 0.1264236179284866091 ) ) ;
#35915 = ITEM_DEFINED_TRANSFORMATION ( 'NONE', 'NONE', #39264,  #20860 ) ;
#35916 = FACE_OUTER_BOUND ( 'NONE', #6568, .T. ) ;
#35917 = CARTESIAN_POINT ( 'NONE',  ( 0.9412147342319837628, -0.1574803149606297803, 1.055610236112945577 ) ) ;
#35918 = CARTESIAN_POINT ( 'NONE',  ( -0.6971942568897626646, 0.07405724077823318263, 0.1574803149068664809 ) ) ;
#35919 = CIRCLE ( 'NONE', #17585, 0.09842519685039370636 ) ;
#35920 = ORIENTED_EDGE ( 'NONE', *, *, #37498, .T. ) ;
#35921 = EDGE_CURVE ( 'NONE', #27211, #712, #27789, .T. ) ;
#35922 = CARTESIAN_POINT ( 'NONE',  ( -0.8019270111902716547, -0.1787899950787401604, 1.274606299158834277 ) ) ;
#35923 = EDGE_LOOP ( 'NONE', ( #18530, #46281, #38702, #24602, #35517, #11783, #8370, #18402, #11468, #42630, #31202, #22065 ) ) ;
#35924 = CARTESIAN_POINT ( 'NONE',  ( -0.1787899950787401604, -1.149606299158835387, -0.07405724077823318263 ) ) ;
#35925 = CARTESIAN_POINT ( 'NONE',  ( -0.1787899950787401604, -1.375984251914741163, 0.07405724077823318263 ) ) ;
#35926 = EDGE_CURVE ( 'NONE', #26852, #18241, #36483, .T. ) ;
#35927 = CARTESIAN_POINT ( 'NONE',  ( 0.3906197235759846786, 4.466152701071653354E-17, 0.000000000000000000 ) ) ;
#35928 = ( CONVERSION_BASED_UNIT ( 'INCH', #20836 ) LENGTH_UNIT ( ) NAMED_UNIT ( #17625 ) ) ;
#35929 = B_SPLINE_CURVE_WITH_KNOTS ( 'NONE', 3,
 ( #11965, #20074, #8574, #26817, #37825, #5209, #4981, #16496, #19603, #27542, #16031, #45455, #4735, #19837, #12677, #41854, #8105 ),
 .UNSPECIFIED., .F., .F.,
 ( 4, 2, 2, 2, 2, 1, 2, 2, 4 ),
 ( 0.000000000000000000, 0.2500000000000096034, 0.3750000000000056621, 0.5000000000000017764, 0.6249999999999978906, 0.6874999999999988898, 0.7187500000000009992, 0.7500000000000029976, 1.000000000000000000 ),
 .UNSPECIFIED. ) ;
#35930 = CARTESIAN_POINT ( 'NONE',  ( -0.9412147342319837628, -0.1574803149606297803, 0.2386811023622048278 ) ) ;
#35931 = CARTESIAN_POINT ( 'NONE',  ( -1.033464566929134687, -0.06523048226347956391, 0.9424212597349932441 ) ) ;
#35932 = CARTESIAN_POINT ( 'NONE',  ( -0.8759842519685039353, -0.1574803149606299191, 0.7480314960629921295 ) ) ;
#35933 = VECTOR ( 'NONE', #47348, 39.37007874015748854 ) ;
#35934 = CARTESIAN_POINT ( 'NONE',  ( -0.06523048226347956391, -0.1776574803149607584, 0.1574803149606297803 ) ) ;
#35935 = CARTESIAN_POINT ( 'NONE',  ( 0.7646288533564489232, -0.1113553986120547346, 1.835629921152314825 ) ) ;
#35936 = VERTEX_POINT ( 'NONE', #29147 ) ;
#35937 = CARTESIAN_POINT ( 'NONE',  ( 0.6195511811023621807, 0.9842519685039365918, -1.186023622047243986 ) ) ;
#35938 = EDGE_CURVE ( 'NONE', #43256, #13671, #9394, .T. ) ;
#35939 = CARTESIAN_POINT ( 'NONE',  ( 0.9412147342319837628, -0.1574803149606297803, 0.7898622047244097111 ) ) ;
#35940 = DIRECTION ( 'NONE',  ( -0.000000000000000000, -1.000000000000000000, -8.673617379884034486E-16 ) ) ;
#35941 = CARTESIAN_POINT ( 'NONE',  ( -0.9412147342319837628, -0.1574803149606297803, 1.606791338475149766 ) ) ;
#35943 = DIRECTION ( 'NONE',  ( 1.000000000000000000, 0.000000000000000000, -1.822029033848725275E-16 ) ) ;
#35942 = DIRECTION ( 'NONE',  ( 0.000000000000000000, 0.000000000000000000, -1.000000000000000000 ) ) ;
#35944 = CARTESIAN_POINT ( 'NONE',  ( 1.033464566929133799, 0.000000000000000000, 0.1574803148531029595 ) ) ;
#35945 = ORIENTED_EDGE ( 'NONE', *, *, #20053, .T. ) ;
#35946 = VERTEX_POINT ( 'NONE', #9547 ) ;
#35947 = CARTESIAN_POINT ( 'NONE',  ( 0.8107537697050234415, -0.1574803149606297803, 0.2337598425196852070 ) ) ;
#35948 = CARTESIAN_POINT ( 'NONE',  ( -0.06523048226347956391, 0.09301181113114896648, -0.1574803149606300301 ) ) ;
#35949 = B_SPLINE_CURVE_WITH_KNOTS ( 'NONE', 3,
 ( #2022, #19521, #5372, #12603, #34631, #20227, #23373, #41776, #8497, #37500, #1781, #30358, #1061, #9218, #27706, #37981, #34171, #12360, #22886, #5133, #33939 ),
 .UNSPECIFIED., .F., .F.,
 ( 4, 2, 1, 1, 2, 2, 2, 1, 1, 1, 2, 2, 4 ),
 ( 0.000000000000000000, 0.1249999999999948097, 0.1874999999999923672, 0.2187499999999910072, 0.2343749999999906186, 0.2499999999999902855, 0.3749999999999891753, 0.4374999999999888423, 0.4687499999999888423, 0.4843749999999888978, 0.4921874999999891753, 0.4999999999999894529, 1.000000000000000000 ),
 .UNSPECIFIED. ) ;
#35950 = CARTESIAN_POINT ( 'NONE',  ( 0.7185039370078739607, 0.000000000000000000, 4.498031496062992574 ) ) ;
#35951 = CARTESIAN_POINT ( 'NONE',  ( 0.1574803149606300301, -1.609744094380661572, -0.06523048226347956391 ) ) ;
#35952 = CARTESIAN_POINT ( 'NONE',  ( 0.1264236179284866091, -0.6205708660879685201, 0.1264236179284866091 ) ) ;
#35953 = CARTESIAN_POINT ( 'NONE',  ( -0.1574803149606297803, -1.048720472440944684, 0.06523048226347956391 ) ) ;
#35954 = CARTESIAN_POINT ( 'NONE',  ( 1.033464566929134687, 0.06523048226347956391, 0.9867125983176702197 ) ) ;
#35955 = CARTESIAN_POINT ( 'NONE',  ( 0.7185039370078739607, 1.928577636452523993E-17, 0.5413385826771653919 ) ) ;
#35956 = CIRCLE ( 'NONE', #44377, 0.1003937007874010356 ) ;
#35957 = ORIENTED_EDGE ( 'NONE', *, *, #19796, .T. ) ;
#35958 = ORIENTED_EDGE ( 'NONE', *, *, #28013, .T. ) ;
#35959 = ORIENTED_EDGE ( 'NONE', *, *, #14563, .T. ) ;
#35960 = CARTESIAN_POINT ( 'NONE',  ( -1.002407869896990045, 0.1264236179284866091, 1.606791338528913426 ) ) ;
#35961 = CARTESIAN_POINT ( 'NONE',  ( 0.7495606340400177148, -0.1264236179284866091, 1.587106299158834721 ) ) ;
#35962 = CARTESIAN_POINT ( 'NONE',  ( -1.002407869896990045, 0.1264236179284866091, 0.6225393700249762796 ) ) ;
#35963 = CARTESIAN_POINT ( 'NONE',  ( 1.002407869896990045, -0.1264236179284866091, 0.2189960629383626012 ) ) ;
#35964 = DIRECTION ( 'NONE',  ( 0.000000000000000000, 0.000000000000000000, -1.000000000000000000 ) ) ;
#35965 = CARTESIAN_POINT ( 'NONE',  ( 1.054774247047244540, -0.07405724077823318263, 0.7726377952218266287 ) ) ;
#35966 = CARTESIAN_POINT ( 'NONE',  ( -0.6971942568897637749, 2.189545951927499583E-17, 0.7111220471903307860 ) ) ;
#35967 = CIRCLE ( 'NONE', #15308, 0.04921259842519691563 ) ;
#35968 = CARTESIAN_POINT ( 'NONE',  ( 0.1588219152425836833, -0.09266989036297294813, 0.1937372027061967927 ) ) ;
#35969 = CARTESIAN_POINT ( 'NONE',  ( 1.033464566929133799, 0.000000000000000000, 1.151574803149606474 ) ) ;
#35970 = CARTESIAN_POINT ( 'NONE',  ( 0.1574803149606300301, -0.2711614172153075097, -0.06523048226347956391 ) ) ;
#35971 = CARTESIAN_POINT ( 'NONE',  ( -0.6971942568897648851, -0.07405724077823297447, 1.427165354276944687 ) ) ;
#35972 = CARTESIAN_POINT ( 'NONE',  ( -0.7646288533564489232, -0.1113553986120547346, 0.3887795275590551491 ) ) ;
#35973 = CARTESIAN_POINT ( 'NONE',  ( 0.9500414927467377701, 0.1787899950787401604, 1.530511810969859221 ) ) ;
#35974 = CARTESIAN_POINT ( 'NONE',  ( -0.7646288533564489232, 0.1113553986120547346, 0.3690944880814492901 ) ) ;
#35975 = ORIENTED_EDGE ( 'NONE', *, *, #45978, .T. ) ;
#35976 = EDGE_CURVE ( 'NONE', #9930, #18657, #24168, .T. ) ;
#35977 = DIRECTION ( 'NONE',  ( 1.000000000000000000, 0.000000000000000000, 0.000000000000000000 ) ) ;
#35978 = CARTESIAN_POINT ( 'NONE',  ( 0.07405724077823318263, -1.696974361930027708, 0.1787899950787401604 ) ) ;
#35979 = ORIENTED_EDGE ( 'NONE', *, *, #15840, .F. ) ;
#35980 = EDGE_CURVE ( 'NONE', #44026, #9783, #44976, .T. ) ;
#35981 = CARTESIAN_POINT ( 'NONE',  ( 1.033464566929134687, 0.06523048226347956391, 0.4847440944881890590 ) ) ;
#35982 = VERTEX_POINT ( 'NONE', #15442 ) ;
#35983 = CARTESIAN_POINT ( 'NONE',  ( 0.9500414927467378812, 0.1787899950787401604, 1.446850393647023614 ) ) ;
#35984 = DIRECTION ( 'NONE',  ( 1.000000000000000000, 0.000000000000000000, -1.822029033848725275E-16 ) ) ;
#35985 = CARTESIAN_POINT ( 'NONE',  ( 0.07405724077823318263, -0.8543307086076546986, 0.1787899950787401604 ) ) ;
#35986 = AXIS2_PLACEMENT_3D ( 'NONE', #22732, #2675, #18891 ) ;
#35987 = DIRECTION ( 'NONE',  ( -1.000000000000000000, 0.000000000000000000, 0.000000000000000000 ) ) ;
#35988 = CARTESIAN_POINT ( 'NONE',  ( 0.1644020957507539848, -0.1623118080249112138, 7.560884646099310910E-18 ) ) ;
#35989 = CARTESIAN_POINT ( 'NONE',  ( 0.6971942568897626646, -0.07405724077823297447, 0.3198818897100162983 ) ) ;
#35990 = CARTESIAN_POINT ( 'NONE',  ( 0.1787899950787401604, -0.1566200312213647527, 0.07405724077823318263 ) ) ;
#35992 = AXIS2_PLACEMENT_3D ( 'NONE', #24056, #12333, #19964 ) ;
#35991 = CARTESIAN_POINT ( 'NONE',  ( 3.284318927891251994E-17, -0.3056102361667090705, 0.1787899950787401882 ) ) ;
#35993 = CARTESIAN_POINT ( 'NONE',  ( 3.284318927891251994E-17, 0.04379921265218874454, 0.1787899950787401882 ) ) ;
#35994 = DIRECTION ( 'NONE',  ( -1.000000000000000000, 0.000000000000000000, 0.000000000000000000 ) ) ;
#35995 = CARTESIAN_POINT ( 'NONE',  ( -0.8107537697050254399, -0.1574803149606297803, 1.690452755905512916 ) ) ;
#35996 = CARTESIAN_POINT ( 'NONE',  ( 1.054774247047244540, -0.07405724077823318263, 0.6496062991588353874 ) ) ;
#35997 = AXIS2_PLACEMENT_3D ( 'NONE', #470, #15125, #37371 ) ;
#35998 = CARTESIAN_POINT ( 'NONE',  ( -0.6971942568897648851, -0.07405724077823297447, 1.033464566875371027 ) ) ;
#36000 = LINE ( 'NONE', #3158, #11653 ) ;
#35999 = CARTESIAN_POINT ( 'NONE',  ( -1.014932596384295227, 0.08658232834094778396, 0.03937007874015843040 ) ) ;
#36001 = CARTESIAN_POINT ( 'NONE',  ( 0.1270800023317771588, -1.669335148165722371, -0.1270800023317771588 ) ) ;
#36002 = CARTESIAN_POINT ( 'NONE',  ( -0.1264236179284866091, -0.4384842519147402196, -0.1264236179284866091 ) ) ;
#36003 = CARTESIAN_POINT ( 'NONE',  ( 0.7495606340400177148, 0.1264236179284866091, 1.656003936954110412 ) ) ;
#36005 = DIRECTION ( 'NONE',  ( 0.000000000000000000, 6.938893903907222856E-15, 1.000000000000000000 ) ) ;
#36004 = CARTESIAN_POINT ( 'NONE',  ( 0.7495606340400177148, 0.1264236179284866091, 1.926673228292693052 ) ) ;
#36006 = ORIENTED_EDGE ( 'NONE', *, *, #254, .F. ) ;
#36007 = CARTESIAN_POINT ( 'NONE',  ( 0.8107537697050254399, -0.1574803149606297803, 1.326279527451528661 ) ) ;
#36009 = CARTESIAN_POINT ( 'NONE',  ( -0.1787899950787401604, -0.08169291333206318839, 0.07405724077823318263 ) ) ;
#36008 = CARTESIAN_POINT ( 'NONE',  ( -0.1113553986120547346, -0.9183070865066457200, 0.1113553986120547346 ) ) ;
#36010 = CARTESIAN_POINT ( 'NONE',  ( 1.002407869896990045, -0.1264236179284866091, 0.5290354330171024300 ) ) ;
#36011 = CARTESIAN_POINT ( 'NONE',  ( 0.1787899950787401882, -1.083169291284818980, -2.189545951927503898E-17 ) ) ;
#36012 = CARTESIAN_POINT ( 'NONE',  ( 0.9500414927467378812, 0.1787899950787401604, 0.1525590550643468046 ) ) ;
#36013 = CARTESIAN_POINT ( 'NONE',  ( 0.1574803149606300023, 2.117069812090769609, -1.766975050165344951 ) ) ;
#36014 = CARTESIAN_POINT ( 'NONE',  ( -0.8019270111902717657, 0.1787899950787401604, 1.569881889710015299 ) ) ;
#36015 = ORIENTED_EDGE ( 'NONE', *, *, #3680, .T. ) ;
#36016 = CARTESIAN_POINT ( 'NONE',  ( 0.5962569168439626477, 4.766607801171850497E-17, 0.000000000000000000 ) ) ;
#36017 = CARTESIAN_POINT ( 'NONE',  ( 1.054774247047244096, 0.000000000000000000, 1.168799212544661348 ) ) ;
#36018 = ORIENTED_EDGE ( 'NONE', *, *, #42928, .T. ) ;
#36019 = CARTESIAN_POINT ( 'NONE',  ( 0.8759842519685039353, -0.1574803149606299191, 1.496062992125984259 ) ) ;
#36020 = CARTESIAN_POINT ( 'NONE',  ( 0.8759842519685039353, -0.1787899950787401882, 1.823326771599779406 ) ) ;
#36021 = CARTESIAN_POINT ( 'NONE',  ( -0.7185039370078746268, 0.06523048226347956391, 0.5782480314960627421 ) ) ;
#36022 = CARTESIAN_POINT ( 'NONE',  ( -1.054774247047244540, 0.07405724077823318263, 0.9301181101824563813 ) ) ;
#36023 = CARTESIAN_POINT ( 'NONE',  ( -1.033464566929136907, -0.06523048226347749612, 1.621555118110237670 ) ) ;
#36024 = DIRECTION ( 'NONE',  ( 0.000000000000000000, -1.000000000000000000, 0.000000000000000000 ) ) ;
#36025 = CARTESIAN_POINT ( 'NONE',  ( 0.7495606340400177148, -0.1264236179284866091, 0.2485236219934806867 ) ) ;
#36026 = CARTESIAN_POINT ( 'NONE',  ( -1.054774247047244096, 0.000000000000000000, 0.2583661416785200671 ) ) ;
#36027 = CARTESIAN_POINT ( 'NONE',  ( -0.8759842519685039353, -0.1787899950787401882, 0.5241141731745827537 ) ) ;
#36028 = CARTESIAN_POINT ( 'NONE',  ( 0.8107537697050253289, -0.1574803149606297803, 1.562499999892472458 ) ) ;
#36029 = ORIENTED_EDGE ( 'NONE', *, *, #36038, .F. ) ;
#36030 = AXIS2_PLACEMENT_3D ( 'NONE', #9252, #39172, #31315 ) ;
#36031 = CARTESIAN_POINT ( 'NONE',  ( 3.284318927891251994E-17, -0.03494094482812622193, 0.1787899950787401882 ) ) ;
#36032 = MANIFOLD_SOLID_BREP ( 'Handle Arm Left', #33946 ) ;
#36033 = CARTESIAN_POINT ( 'NONE',  ( 0.7495606340400177148, -0.1264236179284866091, 0.7603346456155274380 ) ) ;
#36034 = CARTESIAN_POINT ( 'NONE',  ( -1.002407869896990045, -0.1264236179284866091, 1.867618110182456714 ) ) ;
#36035 = VECTOR ( 'NONE', #28191, 39.37007874015748143 ) ;
#36036 = EDGE_CURVE ( 'NONE', #46399, #44357, #4374, .T. ) ;
#36037 = AXIS2_PLACEMENT_3D ( 'NONE', #15169, #40760, #22807 ) ;
#36038 = EDGE_CURVE ( 'NONE', #17227, #27120, #13797, .T. ) ;
#36039 = CYLINDRICAL_SURFACE ( 'NONE', #16876, 0.02900000000000000147 ) ;
#36040 = DIRECTION ( 'NONE',  ( 1.000000000000000000, 0.000000000000000000, 0.000000000000000000 ) ) ;
#36041 = CARTESIAN_POINT ( 'NONE',  ( 3.284318927891251994E-17, -1.266364125709553257, 0.1787899950787401882 ) ) ;
#36042 = ORIENTED_EDGE ( 'NONE', *, *, #27705, .F. ) ;
#36043 = CARTESIAN_POINT ( 'NONE',  ( -1.094772975963752103E-17, -0.2071850393163153503, -0.1787899950787401882 ) ) ;
#36044 = ADVANCED_FACE ( 'NONE', ( #4615 ), #11754, .T. ) ;
#36045 = DIRECTION ( 'NONE',  ( 1.000000000000000000, 0.000000000000000000, 0.000000000000000000 ) ) ;
#36046 = ORIENTED_EDGE ( 'NONE', *, *, #23757, .F. ) ;
#36047 = EDGE_CURVE ( 'NONE', #34943, #34914, #36764, .T. ) ;
#36048 = CYLINDRICAL_SURFACE ( 'NONE', #20796, 0.09842519685039320676 ) ;
#36049 = CARTESIAN_POINT ( 'NONE',  ( 0.8759842519685039353, 0.1574803149606299191, 1.948818897637795367 ) ) ;
#36050 = CARTESIAN_POINT ( 'NONE',  ( 0.1787899950787401604, -1.641732283410802573, 0.07405724077823318263 ) ) ;
#36051 = CARTESIAN_POINT ( 'NONE',  ( 0.1787899950787401604, -0.7312992125446612368, -0.07405724077823318263 ) ) ;
#36052 = CIRCLE ( 'NONE', #17683, 0.09842519685039370636 ) ;
#36053 = CARTESIAN_POINT ( 'NONE',  ( -1.002407869896990045, -0.1264236179284866091, 0.4158464566391496531 ) ) ;
#36054 = CARTESIAN_POINT ( 'NONE',  ( -0.8107537697050254399, 0.1574803149606300301, 1.203248031496062520 ) ) ;
#36055 = CARTESIAN_POINT ( 'NONE',  ( 1.002407869896990045, -0.1264236179284866091, 1.203248031442299304 ) ) ;
#36056 = CARTESIAN_POINT ( 'NONE',  ( 0.8759842519685039353, 0.1787899950787401882, 1.488681102308440751 ) ) ;
#36057 = VECTOR ( 'NONE', #38279, 39.37007874015748143 ) ;
#36058 = CARTESIAN_POINT ( 'NONE',  ( -1.033464566929133799, 0.000000000000000000, 1.899606299212598604 ) ) ;
#36059 = CARTESIAN_POINT ( 'NONE',  ( -1.033464566929133799, 0.000000000000000000, 0.5905511809948347235 ) ) ;
#36060 = VECTOR ( 'NONE', #14145, 39.37007874015748143 ) ;
#36061 = CARTESIAN_POINT ( 'NONE',  ( -0.8759842519685039353, 0.000000000000000000, 0.000000000000000000 ) ) ;
#36062 = CARTESIAN_POINT ( 'NONE',  ( -1.033464566929134687, 0.06523048226347956391, 1.734744094380662904 ) ) ;
#36063 = CARTESIAN_POINT ( 'NONE',  ( 0.6971942568897637749, 2.189545951927499583E-17, 0.2386811023084413619 ) ) ;
#36064 = CARTESIAN_POINT ( 'NONE',  ( -1.033464566929133799, 0.000000000000000000, 1.348425196850393748 ) ) ;
#36066 = CARTESIAN_POINT ( 'NONE',  ( 0.2204724409448818867, 0.07955613945526338049, -0.1377952755905511861 ) ) ;
#36065 = CARTESIAN_POINT ( 'NONE',  ( 0.8759842519685039353, -0.1787899950787401882, 1.075295275536787276 ) ) ;
#36067 = DIRECTION ( 'NONE',  ( 0.000000000000000000, 0.000000000000000000, -1.000000000000000000 ) ) ;
#36068 = CARTESIAN_POINT ( 'NONE',  ( -0.8759842519685039353, 0.1787899950787401882, 1.213090551127338435 ) ) ;
#36069 = CARTESIAN_POINT ( 'NONE',  ( 0.7185039370078746268, 0.06523048226347956391, 0.5290354329633386588 ) ) ;
#36070 = ORIENTED_EDGE ( 'NONE', *, *, #10741, .F. ) ;
#36071 = DIRECTION ( 'NONE',  ( 0.000000000000000000, -0.7880107536067204599, 0.6156614753256602901 ) ) ;
#36072 = CARTESIAN_POINT ( 'NONE',  ( 0.9294026713671079687, 0.1625504865516811670, 0.03937007694543066122 ) ) ;
#36073 = CARTESIAN_POINT ( 'NONE',  ( 0.7646288533564489232, -0.1113553986120547346, 0.2706692913385826960 ) ) ;
#36074 = CARTESIAN_POINT ( 'NONE',  ( -0.9873396505805591694, -0.1113553986120547346, 0.3887795274515282729 ) ) ;
#36075 = ORIENTED_EDGE ( 'NONE', *, *, #41625, .F. ) ;
#36076 = CARTESIAN_POINT ( 'NONE',  ( 0.9500414927467378812, 0.1787899950787401604, 1.407480314906865981 ) ) ;
#36078 = CARTESIAN_POINT ( 'NONE',  ( -0.7185039370078739607, 1.928577636452523993E-17, 0.2952755904436539236 ) ) ;
#36077 = CARTESIAN_POINT ( 'NONE',  ( -0.4620708661417322616, 0.9842519685039370358, -0.7135826771653542844 ) ) ;
#36079 = DIRECTION ( 'NONE',  ( 0.000000000000000000, 0.000000000000000000, 1.000000000000000000 ) ) ;
#36080 = CARTESIAN_POINT ( 'NONE',  ( 0.1787899950787401882, -0.02017716530056720692, -2.189545951927503898E-17 ) ) ;
#36081 = ORIENTED_EDGE ( 'NONE', *, *, #4516, .T. ) ;
#36082 = ( BOUNDED_CURVE ( )  B_SPLINE_CURVE ( 2, ( #14057, #18122, #3260, #24841, #43753, #25325, #32042, #3511, #32768 ),
 .UNSPECIFIED., .F., .F. ) 
 B_SPLINE_CURVE_WITH_KNOTS ( ( 3, 2, 2, 2, 3 ),
 ( 0.07499999999999999722, 0.07749999999999999944, 0.08000000000000000167, 0.08250000000000000389, 0.08500000000000000611 ),
 .UNSPECIFIED. ) 
 CURVE ( )  GEOMETRIC_REPRESENTATION_ITEM ( )  RATIONAL_B_SPLINE_CURVE ( ( 1.000000000000000000, 0.9238795325112869605, 1.000000000000000000, 0.9238795325112869605, 1.000000000000000000, 0.9238795325112869605, 1.000000000000000000, 0.9238795325112869605, 1.000000000000000000 ) ) 
 REPRESENTATION_ITEM ( '' )  ) ;
#36083 = CARTESIAN_POINT ( 'NONE',  ( -0.1377952755905513527, 1.687505431895961344E-17, -0.3001770169643759867 ) ) ;
#36084 = CARTESIAN_POINT ( 'NONE',  ( 0.1293255151920606749, -0.09842519685039366473, -0.2107669498569183786 ) ) ;
#36085 = ( BOUNDED_CURVE ( )  B_SPLINE_CURVE ( 2, ( #17389, #46386, #24590, #39898, #39187, #46152, #46618, #13346, #9978 ),
 .UNSPECIFIED., .F., .T. ) 
 B_SPLINE_CURVE_WITH_KNOTS ( ( 3, 2, 2, 2, 3 ),
 ( 0.2500000000000000000, 0.2525000000000000022, 0.2550000000000000044, 0.2575000000000000067, 0.2600000000000000089 ),
 .UNSPECIFIED. ) 
 CURVE ( )  GEOMETRIC_REPRESENTATION_ITEM ( )  RATIONAL_B_SPLINE_CURVE ( ( 1.000000000000000000, 0.9238795325112869605, 1.000000000000000000, 0.9238795325112869605, 1.000000000000000000, 0.9238795325112869605, 1.000000000000000000, 0.9238795325112869605, 1.000000000000000000 ) ) 
 REPRESENTATION_ITEM ( '' )  ) ;
#36086 = VERTEX_POINT ( 'NONE', #19487 ) ;
#36087 = ADVANCED_FACE ( 'NONE', ( #34135 ), #1265, .T. ) ;
#36088 = CARTESIAN_POINT ( 'NONE',  ( 0.6971942568897626646, -0.07405724077823297447, 0.5610236219934807700 ) ) ;
#36089 = ORIENTED_EDGE ( 'NONE', *, *, #8998, .F. ) ;
#36090 = CARTESIAN_POINT ( 'NONE',  ( -0.6971942568897648851, 0.07405724077823318263, 1.496062992072220599 ) ) ;
#36091 = CARTESIAN_POINT ( 'NONE',  ( 0.1574803149606300301, 0.07824803160359000698, 0.06523048226347956391 ) ) ;
#36092 = CARTESIAN_POINT ( 'NONE',  ( -1.002407869896990045, 0.1264236179284866091, 1.134350393647023614 ) ) ;
#36093 = CARTESIAN_POINT ( 'NONE',  ( -1.033464566929133799, 0.000000000000000000, 0.1279527559055118058 ) ) ;
#36094 = CARTESIAN_POINT ( 'NONE',  ( -0.7495606340400177148, -0.1264236179284866091, 1.031003936954110189 ) ) ;
#36095 = EDGE_CURVE ( 'NONE', #30092, #43921, #10093, .T. ) ;
#36096 = VECTOR ( 'NONE', #41035, 39.37007874015748143 ) ;
#36097 = FACE_OUTER_BOUND ( 'NONE', #16479, .T. ) ;
#36098 = DIRECTION ( 'NONE',  ( 1.822029033848725028E-16, 0.000000000000000000, 1.000000000000000000 ) ) ;
#36099 = CARTESIAN_POINT ( 'NONE',  ( -0.1787899950787401604, -0.8800452280717578901, 0.07405724077823318263 ) ) ;
#36100 = ORIENTED_EDGE ( 'NONE', *, *, #25382, .T. ) ;
#36101 = CARTESIAN_POINT ( 'NONE',  ( 0.1099139000111727243, -0.5708661417322835607, 1.120507485783946100 ) ) ;
#36102 = CARTESIAN_POINT ( 'NONE',  ( 0.7628455132511623438, 0.1385261779602319776, 0.03937407183360309981 ) ) ;
#36103 = ORIENTED_EDGE ( 'NONE', *, *, #7622, .F. ) ;
#36104 = VERTEX_POINT ( 'NONE', #42227 ) ;
#36105 = CARTESIAN_POINT ( 'NONE',  ( 0.1574803149606300023, -0.2714884749021748700, -1.284167712019357976 ) ) ;
#36106 = VECTOR ( 'NONE', #11833, 39.37007874015748854 ) ;
#36107 = VECTOR ( 'NONE', #47388, 39.37007874015748854 ) ;
#36108 = EDGE_CURVE ( 'NONE', #24890, #10722, #4060, .T. ) ;
#36110 = CYLINDRICAL_SURFACE ( 'NONE', #37943, 0.1574803149606299191 ) ;
#36109 = CIRCLE ( 'NONE', #21556, 0.1864803149606298061 ) ;
#36111 = CARTESIAN_POINT ( 'NONE',  ( -0.6971942568897637749, 2.189545951927499583E-17, 0.6717519684501732646 ) ) ;
#36112 = DIRECTION ( 'NONE',  ( 0.000000000000000000, 0.000000000000000000, -1.000000000000000000 ) ) ;
#36113 = CARTESIAN_POINT ( 'NONE',  ( -0.7495606340400177148, -0.1264236179284866091, 1.744586614119464807 ) ) ;
#36114 = EDGE_LOOP ( 'NONE', ( #14060, #45841, #4103, #29648 ) ) ;
#36115 = CARTESIAN_POINT ( 'NONE',  ( 0.7185039370078739607, 1.928577636452523993E-17, 0.6102362203649134287 ) ) ;
#36116 = CARTESIAN_POINT ( 'NONE',  ( -0.6971942568897637749, 2.189545951927499583E-17, 0.1254921259304885850 ) ) ;
#36117 = ORIENTED_EDGE ( 'NONE', *, *, #6428, .F. ) ;
#36118 = CARTESIAN_POINT ( 'NONE',  ( 0.8107537697050253289, 0.1574803149606300301, 0.6520669291338586637 ) ) ;
#36119 = CARTESIAN_POINT ( 'NONE',  ( -0.1797182628040039365, -0.8277997150948562810, 0.000000000000000000 ) ) ;
#36120 = CARTESIAN_POINT ( 'NONE',  ( 0.2471922904502826257, 0.09842519685039370636, 0.006585516632626051831 ) ) ;
#36121 = CARTESIAN_POINT ( 'NONE',  ( -0.9412147342319837628, -0.1574803149606297803, 1.449311023514519681 ) ) ;
#36122 = CARTESIAN_POINT ( 'NONE',  ( 1.002407869896990045, -0.1264236179284866091, 0.7701771653005669016 ) ) ;
#36123 = CARTESIAN_POINT ( 'NONE',  ( -0.1113553986120547346, -0.6525590551181101873, 0.1113553986120547346 ) ) ;
#36124 = CARTESIAN_POINT ( 'NONE',  ( 0.9412147342319837628, 0.1574803149606300301, 1.621555118002709683 ) ) ;
#36125 = CARTESIAN_POINT ( 'NONE',  ( -0.2559055118110236116, 0.08129156908512058521, -0.05439871778755192566 ) ) ;
#36126 = CONICAL_SURFACE ( 'NONE', #5511, 0.2559055118110236116, 1.047197551196597409 ) ;
#36127 = CARTESIAN_POINT ( 'NONE',  ( 1.033464566929134687, -0.06523048226347956391, 1.227854330708661124 ) ) ;
#36128 = CARTESIAN_POINT ( 'NONE',  ( -0.1476377952755905387, 0.4754249043493458116, -0.4843814799190158116 ) ) ;
#36129 = CARTESIAN_POINT ( 'NONE',  ( 0.7759784704967711555, -0.1388558036440012133, 1.986221128314594742 ) ) ;
#36130 = DIRECTION ( 'NONE',  ( 8.117793622096712470E-16, -0.6156614753256580697, -0.7880107536067222362 ) ) ;
#36131 = EDGE_CURVE ( 'NONE', #22180, #47216, #41332, .T. ) ;
#36132 = VECTOR ( 'NONE', #30267, 39.37007874015748143 ) ;
#36134 = CARTESIAN_POINT ( 'NONE',  ( 0.9873396505805591694, -0.1113553986120547346, 0.2706692912310554866 ) ) ;
#36133 = CARTESIAN_POINT ( 'NONE',  ( 1.002407869896990045, -0.1264236179284866091, 0.6471456692375747721 ) ) ;
#36135 = CARTESIAN_POINT ( 'NONE',  ( -0.7646288533564489232, 0.1113553986120547346, 0.6938976377952755792 ) ) ;
#36136 = DIRECTION ( 'NONE',  ( 0.000000000000000000, 0.000000000000000000, 1.000000000000000000 ) ) ;
#36137 = ORIENTED_EDGE ( 'NONE', *, *, #25255, .F. ) ;
#36138 = CARTESIAN_POINT ( 'NONE',  ( 0.8759842519685039353, 0.000000000000000000, 4.498031496062992574 ) ) ;
#36139 = CIRCLE ( 'NONE', #13963, 0.02900000000000064679 ) ;
#36141 = FACE_OUTER_BOUND ( 'NONE', #12600, .T. ) ;
#36140 = AXIS2_PLACEMENT_3D ( 'NONE', #28137, #6533, #43420 ) ;
#36142 = CARTESIAN_POINT ( 'NONE',  ( 0.9500414927467378812, -0.1787899950787401604, 1.038385826717890259 ) ) ;
#36143 = VERTEX_POINT ( 'NONE', #27432 ) ;
#36144 = CARTESIAN_POINT ( 'NONE',  ( 0.2559055118110236116, 0.1477471161312027548, -0.3149606299212598381 ) ) ;
#36145 = CARTESIAN_POINT ( 'NONE',  ( 0.07444174185955046430, 0.02603886758230882295, -0.1797182628040039087 ) ) ;
#36146 = CARTESIAN_POINT ( 'NONE',  ( 0.1264236179284866091, -1.161909448765133801, -0.1264236179284866091 ) ) ;
#36147 = CARTESIAN_POINT ( 'NONE',  ( 0.06523048226347956391, -1.550688976377951889, 0.1574803149606297803 ) ) ;
#36148 = DIRECTION ( 'NONE',  ( 0.000000000000000000, 0.000000000000000000, -1.000000000000000000 ) ) ;
#36149 = VERTEX_POINT ( 'NONE', #16836 ) ;
#36150 = CARTESIAN_POINT ( 'NONE',  ( -1.002407869896990045, 0.1264236179284866091, 0.02706692908009476414 ) ) ;
#36152 = ORIENTED_EDGE ( 'NONE', *, *, #19162, .T. ) ;
#36151 = AXIS2_PLACEMENT_3D ( 'NONE', #12148, #23405, #16450 ) ;
#36153 = CARTESIAN_POINT ( 'NONE',  ( 1.054774247047244540, -0.07405724077823318263, 1.953740157426552715 ) ) ;
#36154 = ORIENTED_EDGE ( 'NONE', *, *, #39010, .T. ) ;
#36155 = CARTESIAN_POINT ( 'NONE',  ( 0.06523048226347956391, -1.407972440837354622, -0.1574803149606300301 ) ) ;
#36156 = CARTESIAN_POINT ( 'NONE',  ( -0.7495606340400177148, -0.1264236179284866091, 1.980807086560409491 ) ) ;
#36157 = CARTESIAN_POINT ( 'NONE',  ( -0.8019270111902717657, -0.1787899950787401604, 1.702755905458047003 ) ) ;
#36158 = CARTESIAN_POINT ( 'NONE',  ( 0.7495606340400177148, 0.1264236179284866091, 0.9079724408911180600 ) ) ;
#36159 = CARTESIAN_POINT ( 'NONE',  ( -0.6971942568897648851, 0.07405724077823318263, 1.062992125930488418 ) ) ;
#36160 = CARTESIAN_POINT ( 'NONE',  ( -0.8759842519685039353, -0.1787899950787401882, 0.3715551180564728440 ) ) ;
#36161 = EDGE_CURVE ( 'NONE', #26252, #15853, #34708, .T. ) ;
#36162 = CARTESIAN_POINT ( 'NONE',  ( -0.7646288533564489232, -0.1113553986120547346, 0.6643700787401575214 ) ) ;
#36163 = CARTESIAN_POINT ( 'NONE',  ( -0.8759842519685039353, -0.1787899950787401882, 1.867618110182456714 ) ) ;
#36164 = CARTESIAN_POINT ( 'NONE',  ( -0.8107537697050254399, 0.1574803149606300301, 1.478838582677165059 ) ) ;
#36165 = CARTESIAN_POINT ( 'NONE',  ( -0.8759842519685039353, -0.1574803149606299191, 1.889763779527559251 ) ) ;
#36166 = CARTESIAN_POINT ( 'NONE',  ( -1.033464566929134687, -0.06523048226347956391, 1.897145669291339543 ) ) ;
#36167 = CARTESIAN_POINT ( 'NONE',  ( 0.07405724077823318263, -0.3977617635048297240, 0.1787899950787401604 ) ) ;
#36168 = CARTESIAN_POINT ( 'NONE',  ( -0.07591074332868011365, -0.09842519685039370636, 0.1427273573094925141 ) ) ;
#36169 = CARTESIAN_POINT ( 'NONE',  ( 0.1822895153388602307, 2.589602477342551251E-17, 0.2114570894355444486 ) ) ;
#36170 = DIRECTION ( 'NONE',  ( -0.000000000000000000, 1.000000000000000000, -3.995705278811693553E-31 ) ) ;
#36171 = EDGE_CURVE ( 'NONE', #32743, #27640, #38170, .T. ) ;
#36172 = CARTESIAN_POINT ( 'NONE',  ( -0.8019270111902717657, 0.1787899950787401604, 0.1525590550643468046 ) ) ;
#36173 = AXIS2_PLACEMENT_3D ( 'NONE', #18342, #7324, #33702 ) ;
#36174 = CARTESIAN_POINT ( 'NONE',  ( 0.7185039370078739607, 0.000000000000000000, 4.498031496062992574 ) ) ;
#36175 = ORIENTED_EDGE ( 'NONE', *, *, #22498, .F. ) ;
#36176 = ORIENTED_EDGE ( 'NONE', *, *, #9551, .F. ) ;
#36177 = CARTESIAN_POINT ( 'NONE',  ( -1.054774247047244540, 0.07405724077823318263, 1.368110236166710125 ) ) ;
#36178 = ORIENTED_EDGE ( 'NONE', *, *, #476, .F. ) ;
#36179 = AXIS2_PLACEMENT_3D ( 'NONE', #8717, #16403, #31029 ) ;
#36180 = CARTESIAN_POINT ( 'NONE',  ( -0.1264236179284866091, -1.220964566875370139, 0.1264236179284866091 ) ) ;
#36181 = CARTESIAN_POINT ( 'NONE',  ( -0.07405724077823318263, -1.410433070812377565, 0.1787899950787401604 ) ) ;
#36182 = CARTESIAN_POINT ( 'NONE',  ( -0.1377952755905511861, 1.808041534174241898E-17, -0.2495040853978291451 ) ) ;
#36183 = DIRECTION ( 'NONE',  ( -0.9955207525527449697, 0.09454327705773898916, 0.000000000000000000 ) ) ;
#36184 = CARTESIAN_POINT ( 'NONE',  ( 1.033464566929134687, -0.06523048226347956391, 0.3617125984251968740 ) ) ;
#36185 = CARTESIAN_POINT ( 'NONE',  ( -1.033464566929133799, 0.000000000000000000, 0.2460629921259842590 ) ) ;
#36186 = CARTESIAN_POINT ( 'NONE',  ( -0.8759842519685039353, 0.1574803149606299191, 0.9153543306011338032 ) ) ;
#36187 = AXIS2_PLACEMENT_3D ( 'NONE', #11552, #41623, #9071 ) ;
#36188 = CARTESIAN_POINT ( 'NONE',  ( 0.6971942568897626646, -0.07405724077823297447, 0.4822834645131655606 ) ) ;
#36189 = CARTESIAN_POINT ( 'NONE',  ( 0.9412147342319837628, -0.1574803149606297803, 1.882381889656251861 ) ) ;
#36190 = ORIENTED_EDGE ( 'NONE', *, *, #28317, .T. ) ;
#36191 = CARTESIAN_POINT ( 'NONE',  ( 1.033464566929133799, 0.000000000000000000, 1.624015748031496287 ) ) ;
#36192 = CARTESIAN_POINT ( 'NONE',  ( 0.7185039370078746268, 0.06523048226347956391, 0.7357283464566919395 ) ) ;
#36193 = CARTESIAN_POINT ( 'NONE',  ( 0.07691592068038602403, -0.2510868047526202962, -0.04147023971060104924 ) ) ;
#36194 = FACE_OUTER_BOUND ( 'NONE', #38021, .T. ) ;
#36196 = CARTESIAN_POINT ( 'NONE',  ( 0.1566053014577344915, -0.1147315712536507021, -0.08204192511022338763 ) ) ;
#36195 = CYLINDRICAL_SURFACE ( 'NONE', #41550, 0.1574803149606299191 ) ;
#36197 = CARTESIAN_POINT ( 'NONE',  ( 0.8107537697050253289, 0.1574803149606300301, 0.2485236219397170265 ) ) ;
#36198 = ORIENTED_EDGE ( 'NONE', *, *, #14473, .F. ) ;
#36199 = CARTESIAN_POINT ( 'NONE',  ( -0.1787899950787401604, -0.04232283459190579189, -0.07405724077823318263 ) ) ;
#36200 = ORIENTED_EDGE ( 'NONE', *, *, #24908, .T. ) ;
#36201 = CARTESIAN_POINT ( 'NONE',  ( 2.892866454678787531E-17, 0.1102362205799679168, 0.1574803149606299191 ) ) ;
#36202 = CARTESIAN_POINT ( 'NONE',  ( 0.8759842519685039353, -0.1574803149606299191, 1.840551180994834501 ) ) ;
#36203 = CARTESIAN_POINT ( 'NONE',  ( 0.1574803149606300301, -1.531003936900347639, -0.06523048226347956391 ) ) ;
#36204 = CARTESIAN_POINT ( 'NONE',  ( -0.1787899950787401882, -0.6747047243556849594, 0.000000000000000000 ) ) ;
#36205 = CARTESIAN_POINT ( 'NONE',  ( -0.9412147342319837628, -0.1574803149606297803, 0.1500984250893234451 ) ) ;
#36206 = CARTESIAN_POINT ( 'NONE',  ( -0.1574803149606297803, -1.088090551181102539, 0.06523048226347956391 ) ) ;
#36207 = CARTESIAN_POINT ( 'NONE',  ( 0.9412147342319837628, 0.1574803149606300301, 0.9916338581601894520 ) ) ;
#36208 = ( BOUNDED_CURVE ( )  B_SPLINE_CURVE ( 2, ( #46144, #46380, #9266, #5421, #42062, #13559, #27272, #20040, #5901 ),
 .UNSPECIFIED., .F., .T. ) 
 B_SPLINE_CURVE_WITH_KNOTS ( ( 3, 2, 2, 2, 3 ),
 ( 0.5999999999999999778, 0.6025000000000000355, 0.6049999999999999822, 0.6075000000000000400, 0.6099999999999999867 ),
 .UNSPECIFIED. ) 
 CURVE ( )  GEOMETRIC_REPRESENTATION_ITEM ( )  RATIONAL_B_SPLINE_CURVE ( ( 1.000000000000000000, 0.9238795325112869605, 1.000000000000000000, 0.9238795325112869605, 1.000000000000000000, 0.9238795325112869605, 1.000000000000000000, 0.9238795325112829637, 1.000000000000000000 ) ) 
 REPRESENTATION_ITEM ( '' )  ) ;
#36209 = CONICAL_SURFACE ( 'NONE', #30854, 0.1574803149606299191, 0.9599310885968735940 ) ;
#36210 = CARTESIAN_POINT ( 'NONE',  ( -1.054774247047244540, -0.07405724077823318263, 0.3346456692375748831 ) ) ;
#36211 = VERTEX_POINT ( 'NONE', #41495 ) ;
#36212 = ORIENTED_EDGE ( 'NONE', *, *, #8645, .F. ) ;
#36213 = VERTEX_POINT ( 'NONE', #5333 ) ;
#36214 = CARTESIAN_POINT ( 'NONE',  ( -0.8019270111902717657, 0.1787899950787401604, 1.653543307032850462 ) ) ;
#36215 = EDGE_CURVE ( 'NONE', #5433, #33302, #24049, .T. ) ;
#36216 = CARTESIAN_POINT ( 'NONE',  ( 0.6971942568897637749, 2.189545951927499583E-17, 1.621555118056472455 ) ) ;
#36217 = EDGE_CURVE ( 'NONE', #2118, #34930, #10964, .T. ) ;
#36218 = CARTESIAN_POINT ( 'NONE',  ( -0.9500414927467378812, -0.1787899950787401604, 0.8070866141194653620 ) ) ;
#36219 = AXIS2_PLACEMENT_3D ( 'NONE', #7169, #21794, #26099 ) ;
#36220 = AXIS2_PLACEMENT_3D ( 'NONE', #22864, #33211, #25994 ) ;
#36221 = CARTESIAN_POINT ( 'NONE',  ( 1.054774247047244096, 0.000000000000000000, 0.1845472440407248116 ) ) ;
#36222 = CARTESIAN_POINT ( 'NONE',  ( -0.8107537697050254399, -0.1574803149606297803, 0.4601377951680635792 ) ) ;
#36223 = CARTESIAN_POINT ( 'NONE',  ( -0.9500414927467377701, -0.1787899950787401604, 0.6840551180564720113 ) ) ;
#36224 = LINE ( 'NONE', #6962, #11617 ) ;
#36225 = ADVANCED_FACE ( 'NONE', ( #41973 ), #9181, .T. ) ;
#36226 = DIRECTION ( 'NONE',  ( -5.902779916321932142E-16, 0.2126700594527800581, -0.9771240687918557599 ) ) ;
#36227 = CARTESIAN_POINT ( 'NONE',  ( 0.1574803149606299191, -0.1948818896562523328, -1.928577636452523993E-17 ) ) ;
#36228 = ORIENTED_EDGE ( 'NONE', *, *, #43595, .F. ) ;
#36229 = CARTESIAN_POINT ( 'NONE',  ( -0.9412147342319837628, 0.1574803149606300301, 1.513287401574803681 ) ) ;
#36230 = CARTESIAN_POINT ( 'NONE',  ( -0.9412147342319837628, -0.1574803149606297803, 0.3961614173228344971 ) ) ;
#36231 = CARTESIAN_POINT ( 'NONE',  ( 0.9500414927467377701, -0.1787899950787401604, 1.397637795221827517 ) ) ;
#36232 = DIRECTION ( 'NONE',  ( 0.000000000000000000, 0.000000000000000000, -1.000000000000000000 ) ) ;
#36233 = ORIENTED_EDGE ( 'NONE', *, *, #29221, .T. ) ;
#36234 = ADVANCED_FACE ( 'NONE', ( #31714 ), #19953, .T. ) ;
#36235 = ADVANCED_FACE ( 'NONE', ( #6040 ), #8701, .T. ) ;
#36236 = CARTESIAN_POINT ( 'NONE',  ( 0.1264236179284866091, -1.763411369804041451, -0.1264236179284866091 ) ) ;
#36237 = ORIENTED_EDGE ( 'NONE', *, *, #7036, .F. ) ;
#36238 = ORIENTED_EDGE ( 'NONE', *, *, #1961, .F. ) ;
#36239 = CARTESIAN_POINT ( 'NONE',  ( -0.7185039370078739607, 0.000000000000000000, -2.869337061179095023E-17 ) ) ;
#36240 = CARTESIAN_POINT ( 'NONE',  ( 0.1787899950787401604, -0.4212598424659216856, 0.07405724077823318263 ) ) ;
#36241 = CARTESIAN_POINT ( 'NONE',  ( 0.1264236179284866091, -0.9207677164816693294, -0.1264236179284866091 ) ) ;
#36242 = CARTESIAN_POINT ( 'NONE',  ( -0.2471902452994138577, -0.09796597228571106430, -0.01325394226265560506 ) ) ;
#36243 = CARTESIAN_POINT ( 'NONE',  ( 0.2204724409448818867, 0.000000000000000000, 0.000000000000000000 ) ) ;
#36244 = CARTESIAN_POINT ( 'NONE',  ( -0.1797182628040039087, -0.2347879040712344823, 0.07444174185955065859 ) ) ;
#36245 = AXIS2_PLACEMENT_3D ( 'NONE', #28779, #6209, #20838 ) ;
#36246 = CARTESIAN_POINT ( 'NONE',  ( -1.094772975963752103E-17, -0.1443168816150655620, -0.1787899950787401882 ) ) ;
#36247 = CARTESIAN_POINT ( 'NONE',  ( -0.1787899950787401604, -0.2785433070328505734, -0.07405724077823318263 ) ) ;
#36248 = CARTESIAN_POINT ( 'NONE',  ( -0.07405724077823318263, -0.07677165348954355373, 0.1787899950787401604 ) ) ;
#36249 = DIRECTION ( 'NONE',  ( 0.000000000000000000, 1.000000000000000000, 0.000000000000000000 ) ) ;
#36250 = CARTESIAN_POINT ( 'NONE',  ( 1.054774247047244540, 0.07405724077823318263, 0.5757874015210394658 ) ) ;
#36251 = CARTESIAN_POINT ( 'NONE',  ( -0.8759842519685039353, -0.1787899950787401882, 0.9621062991588346103 ) ) ;
#36253 = CARTESIAN_POINT ( 'NONE',  ( 0.8759842519685039353, 0.1574803149606299191, 1.702755905404283565 ) ) ;
#36252 = DIRECTION ( 'NONE',  ( 1.822029033848725028E-16, 0.000000000000000000, 1.000000000000000000 ) ) ;
#36254 = CARTESIAN_POINT ( 'NONE',  ( -0.1270800023317771588, -1.767760345016116119, 0.1270800023317771588 ) ) ;
#36255 = CARTESIAN_POINT ( 'NONE',  ( 0.9873396505805591694, -0.1113553986120547346, 1.697834645669291209 ) ) ;
#36256 = CARTESIAN_POINT ( 'NONE',  ( 1.054774247047244540, -0.07405724077823318263, 1.717519684985606476 ) ) ;
#36258 = DIRECTION ( 'NONE',  ( 0.7986355100472770641, 0.000000000000000000, -0.6018150231520690285 ) ) ;
#36257 = CARTESIAN_POINT ( 'NONE',  ( -0.8070866141732283561, -0.0009842519685049383633, 0.6590551181102368705 ) ) ;
#36259 = CARTESIAN_POINT ( 'NONE',  ( 0.8019270111902716547, -0.1787899950787401604, 0.4822834645131655606 ) ) ;
#36260 = ORIENTED_EDGE ( 'NONE', *, *, #16477, .F. ) ;
#36261 = EDGE_CURVE ( 'NONE', #26896, #3387, #45576, .T. ) ;
#36262 = CARTESIAN_POINT ( 'NONE',  ( 0.1645760587280559184, -0.1627877146821092580, -0.0008175030223465492218 ) ) ;
#36264 = CARTESIAN_POINT ( 'NONE',  ( -0.1264236179284866091, -0.04970472435568527164, -0.1264236179284866091 ) ) ;
#36263 = CARTESIAN_POINT ( 'NONE',  ( -0.1113553986120547346, -0.9281496061916850726, -0.1113553986120547346 ) ) ;
#36265 = CARTESIAN_POINT ( 'NONE',  ( -0.6971942568897626646, 0.07405724077823318263, 0.3986220471903312301 ) ) ;
#36266 = CARTESIAN_POINT ( 'NONE',  ( 0.6971942568897626646, -0.07405724077823297447, 0.6348425196312760255 ) ) ;
#36267 = CARTESIAN_POINT ( 'NONE',  ( -0.1787899950787401882, -1.063484251914740275, 0.000000000000000000 ) ) ;
#36268 = CARTESIAN_POINT ( 'NONE',  ( 1.054774247047244540, 0.07405724077823318263, 0.06889763774151215492 ) ) ;
#36269 = EDGE_CURVE ( 'NONE', #12883, #10419, #14787, .T. ) ;
#36270 = CARTESIAN_POINT ( 'NONE',  ( -0.8759842519685039353, -0.1787899950787401882, 1.547736220418677089 ) ) ;
#36271 = VERTEX_POINT ( 'NONE', #16388 ) ;
#36272 = CARTESIAN_POINT ( 'NONE',  ( -1.054774247047244540, 0.07405724077823318263, 1.171259842465921741 ) ) ;
#36273 = DIRECTION ( 'NONE',  ( -0.8191520442889873577, 1.003171929053519323E-16, 0.5735764363510523767 ) ) ;
#36274 = EDGE_CURVE ( 'NONE', #44909, #6306, #17073, .T. ) ;
#36275 = CARTESIAN_POINT ( 'NONE',  ( 1.054774247047244096, 0.000000000000000000, 1.208169291284818980 ) ) ;
#36276 = CARTESIAN_POINT ( 'NONE',  ( -0.7185039370078746268, -0.06523048226347956391, 0.7308070865066471633 ) ) ;
#36277 = CARTESIAN_POINT ( 'NONE',  ( 1.054774247047244540, -0.07405724077823318263, 1.751968503883245765 ) ) ;
#36278 = CARTESIAN_POINT ( 'NONE',  ( -0.9412147342319837628, 0.1574803149606300301, 0.5684055118110235005 ) ) ;
#36279 = CARTESIAN_POINT ( 'NONE',  ( -0.7495606340400177148, -0.1264236179284866091, 0.9128937007336377363 ) ) ;
#36280 = CARTESIAN_POINT ( 'NONE',  ( -0.9412147342319837628, -0.1574803149606297803, 1.616633858267715773 ) ) ;
#36281 = DIRECTION ( 'NONE',  ( 0.000000000000000000, -0.7880107536067207930, 0.6156614753256598460 ) ) ;
#36282 = CARTESIAN_POINT ( 'NONE',  ( 0.8759842519685039353, -0.1787899950787401882, 0.3321850393163153226 ) ) ;
#36283 = CARTESIAN_POINT ( 'NONE',  ( -1.054774247047244540, 0.07405724077823318263, 0.2608267715997797387 ) ) ;
#36284 = CARTESIAN_POINT ( 'NONE',  ( -0.6971942568897626646, -0.07405724077823297447, 0.6742125983714335469 ) ) ;
#36285 = CARTESIAN_POINT ( 'NONE',  ( 0.8759842519685039353, -0.1574803149606299191, 1.564960629813732185 ) ) ;
#36286 = VERTEX_POINT ( 'NONE', #23337 ) ;
#36287 = CARTESIAN_POINT ( 'NONE',  ( -0.07405724077823318263, -0.01279527553678766298, -0.1787899950787401604 ) ) ;
#36288 = ORIENTED_EDGE ( 'NONE', *, *, #32273, .T. ) ;
#36289 = CARTESIAN_POINT ( 'NONE',  ( 1.054774247047244540, -0.07405724077823318263, 0.7332677164816707727 ) ) ;
#36290 = CARTESIAN_POINT ( 'NONE',  ( 0.7495606340400177148, -0.1264236179284866091, 1.075295275536787276 ) ) ;
#36291 = CARTESIAN_POINT ( 'NONE',  ( -1.054774247047244540, -0.07405724077823318263, 1.909448818843873186 ) ) ;
#36292 = VECTOR ( 'NONE', #11020, 39.37007874015748854 ) ;
#36293 = ORIENTED_EDGE ( 'NONE', *, *, #47402, .F. ) ;
#36294 = CARTESIAN_POINT ( 'NONE',  ( -0.7185039370078746268, -0.06523048226347956391, 0.1894685039370079815 ) ) ;
#36295 = CARTESIAN_POINT ( 'NONE',  ( 0.1264236179284866091, -1.330340503662309271, -0.1264236179284866091 ) ) ;
#36296 = CONICAL_SURFACE ( 'NONE', #14832, 0.1787899950787401049, 1.047197551196598297 ) ;
#36297 = ORIENTED_EDGE ( 'NONE', *, *, #7261, .T. ) ;
#36298 = CARTESIAN_POINT ( 'NONE',  ( 0.1264236179284866091, -0.3400590550643468601, 0.1264236179284866091 ) ) ;
#36299 = ORIENTED_EDGE ( 'NONE', *, *, #4702, .F. ) ;
#36300 = CARTESIAN_POINT ( 'NONE',  ( 0.6971942568897637749, 2.189545951927499583E-17, 1.222933070812378009 ) ) ;
#36301 = CARTESIAN_POINT ( 'NONE',  ( 0.0003553830333943102347, -0.1260611533335281031, -0.05724849586115477590 ) ) ;
#36302 = EDGE_CURVE ( 'NONE', #36580, #5319, #16616, .T. ) ;
#36303 = CARTESIAN_POINT ( 'NONE',  ( -0.2471922891335203709, -0.07779967023288102135, 0.07764737426212238447 ) ) ;
#36304 = CARTESIAN_POINT ( 'NONE',  ( 0.8759842519685039353, -0.1574803149606299191, 1.968503937007874072 ) ) ;
#36305 = CARTESIAN_POINT ( 'NONE',  ( 0.1787899950787401882, -1.639271653489543290, -2.189545951927503898E-17 ) ) ;
#36306 = CARTESIAN_POINT ( 'NONE',  ( -0.1264236179284866091, -0.7977362204186770889, -0.1264236179284866091 ) ) ;
#36307 = CARTESIAN_POINT ( 'NONE',  ( -0.8019270111902716547, 0.1787899950787401604, 0.5118110235682844511 ) ) ;
#36308 = DIRECTION ( 'NONE',  ( 0.5735764363510447161, -0.8191520442889925757, 1.003171929053525486E-16 ) ) ;
#36309 = CARTESIAN_POINT ( 'NONE',  ( 0.1797182628040039087, -1.317465069425564295, -0.07444174185955065859 ) ) ;
#36310 = CARTESIAN_POINT ( 'NONE',  ( 1.033464566929133799, 0.000000000000000000, 1.427165354330708569 ) ) ;
#36311 = CARTESIAN_POINT ( 'NONE',  ( 1.054774247047244540, 0.07405724077823318263, 1.289370078686393750 ) ) ;
#36312 = CARTESIAN_POINT ( 'NONE',  ( 1.002407869896990045, 0.1264236179284866091, 1.719980314906866203 ) ) ;
#36313 = EDGE_CURVE ( 'NONE', #40174, #38091, #34589, .T. ) ;
#36314 = CARTESIAN_POINT ( 'NONE',  ( 0.9873396505805591694, 0.1113553986120547346, 0.01476377952755905665 ) ) ;
#36316 = CARTESIAN_POINT ( 'NONE',  ( -0.7633311516264269514, 0.1159584800571472618, 1.980764034584741706 ) ) ;
#36315 = LINE ( 'NONE', #10435, #45827 ) ;
#36317 = DIRECTION ( 'NONE',  ( 0.000000000000000000, 0.8660254037844384856, -0.5000000000000003331 ) ) ;
#36318 = CARTESIAN_POINT ( 'NONE',  ( -0.9873396505805591694, 0.1113553986120547346, 1.658464566821606256 ) ) ;
#36319 = CARTESIAN_POINT ( 'NONE',  ( 0.9500414927467378812, -0.1787899950787401604, 0.09350393695411057804 ) ) ;
#36320 = EDGE_CURVE ( 'NONE', #39036, #1915, #21483, .T. ) ;
#36321 = CARTESIAN_POINT ( 'NONE',  ( 0.7027381063308457687, 0.03433744138758834663, 0.03937047675465409763 ) ) ;
#36323 = CARTESIAN_POINT ( 'NONE',  ( -0.8107537697050254399, -0.1574803149606297803, 0.5388779526483779003 ) ) ;
#36322 = CARTESIAN_POINT ( 'NONE',  ( 0.8019270111902716547, -0.1787899950787401604, 1.190944881836001112 ) ) ;
#36324 = CARTESIAN_POINT ( 'NONE',  ( -0.8759842519685039353, -0.1574803149606299191, 1.919291338475149544 ) ) ;
#36325 = CARTESIAN_POINT ( 'NONE',  ( -0.9500414927467378812, -0.1787899950787401604, 1.195866141678520345 ) ) ;
#36326 = CARTESIAN_POINT ( 'NONE',  ( 1.033464566929134687, 0.06523048226347956391, 0.4749015746956221085 ) ) ;
#36327 = ORIENTED_EDGE ( 'NONE', *, *, #23644, .T. ) ;
#36328 = AXIS2_PLACEMENT_3D ( 'NONE', #29731, #29019, #44273 ) ;
#36329 = ADVANCED_FACE ( 'NONE', ( #32182 ), #20889, .T. ) ;
#36330 = CARTESIAN_POINT ( 'NONE',  ( 0.9213771321876901288, 0.1657552102673074401, 0.03937007882159332395 ) ) ;
#36331 = CARTESIAN_POINT ( 'NONE',  ( -1.033464566929133799, 0.000000000000000000, 0.3937007872940480047 ) ) ;
#36332 = ORIENTED_EDGE ( 'NONE', *, *, #13087, .F. ) ;
#36333 = CARTESIAN_POINT ( 'NONE',  ( 1.054774247047244540, 0.07405724077823318263, 1.481299212544662680 ) ) ;
#36334 = EDGE_CURVE ( 'NONE', #13902, #28460, #32431, .T. ) ;
#36336 = CARTESIAN_POINT ( 'NONE',  ( 0.8759842519685039353, 0.000000000000000000, 4.498031496062992574 ) ) ;
#36335 = CARTESIAN_POINT ( 'NONE',  ( -1.033464566929134687, 0.06523048226347956391, 0.09104330708661413640 ) ) ;
#36337 = CARTESIAN_POINT ( 'NONE',  ( -0.1787899950787401882, -0.0004921259304884630223, 0.000000000000000000 ) ) ;
#36338 = VERTEX_POINT ( 'NONE', #17311 ) ;
#36339 = CARTESIAN_POINT ( 'NONE',  ( -1.181162989532618060E-16, -0.0009842519685041700977, -0.3937007874015748254 ) ) ;
#36340 = EDGE_LOOP ( 'NONE', ( #35392, #20977, #19038, #28398 ) ) ;
#36341 = PLANE ( 'NONE',  #31384 ) ;
#36342 = SURFACE_STYLE_USAGE ( .BOTH. , #43973 ) ;
#36343 = CARTESIAN_POINT ( 'NONE',  ( 0.8019270111902717657, 0.1787899950787401604, 0.5118110235682844511 ) ) ;
#36344 = ORIENTED_EDGE ( 'NONE', *, *, #10580, .T. ) ;
#36345 = CARTESIAN_POINT ( 'NONE',  ( -0.6971942568897648851, -0.07405724077823297447, 1.500984251914741829 ) ) ;
#36346 = CARTESIAN_POINT ( 'NONE',  ( 0.1574803149606299191, 0.08070866152484981737, -1.928577636452523993E-17 ) ) ;
#36347 = CARTESIAN_POINT ( 'NONE',  ( -0.6971942568897637749, 2.189545951927499583E-17, 1.188484251914740275 ) ) ;
#36348 = CARTESIAN_POINT ( 'NONE',  ( -0.7185039370078739607, 1.928577636452523993E-17, 0.1082677165354330728 ) ) ;
#36349 = ORIENTED_EDGE ( 'NONE', *, *, #9712, .F. ) ;
#36350 = CARTESIAN_POINT ( 'NONE',  ( -0.6971942568897648851, 0.07405724077823318263, 1.023622047190330342 ) ) ;
#36351 = CARTESIAN_POINT ( 'NONE',  ( -0.8019270111902717657, -0.1787899950787401604, 0.8415354330171019859 ) ) ;
#36352 = CARTESIAN_POINT ( 'NONE',  ( -1.054774247047244096, 0.000000000000000000, 0.1845472440407248116 ) ) ;
#36353 = LINE ( 'NONE', #28454, #6524 ) ;
#36354 = AXIS2_PLACEMENT_3D ( 'NONE', #22520, #22278, #18682 ) ;
#36355 = FACE_OUTER_BOUND ( 'NONE', #15328, .T. ) ;
#36356 = CARTESIAN_POINT ( 'NONE',  ( -1.094772975963752103E-17, -0.8529782989378996705, -0.1787899950787401882 ) ) ;
#36357 = CARTESIAN_POINT ( 'NONE',  ( 0.01517891734636545205, -0.08956197014793249034, 0.1509071277318320969 ) ) ;
#36358 = CARTESIAN_POINT ( 'NONE',  ( -0.1264236179284866091, 0.1126968504474643862, -0.1264236179284866091 ) ) ;
#36359 = ORIENTED_EDGE ( 'NONE', *, *, #20013, .T. ) ;
#36360 = AXIS2_PLACEMENT_3D ( 'NONE', #17054, #9874, #28099 ) ;
#36361 = CIRCLE ( 'NONE', #1118, 0.02900000000000052189 ) ;
#36362 = ORIENTED_EDGE ( 'NONE', *, *, #13121, .F. ) ;
#36363 = CARTESIAN_POINT ( 'NONE',  ( 0.8107537697050254399, 0.1574803149606300301, 0.7701771653543307838 ) ) ;
#36364 = DIRECTION ( 'NONE',  ( 0.000000000000000000, -1.000000000000000000, 0.000000000000000000 ) ) ;
#36365 = CARTESIAN_POINT ( 'NONE',  ( -0.8759842519685039353, -0.1787899950787401882, 0.7603346456155274380 ) ) ;
#36366 = VERTEX_POINT ( 'NONE', #42681 ) ;
#36367 = CARTESIAN_POINT ( 'NONE',  ( -1.002407869896990045, 0.1264236179284866091, 1.843011810969858333 ) ) ;
#36368 = CARTESIAN_POINT ( 'NONE',  ( 0.7646288533564489232, -0.1113553986120547346, 0.7037401574803149318 ) ) ;
#36369 = CARTESIAN_POINT ( 'NONE',  ( -0.1270800023317771588, -0.7835083765121790833, 0.1270800023317771588 ) ) ;
#36370 = CARTESIAN_POINT ( 'NONE',  ( 0.06594017991656314637, -0.2574235754679920496, -0.3092881115733853714 ) ) ;
#36371 = CARTESIAN_POINT ( 'NONE',  ( -1.033464566929133799, 0.000000000000000000, 1.338582677057826853 ) ) ;
#36372 = CARTESIAN_POINT ( 'NONE',  ( 0.6971942568897626646, -0.07405724077823297447, 0.7972440944344250102 ) ) ;
#36373 = CARTESIAN_POINT ( 'NONE',  ( -0.06523048226347956391, -0.5861220472440943352, -0.1574803149606300301 ) ) ;
#36374 = CARTESIAN_POINT ( 'NONE',  ( -0.01694847244370521061, 0.1204840602458819576, -0.1578856350490314697 ) ) ;
#36375 = ORIENTED_EDGE ( 'NONE', *, *, #20826, .T. ) ;
#36376 = CARTESIAN_POINT ( 'NONE',  ( 1.033464566929133799, 0.000000000000000000, 1.574803149498771537 ) ) ;
#36377 = CARTESIAN_POINT ( 'NONE',  ( 1.033464566929134687, 0.06523048226347956391, 1.232775590551179912 ) ) ;
#36379 = DIRECTION ( 'NONE',  ( 0.000000000000000000, 0.000000000000000000, 1.000000000000000000 ) ) ;
#36378 = CARTESIAN_POINT ( 'NONE',  ( 0.8528693833544092051, -0.1722797369867551665, 1.987786336861242287 ) ) ;
#36380 = DIRECTION ( 'NONE',  ( 1.000000000000000000, 0.000000000000000000, -1.822029033848725275E-16 ) ) ;
#36381 = ( BOUNDED_CURVE ( )  B_SPLINE_CURVE ( 2, ( #9827, #38811, #35463, #27832, #31645, #9590, #24211, #38578, #21054 ),
 .UNSPECIFIED., .F., .T. ) 
 B_SPLINE_CURVE_WITH_KNOTS ( ( 3, 2, 2, 2, 3 ),
 ( 0.07499999999999999722, 0.07749999999999999944, 0.08000000000000000167, 0.08250000000000000389, 0.08500000000000000611 ),
 .UNSPECIFIED. ) 
 CURVE ( )  GEOMETRIC_REPRESENTATION_ITEM ( )  RATIONAL_B_SPLINE_CURVE ( ( 1.000000000000000000, 0.9238795325112869605, 1.000000000000000000, 0.9238795325112869605, 1.000000000000000000, 0.9238795325112869605, 1.000000000000000000, 0.9238795325112869605, 1.000000000000000000 ) ) 
 REPRESENTATION_ITEM ( '' )  ) ;
#36382 = EDGE_CURVE ( 'NONE', #41308, #22445, #9894, .T. ) ;
#36384 = CYLINDRICAL_SURFACE ( 'NONE', #22334, 0.1574803149606299191 ) ;
#36383 = CARTESIAN_POINT ( 'NONE',  ( 1.054774247047244540, -0.07405724077823318263, 0.6102362204186774219 ) ) ;
#36385 = CIRCLE ( 'NONE', #37147, 0.2952755905511810774 ) ;
#36387 = ( BOUNDED_CURVE ( )  B_SPLINE_CURVE ( 2, ( #37023, #22154, #15000, #33225, #29651, #26009, #7780, #22395, #4174 ),
 .UNSPECIFIED., .F., .T. ) 
 B_SPLINE_CURVE_WITH_KNOTS ( ( 3, 2, 2, 2, 3 ),
 ( 0.8000000000000000444, 0.8024999999999999911, 0.8050000000000000488, 0.8074999999999999956, 0.8100000000000000533 ),
 .UNSPECIFIED. ) 
 CURVE ( )  GEOMETRIC_REPRESENTATION_ITEM ( )  RATIONAL_B_SPLINE_CURVE ( ( 1.000000000000000000, 0.9238795325112869605, 1.000000000000000000, 0.9238795325112869605, 1.000000000000000000, 0.9238795325112869605, 1.000000000000000000, 0.9238795325112869605, 1.000000000000000000 ) ) 
 REPRESENTATION_ITEM ( '' )  ) ;
#36386 = CARTESIAN_POINT ( 'NONE',  ( -0.1574803149606299191, -0.9875035750853327077, -1.463737590216208861 ) ) ;
#36388 = ORIENTED_EDGE ( 'NONE', *, *, #18537, .T. ) ;
#36389 = CARTESIAN_POINT ( 'NONE',  ( -0.8759842519685039353, 0.1574803149606299191, 1.161417322834645605 ) ) ;
#36390 = AXIS2_PLACEMENT_3D ( 'NONE', #30657, #45690, #23450 ) ;
#36391 = FACE_OUTER_BOUND ( 'NONE', #33570, .T. ) ;
#36392 = CARTESIAN_POINT ( 'NONE',  ( 0.8759842519685039353, 0.1787899950787401882, 1.016240157426551161 ) ) ;
#36393 = ADVANCED_FACE ( 'NONE', ( #21134 ), #42920, .T. ) ;
#36394 = CARTESIAN_POINT ( 'NONE',  ( 0.7185039370078739607, 1.928577636452523993E-17, 1.604330708661417360 ) ) ;
#36395 = CARTESIAN_POINT ( 'NONE',  ( 3.284318927891251994E-17, -1.255413385773007873, 0.1787899950787401882 ) ) ;
#36396 = CARTESIAN_POINT ( 'NONE',  ( 0.06523048226347956391, -1.471948818897638178, 0.1574803149606297803 ) ) ;
#36397 = DIRECTION ( 'NONE',  ( 0.000000000000000000, 0.000000000000000000, 1.000000000000000000 ) ) ;
#36398 = CARTESIAN_POINT ( 'NONE',  ( -0.8759842519685039353, -0.1787899950787401882, 0.1697834645131655606 ) ) ;
#36399 = CARTESIAN_POINT ( 'NONE',  ( -0.6971942568897648851, 0.07405724077823318263, 1.934055118056471567 ) ) ;
#36400 = CARTESIAN_POINT ( 'NONE',  ( -0.6971942568897648851, -0.07405724077823297447, 1.737204724355685848 ) ) ;
#36401 = CARTESIAN_POINT ( 'NONE',  ( -0.8759842519685039353, 0.1787899950787401882, 1.055610236166708793 ) ) ;
#36402 = CARTESIAN_POINT ( 'NONE',  ( -0.9500414927467378812, 0.1787899950787401604, 0.4281496062454490659 ) ) ;
#36403 = CARTESIAN_POINT ( 'NONE',  ( -0.2471922904502826535, 0.06774690380565037695, 0.09545378441109995948 ) ) ;
#36404 = CARTESIAN_POINT ( 'NONE',  ( 0.1592646090380165913, 0.04727201993825761589, 0.1404638620642217617 ) ) ;
#36405 = CARTESIAN_POINT ( 'NONE',  ( -1.033464566929133799, 0.000000000000000000, 1.899606299212598604 ) ) ;
#36406 = DIRECTION ( 'NONE',  ( -1.000000000000000000, 3.469446951953626022E-15, 0.000000000000000000 ) ) ;
#36407 = CARTESIAN_POINT ( 'NONE',  ( -0.1787899950787401882, -0.4494349918512858255, 0.000000000000000000 ) ) ;
#36408 = CARTESIAN_POINT ( 'NONE',  ( 0.05546883683243283847, -0.09842519685039370636, 0.1418485093170885891 ) ) ;
#36409 = LINE ( 'NONE', #3566, #44011 ) ;
#36410 = CARTESIAN_POINT ( 'NONE',  ( 0.4736248074375795647, 1.690605217543005745, -0.5092277576975118292 ) ) ;
#36411 = CARTESIAN_POINT ( 'NONE',  ( -1.054774247047244540, -0.07405724077823318263, 0.2952755904974176393 ) ) ;
#36412 = ORIENTED_EDGE ( 'NONE', *, *, #27851, .T. ) ;
#36413 = CARTESIAN_POINT ( 'NONE',  ( -0.6971942568897637749, 2.189545951927499583E-17, 1.306594488135212728 ) ) ;
#36414 = ORIENTED_EDGE ( 'NONE', *, *, #3693, .F. ) ;
#36415 = AXIS2_PLACEMENT_3D ( 'NONE', #10229, #32524, #43749 ) ;
#36416 = CARTESIAN_POINT ( 'NONE',  ( -0.1787899950787401882, -1.107775590497417362, 0.000000000000000000 ) ) ;
#36417 = CARTESIAN_POINT ( 'NONE',  ( -0.1264236179284866091, -1.373523621993480326, 0.1264236179284866091 ) ) ;
#36418 = CARTESIAN_POINT ( 'NONE',  ( 0.3246033735368759610, 4.766607801171850497E-17, 0.000000000000000000 ) ) ;
#36419 = CARTESIAN_POINT ( 'NONE',  ( 0.8759842519685039353, -0.1574803149606299191, 0.3543307086614173040 ) ) ;
#36420 = CARTESIAN_POINT ( 'NONE',  ( 0.1270800023317771588, -0.5768154631263527898, 0.1270800023317771588 ) ) ;
#36421 = CARTESIAN_POINT ( 'NONE',  ( 0.1574803149606300023, 1.117014023967195735, -3.442880580079816788 ) ) ;
#36422 = CARTESIAN_POINT ( 'NONE',  ( -0.7185039370078739607, 1.928577636452523993E-17, 0.9251968502861732668 ) ) ;
#36423 = CARTESIAN_POINT ( 'NONE',  ( 0.8759842519685039353, 0.1787899950787401882, 0.4306102361667086820 ) ) ;
#36424 = CARTESIAN_POINT ( 'NONE',  ( 0.1113553986120547346, -0.1210629921259842590, -0.1113553986120547346 ) ) ;
#36425 = ORIENTED_EDGE ( 'NONE', *, *, #21041, .F. ) ;
#36426 = CARTESIAN_POINT ( 'NONE',  ( 0.7646288533564489232, -0.1113553986120547346, 1.796259842412157415 ) ) ;
#36427 = ORIENTED_EDGE ( 'NONE', *, *, #554, .T. ) ;
#36428 = CARTESIAN_POINT ( 'NONE',  ( 0.9873396505805591694, -0.1113553986120547346, 0.2312992124908980207 ) ) ;
#36429 = CARTESIAN_POINT ( 'NONE',  ( 0.9873396505805591694, 0.1113553986120547346, 0.7627952755905511584 ) ) ;
#36430 = CARTESIAN_POINT ( 'NONE',  ( -0.8759842519685039353, 0.1574803149606299191, 1.082677165354330784 ) ) ;
#36431 = EDGE_CURVE ( 'NONE', #47229, #2766, #29527, .T. ) ;
#36432 = FACE_OUTER_BOUND ( 'NONE', #23102, .T. ) ;
#36433 = CARTESIAN_POINT ( 'NONE',  ( 0.8759842519685039353, 0.1574803149606299191, 0.2066929132782996115 ) ) ;
#36434 = ORIENTED_EDGE ( 'NONE', *, *, #554, .F. ) ;
#36436 = CARTESIAN_POINT ( 'NONE',  ( 0.07405724077823318263, -0.02755905506434671789, 0.1787899950787401604 ) ) ;
#36435 = AXIS2_PLACEMENT_3D ( 'NONE', #21506, #43065, #47156 ) ;
#36437 = EDGE_CURVE ( 'NONE', #17013, #25548, #24980, .T. ) ;
#36438 = ORIENTED_EDGE ( 'NONE', *, *, #45043, .T. ) ;
#36439 = CARTESIAN_POINT ( 'NONE',  ( 1.614954907737318939E-16, -8.878505979408855953E-16, 0.3937007874015748254 ) ) ;
#36440 = CARTESIAN_POINT ( 'NONE',  ( 0.1264236179284866091, -1.629429133804503937, -0.1264236179284866091 ) ) ;
#36441 = CARTESIAN_POINT ( 'NONE',  ( 2.892866454678787531E-17, -1.582677165246803019, 0.1574803149606299191 ) ) ;
#36442 = CARTESIAN_POINT ( 'NONE',  ( -0.1787899950787401604, -0.7116141731745821986, 0.07405724077823318263 ) ) ;
#36443 = CARTESIAN_POINT ( 'NONE',  ( -1.033464566929134687, 0.06523048226347956391, 0.1599409447743626866 ) ) ;
#36444 = CARTESIAN_POINT ( 'NONE',  ( -0.1113553986120547346, -1.006889763779527547, 0.1113553986120547346 ) ) ;
#36445 = CARTESIAN_POINT ( 'NONE',  ( 0.9873396505805591694, 0.1113553986120547346, 0.9891732282389291697 ) ) ;
#36446 = DIRECTION ( 'NONE',  ( 0.000000000000000000, -0.6156614753256628436, -0.7880107536067184615 ) ) ;
#36447 = ORIENTED_EDGE ( 'NONE', *, *, #18770, .F. ) ;
#36448 = ORIENTED_EDGE ( 'NONE', *, *, #35592, .T. ) ;
#36449 = CARTESIAN_POINT ( 'NONE',  ( -1.054774247047244540, 0.07405724077823318263, 1.564960629867495845 ) ) ;
#36450 = ORIENTED_EDGE ( 'NONE', *, *, #32438, .F. ) ;
#36451 = CARTESIAN_POINT ( 'NONE',  ( 0.8759842519685039353, -0.1787899950787401882, 1.552657480261196765 ) ) ;
#36452 = CARTESIAN_POINT ( 'NONE',  ( -0.8019270111902717657, 0.1787899950787401604, 0.7874015747493863238 ) ) ;
#36453 = CARTESIAN_POINT ( 'NONE',  ( -0.4338976377952755703, -0.2559055118110236116, 0.000000000000000000 ) ) ;
#36454 = CARTESIAN_POINT ( 'NONE',  ( 1.002407869896990045, -0.1264236179284866091, 0.7308070865604093802 ) ) ;
#36455 = CARTESIAN_POINT ( 'NONE',  ( -0.7495606340400177148, -0.1264236179284866091, 0.6766732282926929409 ) ) ;
#36456 = CARTESIAN_POINT ( 'NONE',  ( 0.01230737760510393873, -0.07955613945526318620, 0.1377952755905511861 ) ) ;
#36457 = CARTESIAN_POINT ( 'NONE',  ( -1.002407869896990045, 0.1264236179284866091, 1.646161417269070837 ) ) ;
#36458 = CARTESIAN_POINT ( 'NONE',  ( -0.8107537697050253289, -0.1574803149606297803, 1.956200787294048338 ) ) ;
#36459 = EDGE_LOOP ( 'NONE', ( #11407, #2090, #3503, #30198 ) ) ;
#36460 = CARTESIAN_POINT ( 'NONE',  ( 0.7185039370078760701, -0.06523048226348075740, 0.9670275589475921807 ) ) ;
#36461 = CARTESIAN_POINT ( 'NONE',  ( 0.9500414927467377701, 0.1787899950787401604, 1.491141732229701145 ) ) ;
#36462 = CARTESIAN_POINT ( 'NONE',  ( 0.09178263254600295407, -0.09851384182930648936, -0.1728663888072523580 ) ) ;
#36463 = CARTESIAN_POINT ( 'NONE',  ( -0.8107537697050254399, 0.1574803149606300301, 0.3666338581601893964 ) ) ;
#36464 = VERTEX_POINT ( 'NONE', #3404 ) ;
#36465 = EDGE_CURVE ( 'NONE', #10105, #38268, #10615, .T. ) ;
#36466 = CARTESIAN_POINT ( 'NONE',  ( -0.1787899950787401604, -1.667446802874908096, 0.07405724077823318263 ) ) ;
#36467 = ORIENTED_EDGE ( 'NONE', *, *, #41740, .F. ) ;
#36468 = ( NAMED_UNIT ( * ) PLANE_ANGLE_UNIT ( ) SI_UNIT ( $, .RADIAN. ) ) ;
#36469 = ORIENTED_EDGE ( 'NONE', *, *, #43149, .F. ) ;
#36470 = DIRECTION ( 'NONE',  ( 1.000000000000000000, -3.469446951953613794E-15, -1.144917494144692682E-16 ) ) ;
#36471 = CARTESIAN_POINT ( 'NONE',  ( 3.284318927891251994E-17, -0.8567913385289133155, 0.1787899950787401882 ) ) ;
#36472 = FACE_OUTER_BOUND ( 'NONE', #16928, .T. ) ;
#36473 = LENGTH_MEASURE_WITH_UNIT ( LENGTH_MEASURE( 0.02539999999999999897 ), #40032 ) ;
#36474 = CARTESIAN_POINT ( 'NONE',  ( 0.9500414927467378812, 0.1787899950787401604, 1.761811023568284007 ) ) ;
#36475 = CARTESIAN_POINT ( 'NONE',  ( 0.6971942568897626646, 0.07405724077823318263, 0.3543307086076538659 ) ) ;
#36476 = CARTESIAN_POINT ( 'NONE',  ( 0.7646288533564489232, 0.1113553986120547346, 0.3001968503937008093 ) ) ;
#36477 = CARTESIAN_POINT ( 'NONE',  ( 0.1270800023317771588, -0.1339020772995811182, -0.1270800023317771588 ) ) ;
#36478 = CARTESIAN_POINT ( 'NONE',  ( -0.1264236179284866091, -0.06065546429223091229, -0.1264236179284866091 ) ) ;
#36479 = CARTESIAN_POINT ( 'NONE',  ( 0.1264236179284866091, -0.3006889763241893943, 0.1264236179284866091 ) ) ;
#36480 = CARTESIAN_POINT ( 'NONE',  ( 0.1264236179284866091, -0.09891732278088229136, -0.1264236179284866091 ) ) ;
#36481 = DIRECTION ( 'NONE',  ( 0.000000000000000000, 0.000000000000000000, 1.000000000000000000 ) ) ;
#36482 = CARTESIAN_POINT ( 'NONE',  ( 1.054774247047244540, 0.07405724077823318263, 0.6545275590013545086 ) ) ;
#36483 = ( BOUNDED_CURVE ( )  B_SPLINE_CURVE ( 2, ( #32955, #13379, #14488, #43703, #13156, #42572, #38534, #21677, #6160 ),
 .UNSPECIFIED., .F., .T. ) 
 B_SPLINE_CURVE_WITH_KNOTS ( ( 3, 2, 2, 2, 3 ),
 ( 0.3200000000000000067, 0.3225000000000000089, 0.3250000000000000111, 0.3275000000000000133, 0.3300000000000000155 ),
 .UNSPECIFIED. ) 
 CURVE ( )  GEOMETRIC_REPRESENTATION_ITEM ( )  RATIONAL_B_SPLINE_CURVE ( ( 1.000000000000000000, 0.9238795325112869605, 1.000000000000000000, 0.9238795325112869605, 1.000000000000000000, 0.9238795325112869605, 1.000000000000000000, 0.9238795325112869605, 1.000000000000000000 ) ) 
 REPRESENTATION_ITEM ( '' )  ) ;
#36484 = ADVANCED_FACE ( 'NONE', ( #17545 ), #5529, .T. ) ;
#36485 = CARTESIAN_POINT ( 'NONE',  ( 0.8759842519685039353, 0.1574803149606299191, 1.122047244094488194 ) ) ;
#36486 = DIRECTION ( 'NONE',  ( -0.000000000000000000, 1.000000000000000000, -0.000000000000000000 ) ) ;
#36487 = DIRECTION ( 'NONE',  ( 0.000000000000000000, 0.000000000000000000, -1.000000000000000000 ) ) ;
#36488 = CARTESIAN_POINT ( 'NONE',  ( 0.6971942568897648851, -0.07405724077823297447, 1.702755905458047003 ) ) ;
#36490 = CARTESIAN_POINT ( 'NONE',  ( -0.2559055118110236116, -4.908314874579054539E-16, -0.02740704184215039460 ) ) ;
#36489 = CARTESIAN_POINT ( 'NONE',  ( 0.04485236092672649499, -0.5708661417322835607, 1.206847064312616125 ) ) ;
#36491 = EDGE_CURVE ( 'NONE', #18854, #35809, #36000, .T. ) ;
#36492 = DIRECTION ( 'NONE',  ( 0.000000000000000000, 0.000000000000000000, 1.000000000000000000 ) ) ;
#36493 = CARTESIAN_POINT ( 'NONE',  ( 0.1787899950787401604, -0.2588582676627719792, -0.07405724077823318263 ) ) ;
#36494 = CARTESIAN_POINT ( 'NONE',  ( 0.7185039370078739607, 1.928577636452523993E-17, 0.4921259841444416971 ) ) ;
#36495 = CARTESIAN_POINT ( 'NONE',  ( 0.07405724077823318263, -1.051181102308440529, 0.1787899950787401604 ) ) ;
#36496 = CARTESIAN_POINT ( 'NONE',  ( 1.002407869896990045, 0.1264236179284866091, 0.07135826766277185429 ) ) ;
#36497 = CARTESIAN_POINT ( 'NONE',  ( 0.1630380177252895857, 0.08011815157765787843, -0.1387688440578072890 ) ) ;
#36498 = EDGE_CURVE ( 'NONE', #21060, #7011, #9883, .T. ) ;
#36499 = CARTESIAN_POINT ( 'NONE',  ( -1.002407869896990045, -0.1264236179284866091, 1.592027559001354398 ) ) ;
#36500 = ORIENTED_EDGE ( 'NONE', *, *, #4790, .F. ) ;
#36501 = CARTESIAN_POINT ( 'NONE',  ( -0.9500414927467378812, -0.1787899950787401604, 1.200787401521039355 ) ) ;
#36502 = CARTESIAN_POINT ( 'NONE',  ( 0.9412147342319837628, -0.1574803149606297803, 1.026082677165353729 ) ) ;
#36503 = CARTESIAN_POINT ( 'NONE',  ( 0.8019270111902717657, 0.1787899950787401604, 1.102362204670646495 ) ) ;
#36504 = CARTESIAN_POINT ( 'NONE',  ( 0.8019270111902717657, -0.1787899950787401604, 1.860236220418677089 ) ) ;
#36505 = CARTESIAN_POINT ( 'NONE',  ( -0.7646288533564489232, -0.1113553986120547346, 0.5462598425196850682 ) ) ;
#36506 = CARTESIAN_POINT ( 'NONE',  ( -1.054774247047244096, 0.000000000000000000, 1.045767716481669440 ) ) ;
#36507 = CARTESIAN_POINT ( 'NONE',  ( 0.1631207519397802896, 0.08463291909039739880, -0.1344936127549162252 ) ) ;
#36508 = CARTESIAN_POINT ( 'NONE',  ( -0.1623289600446945202, -0.2017735634833314473, -0.03395687952546246058 ) ) ;
#36509 = CARTESIAN_POINT ( 'NONE',  ( 0.8759842519685039353, 0.1787899950787401882, 0.2731299212060791515 ) ) ;
#36510 = CARTESIAN_POINT ( 'NONE',  ( -1.054774247047244096, 0.000000000000000000, 0.2977362204186775885 ) ) ;
#36511 = CARTESIAN_POINT ( 'NONE',  ( -1.054774247047244540, -0.07405724077823318263, 0.6889763778989935750 ) ) ;
#36512 = CARTESIAN_POINT ( 'NONE',  ( 0.9412147342319837628, -0.1574803149606297803, 1.685531495955465697 ) ) ;
#36513 = ORIENTED_EDGE ( 'NONE', *, *, #6936, .F. ) ;
#36514 = ( BOUNDED_CURVE ( )  B_SPLINE_CURVE ( 2, ( #5501, #12486, #24202, #13188, #34761, #37871, #35229, #8864, #42137 ),
 .UNSPECIFIED., .F., .T. ) 
 B_SPLINE_CURVE_WITH_KNOTS ( ( 3, 2, 2, 2, 3 ),
 ( 0.2800000000000000266, 0.2824999999999999734, 0.2849999999999999756, 0.2874999999999999778, 0.2899999999999999800 ),
 .UNSPECIFIED. ) 
 CURVE ( )  GEOMETRIC_REPRESENTATION_ITEM ( )  RATIONAL_B_SPLINE_CURVE ( ( 1.000000000000000000, 0.9238795325112869605, 1.000000000000000000, 0.9238795325112869605, 1.000000000000000000, 0.9238795325112869605, 1.000000000000000000, 0.9238795325112869605, 1.000000000000000000 ) ) 
 REPRESENTATION_ITEM ( '' )  ) ;
#36515 = CARTESIAN_POINT ( 'NONE',  ( 0.1264236179284866091, 0.009350393754550925460, 0.1264236179284866091 ) ) ;
#36516 = CARTESIAN_POINT ( 'NONE',  ( 0.9500414927467378812, 0.1787899950787401604, 0.7431102361667091261 ) ) ;
#36517 = CARTESIAN_POINT ( 'NONE',  ( 0.8019270111902716547, -0.1787899950787401604, 0.9990157479777320715 ) ) ;
#36518 = CARTESIAN_POINT ( 'NONE',  ( -0.8019270111902716547, 0.1787899950787401604, 1.884842519631275026 ) ) ;
#36519 = CARTESIAN_POINT ( 'NONE',  ( 1.054774247047244540, 0.07405724077823318263, 1.874999999946236784 ) ) ;
#36520 = EDGE_LOOP ( 'NONE', ( #14745, #30064, #1010, #16008 ) ) ;
#36521 = CARTESIAN_POINT ( 'NONE',  ( 0.7185039370078739607, 1.928577636452523993E-17, 1.328740157480315043 ) ) ;
#36522 = CARTESIAN_POINT ( 'NONE',  ( 0.1264236179284866091, -1.222072787126875948, 0.1264236179284866091 ) ) ;
#36523 = VERTEX_POINT ( 'NONE', #493 ) ;
#36524 = CARTESIAN_POINT ( 'NONE',  ( 0.1787899950787401604, -0.2145669290800947537, -0.07405724077823318263 ) ) ;
#36525 = CARTESIAN_POINT ( 'NONE',  ( -0.7185039370078692977, 0.06523048226347515077, 1.710137795168064079 ) ) ;
#36526 = ORIENTED_EDGE ( 'NONE', *, *, #315, .F. ) ;
#36527 = CARTESIAN_POINT ( 'NONE',  ( 0.7495606340400177148, 0.1264236179284866091, 1.139271653489543290 ) ) ;
#36528 = CARTESIAN_POINT ( 'NONE',  ( 0.002317115957654733525, -0.1361028492805151369, -0.03985382897137078329 ) ) ;
#36529 = DIRECTION ( 'NONE',  ( -1.000000000000000000, 0.000000000000000000, 0.000000000000000000 ) ) ;
#36530 = AXIS2_PLACEMENT_3D ( 'NONE', #44768, #8598, #30448 ) ;
#36531 = CARTESIAN_POINT ( 'NONE',  ( 0.9412147342319837628, -0.1574803149606297803, 1.970964566929134021 ) ) ;
#36532 = ADVANCED_FACE ( 'NONE', ( #14671 ), #25706, .F. ) ;
#36533 = CARTESIAN_POINT ( 'NONE',  ( 0.1264236179284866091, -1.683562992072220599, 0.1264236179284866091 ) ) ;
#36534 = CARTESIAN_POINT ( 'NONE',  ( -1.094772975963752103E-17, -1.624507873961984261, -0.1787899950787401882 ) ) ;
#36535 = CARTESIAN_POINT ( 'NONE',  ( -0.9500414927467377701, 0.1787899950787401604, 0.4675196849856070314 ) ) ;
#36536 = CYLINDRICAL_SURFACE ( 'NONE', #22427, 0.1968503937007874405 ) ;
#36537 = CARTESIAN_POINT ( 'NONE',  ( 3.301370929368692659E-17, -1.251028061551548998, 0.1797182628040039365 ) ) ;
#36538 = CARTESIAN_POINT ( 'NONE',  ( -0.01990234270466676239, 0.2840036093443637499, -0.08759220388352539910 ) ) ;
#36539 = CARTESIAN_POINT ( 'NONE',  ( 0.6971942568897648851, 0.07405724077823318263, 1.186023621993481658 ) ) ;
#36540 = CARTESIAN_POINT ( 'NONE',  ( 0.9500414927467377701, 0.1787899950787401604, 1.722440944828126153 ) ) ;
#36541 = DIRECTION ( 'NONE',  ( 1.822029033848725028E-16, 0.000000000000000000, 1.000000000000000000 ) ) ;
#36542 = CARTESIAN_POINT ( 'NONE',  ( 0.1637370781294386346, 0.08228090712086977287, 0.1377952755905510474 ) ) ;
#36543 = CARTESIAN_POINT ( 'NONE',  ( 0.1377952755905510751, 1.687505431895957647E-17, -0.02633646578327370619 ) ) ;
#36544 = DIRECTION ( 'NONE',  ( -4.275490733183370330E-15, 0.000000000000000000, 1.000000000000000000 ) ) ;
#36545 = CARTESIAN_POINT ( 'NONE',  ( 1.033464566929133799, 0.000000000000000000, 0.7480314959554645871 ) ) ;
#36546 = CARTESIAN_POINT ( 'NONE',  ( 1.054774247047244540, -0.07405724077823318263, 0.2165354330171024577 ) ) ;
#36547 = CARTESIAN_POINT ( 'NONE',  ( 0.7287427869149385451, -0.08289353061996172778, 0.03937277022166233570 ) ) ;
#36548 = DIRECTION ( 'NONE',  ( -0.000000000000000000, -0.000000000000000000, -1.000000000000000000 ) ) ;
#36549 = FACE_OUTER_BOUND ( 'NONE', #33364, .T. ) ;
#36550 = CARTESIAN_POINT ( 'NONE',  ( -0.6971942568897637749, 2.189545951927499583E-17, 1.183562992072220599 ) ) ;
#36551 = CARTESIAN_POINT ( 'NONE',  ( 0.9412147342319837628, 0.1574803149606300301, 0.6766732282389293918 ) ) ;
#36552 = ORIENTED_EDGE ( 'NONE', *, *, #30584, .F. ) ;
#36553 = CARTESIAN_POINT ( 'NONE',  ( -0.6971942568897648851, 0.07405724077823318263, 1.067913385773007651 ) ) ;
#36554 = CYLINDRICAL_SURFACE ( 'NONE', #9246, 0.1673228346456687721 ) ;
#36555 = CARTESIAN_POINT ( 'NONE',  ( 0.8518726721728578921, 0.1743242345900581913, 0.03937026678633583771 ) ) ;
#36556 = CARTESIAN_POINT ( 'NONE',  ( 0.06523048226347956391, -1.029035432963338215, 0.1574803149606297803 ) ) ;
#36557 = CARTESIAN_POINT ( 'NONE',  ( -0.7185039370078746268, 0.06523048226347956391, 0.4502952754830242266 ) ) ;
#36558 = CARTESIAN_POINT ( 'NONE',  ( 0.0003577594938017307079, 0.01348597669578762911, 0.1377974493690218849 ) ) ;
#36559 = CARTESIAN_POINT ( 'NONE',  ( 0.6971942568897648851, -0.07405724077823297447, 1.422244094434426120 ) ) ;
#36560 = FACE_OUTER_BOUND ( 'NONE', #19206, .T. ) ;
#36561 = CARTESIAN_POINT ( 'NONE',  ( -0.9500414927467377701, 0.1787899950787401604, 0.06889763774151215492 ) ) ;
#36562 = CARTESIAN_POINT ( 'NONE',  ( -0.1264236179284866091, -0.2022637794737956740, -0.1264236179284866091 ) ) ;
#36563 = ORIENTED_EDGE ( 'NONE', *, *, #18701, .T. ) ;
#36564 = VECTOR ( 'NONE', #2813, 39.37007874015748143 ) ;
#36565 = CARTESIAN_POINT ( 'NONE',  ( 0.8759842519685039353, -0.1574803149606299191, 0.6594488187901103027 ) ) ;
#36566 = DIRECTION ( 'NONE',  ( 1.000000000000000000, 0.000000000000000000, 0.000000000000000000 ) ) ;
#36567 = CARTESIAN_POINT ( 'NONE',  ( -0.1006623723854965097, 0.09658349877441903264, 0.2273156230721088411 ) ) ;
#36568 = CARTESIAN_POINT ( 'NONE',  ( 1.054774247047244540, 0.07405724077823318263, 0.6594488188438737408 ) ) ;
#36569 = VERTEX_POINT ( 'NONE', #11316 ) ;
#36570 = CARTESIAN_POINT ( 'NONE',  ( -1.054774247047244096, 0.000000000000000000, 1.439468503883244210 ) ) ;
#36571 = CARTESIAN_POINT ( 'NONE',  ( -0.1113553986120547346, 0.05610236231225141507, -0.1113553986120547346 ) ) ;
#36572 = CARTESIAN_POINT ( 'NONE',  ( -0.6971942568897637749, 2.189545951927499583E-17, 1.070374015694267600 ) ) ;
#36573 = CARTESIAN_POINT ( 'NONE',  ( -0.2559055118110235560, -0.04862481504115584441, -0.03719749321262351416 ) ) ;
#36574 = CARTESIAN_POINT ( 'NONE',  ( -0.8759842519685039353, 0.1787899950787401882, 0.8636811023084409733 ) ) ;
#36575 = CARTESIAN_POINT ( 'NONE',  ( 0.01230737760510407577, 0.1591122789105269553, -1.502406898952441074E-18 ) ) ;
#36576 = CARTESIAN_POINT ( 'NONE',  ( -1.033464566929133799, 0.000000000000000000, 1.889763779420031486 ) ) ;
#36577 = CARTESIAN_POINT ( 'NONE',  ( -0.1264236179284866091, -0.7594743619300257098, 0.1264236179284866091 ) ) ;
#36578 = VERTEX_POINT ( 'NONE', #15627 ) ;
#36579 = CARTESIAN_POINT ( 'NONE',  ( 0.7167570750452111339, 0.08279236175412563181, 0.03937007863263047164 ) ) ;
#36580 = VERTEX_POINT ( 'NONE', #40510 ) ;
#36581 = VERTEX_POINT ( 'NONE', #4096 ) ;
#36582 = EDGE_CURVE ( 'NONE', #5868, #6940, #18133, .T. ) ;
#36583 = CARTESIAN_POINT ( 'NONE',  ( -0.8107537697050254399, 0.1574803149606300301, 0.5634842518609766149 ) ) ;
#36584 = CARTESIAN_POINT ( 'NONE',  ( -1.054774247047244540, 0.07405724077823318263, 0.7726377952218265177 ) ) ;
#36585 = DIRECTION ( 'NONE',  ( 0.000000000000000000, 0.7880107536067200158, -0.6156614753256608452 ) ) ;
#36586 = EDGE_CURVE ( 'NONE', #34984, #14850, #4557, .T. ) ;
#36587 = AXIS2_PLACEMENT_3D ( 'NONE', #28906, #3701, #18082 ) ;
#36588 = MANIFOLD_SOLID_BREP ( 'Threaded Bushing', #18609 ) ;
#36589 = EDGE_CURVE ( 'NONE', #20673, #9638, #4731, .T. ) ;
#36590 = CARTESIAN_POINT ( 'NONE',  ( -1.054774247047244096, 0.000000000000000000, 1.759350393647023614 ) ) ;
#36591 = CIRCLE ( 'NONE', #42669, 0.09842519685039370636 ) ;
#36592 = CARTESIAN_POINT ( 'NONE',  ( -0.9500414927467377701, -0.1787899950787401604, 0.09842519679663024046 ) ) ;
#36593 = CARTESIAN_POINT ( 'NONE',  ( 0.9873396505805591694, 0.1113553986120547346, 0.6446850393700788162 ) ) ;
#36594 = CARTESIAN_POINT ( 'NONE',  ( 3.301370929368692659E-17, -0.7785871166696594070, 0.1797182628040039365 ) ) ;
#36595 = FACE_OUTER_BOUND ( 'NONE', #20177, .T. ) ;
#36596 = CARTESIAN_POINT ( 'NONE',  ( -0.9873396505805591694, -0.1113553986120547346, 1.491141732175936818 ) ) ;
#36597 = CARTESIAN_POINT ( 'NONE',  ( 1.054774247047244540, -0.07405724077823318263, 0.8120078739619844832 ) ) ;
#36598 = CARTESIAN_POINT ( 'NONE',  ( 0.9412147342319837628, 0.1574803149606300301, 0.1648622046168823629 ) ) ;
#36599 = CARTESIAN_POINT ( 'NONE',  ( 0.8759842519685039353, 0.1574803149606299191, 1.397637795275590511 ) ) ;
#36601 = CARTESIAN_POINT ( 'NONE',  ( 0.000000000000000000, 0.000000000000000000, 0.000000000000000000 ) ) ;
#36600 = CARTESIAN_POINT ( 'NONE',  ( 0.9315392539442560738, -0.1672740577352537228, 1.989187881297329152 ) ) ;
#36602 = CARTESIAN_POINT ( 'NONE',  ( 1.033464566929133799, 0.000000000000000000, 1.496062992018456494 ) ) ;
#36603 = VERTEX_POINT ( 'NONE', #37649 ) ;
#36605 = FACE_OUTER_BOUND ( 'NONE', #27639, .T. ) ;
#36604 = CARTESIAN_POINT ( 'NONE',  ( 0.7495606340400177148, -0.1264236179284866091, 0.7947834645131652831 ) ) ;
#36606 = CARTESIAN_POINT ( 'NONE',  ( 0.07405724077823318263, -0.6968503936470246130, 0.1787899950787401604 ) ) ;
#36607 = DIRECTION ( 'NONE',  ( 1.822029033848725028E-16, 0.000000000000000000, 1.000000000000000000 ) ) ;
#36608 = ORIENTED_EDGE ( 'NONE', *, *, #19997, .F. ) ;
#36609 = CARTESIAN_POINT ( 'NONE',  ( 0.9412147342319837628, -0.1574803149606297803, 0.6225393699712132856 ) ) ;
#36610 = LINE ( 'NONE', #18391, #2236 ) ;
#36611 = CARTESIAN_POINT ( 'NONE',  ( 1.054774247047244540, 0.07405724077823318263, 0.9694881889226144578 ) ) ;
#36612 = LINE ( 'NONE', #3771, #32619 ) ;
#36613 = CARTESIAN_POINT ( 'NONE',  ( 0.1113553986120547346, -1.538385826771653475, -0.1113553986120547346 ) ) ;
#36614 = LINE ( 'NONE', #21511, #47456 ) ;
#36615 = CIRCLE ( 'NONE', #10598, 0.2362204724409449064 ) ;
#36616 = VERTEX_POINT ( 'NONE', #36943 ) ;
#36617 = FACE_OUTER_BOUND ( 'NONE', #43628, .T. ) ;
#36618 = CARTESIAN_POINT ( 'NONE',  ( -0.7495606340400177148, -0.1264236179284866091, 0.08612204719033110523 ) ) ;
#36619 = ORIENTED_EDGE ( 'NONE', *, *, #39590, .F. ) ;
#36620 = LINE ( 'NONE', #37077, #35196 ) ;
#36621 = CARTESIAN_POINT ( 'NONE',  ( -1.054774247047244096, 0.000000000000000000, 1.636318897584031484 ) ) ;
#36622 = ORIENTED_EDGE ( 'NONE', *, *, #4855, .F. ) ;
#36623 = CARTESIAN_POINT ( 'NONE',  ( -1.054774247047244096, 0.000000000000000000, 1.085137795221826629 ) ) ;
#36624 = AXIS2_PLACEMENT_3D ( 'NONE', #26619, #8138, #41174 ) ;
#36625 = CARTESIAN_POINT ( 'NONE',  ( -0.6971942568897637749, 2.189545951927499583E-17, 0.3617125983714334359 ) ) ;
#36626 = CARTESIAN_POINT ( 'NONE',  ( 0.7646288533564489232, 0.1113553986120547346, 0.4084645668216063119 ) ) ;
#36627 = CARTESIAN_POINT ( 'NONE',  ( 0.7495606340400177148, 0.1264236179284866091, 0.07627952750529173875 ) ) ;
#36628 = CARTESIAN_POINT ( 'NONE',  ( -0.3053406547161472417, 0.05476901150469701274, -0.7174944170560512147 ) ) ;
#36629 = CARTESIAN_POINT ( 'NONE',  ( 0.1787899950787401604, -0.3928405036623095481, 0.07405724077823318263 ) ) ;
#36630 = CARTESIAN_POINT ( 'NONE',  ( 0.01579235578554630259, -0.09842519685039370636, 0.1544717903359340561 ) ) ;
#36631 = ADVANCED_FACE ( 'NONE', ( #40979 ), #22794, .T. ) ;
#36632 = CARTESIAN_POINT ( 'NONE',  ( -0.7495606340400177148, -0.1264236179284866091, 0.3617125983714334359 ) ) ;
#36633 = ADVANCED_FACE ( 'NONE', ( #41200 ), #8406, .T. ) ;
#36634 = ORIENTED_EDGE ( 'NONE', *, *, #17360, .T. ) ;
#36635 = ORIENTED_EDGE ( 'NONE', *, *, #46027, .F. ) ;
#36636 = EDGE_CURVE ( 'NONE', #30501, #5626, #11086, .T. ) ;
#36637 = CARTESIAN_POINT ( 'NONE',  ( -0.9500414927467377701, 0.1787899950787401604, 1.333661417269071281 ) ) ;
#36638 = EDGE_LOOP ( 'NONE', ( #10087, #536, #34378, #2856 ) ) ;
#36639 = ADVANCED_FACE ( 'NONE', ( #34534 ), #20069, .T. ) ;
#36640 = CARTESIAN_POINT ( 'NONE',  ( 0.1787899950787401882, -1.166830708607653477, -2.189545951927503898E-17 ) ) ;
#36641 = CARTESIAN_POINT ( 'NONE',  ( -0.07405724077823318263, -1.307086614119465695, -0.1787899950787401604 ) ) ;
#36642 = CIRCLE ( 'NONE', #32070, 0.1968503937007874127 ) ;
#36643 = DIRECTION ( 'NONE',  ( -1.000000000000000000, 0.000000000000000000, 0.000000000000000000 ) ) ;
#36644 = CARTESIAN_POINT ( 'NONE',  ( 1.033464566929134687, 0.06523048226347956391, 0.3666338582677165503 ) ) ;
#36645 = DIRECTION ( 'NONE',  ( 0.000000000000000000, -1.000000000000000000, 0.000000000000000000 ) ) ;
#36646 = CARTESIAN_POINT ( 'NONE',  ( -0.9412147342319837628, -0.1574803149606297803, 0.9374999998924736788 ) ) ;
#36647 = AXIS2_PLACEMENT_3D ( 'NONE', #13384, #42799, #31137 ) ;
#36648 = CARTESIAN_POINT ( 'NONE',  ( -0.1574803149606299191, -0.1062992125984252023, 0.000000000000000000 ) ) ;
#36649 = CARTESIAN_POINT ( 'NONE',  ( 0.7185039370078746268, 0.06523048226347956391, 1.788877952648378233 ) ) ;
#36650 = ORIENTED_EDGE ( 'NONE', *, *, #6974, .T. ) ;
#36651 = DIRECTION ( 'NONE',  ( 1.000000000000000000, 0.000000000000000000, 0.000000000000000000 ) ) ;
#36652 = CARTESIAN_POINT ( 'NONE',  ( 0.7646288533564489232, -0.1113553986120547346, 0.9399606299212598381 ) ) ;
#36653 = AXIS2_PLACEMENT_3D ( 'NONE', #17644, #25073, #13358 ) ;
#36654 = CARTESIAN_POINT ( 'NONE',  ( 0.8759842519685039353, 0.1574803149606299191, 1.358267716535433323 ) ) ;
#36656 = CARTESIAN_POINT ( 'NONE',  ( 0.8107537697050254399, -0.1574803149606297803, 1.532972440944882386 ) ) ;
#36655 = FACE_OUTER_BOUND ( 'NONE', #42503, .T. ) ;
#36657 = DIRECTION ( 'NONE',  ( 0.000000000000000000, 0.000000000000000000, 1.000000000000000000 ) ) ;
#36658 = CARTESIAN_POINT ( 'NONE',  ( -0.3070711847658871285, 0.04416910270118645093, 1.037751739429055409 ) ) ;
#36659 = CARTESIAN_POINT ( 'NONE',  ( -0.07405724077823318263, -0.04724409443442544737, -0.1787899950787401604 ) ) ;
#36660 = ORIENTED_EDGE ( 'NONE', *, *, #26606, .T. ) ;
#36661 = DIRECTION ( 'NONE',  ( -1.000000000000000000, 0.000000000000000000, 0.000000000000000000 ) ) ;
#36662 = DIRECTION ( 'NONE',  ( -1.000000000000000000, 0.000000000000000000, 0.000000000000000000 ) ) ;
#36663 = CARTESIAN_POINT ( 'NONE',  ( -0.1264236179284866091, -1.540846456639149542, -0.1264236179284866091 ) ) ;
#36664 = CARTESIAN_POINT ( 'NONE',  ( -0.06523048226347956391, -1.585137795168063413, 0.1574803149606297803 ) ) ;
#36665 = CARTESIAN_POINT ( 'NONE',  ( 0.07405724077823318263, -0.7017716534895438452, 0.1787899950787401604 ) ) ;
#36666 = CARTESIAN_POINT ( 'NONE',  ( -1.033464566929133799, 0.000000000000000000, 0.07874015737278799998 ) ) ;
#36667 = CARTESIAN_POINT ( 'NONE',  ( 0.1574803149606300301, -1.073326771653543066, 0.06523048226347956391 ) ) ;
#36668 = CARTESIAN_POINT ( 'NONE',  ( 0.7185039370078746268, 0.06523048226347956391, 1.001476377845228027 ) ) ;
#36669 = CARTESIAN_POINT ( 'NONE',  ( -0.8070866141732283561, -0.0009842519685049383633, 0.7574803149606299524 ) ) ;
#36670 = CARTESIAN_POINT ( 'NONE',  ( -1.002407869896990045, 0.1264236179284866091, 0.3813976377415121966 ) ) ;
#36671 = VERTEX_POINT ( 'NONE', #31192 ) ;
#36672 = EDGE_LOOP ( 'NONE', ( #14316, #17318, #25918, #47220 ) ) ;
#36673 = ORIENTED_EDGE ( 'NONE', *, *, #29273, .T. ) ;
#36674 = CARTESIAN_POINT ( 'NONE',  ( -1.002407869896990045, 0.1264236179284866091, 1.685531496009228469 ) ) ;
#36675 = CARTESIAN_POINT ( 'NONE',  ( 1.002407869896990045, -0.1264236179284866091, 1.754429133804503715 ) ) ;
#36676 = CARTESIAN_POINT ( 'NONE',  ( -0.8019270111902717657, 0.1787899950787401604, 0.8661417322297003674 ) ) ;
#36677 = CARTESIAN_POINT ( 'NONE',  ( 0.6971942568897626646, -0.07405724077823297447, 0.3248031495525359746 ) ) ;
#36678 = CARTESIAN_POINT ( 'NONE',  ( -0.7646288533564489232, 0.1113553986120547346, 0.2608267716535432879 ) ) ;
#36679 = CARTESIAN_POINT ( 'NONE',  ( -0.7495606340400177148, -0.1264236179284866091, 0.7160433070328504623 ) ) ;
#36680 = CARTESIAN_POINT ( 'NONE',  ( -0.3161444924769509779, 1.690605217543007077, -0.5092277576975137166 ) ) ;
#36681 = TOROIDAL_SURFACE ( 'NONE', #26744, 0.3912448816427699927, 0.04921259842519685318 ) ;
#36682 = FACE_OUTER_BOUND ( 'NONE', #27850, .T. ) ;
#36683 = CARTESIAN_POINT ( 'NONE',  ( -1.002407869896990045, 0.1264236179284866091, 1.606791338528913426 ) ) ;
#36684 = CARTESIAN_POINT ( 'NONE',  ( -0.8107537697050253289, 0.1574803149606300301, 1.902066929026330788 ) ) ;
#36685 = VERTEX_POINT ( 'NONE', #1212 ) ;
#36686 = CARTESIAN_POINT ( 'NONE',  ( -0.7646288533564489232, -0.1113553986120547346, 1.648622047244094668 ) ) ;
#36687 = FACE_OUTER_BOUND ( 'NONE', #7680, .T. ) ;
#36688 = CARTESIAN_POINT ( 'NONE',  ( 1.002407869896990045, -0.1264236179284866091, 1.400098425143086800 ) ) ;
#36689 = CARTESIAN_POINT ( 'NONE',  ( -0.7646288533564489232, -0.1113553986120547346, 1.569881889763779625 ) ) ;
#36690 = ORIENTED_EDGE ( 'NONE', *, *, #30763, .F. ) ;
#36691 = VECTOR ( 'NONE', #20236, 39.37007874015748854 ) ;
#36692 = EDGE_CURVE ( 'NONE', #28921, #40494, #35636, .T. ) ;
#36693 = VERTEX_POINT ( 'NONE', #37894 ) ;
#36694 = AXIS2_PLACEMENT_3D ( 'NONE', #13672, #38839, #46019 ) ;
#36695 = ( LENGTH_UNIT ( ) NAMED_UNIT ( * ) SI_UNIT ( $, .METRE. ) ) ;
#36696 = VERTEX_POINT ( 'NONE', #12262 ) ;
#36697 = EDGE_CURVE ( 'NONE', #6075, #32411, #44167, .T. ) ;
#36698 = DIRECTION ( 'NONE',  ( 0.000000000000000000, 0.000000000000000000, 1.000000000000000000 ) ) ;
#36699 = CARTESIAN_POINT ( 'NONE',  ( 0.07405724077823318263, -0.4261811023084413064, 0.1787899950787401604 ) ) ;
#36700 = CARTESIAN_POINT ( 'NONE',  ( -0.1787899950787401882, -0.9453740156942677109, 0.000000000000000000 ) ) ;
#36701 = FACE_OUTER_BOUND ( 'NONE', #47198, .T. ) ;
#36702 = CARTESIAN_POINT ( 'NONE',  ( 1.054774247047244096, 0.000000000000000000, 1.793799212544661348 ) ) ;
#36703 = CARTESIAN_POINT ( 'NONE',  ( 0.1797182628040039365, -0.2569335733625732199, -2.200913952912460540E-17 ) ) ;
#36704 = CARTESIAN_POINT ( 'NONE',  ( -0.1264236179284866091, -0.1787657005127031573, -0.1264236179284866091 ) ) ;
#36705 = CARTESIAN_POINT ( 'NONE',  ( 0.2471889898699782262, -0.06575181108683454678, -0.09853485309448883900 ) ) ;
#36706 = CARTESIAN_POINT ( 'NONE',  ( 0.6971942568897626646, -0.07405724077823297447, 0.5561023621509617598 ) ) ;
#36707 = AXIS2_PLACEMENT_3D ( 'NONE', #15829, #41406, #5011 ) ;
#36708 = CARTESIAN_POINT ( 'NONE',  ( 0.1377952755905510474, 1.687505431895957647E-17, -0.2610569382242185488 ) ) ;
#36709 = DIRECTION ( 'NONE',  ( 0.000000000000000000, -0.7880107536067197938, 0.6156614753256609562 ) ) ;
#36710 = DIRECTION ( 'NONE',  ( -0.5735764363510409414, -0.6455006197386570221, 0.5043203561029929727 ) ) ;
#36711 = CARTESIAN_POINT ( 'NONE',  ( 0.6971942568897648851, -0.07405724077823297447, 1.899606299158834943 ) ) ;
#36713 = CARTESIAN_POINT ( 'NONE',  ( 0.8107537697050254399, 0.1574803149606300301, 0.1304133857192446289 ) ) ;
#36712 = DIRECTION ( 'NONE',  ( 1.000000000000000000, 0.000000000000000000, -1.822029033848725275E-16 ) ) ;
#36714 = ORIENTED_EDGE ( 'NONE', *, *, #29963, .T. ) ;
#36715 = LINE ( 'NONE', #11325, #22894 ) ;
#36716 = CARTESIAN_POINT ( 'NONE',  ( -1.094772975963752103E-17, -0.2908464566391499861, -0.1787899950787401882 ) ) ;
#36717 = CARTESIAN_POINT ( 'NONE',  ( -0.7495606340400177148, 0.1264236179284866091, 0.4355314960092284138 ) ) ;
#36718 = AXIS2_PLACEMENT_3D ( 'NONE', #10824, #21338, #29311 ) ;
#36719 = ADVANCED_FACE ( 'NONE', ( #38355 ), #36126, .T. ) ;
#36720 = CARTESIAN_POINT ( 'NONE',  ( 0.07405724077823318263, -1.090551181048598606, 0.1787899950787401604 ) ) ;
#36721 = CARTESIAN_POINT ( 'NONE',  ( 0.6971942568897626646, 0.07405724077823318263, 0.1230314960092287191 ) ) ;
#36722 = CARTESIAN_POINT ( 'NONE',  ( -0.8759842519685039353, 0.000000000000000000, 0.000000000000000000 ) ) ;
#36723 = CARTESIAN_POINT ( 'NONE',  ( -1.054774247047244096, 0.000000000000000000, 1.557578740103716441 ) ) ;
#36724 = ORIENTED_EDGE ( 'NONE', *, *, #19643, .F. ) ;
#36725 = CARTESIAN_POINT ( 'NONE',  ( -0.6971942568897648851, 0.07405724077823318263, 1.146653543253323582 ) ) ;
#36727 = AXIS2_PLACEMENT_3D ( 'NONE', #6715, #37302, #11223 ) ;
#36726 = LINE ( 'NONE', #25947, #12314 ) ;
#36728 = CARTESIAN_POINT ( 'NONE',  ( 1.054774247047244540, -0.07405724077823318263, 1.245078740103716886 ) ) ;
#36729 = CARTESIAN_POINT ( 'NONE',  ( -0.1113553986120547346, -1.203740157372787500, -0.1113553986120547346 ) ) ;
#36730 = CARTESIAN_POINT ( 'NONE',  ( -0.7646288533564489232, -0.1113553986120547346, 0.5856299212598424786 ) ) ;
#36731 = CARTESIAN_POINT ( 'NONE',  ( -1.054774247047244096, 0.000000000000000000, 1.085137795221826629 ) ) ;
#36732 = CARTESIAN_POINT ( 'NONE',  ( 0.1644020957507537628, 0.08115590401245550978, 0.1405661490837558925 ) ) ;
#36733 = CARTESIAN_POINT ( 'NONE',  ( -0.05614424849857162919, -0.2630793352783083461, -0.05546260682012697785 ) ) ;
#36734 = CARTESIAN_POINT ( 'NONE',  ( 0.7495606340400177148, 0.1264236179284866091, 0.3567913385289137596 ) ) ;
#36735 = CARTESIAN_POINT ( 'NONE',  ( -0.6971942568897637749, 2.189545951927499583E-17, 0.1993110235682838682 ) ) ;
#36736 = CARTESIAN_POINT ( 'NONE',  ( -1.002407869896990045, -0.1264236179284866091, 0.8046259841982047467 ) ) ;
#36737 = CARTESIAN_POINT ( 'NONE',  ( 1.033464566929134687, -0.06523048226347956391, 1.690452755797984929 ) ) ;
#36738 = CARTESIAN_POINT ( 'NONE',  ( -0.1264236179284866091, 0.02903543312462964626, -0.1264236179284866091 ) ) ;
#36739 = ORIENTED_EDGE ( 'NONE', *, *, #18830, .T. ) ;
#36740 = CARTESIAN_POINT ( 'NONE',  ( 0.6971942568897637749, 2.189545951927499583E-17, 0.7554133857730077617 ) ) ;
#36741 = CARTESIAN_POINT ( 'NONE',  ( 0.8759842519685039353, -0.1787899950787401882, 1.119586614119464585 ) ) ;
#36742 = CARTESIAN_POINT ( 'NONE',  ( -1.054774247047244096, 0.000000000000000000, 1.833169291284818758 ) ) ;
#36743 = ORIENTED_EDGE ( 'NONE', *, *, #11703, .T. ) ;
#36744 = EDGE_CURVE ( 'NONE', #35290, #22349, #13198, .T. ) ;
#36745 = CARTESIAN_POINT ( 'NONE',  ( 0.7495606340400177148, -0.1264236179284866091, 1.897145669237574772 ) ) ;
#36746 = ADVANCED_FACE ( 'NONE', ( #19430 ), #46239, .T. ) ;
#36747 = AXIS2_PLACEMENT_3D ( 'NONE', #2295, #27033, #20275 ) ;
#36748 = CARTESIAN_POINT ( 'NONE',  ( 0.8759842519685039353, -0.1574803149606299191, 1.604330708553889595 ) ) ;
#36749 = CARTESIAN_POINT ( 'NONE',  ( -0.1787899950787401882, -1.354946802874907652, 0.000000000000000000 ) ) ;
#36750 = ORIENTED_EDGE ( 'NONE', *, *, #15768, .F. ) ;
#36751 = CARTESIAN_POINT ( 'NONE',  ( 3.284318927891251994E-17, -0.2662401574265516047, 0.1787899950787401882 ) ) ;
#36752 = CARTESIAN_POINT ( 'NONE',  ( -0.8759842519685039353, 0.1574803149606299191, 1.702755905404283565 ) ) ;
#36753 = ORIENTED_EDGE ( 'NONE', *, *, #33083, .T. ) ;
#36754 = CARTESIAN_POINT ( 'NONE',  ( 0.6971942568897648851, -0.07405724077823297447, 1.186023621993481658 ) ) ;
#36755 = EDGE_CURVE ( 'NONE', #12403, #43186, #15485, .T. ) ;
#36756 = AXIS2_PLACEMENT_3D ( 'NONE', #5915, #42078, #5680 ) ;
#36757 = CARTESIAN_POINT ( 'NONE',  ( 0.8107537697050254399, 0.1574803149606300301, 1.390255905404285119 ) ) ;
#36758 = ( BOUNDED_CURVE ( )  B_SPLINE_CURVE ( 2, ( #18388, #35889, #3043, #32564, #28489, #14335, #28980, #25360, #25601 ),
 .UNSPECIFIED., .F., .T. ) 
 B_SPLINE_CURVE_WITH_KNOTS ( ( 3, 2, 2, 2, 3 ),
 ( 0.1700000000000000122, 0.1724999999999999867, 0.1749999999999999889, 0.1774999999999999911, 0.1799999999999999933 ),
 .UNSPECIFIED. ) 
 CURVE ( )  GEOMETRIC_REPRESENTATION_ITEM ( )  RATIONAL_B_SPLINE_CURVE ( ( 1.000000000000000000, 0.9238795325112869605, 1.000000000000000000, 0.9238795325112869605, 1.000000000000000000, 0.9238795325112869605, 1.000000000000000000, 0.9238795325112869605, 1.000000000000000000 ) ) 
 REPRESENTATION_ITEM ( '' )  ) ;
#36759 = CARTESIAN_POINT ( 'NONE',  ( 1.002407869896990045, -0.1264236179284866091, 1.473917322780881722 ) ) ;
#36760 = CARTESIAN_POINT ( 'NONE',  ( 0.7495606340400177148, 0.1264236179284866091, 0.1156496062454492185 ) ) ;
#36761 = CARTESIAN_POINT ( 'NONE',  ( -0.1787899950787401604, -1.622047244040725866, -0.07405724077823318263 ) ) ;
#36762 = CARTESIAN_POINT ( 'NONE',  ( 0.1264236179284866091, -1.747539370024976391, -0.1264236179284866091 ) ) ;
#36763 = CARTESIAN_POINT ( 'NONE',  ( -1.002407869896990045, 0.1264236179284866091, 0.4256889763241890057 ) ) ;
#36764 = LINE ( 'NONE', #33908, #38519 ) ;
#36765 = CARTESIAN_POINT ( 'NONE',  ( -0.1797182628040039365, -1.339610738716903393, 0.000000000000000000 ) ) ;
#36766 = CARTESIAN_POINT ( 'NONE',  ( 0.8107537697050254399, 0.1574803149606300301, 1.439468503937006760 ) ) ;
#36767 = CARTESIAN_POINT ( 'NONE',  ( 0.8019270111902717657, 0.1787899950787401604, 1.377952755851748146 ) ) ;
#36768 = CARTESIAN_POINT ( 'NONE',  ( 0.6971942568897648851, -0.07405724077823297447, 1.658464566875369472 ) ) ;
#36769 = DIRECTION ( 'NONE',  ( 1.000000000000000000, 0.000000000000000000, -1.822029033848725275E-16 ) ) ;
#36770 = CARTESIAN_POINT ( 'NONE',  ( -0.03645729789547116212, 0.1299212598425194265, 0.1690525858836274820 ) ) ;
#36771 = CARTESIAN_POINT ( 'NONE',  ( -1.181162989532618060E-16, -0.3937007874015746034, -0.2952755905511816326 ) ) ;
#36772 = CARTESIAN_POINT ( 'NONE',  ( 0.1498753904841984286, -1.109813247426106378E-16, -0.1377952755905511861 ) ) ;
#36773 = CARTESIAN_POINT ( 'NONE',  ( 0.8759842519685039353, 0.000000000000000000, 4.498031496062992574 ) ) ;
#36774 = DIRECTION ( 'NONE',  ( 0.000000000000000000, 0.000000000000000000, 1.000000000000000000 ) ) ;
#36776 = CARTESIAN_POINT ( 'NONE',  ( 0.9500414927467378812, -0.1787899950787401604, 0.2509842519147403861 ) ) ;
#36775 = ( BOUNDED_CURVE ( )  B_SPLINE_CURVE ( 2, ( #2103, #45947, #38064, #13159, #9550, #38773, #5933, #35191, #18144 ),
 .UNSPECIFIED., .F., .F. ) 
 B_SPLINE_CURVE_WITH_KNOTS ( ( 3, 2, 2, 2, 3 ),
 ( 0.06500000000000000222, 0.06750000000000000444, 0.07000000000000000666, 0.07249999999999999500, 0.07499999999999999722 ),
 .UNSPECIFIED. ) 
 CURVE ( )  GEOMETRIC_REPRESENTATION_ITEM ( )  RATIONAL_B_SPLINE_CURVE ( ( 1.000000000000000000, 0.9238795325112869605, 1.000000000000000000, 0.9238795325112869605, 1.000000000000000000, 0.9238795325112869605, 1.000000000000000000, 0.9238795325112869605, 1.000000000000000000 ) ) 
 REPRESENTATION_ITEM ( '' )  ) ;
#36777 = CARTESIAN_POINT ( 'NONE',  ( 0.7182464370288005329, -0.06544858470024300656, 0.03937008086776665194 ) ) ;
#36779 = DIRECTION ( 'NONE',  ( -1.000000000000000000, 0.000000000000000000, -0.000000000000000000 ) ) ;
#36778 = CARTESIAN_POINT ( 'NONE',  ( 1.054774247047244096, 0.000000000000000000, 1.281988188922614125 ) ) ;
#36780 = AXIS2_PLACEMENT_3D ( 'NONE', #45825, #21137, #35312 ) ;
#36781 = LINE ( 'NONE', #96, #2368 ) ;
#36782 = CARTESIAN_POINT ( 'NONE',  ( -0.8759842519685039353, -0.1787899950787401882, 1.193405511757259951 ) ) ;
#36783 = CARTESIAN_POINT ( 'NONE',  ( 0.7185039370078746268, -0.06523048226347956391, 0.7308070865066471633 ) ) ;
#36784 = ORIENTED_EDGE ( 'NONE', *, *, #36269, .T. ) ;
#36785 = FILL_AREA_STYLE_COLOUR ( '', #38325 ) ;
#36786 = CARTESIAN_POINT ( 'NONE',  ( 0.8915560649286792261, 0.1728905949868962677, 0.03937011864913666365 ) ) ;
#36787 = CARTESIAN_POINT ( 'NONE',  ( -0.9412147342319837628, -0.1574803149606297803, 0.3075787400499532809 ) ) ;
#36788 = PRODUCT_DEFINITION_SHAPE ( 'NONE', 'NONE',  #47462 ) ;
#36789 = AXIS2_PLACEMENT_3D ( 'NONE', #8594, #26836, #22984 ) ;
#36790 = CARTESIAN_POINT ( 'NONE',  ( 0.7185039370078739607, 1.928577636452523993E-17, 0.4133858266641267654 ) ) ;
#36791 = CARTESIAN_POINT ( 'NONE',  ( -0.7185039370078746268, -0.06523048226347956391, 1.173720472440945573 ) ) ;
#36792 = CARTESIAN_POINT ( 'NONE',  ( 0.8070866141732283561, -0.3937007874015746034, 0.7574803149606299524 ) ) ;
#36794 = CARTESIAN_POINT ( 'NONE',  ( -0.8759842519685039353, -0.1574803149606299191, 1.377952755905512028 ) ) ;
#36793 = CARTESIAN_POINT ( 'NONE',  ( 2.892866454678787531E-17, 0.06102362204724409711, 0.1574803149606299191 ) ) ;
#36796 = CIRCLE ( 'NONE', #5401, 0.5708661417322835607 ) ;
#36795 = CARTESIAN_POINT ( 'NONE',  ( -0.1787899950787401604, -0.1604330708123782034, -0.07405724077823318263 ) ) ;
#36797 = ORIENTED_EDGE ( 'NONE', *, *, #30093, .T. ) ;
#36798 = CARTESIAN_POINT ( 'NONE',  ( -0.7185039370078739607, 1.928577636452523993E-17, 0.3838582677165354173 ) ) ;
#36799 = CARTESIAN_POINT ( 'NONE',  ( -0.04858533447342696515, -0.07294156354243679086, 0.2573812140284292838 ) ) ;
#36800 = ORIENTED_EDGE ( 'NONE', *, *, #4750, .T. ) ;
#36801 = CARTESIAN_POINT ( 'NONE',  ( 1.054774247047244096, 0.000000000000000000, 0.5388779527021417826 ) ) ;
#36802 = EDGE_CURVE ( 'NONE', #35946, #7112, #28790, .T. ) ;
#36803 = VERTEX_POINT ( 'NONE', #5990 ) ;
#36804 = CARTESIAN_POINT ( 'NONE',  ( -9.642888182262618425E-18, 0.05118110246973173183, -0.1574803149606299191 ) ) ;
#36805 = CARTESIAN_POINT ( 'NONE',  ( -0.7495606340400177148, 0.1264236179284866091, 1.144192913332062966 ) ) ;
#36806 = ORIENTED_EDGE ( 'NONE', *, *, #34319, .T. ) ;
#36807 = CARTESIAN_POINT ( 'NONE',  ( -0.2559055118110235560, -0.07545482141442715063, -0.05057764367740170269 ) ) ;
#36808 = EDGE_CURVE ( 'NONE', #10105, #38112, #31047, .T. ) ;
#36809 = CARTESIAN_POINT ( 'NONE',  ( -0.8019270111902717657, -0.1787899950787401604, 0.2116141731745827814 ) ) ;
#36810 = LINE ( 'NONE', #824, #30314 ) ;
#36811 = DIRECTION ( 'NONE',  ( 0.000000000000000000, 1.000000000000000000, 0.000000000000000000 ) ) ;
#36812 = CARTESIAN_POINT ( 'NONE',  ( 0.1787899950787401882, -0.8628208186229389121, -2.189545951927503898E-17 ) ) ;
#36813 = ORIENTED_EDGE ( 'NONE', *, *, #38043, .F. ) ;
#36814 = CARTESIAN_POINT ( 'NONE',  ( 0.07405724077823318263, 0.1299212598962831977, 0.1787899950787401604 ) ) ;
#36815 = ORIENTED_EDGE ( 'NONE', *, *, #3195, .F. ) ;
#36816 = B_SPLINE_CURVE_WITH_KNOTS ( 'NONE', 3,
 ( #46102, #13301, #27965, #2523, #17378, #27744, #42309, #46375, #1821, #31558, #23878, #13556, #24581, #2753, #32016, #46608, #46137, #27265, #5897, #5413, #20268, #42056, #16692, #31320, #45895, #3228, #39643, #18565, #39410, #43482, #42998, #7069, #2987, #100, #7316, #10207, #32975, #43963, #11161, #21443, #32502, #28918, #25296, #24812, #14746, #6593, #29418, #14507, #3942, #36072, #3715, #36330, #25779, #21935, #29169, #40349, #17619, #36786, #21206, #10689, #7541, #22153, #33222, #3482, #10449, #47085, #32264, #46843, #25048, #10927, #43723, #14032, #18095, #32741, #47337, #25549, #40120, #36555, #44891, #34157, #26729, #5119, #19025, #37730, #15225, #29872, #30342, #44414 ),
 .UNSPECIFIED., .F., .F.,
 ( 4, 2, 2, 1, 1, 2, 2, 2, 2, 2, 2, 2, 2, 2, 2, 2, 1, 1, 1, 1, 1, 2, 2, 2, 2, 2, 1, 1, 1, 2, 2, 2, 2, 1, 1, 2, 2, 2, 2, 1, 1, 1, 2, 2, 2, 2, 1, 1, 1, 2, 2, 2, 4 ),
 ( 0.000000000000000000, 0.06249999999922203897, 0.09374999999883308621, 0.1093749999986385890, 0.1171874999985414306, 0.1210937499984927890, 0.1249999999984441335, 0.1874999999976660059, 0.2187499999972769282, 0.2499999999968878228, 0.3124999999961092234, 0.3437499999957202568, 0.3593749999955259122, 0.3749999999953315122, 0.4374999999945541895, 0.4687499999941655004, 0.4843749999939712669, 0.4921874999938741224, 0.4960937499938254946, 0.4980468749938006257, 0.4990234374937876360, 0.4995117187437816964, 0.4999999999937758122, 0.5624999999945692331, 0.5937499999949663598, 0.6093749999951645346, 0.6171874999952633445, 0.6210937499953124163, 0.6230468749953369523, 0.6240234374953490537, 0.6249999999953610441, 0.6874999999961505237, 0.7187499999965453190, 0.7343749999967427167, 0.7421874999968420816, 0.7460937499968910425, 0.7499999999969400033, 0.7812499999973340215, 0.7968749999975310860, 0.8046874999976295628, 0.8085937499976788567, 0.8105468749977035037, 0.8115234374977157161, 0.8124999999977280396, 0.8437499999980859755, 0.8593749999982649435, 0.8671874999983544274, 0.8710937499983996135, 0.8730468749984222621, 0.8740234374984335863, 0.8749999999984447996, 0.9374999999992223998, 1.000000000000000000 ),
 .UNSPECIFIED. ) ;
#36817 = EDGE_CURVE ( 'NONE', #45011, #8121, #43355, .T. ) ;
#36818 = CARTESIAN_POINT ( 'NONE',  ( -0.8019270111902717657, 0.1787899950787401604, 0.7431102361667091261 ) ) ;
#36819 = CARTESIAN_POINT ( 'NONE',  ( 0.4736248074375850603, 1.357244529069700612, -1.397888825503269761 ) ) ;
#36821 = VERTEX_POINT ( 'NONE', #21314 ) ;
#36820 = AXIS2_PLACEMENT_3D ( 'NONE', #8589, #24399, #27321 ) ;
#36822 = EDGE_CURVE ( 'NONE', #20918, #42760, #46384, .T. ) ;
#36823 = PRODUCT_DEFINITION ( 'UNKNOWN', '', #34712, #2478 ) ;
#36824 = MECHANICAL_DESIGN_GEOMETRIC_PRESENTATION_REPRESENTATION (  '', ( #7733 ), #23783 ) ;
#36825 = CARTESIAN_POINT ( 'NONE',  ( -0.7495606340400177148, 0.1264236179284866091, 0.08120078734781142893 ) ) ;
#36826 = CARTESIAN_POINT ( 'NONE',  ( -0.8759842519685039353, -0.1574803149606299191, 0.9055118110236221041 ) ) ;
#36827 = CARTESIAN_POINT ( 'NONE',  ( 1.033464566929133799, 0.000000000000000000, 0.6397637795275591399 ) ) ;
#36828 = CARTESIAN_POINT ( 'NONE',  ( -0.1797182628040039365, -0.9852800300554862556, 0.000000000000000000 ) ) ;
#36829 = CARTESIAN_POINT ( 'NONE',  ( 0.04257025887484965077, -0.2709160761539660123, -0.3049284531893265981 ) ) ;
#36830 = CARTESIAN_POINT ( 'NONE',  ( -0.9412147342319837628, -0.1574803149606297803, 1.488681102254677535 ) ) ;
#36831 = CIRCLE ( 'NONE', #15390, 0.1574803149606299191 ) ;
#36832 = CARTESIAN_POINT ( 'NONE',  ( 0.8019270111902717657, 0.1787899950787401604, 0.8267716534895444003 ) ) ;
#36833 = CARTESIAN_POINT ( 'NONE',  ( -1.054774247047244096, 0.000000000000000000, 1.993110236166708793 ) ) ;
#36834 = CARTESIAN_POINT ( 'NONE',  ( 0.7185039370078746268, 0.06523048226347956391, 1.444389763779527991 ) ) ;
#36836 = DIRECTION ( 'NONE',  ( 1.000000000000000000, 0.000000000000000000, 0.000000000000000000 ) ) ;
#36835 = CARTESIAN_POINT ( 'NONE',  ( 0.7767998692430261309, -0.1394856968632323391, 1.986240030985245264 ) ) ;
#36837 = CARTESIAN_POINT ( 'NONE',  ( 0.8759842519685039353, 0.1787899950787401882, 0.7800196849856062542 ) ) ;
#36838 = CARTESIAN_POINT ( 'NONE',  ( -0.1264236179284866091, -0.7829724408911181710, 0.1264236179284866091 ) ) ;
#36839 = DIRECTION ( 'NONE',  ( 0.000000000000000000, 1.000000000000000000, 0.000000000000000000 ) ) ;
#36840 = CARTESIAN_POINT ( 'NONE',  ( 0.7495606340400177148, -0.1264236179284866091, 1.031003936954110189 ) ) ;
#36841 = EDGE_CURVE ( 'NONE', #3105, #43609, #10803, .T. ) ;
#36842 = CARTESIAN_POINT ( 'NONE',  ( 0.1574803149606300301, -1.658956692913385655, -0.06523048226347956391 ) ) ;
#36843 = CARTESIAN_POINT ( 'NONE',  ( -0.9412147342319837628, -0.1574803149606297803, 0.5142716535433068392 ) ) ;
#36844 = VERTEX_POINT ( 'NONE', #42632 ) ;
#36845 = CARTESIAN_POINT ( 'NONE',  ( -0.1476377952755905387, 1.126631386849005878, -3.440787370833236380 ) ) ;
#36846 = CARTESIAN_POINT ( 'NONE',  ( -0.8759842519685039353, 0.1787899950787401882, 0.07135826766277185429 ) ) ;
#36847 = ORIENTED_EDGE ( 'NONE', *, *, #20684, .F. ) ;
#36848 = EDGE_CURVE ( 'NONE', #12706, #14162, #895, .T. ) ;
#36849 = CARTESIAN_POINT ( 'NONE',  ( -0.1574803149606300301, 0.05856299223351124628, -0.06523048226347956391 ) ) ;
#36850 = CARTESIAN_POINT ( 'NONE',  ( 3.284318927891251994E-17, -1.452263779473795369, 0.1787899950787401882 ) ) ;
#36851 = CARTESIAN_POINT ( 'NONE',  ( 0.3551574803149606385, 0.1574803149606299191, 1.928577636452523993E-17 ) ) ;
#36852 = MECHANICAL_DESIGN_GEOMETRIC_PRESENTATION_REPRESENTATION (  '', ( #33047 ), #23855 ) ;
#36853 = CARTESIAN_POINT ( 'NONE',  ( -1.054774247047244096, 0.000000000000000000, 1.754429133804503715 ) ) ;
#36854 = CARTESIAN_POINT ( 'NONE',  ( -1.054774247047244096, 0.000000000000000000, 0.8489173227808819444 ) ) ;
#36855 = AXIS2_PLACEMENT_3D ( 'NONE', #38717, #27013, #23629 ) ;
#36856 = CARTESIAN_POINT ( 'NONE',  ( -1.054774247047244096, 0.000000000000000000, 0.3420275590013546751 ) ) ;
#36857 = CARTESIAN_POINT ( 'NONE',  ( -0.7185039370078732945, -0.06523048226347920309, 0.1500984251968504879 ) ) ;
#36858 = CARTESIAN_POINT ( 'NONE',  ( 0.1571284080983731402, 0.02678626661725594035, 0.1404155760989011514 ) ) ;
#36859 = CARTESIAN_POINT ( 'NONE',  ( 0.07975836855958620686, 0.08959396230938582173, -0.2393845553081391520 ) ) ;
#36860 = CARTESIAN_POINT ( 'NONE',  ( -0.2741498948998220553, 0.1449524278970012459, -0.9602547136744080669 ) ) ;
#36861 = CARTESIAN_POINT ( 'NONE',  ( -1.094772975963752103E-17, -0.4199074327961677122, -0.1787899950787401882 ) ) ;
#36862 = CARTESIAN_POINT ( 'NONE',  ( -0.2158178664699031413, -0.08955986809707854046, 0.08935017772872932973 ) ) ;
#36863 = CYLINDRICAL_SURFACE ( 'NONE', #1142, 0.1574803149606299191 ) ;
#36864 = LINE ( 'NONE', #25625, #31877 ) ;
#36865 = PRODUCT_RELATED_PRODUCT_CATEGORY ( 'part', '', ( #38465 ) ) ;
#36866 = CARTESIAN_POINT ( 'NONE',  ( 0.2559055015491151774, -0.08324699190379426794, -0.05567992556649694474 ) ) ;
#36867 = CARTESIAN_POINT ( 'NONE',  ( -0.8759842519685039353, 0.1787899950787401882, 0.2682086613635594752 ) ) ;
#36868 = ORIENTED_EDGE ( 'NONE', *, *, #21081, .F. ) ;
#36869 = CARTESIAN_POINT ( 'NONE',  ( -1.054774247047244540, 0.07405724077823318263, 1.328740157426552049 ) ) ;
#36870 = EDGE_LOOP ( 'NONE', ( #25662, #17359, #5512, #46427 ) ) ;
#36871 = AXIS2_PLACEMENT_3D ( 'NONE', #18545, #33201, #323 ) ;
#36872 = CARTESIAN_POINT ( 'NONE',  ( -0.07405724077823318263, -1.257874015694269376, 0.1787899950787401604 ) ) ;
#36873 = CARTESIAN_POINT ( 'NONE',  ( -0.07405724077823318263, -1.582677165300567346, -0.1787899950787401604 ) ) ;
#36874 = CIRCLE ( 'NONE', #16238, 0.03937007874015748671 ) ;
#36875 = FACE_BOUND ( 'NONE', #29605, .T. ) ;
#36876 = DIRECTION ( 'NONE',  ( -1.000000000000000000, 0.000000000000000000, 0.000000000000000000 ) ) ;
#36877 = CARTESIAN_POINT ( 'NONE',  ( 0.9873396505805591694, -0.1113553986120547346, 0.3592519685039369803 ) ) ;
#36878 = CARTESIAN_POINT ( 'NONE',  ( -0.1270800023317771588, -0.6358705812365885723, -0.1270800023317771588 ) ) ;
#36879 = CARTESIAN_POINT ( 'NONE',  ( 0.000000000000000000, 0.08719492171395763769, -0.5641677032617172793 ) ) ;
#36880 = CARTESIAN_POINT ( 'NONE',  ( -0.7185039370078746268, -0.06523048226347956391, 1.006397637687749036 ) ) ;
#36881 = DIRECTION ( 'NONE',  ( 0.8191520442889873577, 0.000000000000000000, 0.5735764363510523767 ) ) ;
#36882 = CARTESIAN_POINT ( 'NONE',  ( -0.1113553986120547346, -0.3080708661417322913, -0.1113553986120547346 ) ) ;
#36883 = AXIS2_PLACEMENT_3D ( 'NONE', #22069, #21355, #18478 ) ;
#36884 = AXIS2_PLACEMENT_3D ( 'NONE', #10263, #10982, #3289 ) ;
#36885 = ORIENTED_EDGE ( 'NONE', *, *, #33954, .F. ) ;
#36886 = CARTESIAN_POINT ( 'NONE',  ( 0.9873396505805591694, -0.1113553986120547346, 2.002952755797984263 ) ) ;
#36887 = ORIENTED_EDGE ( 'NONE', *, *, #32273, .F. ) ;
#36888 = CARTESIAN_POINT ( 'NONE',  ( -0.1251538622671300172, -0.09137144579352629581, -0.1276842799123791561 ) ) ;
#36889 = CARTESIAN_POINT ( 'NONE',  ( 1.033464566929134687, 0.06523048226347956391, 0.9178149606299221830 ) ) ;
#36890 = CARTESIAN_POINT ( 'NONE',  ( 0.7185039370078714072, 0.06523048226347728795, 1.365649606299213614 ) ) ;
#36891 = CARTESIAN_POINT ( 'NONE',  ( -0.1113553986120547346, -0.5246062991050708391, 0.1113553986120547346 ) ) ;
#36892 = DIRECTION ( 'NONE',  ( 1.000000000000000000, 0.000000000000000000, 0.000000000000000000 ) ) ;
#36893 = MANIFOLD_SOLID_BREP ( 'Side Bracket', #13265 ) ;
#36894 = CARTESIAN_POINT ( 'NONE',  ( -0.1715440989618680079, -0.08785038237295542118, -0.1863907177286787953 ) ) ;
#36895 = CARTESIAN_POINT ( 'NONE',  ( -0.2664436179446795228, 0.1586070934160168089, 0.8215608667368892171 ) ) ;
#36896 = VERTEX_POINT ( 'NONE', #6751 ) ;
#36897 = EDGE_CURVE ( 'NONE', #3732, #5428, #29308, .T. ) ;
#36898 = ORIENTED_EDGE ( 'NONE', *, *, #26324, .T. ) ;
#36899 = CARTESIAN_POINT ( 'NONE',  ( -0.7185039370078746268, -0.06523048226347956391, 0.6126968502861739330 ) ) ;
#36900 = DIRECTION ( 'NONE',  ( 0.000000000000000000, -1.000000000000000000, 0.000000000000000000 ) ) ;
#36901 = CARTESIAN_POINT ( 'NONE',  ( -0.07405724077823318263, -1.489173228292693718, 0.1787899950787401604 ) ) ;
#36902 = CARTESIAN_POINT ( 'NONE',  ( 0.1787899950787401604, -0.7706692912848194243, -0.07405724077823318263 ) ) ;
#36903 = CARTESIAN_POINT ( 'NONE',  ( 2.892866454678787531E-17, -1.238188976377952777, 0.1574803149606299191 ) ) ;
#36904 = CARTESIAN_POINT ( 'NONE',  ( 0.8107537697050253289, 0.1574803149606300301, 1.035925196742866650 ) ) ;
#36905 = ADVANCED_FACE ( 'NONE', ( #13953 ), #18488, .T. ) ;
#36906 = CARTESIAN_POINT ( 'NONE',  ( 0.8107537697050254399, 0.1574803149606300301, 1.833169291338582640 ) ) ;
#36907 = ORIENTED_EDGE ( 'NONE', *, *, #23701, .F. ) ;
#36908 = ORIENTED_EDGE ( 'NONE', *, *, #31189, .T. ) ;
#36909 = VERTEX_POINT ( 'NONE', #14200 ) ;
#36910 = CARTESIAN_POINT ( 'NONE',  ( -0.8759842519685039353, -0.1787899950787401882, 1.631397637741511808 ) ) ;
#36911 = EDGE_CURVE ( 'NONE', #43060, #6663, #14714, .T. ) ;
#36912 = CARTESIAN_POINT ( 'NONE',  ( 0.6971942568897648851, 0.07405724077823318263, 1.776574803095843924 ) ) ;
#36913 = CARTESIAN_POINT ( 'NONE',  ( -0.7495606340400177148, 0.1264236179284866091, 0.7504921259304880854 ) ) ;
#36914 = DIRECTION ( 'NONE',  ( 0.000000000000000000, 0.000000000000000000, -1.000000000000000000 ) ) ;
#36915 = CARTESIAN_POINT ( 'NONE',  ( 0.9500414927467378812, 0.1787899950787401604, 0.3494094487651343006 ) ) ;
#36916 = EDGE_CURVE ( 'NONE', #17177, #4491, #14910, .T. ) ;
#36917 = CARTESIAN_POINT ( 'NONE',  ( -0.7185039370078778465, -0.06523048226348396317, 1.675688976270425457 ) ) ;
#36918 = CARTESIAN_POINT ( 'NONE',  ( -0.7495606340400177148, 0.1264236179284866091, 1.218011810969858111 ) ) ;
#36919 = VECTOR ( 'NONE', #39805, 39.37007874015748143 ) ;
#36920 = CARTESIAN_POINT ( 'NONE',  ( 0.1113553986120547346, -0.08169291327829980576, 0.1113553986120547346 ) ) ;
#36921 = AXIS2_PLACEMENT_3D ( 'NONE', #2530, #21212, #28685 ) ;
#36922 = CARTESIAN_POINT ( 'NONE',  ( -0.6971942568897648851, -0.07405724077823297447, 1.584645669237574994 ) ) ;
#36923 = CARTESIAN_POINT ( 'NONE',  ( -0.7646288533564489232, -0.1113553986120547346, 1.953740157372787500 ) ) ;
#36924 = VERTEX_POINT ( 'NONE', #6993 ) ;
#36925 = CARTESIAN_POINT ( 'NONE',  ( -0.7185039370078746268, 0.06523048226347956391, 1.562500000000000000 ) ) ;
#36926 = DIRECTION ( 'NONE',  ( -1.000000000000000000, 0.000000000000000000, 0.000000000000000000 ) ) ;
#36927 = CARTESIAN_POINT ( 'NONE',  ( 1.054774247047244540, 0.07405724077823318263, 1.407480314906865981 ) ) ;
#36928 = CARTESIAN_POINT ( 'NONE',  ( -0.07592550097138189846, -0.09851382931116220432, 0.1427603709231669293 ) ) ;
#36929 = CARTESIAN_POINT ( 'NONE',  ( 1.033464566929133799, 0.000000000000000000, 1.062992125876724314 ) ) ;
#36930 = EDGE_LOOP ( 'NONE', ( #25628, #43011, #20172, #24541 ) ) ;
#36931 = AXIS2_PLACEMENT_3D ( 'NONE', #498, #15391, #18494 ) ;
#36932 = ORIENTED_EDGE ( 'NONE', *, *, #42928, .F. ) ;
#36933 = ORIENTED_EDGE ( 'NONE', *, *, #18399, .F. ) ;
#36934 = CARTESIAN_POINT ( 'NONE',  ( -0.07405724077823318263, -0.8641732282926931630, 0.1787899950787401604 ) ) ;
#36935 = CARTESIAN_POINT ( 'NONE',  ( -1.094772975963752103E-17, -0.4089566928596221063, -0.1787899950787401882 ) ) ;
#36936 = CARTESIAN_POINT ( 'NONE',  ( -0.1264236179284866091, -0.9798228345919054449, 0.1264236179284866091 ) ) ;
#36937 = CARTESIAN_POINT ( 'NONE',  ( -1.100456976456230270E-17, -0.2077209749373763736, -0.1797182628040039365 ) ) ;
#36938 = CARTESIAN_POINT ( 'NONE',  ( -0.1113553986120547346, 0.1348425196850393804, 0.1113553986120547346 ) ) ;
#36939 = CARTESIAN_POINT ( 'NONE',  ( -0.1264236179284866091, -0.01033464561552783524, -0.1264236179284866091 ) ) ;
#36940 = CARTESIAN_POINT ( 'NONE',  ( 0.9873396505805591694, -0.1113553986120547346, 0.1525590550105832555 ) ) ;
#36941 = CARTESIAN_POINT ( 'NONE',  ( 1.002407869896990045, 0.1264236179284866091, 0.6963582676627716461 ) ) ;
#36942 = MECHANICAL_DESIGN_GEOMETRIC_PRESENTATION_REPRESENTATION (  '', ( #6313 ), #16308 ) ;
#36943 = CARTESIAN_POINT ( 'NONE',  ( -9.642888182262618425E-18, -0.03740157480314960925, -0.1574803149606299191 ) ) ;
#36945 = LINE ( 'NONE', #42106, #39236 ) ;
#36944 = CARTESIAN_POINT ( 'NONE',  ( -0.1574803149606299191, 0.7443365962042343131, -3.523993443072799270 ) ) ;
#36946 = CARTESIAN_POINT ( 'NONE',  ( 0.6971942568897648851, -0.07405724077823297447, 1.820866141678520789 ) ) ;
#36947 = DIRECTION ( 'NONE',  ( 1.000000000000000000, 0.000000000000000000, -1.822029033848725275E-16 ) ) ;
#36948 = CIRCLE ( 'NONE', #16319, 0.09842519685039370636 ) ;
#36949 = DIRECTION ( 'NONE',  ( 0.000000000000000000, 0.000000000000000000, -1.000000000000000000 ) ) ;
#36951 = CARTESIAN_POINT ( 'NONE',  ( -1.094772975963752103E-17, -0.3302165353793074520, -0.1787899950787401882 ) ) ;
#36950 = CARTESIAN_POINT ( 'NONE',  ( 0.1574803149606300301, -0.9453740156405048278, 0.06523048226347956391 ) ) ;
#36952 = CARTESIAN_POINT ( 'NONE',  ( 0.1566053014577290792, 0.1147315712536952914, 0.08204192511013554123 ) ) ;
#36953 = CARTESIAN_POINT ( 'NONE',  ( -0.1264236179284866091, -1.019192913332062966, 0.1264236179284866091 ) ) ;
#36954 = CARTESIAN_POINT ( 'NONE',  ( 0.8759842519685039353, -0.1787899950787401882, 0.2140748030958428971 ) ) ;
#36955 = ADVANCED_FACE ( 'NONE', ( #11315 ), #25928, .T. ) ;
#36956 = CARTESIAN_POINT ( 'NONE',  ( 0.1574803149606299191, 0.1473293504822035527, -0.9532488779249704836 ) ) ;
#36957 = CARTESIAN_POINT ( 'NONE',  ( 0.9500414927467377701, 0.1787899950787401604, 0.5807086613635594752 ) ) ;
#36958 = CARTESIAN_POINT ( 'NONE',  ( -0.6971942568897648851, -0.07405724077823297447, 1.579724409395055318 ) ) ;
#36959 = EDGE_LOOP ( 'NONE', ( #997, #13110, #47044, #7860 ) ) ;
#36960 = AXIS2_PLACEMENT_3D ( 'NONE', #46189, #35431, #6876 ) ;
#36961 = CARTESIAN_POINT ( 'NONE',  ( -0.8759842519685039353, 0.1574803149606299191, 0.8858267716535432879 ) ) ;
#36962 = CARTESIAN_POINT ( 'NONE',  ( 1.054774247047244540, 0.07405724077823318263, 1.249999999946235896 ) ) ;
#36963 = CARTESIAN_POINT ( 'NONE',  ( 0.6971942568897637749, 2.189545951927499583E-17, 1.970964566875370139 ) ) ;
#36964 = CARTESIAN_POINT ( 'NONE',  ( -0.8019270111902717657, 0.1787899950787401604, 1.097440944828127041 ) ) ;
#36965 = EDGE_CURVE ( 'NONE', #41784, #22273, #39502, .T. ) ;
#36966 = DIRECTION ( 'NONE',  ( -1.000000000000000000, 0.000000000000000000, 0.000000000000000000 ) ) ;
#36967 = CARTESIAN_POINT ( 'NONE',  ( 0.8019270111902716547, -0.1787899950787401604, 0.4084645668753704162 ) ) ;
#36968 = CARTESIAN_POINT ( 'NONE',  ( -0.8759842519685039353, 0.1787899950787401882, 0.2682086613635594752 ) ) ;
#36969 = CARTESIAN_POINT ( 'NONE',  ( -0.8759842519685039353, -0.1787899950787401882, 0.7209645668753701386 ) ) ;
#36970 = CARTESIAN_POINT ( 'NONE',  ( 0.9873396505805591694, -0.1113553986120547346, 1.727362204616881947 ) ) ;
#36971 = VERTEX_POINT ( 'NONE', #37171 ) ;
#36972 = CARTESIAN_POINT ( 'NONE',  ( -0.9873396505805591694, 0.1113553986120547346, 0.8710629920184568276 ) ) ;
#36973 = CARTESIAN_POINT ( 'NONE',  ( 1.054774247047244540, -0.07405724077823318263, 1.048228346402928723 ) ) ;
#36974 = CARTESIAN_POINT ( 'NONE',  ( -1.002407869896990045, -0.1264236179284866091, 1.828248031442299082 ) ) ;
#36975 = ORIENTED_EDGE ( 'NONE', *, *, #3757, .F. ) ;
#36976 = CARTESIAN_POINT ( 'NONE',  ( 0.6971942568897648851, -0.07405724077823297447, 1.894685039316315489 ) ) ;
#36977 = AXIS2_PLACEMENT_3D ( 'NONE', #2217, #12325, #5824 ) ;
#36978 = PLANE ( 'NONE',  #8352 ) ;
#36979 = CARTESIAN_POINT ( 'NONE',  ( 0.1787899950787401604, -1.529651527284356494, -0.07405724077823318263 ) ) ;
#36980 = ORIENTED_EDGE ( 'NONE', *, *, #30144, .F. ) ;
#36981 = CARTESIAN_POINT ( 'NONE',  ( 3.284318927891251994E-17, -0.3056102361667090705, 0.1787899950787401882 ) ) ;
#36982 = DIRECTION ( 'NONE',  ( 0.000000000000000000, 0.000000000000000000, -1.000000000000000000 ) ) ;
#36983 = ORIENTED_EDGE ( 'NONE', *, *, #24241, .T. ) ;
#36984 = AXIS2_PLACEMENT_3D ( 'NONE', #39977, #11728, #4030 ) ;
#36985 = CONICAL_SURFACE ( 'NONE', #33190, 0.08090551181102362266, 0.9599310885968742602 ) ;
#36986 = CARTESIAN_POINT ( 'NONE',  ( 0.1476377952755906220, -0.2237541348899639571, -1.272196386806235813 ) ) ;
#36987 = EDGE_CURVE ( 'NONE', #22073, #758, #35909, .T. ) ;
#36988 = CYLINDRICAL_SURFACE ( 'NONE', #13932, 0.1574803149606299191 ) ;
#36989 = CYLINDRICAL_SURFACE ( 'NONE', #10380, 0.1377952755905511029 ) ;
#36990 = CARTESIAN_POINT ( 'NONE',  ( 1.054774247047244096, 0.000000000000000000, 0.2189960629383626012 ) ) ;
#36991 = CARTESIAN_POINT ( 'NONE',  ( 0.07405724077823318263, -1.686023621993479882, 0.1787899950787401604 ) ) ;
#36992 = CARTESIAN_POINT ( 'NONE',  ( -0.07405724077823318263, -1.686023621993479882, 0.1787899950787401604 ) ) ;
#36993 = PRODUCT_CONTEXT ( 'NONE', #35549, 'mechanical' ) ;
#36994 = CARTESIAN_POINT ( 'NONE',  ( 0.9873396505805591694, -0.1113553986120547346, 1.343503937007874072 ) ) ;
#36995 = VERTEX_POINT ( 'NONE', #30724 ) ;
#36996 = CARTESIAN_POINT ( 'NONE',  ( -0.7495606340400177148, 0.1264236179284866091, 0.5142716534895434011 ) ) ;
#36997 = CARTESIAN_POINT ( 'NONE',  ( -0.1797182628040039087, -1.415890266275959375, 0.07444174185955065859 ) ) ;
#36998 = FACE_BOUND ( 'NONE', #8096, .T. ) ;
#36999 = CARTESIAN_POINT ( 'NONE',  ( 1.054774247047244540, -0.07405724077823318263, 1.363188976324188895 ) ) ;
#37000 = CARTESIAN_POINT ( 'NONE',  ( 1.002407869896990045, 0.1264236179284866091, 1.680610236166708793 ) ) ;
#37001 = CARTESIAN_POINT ( 'NONE',  ( 1.033464566929134687, 0.06523048226347956391, 0.1304133858267717272 ) ) ;
#37002 = DIRECTION ( 'NONE',  ( 0.000000000000000000, 0.000000000000000000, -1.000000000000000000 ) ) ;
#37003 = CARTESIAN_POINT ( 'NONE',  ( 0.3246033735368759610, 0.09842519685039370636, 0.000000000000000000 ) ) ;
#37005 = CARTESIAN_POINT ( 'NONE',  ( -1.033464566929134687, -0.06523048226347956391, 1.936515748031494510 ) ) ;
#37004 = CARTESIAN_POINT ( 'NONE',  ( 0.1574803149606300301, -0.8272637794200329298, 0.06523048226347956391 ) ) ;
#37006 = CARTESIAN_POINT ( 'NONE',  ( 0.7646288533564489232, -0.1113553986120547346, 0.5364173227271189504 ) ) ;
#37007 = CARTESIAN_POINT ( 'NONE',  ( 0.9500414927467378812, 0.1787899950787401604, 0.3444881889226146243 ) ) ;
#37008 = CARTESIAN_POINT ( 'NONE',  ( 0.7331235663779919198, -0.08921757803951906041, 0.03937007923342519117 ) ) ;
#37009 = EDGE_CURVE ( 'NONE', #1825, #9117, #44816, .T. ) ;
#37011 = DIRECTION ( 'NONE',  ( -1.000000000000000000, 0.000000000000000000, 0.000000000000000000 ) ) ;
#37010 = CARTESIAN_POINT ( 'NONE',  ( 0.8019270111902716547, -0.1787899950787401604, 1.230314960576158967 ) ) ;
#37012 = CARTESIAN_POINT ( 'NONE',  ( -0.7185039370078778465, -0.06523048226348396317, 1.911909448711369697 ) ) ;
#37013 = DIRECTION ( 'NONE',  ( 0.000000000000000000, 0.6156614753256598460, 0.7880107536067207930 ) ) ;
#37014 = CARTESIAN_POINT ( 'NONE',  ( -0.6971942568897648851, -0.07405724077823297447, 1.225393700733637514 ) ) ;
#37015 = CARTESIAN_POINT ( 'NONE',  ( 0.8107537697050253289, -0.1574803149606297803, 0.6176181101286932762 ) ) ;
#37016 = VERTEX_POINT ( 'NONE', #4315 ) ;
#37017 = ( LENGTH_UNIT ( ) NAMED_UNIT ( * ) SI_UNIT ( $, .METRE. ) ) ;
#37018 = CARTESIAN_POINT ( 'NONE',  ( 0.1574803149606299191, -0.04724409448818897572, -1.928577636452523993E-17 ) ) ;
#37019 = ORIENTED_EDGE ( 'NONE', *, *, #17859, .T. ) ;
#37020 = CARTESIAN_POINT ( 'NONE',  ( 3.301370929368692659E-17, -0.03055562060666760019, 0.1797182628040039365 ) ) ;
#37021 = VECTOR ( 'NONE', #11479, 39.37007874015748143 ) ;
#37022 = CARTESIAN_POINT ( 'NONE',  ( -0.7646288533564489232, 0.1113553986120547346, 0.4872047243019220208 ) ) ;
#37023 = CARTESIAN_POINT ( 'NONE',  ( -1.033464566929133799, 0.000000000000000000, 1.584645669291338654 ) ) ;
#37024 = CARTESIAN_POINT ( 'NONE',  ( 0.6971942568897648851, -0.07405724077823297447, 1.540354330654897685 ) ) ;
#37025 = EDGE_CURVE ( 'NONE', #7448, #12067, #15385, .T. ) ;
#37027 = CARTESIAN_POINT ( 'NONE',  ( 0.7646288533564489232, 0.1113553986120547346, 1.678149606299212726 ) ) ;
#37026 = CARTESIAN_POINT ( 'NONE',  ( -0.7185039370078739607, 1.928577636452523993E-17, 1.840551181102362266 ) ) ;
#37028 = CARTESIAN_POINT ( 'NONE',  ( 0.07405724077823318263, -0.1309055117572600901, -0.1787899950787401604 ) ) ;
#37029 = ORIENTED_EDGE ( 'NONE', *, *, #44927, .T. ) ;
#37030 = CARTESIAN_POINT ( 'NONE',  ( -1.033464566929133799, 0.000000000000000000, 0.3937007872940476716 ) ) ;
#37031 = CARTESIAN_POINT ( 'NONE',  ( 0.1854358583631518231, -0.08093302715450646778, -0.1783713581459814845 ) ) ;
#37032 = ORIENTED_EDGE ( 'NONE', *, *, #1900, .T. ) ;
#37033 = CARTESIAN_POINT ( 'NONE',  ( 1.002407869896990045, -0.1264236179284866091, 0.8095472440407244230 ) ) ;
#37034 = CARTESIAN_POINT ( 'NONE',  ( -0.8019270111902716547, 0.1787899950787401604, 1.491141732229701145 ) ) ;
#37035 = CARTESIAN_POINT ( 'NONE',  ( 2.892866454678787531E-17, 0.03149606309965303358, 0.1574803149606299191 ) ) ;
#37036 = CARTESIAN_POINT ( 'NONE',  ( -0.8759842519685039353, 0.1787899950787401882, 1.336122047190330786 ) ) ;
#37037 = ORIENTED_EDGE ( 'NONE', *, *, #21530, .F. ) ;
#37038 = ( BOUNDED_CURVE ( )  B_SPLINE_CURVE ( 2, ( #25834, #8073, #37544, #165, #15771, #36843, #11451, #29702, #4225 ),
 .UNSPECIFIED., .F., .F. ) 
 B_SPLINE_CURVE_WITH_KNOTS ( ( 3, 2, 2, 2, 3 ),
 ( 0.2500000000000000000, 0.2525000000000000022, 0.2550000000000000044, 0.2575000000000000067, 0.2600000000000000089 ),
 .UNSPECIFIED. ) 
 CURVE ( )  GEOMETRIC_REPRESENTATION_ITEM ( )  RATIONAL_B_SPLINE_CURVE ( ( 1.000000000000000000, 0.9238795325112869605, 1.000000000000000000, 0.9238795325112869605, 1.000000000000000000, 0.9238795325112869605, 1.000000000000000000, 0.9238795325112869605, 1.000000000000000000 ) ) 
 REPRESENTATION_ITEM ( '' )  ) ;
#37039 = CARTESIAN_POINT ( 'NONE',  ( -0.6971942568897626646, 0.07405724077823318263, 0.3592519684501735977 ) ) ;
#37040 = DIRECTION ( 'NONE',  ( -0.000000000000000000, 1.000000000000000000, -3.995705278811693553E-31 ) ) ;
#37041 = CARTESIAN_POINT ( 'NONE',  ( 0.1787899950787401882, -0.9415609761032539549, -2.189545951927503898E-17 ) ) ;
#37042 = ORIENTED_EDGE ( 'NONE', *, *, #35690, .F. ) ;
#37043 = CARTESIAN_POINT ( 'NONE',  ( -0.7185039370078739607, 1.928577636452523993E-17, 0.8464566928058583350 ) ) ;
#37044 = ORIENTED_EDGE ( 'NONE', *, *, #42296, .T. ) ;
#37045 = EDGE_CURVE ( 'NONE', #46402, #25630, #16101, .T. ) ;
#37046 = MANIFOLD_SOLID_BREP ( 'Side Bracket', #41538 ) ;
#37047 = CARTESIAN_POINT ( 'NONE',  ( -0.005244590715619158044, 1.099487083487566297, -0.04739565599251693157 ) ) ;
#37048 = ( BOUNDED_CURVE ( )  B_SPLINE_CURVE ( 2, ( #12763, #44089, #47222, #33108, #10338, #39768, #36678, #3373, #14878 ),
 .UNSPECIFIED., .F., .F. ) 
 B_SPLINE_CURVE_WITH_KNOTS ( ( 3, 2, 2, 2, 3 ),
 ( 0.1199999999999999956, 0.1224999999999999978, 0.1250000000000000000, 0.1275000000000000022, 0.1300000000000000044 ),
 .UNSPECIFIED. ) 
 CURVE ( )  GEOMETRIC_REPRESENTATION_ITEM ( )  RATIONAL_B_SPLINE_CURVE ( ( 1.000000000000000000, 0.9238795325112869605, 1.000000000000000000, 0.9238795325112869605, 1.000000000000000000, 0.9238795325112869605, 1.000000000000000000, 0.9238795325112869605, 1.000000000000000000 ) ) 
 REPRESENTATION_ITEM ( '' )  ) ;
#37049 = CARTESIAN_POINT ( 'NONE',  ( -0.8759842519685039353, -0.1787899950787401882, 0.05659448813521291560 ) ) ;
#37050 = CARTESIAN_POINT ( 'NONE',  ( -0.9873396505805591694, 0.1113553986120547346, 0.9596456692913386544 ) ) ;
#37051 = CARTESIAN_POINT ( 'NONE',  ( -0.07444174185955065859, -1.017268219031864263, 0.1797182628040039087 ) ) ;
#37052 = CARTESIAN_POINT ( 'NONE',  ( -0.9873396505805591694, 0.1113553986120547346, 0.3986220471365669038 ) ) ;
#37053 = CARTESIAN_POINT ( 'NONE',  ( -1.033464566929133799, 0.000000000000000000, 1.535433070758614127 ) ) ;
#37054 = AXIS2_PLACEMENT_3D ( 'NONE', #18885, #14839, #32602 ) ;
#37055 = EDGE_CURVE ( 'NONE', #21725, #44147, #43081, .T. ) ;
#37056 = CARTESIAN_POINT ( 'NONE',  ( 0.6971942568897626646, -0.07405724077823297447, 0.9153543306548987957 ) ) ;
#37057 = CARTESIAN_POINT ( 'NONE',  ( -0.7185039370078739607, 1.928577636452523993E-17, 1.673228346349165285 ) ) ;
#37058 = CARTESIAN_POINT ( 'NONE',  ( 0.8759842519685039353, 0.1574803149606299191, 1.437007874015747921 ) ) ;
#37060 = CARTESIAN_POINT ( 'NONE',  ( 1.033464566929133799, 0.000000000000000000, 0.9547244094488189781 ) ) ;
#37059 = CARTESIAN_POINT ( 'NONE',  ( 0.7099245333373607192, -0.01040492030921760271, 1.983451210857912761 ) ) ;
#37061 = CARTESIAN_POINT ( 'NONE',  ( 0.7185039370078746268, 0.06523048226347956391, 0.3321850392625518844 ) ) ;
#37062 = EDGE_CURVE ( 'NONE', #20228, #44561, #34393, .T. ) ;
#37064 = CARTESIAN_POINT ( 'NONE',  ( 0.000000000000000000, 0.000000000000000000, 0.000000000000000000 ) ) ;
#37063 = CARTESIAN_POINT ( 'NONE',  ( 0.6971942568897637749, 2.189545951927499583E-17, 0.7898622046706456068 ) ) ;
#37065 = CARTESIAN_POINT ( 'NONE',  ( 0.07405724077823318263, -0.8395669290800948925, -0.1787899950787401604 ) ) ;
#37066 = ORIENTED_EDGE ( 'NONE', *, *, #44107, .T. ) ;
#37067 = CYLINDRICAL_SURFACE ( 'NONE', #8359, 0.1673228346456687721 ) ;
#37068 = CARTESIAN_POINT ( 'NONE',  ( 0.7495606340400177148, -0.1264236179284866091, 1.188484251914740275 ) ) ;
#37069 = EDGE_CURVE ( 'NONE', #9873, #16859, #3540, .T. ) ;
#37070 = LINE ( 'NONE', #4946, #10413 ) ;
#37071 = CARTESIAN_POINT ( 'NONE',  ( -0.1574803149606297803, -1.639271653543306506, 0.06523048226347956391 ) ) ;
#37072 = CARTESIAN_POINT ( 'NONE',  ( 0.6195511811023636239, 1.354170115732554747, -0.4197102375732078561 ) ) ;
#37073 = ORIENTED_EDGE ( 'NONE', *, *, #21081, .T. ) ;
#37074 = DIRECTION ( 'NONE',  ( 0.000000000000000000, 0.2126700594527834443, -0.9771240687918547607 ) ) ;
#37075 = CARTESIAN_POINT ( 'NONE',  ( -0.9500414927467378812, -0.1787899950787401604, 0.2509842519147403861 ) ) ;
#37076 = EDGE_LOOP ( 'NONE', ( #24748, #43777 ) ) ;
#37077 = CARTESIAN_POINT ( 'NONE',  ( 1.054774247047244096, 0.000000000000000000, 1.993110236166708793 ) ) ;
#37078 = CARTESIAN_POINT ( 'NONE',  ( 0.1113553986120547346, -0.3080708660342051375, -0.1113553986120547346 ) ) ;
#37079 = VECTOR ( 'NONE', #6289, 39.37007874015748143 ) ;
#37081 = CARTESIAN_POINT ( 'NONE',  ( 0.9412147342319837628, -0.1574803149606297803, 0.3469488187901108023 ) ) ;
#37080 = VECTOR ( 'NONE', #37469, 39.37007874015748854 ) ;
#37082 = CARTESIAN_POINT ( 'NONE',  ( -0.9500414927467378812, -0.1787899950787401604, 1.628937007820252303 ) ) ;
#37083 = CARTESIAN_POINT ( 'NONE',  ( -1.054774247047244540, -0.07405724077823318263, 0.4576771653005669016 ) ) ;
#37084 = PLANE ( 'NONE',  #15352 ) ;
#37085 = CARTESIAN_POINT ( 'NONE',  ( 0.000000000000000000, 0.000000000000000000, 2.731847993664263218E-16 ) ) ;
#37086 = CARTESIAN_POINT ( 'NONE',  ( 0.000000000000000000, 0.000000000000000000, -0.2610569382242185488 ) ) ;
#37087 = CARTESIAN_POINT ( 'NONE',  ( 0.8019270111902717657, -0.1787899950787401604, 0.08858267711159097113 ) ) ;
#37088 = DIRECTION ( 'NONE',  ( 0.000000000000000000, -1.000000000000000000, 0.000000000000000000 ) ) ;
#37089 = CARTESIAN_POINT ( 'NONE',  ( -0.1787899950787401604, -0.4469743619300260984, 0.07405724077823318263 ) ) ;
#37090 = CARTESIAN_POINT ( 'NONE',  ( -0.2150476131984622175, -0.08955971513628484260, -0.1130403609974334617 ) ) ;
#37091 = CYLINDRICAL_SURFACE ( 'NONE', #37102, 0.009842519685039378616 ) ;
#37092 = CARTESIAN_POINT ( 'NONE',  ( 0.2559054078461202586, -0.02857456808055104658, -0.02996975140571832980 ) ) ;
#37093 = CARTESIAN_POINT ( 'NONE',  ( -0.8759842519685039353, 0.1787899950787401882, 0.3863188975840318173 ) ) ;
#37094 = ORIENTED_EDGE ( 'NONE', *, *, #34319, .F. ) ;
#37095 = CARTESIAN_POINT ( 'NONE',  ( -1.054774247047244096, 0.000000000000000000, 1.444389763725763665 ) ) ;
#37096 = ORIENTED_EDGE ( 'NONE', *, *, #9522, .F. ) ;
#37097 = ADVANCED_FACE ( 'NONE', ( #20373 ), #40776, .T. ) ;
#37098 = CARTESIAN_POINT ( 'NONE',  ( 0.1264236179284866091, -1.329232283410803239, 0.1264236179284866091 ) ) ;
#37099 = CARTESIAN_POINT ( 'NONE',  ( 0.1787899950787401604, -1.558070866087969630, 0.07405724077823318263 ) ) ;
#37100 = ( NAMED_UNIT ( * ) PLANE_ANGLE_UNIT ( ) SI_UNIT ( $, .RADIAN. ) ) ;
#37101 = DIRECTION ( 'NONE',  ( 0.001755765868204999490, -0.6638367987156507111, 0.7478754053698868365 ) ) ;
#37102 = AXIS2_PLACEMENT_3D ( 'NONE', #39966, #44039, #32589 ) ;
#37103 = AXIS2_PLACEMENT_3D ( 'NONE', #6729, #25447, #21840 ) ;
#37104 = FACE_OUTER_BOUND ( 'NONE', #26215, .T. ) ;
#37105 = CARTESIAN_POINT ( 'NONE',  ( -0.9412147342319837628, 0.1574803149606300301, 1.031003936900347639 ) ) ;
#37106 = EDGE_CURVE ( 'NONE', #34560, #7415, #2163, .T. ) ;
#37107 = CARTESIAN_POINT ( 'NONE',  ( 1.002407869896990045, -0.1264236179284866091, 0.5339566928596221063 ) ) ;
#37108 = DIRECTION ( 'NONE',  ( 0.000000000000000000, 0.000000000000000000, 1.000000000000000000 ) ) ;
#37109 = CARTESIAN_POINT ( 'NONE',  ( 0.1113553986120547346, -0.2883858267716535306, 0.1113553986120547346 ) ) ;
#37110 = VECTOR ( 'NONE', #44163, 39.37007874015748143 ) ;
#37111 = CIRCLE ( 'NONE', #11106, 0.2471922904502826812 ) ;
#37112 = CARTESIAN_POINT ( 'NONE',  ( 1.033464566929134687, 0.06523048226347956391, 1.970964566821606034 ) ) ;
#37113 = VERTEX_POINT ( 'NONE', #28296 ) ;
#37114 = CARTESIAN_POINT ( 'NONE',  ( -0.1174123764687494409, -0.08986489419234251763, -0.1348499909742253422 ) ) ;
#37115 = CARTESIAN_POINT ( 'NONE',  ( -0.8019270111902716547, -0.1787899950787401604, 0.9990157479777320715 ) ) ;
#37116 = CARTESIAN_POINT ( 'NONE',  ( 0.9412147342319837628, -0.1574803149606297803, 0.9079724409448818312 ) ) ;
#37117 = DIRECTION ( 'NONE',  ( 0.5735764363510447161, 0.8191520442889925757, 0.000000000000000000 ) ) ;
#37118 = CARTESIAN_POINT ( 'NONE',  ( -0.1523463298590899406, -0.08956081936279648714, 0.06373561487467800657 ) ) ;
#37119 = ORIENTED_EDGE ( 'NONE', *, *, #10681, .T. ) ;
#37120 = CARTESIAN_POINT ( 'NONE',  ( 0.1564632978426661603, 0.02849706681272137429, -0.1403868342279277759 ) ) ;
#37121 = CARTESIAN_POINT ( 'NONE',  ( -0.2610014219173109051, 0.1673399808196281979, 0.8651424297200356328 ) ) ;
#37122 = VERTEX_POINT ( 'NONE', #31191 ) ;
#37123 = CARTESIAN_POINT ( 'NONE',  ( -1.033464566929133799, 0.000000000000000000, 1.309055118110236338 ) ) ;
#37124 = CARTESIAN_POINT ( 'NONE',  ( 0.7185039370078739607, 1.928577636452523993E-17, 1.368110236220472675 ) ) ;
#37125 = CARTESIAN_POINT ( 'NONE',  ( -0.1264236179284866091, -1.491633858213953001, 0.1264236179284866091 ) ) ;
#37126 = CARTESIAN_POINT ( 'NONE',  ( -0.1574803149606299191, -1.287401574803149540, 0.000000000000000000 ) ) ;
#37127 = CARTESIAN_POINT ( 'NONE',  ( 0.8107537697050253289, -0.1574803149606297803, 1.129429133750740277 ) ) ;
#37128 = CARTESIAN_POINT ( 'NONE',  ( 0.6195511811023588500, -5.463695987328330208E-16, -1.186023622047243986 ) ) ;
#37129 = EDGE_CURVE ( 'NONE', #4590, #47236, #40778, .T. ) ;
#37130 = EDGE_LOOP ( 'NONE', ( #16365, #39423, #43735, #8876 ) ) ;
#37131 = EDGE_LOOP ( 'NONE', ( #44415, #15192, #10320, #35844 ) ) ;
#37132 = CARTESIAN_POINT ( 'NONE',  ( -1.002407869896990045, -0.1264236179284866091, 1.754429133804503715 ) ) ;
#37133 = CARTESIAN_POINT ( 'NONE',  ( 0.7495606340400177148, -0.1264236179284866091, 1.665846456639149764 ) ) ;
#37134 = CARTESIAN_POINT ( 'NONE',  ( 0.1113553986120547346, -1.302165354223181026, 0.1113553986120547346 ) ) ;
#37135 = CARTESIAN_POINT ( 'NONE',  ( -1.054774247047244096, 0.000000000000000000, 0.7357283464029290565 ) ) ;
#37136 = CARTESIAN_POINT ( 'NONE',  ( 0.7185039370078739607, 0.000000000000000000, 4.498031496062992574 ) ) ;
#37137 = CARTESIAN_POINT ( 'NONE',  ( 0.7495606340400177148, -0.1264236179284866091, 0.3272637794737956463 ) ) ;
#37138 = DIRECTION ( 'NONE',  ( -1.000000000000000000, 0.000000000000000000, 0.000000000000000000 ) ) ;
#37139 = CARTESIAN_POINT ( 'NONE',  ( -1.054774247047244540, 0.07405724077823318263, 1.245078740103716886 ) ) ;
#37140 = CARTESIAN_POINT ( 'NONE',  ( -0.8759842519685039353, -0.1787899950787401882, 0.7997047243556849594 ) ) ;
#37141 = CARTESIAN_POINT ( 'NONE',  ( -0.8759842519685039353, 0.1787899950787401882, 0.9374999999462362288 ) ) ;
#37142 = CARTESIAN_POINT ( 'NONE',  ( -9.642888182262618425E-18, -0.06692913375074074911, -0.1574803149606299191 ) ) ;
#37143 = CARTESIAN_POINT ( 'NONE',  ( 0.01993724539804073159, 0.05212746764708663105, 0.2739222968686834125 ) ) ;
#37144 = CARTESIAN_POINT ( 'NONE',  ( -0.6971942568897648851, 0.07405724077823318263, 1.658464566875369472 ) ) ;
#37145 = CARTESIAN_POINT ( 'NONE',  ( -1.033464566929134687, 0.06523048226347956391, 1.931594488081448180 ) ) ;
#37146 = ORIENTED_EDGE ( 'NONE', *, *, #13280, .F. ) ;
#37147 = AXIS2_PLACEMENT_3D ( 'NONE', #44327, #19173, #26395 ) ;
#37148 = CARTESIAN_POINT ( 'NONE',  ( -1.033464566929134687, 0.06523048226347956391, 1.626476377952756458 ) ) ;
#37149 = CARTESIAN_POINT ( 'NONE',  ( 0.1721082586868755704, -0.4313654725386900091, -0.9749915214042050859 ) ) ;
#37150 = CARTESIAN_POINT ( 'NONE',  ( 0.9500414927467377701, 0.1787899950787401604, 1.569881889710015299 ) ) ;
#37151 = CARTESIAN_POINT ( 'NONE',  ( -0.09426105192651733355, -0.09851383153318916952, 0.1330962383627474210 ) ) ;
#37152 = DIRECTION ( 'NONE',  ( -0.000000000000000000, 1.000000000000000000, -0.000000000000000000 ) ) ;
#37153 = AXIS2_PLACEMENT_3D ( 'NONE', #21608, #32890, #24969 ) ;
#37154 = CIRCLE ( 'NONE', #17247, 0.1624015748031501782 ) ;
#37155 = ORIENTED_EDGE ( 'NONE', *, *, #27399, .F. ) ;
#37156 = ORIENTED_EDGE ( 'NONE', *, *, #43215, .T. ) ;
#37157 = ORIENTED_EDGE ( 'NONE', *, *, #46352, .T. ) ;
#37158 = EDGE_CURVE ( 'NONE', #33098, #7386, #30118, .T. ) ;
#37159 = CARTESIAN_POINT ( 'NONE',  ( -0.1787899950787401604, -0.9084645668753701386, 0.07405724077823318263 ) ) ;
#37160 = ( BOUNDED_CURVE ( )  B_SPLINE_CURVE ( 2, ( #47307, #40555, #29623, #25971, #40092, #36757, #7287, #3914, #43454 ),
 .UNSPECIFIED., .F., .T. ) 
 B_SPLINE_CURVE_WITH_KNOTS ( ( 3, 2, 2, 2, 3 ),
 ( 0.6800000000000000488, 0.6824999999999999956, 0.6850000000000000533, 0.6875000000000000000, 0.6899999999999999467 ),
 .UNSPECIFIED. ) 
 CURVE ( )  GEOMETRIC_REPRESENTATION_ITEM ( )  RATIONAL_B_SPLINE_CURVE ( ( 1.000000000000000000, 0.9238795325112869605, 1.000000000000000000, 0.9238795325112869605, 1.000000000000000000, 0.9238795325112869605, 1.000000000000000000, 0.9238795325112799661, 1.000000000000000000 ) ) 
 REPRESENTATION_ITEM ( '' )  ) ;
#37161 = EDGE_CURVE ( 'NONE', #8495, #7550, #33960, .T. ) ;
#37162 = CARTESIAN_POINT ( 'NONE',  ( -0.1787899950787401882, -1.142224409395055096, 0.000000000000000000 ) ) ;
#37163 = CARTESIAN_POINT ( 'NONE',  ( 1.002407869896990045, -0.1264236179284866091, 1.788877952702141672 ) ) ;
#37164 = CARTESIAN_POINT ( 'NONE',  ( 0.1797182628040039087, -0.3725831796617855018, -0.07444174185955065859 ) ) ;
#37165 = ADVANCED_FACE ( 'NONE', ( #13439 ), #9842, .T. ) ;
#37166 = CARTESIAN_POINT ( 'NONE',  ( 0.1574803149606300301, 0.1471456692913385988, 0.06523048226347956391 ) ) ;
#37167 = PRODUCT_DEFINITION_SHAPE ( 'NONE', 'NONE',  #47477 ) ;
#37168 = VECTOR ( 'NONE', #31852, 39.37007874015748143 ) ;
#37169 = EDGE_CURVE ( 'NONE', #29186, #27577, #35716, .T. ) ;
#37170 = CARTESIAN_POINT ( 'NONE',  ( 0.7495606340400177148, 0.1264236179284866091, 0.7062007873478109987 ) ) ;
#37172 = CARTESIAN_POINT ( 'NONE',  ( 0.9873396505805591694, -0.1113553986120547346, 1.136811023514519681 ) ) ;
#37171 = CARTESIAN_POINT ( 'NONE',  ( -0.3161444924769509779, 2.177585298233989164, -4.122948637049707266 ) ) ;
#37174 = DIRECTION ( 'NONE',  ( 1.822029033848725028E-16, 0.000000000000000000, 1.000000000000000000 ) ) ;
#37173 = FACE_BOUND ( 'NONE', #6979, .T. ) ;
#37175 = CARTESIAN_POINT ( 'NONE',  ( -0.7185039370078739607, 1.928577636452523993E-17, 0.05905511800270921846 ) ) ;
#37176 = CARTESIAN_POINT ( 'NONE',  ( 0.8019270111902717657, -0.1787899950787401604, 1.865157480261195877 ) ) ;
#37177 = CARTESIAN_POINT ( 'NONE',  ( 1.033464566929133799, 0.000000000000000000, 0.1181102361129454797 ) ) ;
#37178 = CIRCLE ( 'NONE', #30361, 0.09842519685039370636 ) ;
#37179 = CARTESIAN_POINT ( 'NONE',  ( 0.9412147342319837628, 0.1574803149606300301, 0.1353346456692913757 ) ) ;
#37180 = DIRECTION ( 'NONE',  ( -1.000000000000000000, 0.000000000000000000, 0.000000000000000000 ) ) ;
#37181 = CARTESIAN_POINT ( 'NONE',  ( -0.07405724077823318263, -0.3129921259304885850, 0.1787899950787401604 ) ) ;
#37182 = CARTESIAN_POINT ( 'NONE',  ( 0.1631207519397589456, 0.1587913448376443715, 0.006047451551359922690 ) ) ;
#37183 = CARTESIAN_POINT ( 'NONE',  ( 0.1787899950787401604, -1.238188976324190005, -0.07405724077823318263 ) ) ;
#37184 = CARTESIAN_POINT ( 'NONE',  ( 0.8759842519685039353, 0.1787899950787401882, 0.1943897637257641919 ) ) ;
#37185 = CARTESIAN_POINT ( 'NONE',  ( 0.1644020957507537628, 0.08115590401245532937, -0.1405661490837558925 ) ) ;
#37186 = CARTESIAN_POINT ( 'NONE',  ( -0.8019270111902717657, 0.1787899950787401604, 1.766732283410803461 ) ) ;
#37187 = EDGE_LOOP ( 'NONE', ( #11125, #14158, #9233, #39781, #35090, #33804 ) ) ;
#37188 = CARTESIAN_POINT ( 'NONE',  ( -0.8019270111902717657, 0.1787899950787401604, 1.338582677111590069 ) ) ;
#37189 = DIRECTION ( 'NONE',  ( 1.822029033848725028E-16, 0.000000000000000000, 1.000000000000000000 ) ) ;
#37190 = CARTESIAN_POINT ( 'NONE',  ( 0.9500414927467378812, -0.1787899950787401604, 1.279527559001355286 ) ) ;
#37191 = CARTESIAN_POINT ( 'NONE',  ( -0.06523048226347956391, -1.191437007766489531, 0.1574803149606297803 ) ) ;
#37192 = CARTESIAN_POINT ( 'NONE',  ( -0.7495606340400177148, 0.1264236179284866091, 1.021161417269070837 ) ) ;
#37193 = CARTESIAN_POINT ( 'NONE',  ( -0.07175194912964910632, -0.09842519594091171664, -0.1637606677113847553 ) ) ;
#37194 = DIRECTION ( 'NONE',  ( 1.822029033848725028E-16, 0.000000000000000000, 1.000000000000000000 ) ) ;
#37195 = CARTESIAN_POINT ( 'NONE',  ( 0.6971942568897648851, -0.07405724077823297447, 0.4035433070328507954 ) ) ;
#37196 = CARTESIAN_POINT ( 'NONE',  ( -1.054774247047244540, -0.07405724077823318263, 0.4133858267178901480 ) ) ;
#37197 = CARTESIAN_POINT ( 'NONE',  ( 0.8107537697050253289, 0.1574803149606300301, 1.665846456585386548 ) ) ;
#37198 = VERTEX_POINT ( 'NONE', #10317 ) ;
#37199 = VERTEX_POINT ( 'NONE', #25647 ) ;
#37200 = CARTESIAN_POINT ( 'NONE',  ( 0.3302522695077432791, -0.09842519685039370636, 0.000000000000000000 ) ) ;
#37201 = CARTESIAN_POINT ( 'NONE',  ( 1.002407869896990045, -0.1264236179284866091, 0.8882874015210394658 ) ) ;
#37202 = CARTESIAN_POINT ( 'NONE',  ( -1.033464566929134687, -0.06523048226347956391, 0.1648622047244094890 ) ) ;
#37203 = CARTESIAN_POINT ( 'NONE',  ( 1.002407869896990045, -0.1264236179284866091, 1.006397637741511808 ) ) ;
#37204 = CARTESIAN_POINT ( 'NONE',  ( -0.7495606340400177148, -0.1264236179284866091, 1.936515747977732405 ) ) ;
#37205 = ORIENTED_EDGE ( 'NONE', *, *, #21368, .T. ) ;
#37206 = AXIS2_PLACEMENT_3D ( 'NONE', #29344, #4558, #30033 ) ;
#37207 = CARTESIAN_POINT ( 'NONE',  ( 0.8019270111902717657, 0.1787899950787401604, 1.884842519631275026 ) ) ;
#37208 = CARTESIAN_POINT ( 'NONE',  ( -0.8107537697050234415, -0.1574803149606297803, 0.3125000000000000000 ) ) ;
#37209 = CARTESIAN_POINT ( 'NONE',  ( 0.7185039370078746268, -0.06523048226347956391, 0.3075787401574803792 ) ) ;
#37210 = CARTESIAN_POINT ( 'NONE',  ( -0.1787899950787401604, -1.509966487914277788, 0.07405724077823318263 ) ) ;
#37211 = ORIENTED_EDGE ( 'NONE', *, *, #40264, .F. ) ;
#37212 = CARTESIAN_POINT ( 'NONE',  ( 3.284318927891251994E-17, -0.3843503936470239468, 0.1787899950787401882 ) ) ;
#37213 = ORIENTED_EDGE ( 'NONE', *, *, #28604, .F. ) ;
#37214 = CARTESIAN_POINT ( 'NONE',  ( 0.8019270111902717657, -0.1787899950787401604, 1.190944881836001112 ) ) ;
#37215 = CARTESIAN_POINT ( 'NONE',  ( 0.000000000000000000, -0.09842519685039370636, 0.1574803149606299191 ) ) ;
#37216 = CARTESIAN_POINT ( 'NONE',  ( 0.8759842519685039353, -0.1574803149606299191, 0.7381889762704251234 ) ) ;
#37217 = EDGE_CURVE ( 'NONE', #1825, #6014, #3587, .T. ) ;
#37218 = LINE ( 'NONE', #19476, #47063 ) ;
#37219 = CARTESIAN_POINT ( 'NONE',  ( 1.054774247047244096, 0.000000000000000000, 1.518208661363559031 ) ) ;
#37220 = CARTESIAN_POINT ( 'NONE',  ( 0.8759842519685039353, 0.1787899950787401882, 0.1500984251430870220 ) ) ;
#37221 = ADVANCED_FACE ( 'NONE', ( #3813, #21077 ), #7412, .F. ) ;
#37222 = CARTESIAN_POINT ( 'NONE',  ( -0.1787899950787401604, -1.813976377898992354, 0.07405724077823318263 ) ) ;
#37223 = CARTESIAN_POINT ( 'NONE',  ( -0.1787899950787401604, -1.617125984198204414, -0.07405724077823318263 ) ) ;
#37224 = PRODUCT_CONTEXT ( 'NONE', #32771, 'mechanical' ) ;
#37225 = CARTESIAN_POINT ( 'NONE',  ( 0.8759842519685039353, -0.1574803149606299191, 1.338582677165354395 ) ) ;
#37226 = ADVANCED_FACE ( 'NONE', ( #36655 ), #32848, .F. ) ;
#37227 = CARTESIAN_POINT ( 'NONE',  ( -0.8019270111902716547, -0.1787899950787401604, 0.6840551180564720113 ) ) ;
#37229 = SURFACE_STYLE_USAGE ( .BOTH. , #15204 ) ;
#37228 = CARTESIAN_POINT ( 'NONE',  ( 2.892866454678787531E-17, -0.8051181102362204856, 0.1574803149606299191 ) ) ;
#37230 = CARTESIAN_POINT ( 'NONE',  ( 0.1270800023317771588, -1.442957195409817039, 0.1270800023317771588 ) ) ;
#37231 = CARTESIAN_POINT ( 'NONE',  ( 1.033464566929133799, 1.928577636452524610E-17, 4.498031496062992574 ) ) ;
#37232 = CARTESIAN_POINT ( 'NONE',  ( 0.000000000000000000, 0.000000000000000000, -0.04012007874015743186 ) ) ;
#37233 = CARTESIAN_POINT ( 'NONE',  ( 0.7495606340400177148, -0.1264236179284866091, 1.311515747977732405 ) ) ;
#37234 = CARTESIAN_POINT ( 'NONE',  ( 1.054774247047244096, 0.000000000000000000, 1.754429133804503715 ) ) ;
#37235 = DIRECTION ( 'NONE',  ( 1.000000000000000000, -3.469446951953625233E-15, -0.000000000000000000 ) ) ;
#37236 = CARTESIAN_POINT ( 'NONE',  ( 1.033464566929133799, 0.000000000000000000, 0.1181102361129454797 ) ) ;
#37237 = DIRECTION ( 'NONE',  ( 1.000000000000000000, 0.000000000000000000, -1.822029033848725275E-16 ) ) ;
#37238 = FACE_OUTER_BOUND ( 'NONE', #29110, .T. ) ;
#37240 = FACE_OUTER_BOUND ( 'NONE', #46939, .T. ) ;
#37239 = CARTESIAN_POINT ( 'NONE',  ( 0.7495606340400177148, -0.1264236179284866091, 1.227854330654897685 ) ) ;
#37241 = CARTESIAN_POINT ( 'NONE',  ( 0.9412147342319837628, -0.1574803149606297803, 0.7012795274515276622 ) ) ;
#37242 = VERTEX_POINT ( 'NONE', #18432 ) ;
#37243 = SURFACE_STYLE_FILL_AREA ( #33689 ) ;
#37244 = CARTESIAN_POINT ( 'NONE',  ( -0.1594773935179923108, -0.4410959923581745379, -0.9673892061308028145 ) ) ;
#37245 = VERTEX_POINT ( 'NONE', #24928 ) ;
#37246 = CARTESIAN_POINT ( 'NONE',  ( -0.1797182628040039087, -0.07730758911060468808, 0.07444174185955065859 ) ) ;
#37247 = DIRECTION ( 'NONE',  ( -1.000000000000000000, -0.000000000000000000, -0.000000000000000000 ) ) ;
#37249 = CARTESIAN_POINT ( 'NONE',  ( -0.1787899950787401604, -1.223425196796630532, 0.07405724077823318263 ) ) ;
#37248 = CARTESIAN_POINT ( 'NONE',  ( -0.1113553986120547346, -1.046259842412157637, -0.1113553986120547346 ) ) ;
#37250 = DIRECTION ( 'NONE',  ( -1.000000000000000000, 3.469446951953614189E-15, 1.144917494144692682E-16 ) ) ;
#37251 = CARTESIAN_POINT ( 'NONE',  ( -0.7185039370078746268, -0.06523048226347956391, 1.252460629921259061 ) ) ;
#37252 = FACE_BOUND ( 'NONE', #37931, .T. ) ;
#37254 = CARTESIAN_POINT ( 'NONE',  ( 0.7185039370078739607, 1.928577636452523993E-17, 1.919291338582677309 ) ) ;
#37253 = CARTESIAN_POINT ( 'NONE',  ( 0.1564256176496319206, -0.1250799318561882090, 0.06412650594366478551 ) ) ;
#37255 = DIRECTION ( 'NONE',  ( 0.000000000000000000, 0.000000000000000000, -1.000000000000000000 ) ) ;
#37256 = CARTESIAN_POINT ( 'NONE',  ( -0.1787899950787401604, -0.1555118109698585271, 0.07405724077823318263 ) ) ;
#37257 = VERTEX_POINT ( 'NONE', #47442 ) ;
#37258 = LINE ( 'NONE', #40361, #12998 ) ;
#37259 = CARTESIAN_POINT ( 'NONE',  ( -0.1120715992846887249, -0.09842519685039369248, 0.2207285028506147662 ) ) ;
#37260 = CARTESIAN_POINT ( 'NONE',  ( 0.7495606340400177148, -0.1264236179284866091, 0.8390748030958424808 ) ) ;
#37261 = CARTESIAN_POINT ( 'NONE',  ( 0.1574803149606300301, -0.1136811022546777433, -0.06523048226347956391 ) ) ;
#37262 = CARTESIAN_POINT ( 'NONE',  ( -0.7495606340400177148, 0.1264236179284866091, 1.222933070812378009 ) ) ;
#37263 = VECTOR ( 'NONE', #27171, 39.37007874015748143 ) ;
#37264 = DIRECTION ( 'NONE',  ( 0.000000000000000000, 0.000000000000000000, -1.000000000000000000 ) ) ;
#37265 = CARTESIAN_POINT ( 'NONE',  ( 0.8759842519685039353, 0.000000000000000000, 4.498031496062992574 ) ) ;
#37266 = CARTESIAN_POINT ( 'NONE',  ( -0.1787899950787401604, -1.037525543032389974, 0.07405724077823318263 ) ) ;
#37267 = ORIENTED_EDGE ( 'NONE', *, *, #37055, .F. ) ;
#37268 = CARTESIAN_POINT ( 'NONE',  ( -0.1264236179284866091, 0.08316929139234625901, 0.1264236179284866091 ) ) ;
#37269 = VERTEX_POINT ( 'NONE', #33084 ) ;
#37270 = CARTESIAN_POINT ( 'NONE',  ( 1.033464566929134687, -0.06523048226347956391, 1.218011810916094895 ) ) ;
#37271 = EDGE_CURVE ( 'NONE', #38595, #8725, #25160, .T. ) ;
#37272 = LINE ( 'NONE', #22906, #22419 ) ;
#37273 = ADVANCED_FACE ( 'NONE', ( #39748 ), #36195, .T. ) ;
#37274 = CARTESIAN_POINT ( 'NONE',  ( -0.8019270111902716547, -0.1787899950787401604, 0.1328740156942679884 ) ) ;
#37275 = CARTESIAN_POINT ( 'NONE',  ( -0.7185039370078739607, 1.928577636452523993E-17, 0.8956692913385826404 ) ) ;
#37276 = DIRECTION ( 'NONE',  ( 0.000000000000000000, 0.000000000000000000, 1.000000000000000000 ) ) ;
#37277 = CARTESIAN_POINT ( 'NONE',  ( -0.1270800023317771588, -1.029571368638163342, -0.1270800023317771588 ) ) ;
#37278 = CARTESIAN_POINT ( 'NONE',  ( 0.07267052687100558628, -0.2535370473714794182, -0.3104511204119563272 ) ) ;
#37279 = CARTESIAN_POINT ( 'NONE',  ( -0.9873396505805591694, 0.1113553986120547346, 1.500984251860976171 ) ) ;
#37280 = CARTESIAN_POINT ( 'NONE',  ( 0.7495606340400177148, 0.1264236179284866091, 0.9079724408911180600 ) ) ;
#37281 = CARTESIAN_POINT ( 'NONE',  ( 0.8759842519685039353, 0.1787899950787401882, 0.1107283464029295283 ) ) ;
#37282 = CARTESIAN_POINT ( 'NONE',  ( -1.033464566929133799, 0.000000000000000000, 0.08858267716535432601 ) ) ;
#37283 = CARTESIAN_POINT ( 'NONE',  ( 0.9873396505805591694, 0.1113553986120547346, 1.392716535433070835 ) ) ;
#37285 = CARTESIAN_POINT ( 'NONE',  ( -1.181162989532618060E-16, -0.3937007874015746034, -0.3937007874015748254 ) ) ;
#37284 = CARTESIAN_POINT ( 'NONE',  ( 0.7176825515505187436, 0.04481503542554400588, 1.982412129522283406 ) ) ;
#37286 = CARTESIAN_POINT ( 'NONE',  ( 0.8759842519685039353, 0.1574803149606299191, 0.3248031494987720369 ) ) ;
#37287 = CARTESIAN_POINT ( 'NONE',  ( 2.892866454678787531E-17, -0.6771653542231811373, 0.1574803149606299191 ) ) ;
#37288 = VECTOR ( 'NONE', #1513, 39.37007874015748143 ) ;
#37290 = CARTESIAN_POINT ( 'NONE',  ( 0.1595442748538399846, 0.1490840454108145752, 0.02272210951950409674 ) ) ;
#37289 = CARTESIAN_POINT ( 'NONE',  ( 1.054774247047244096, 0.000000000000000000, 0.8489173227808819444 ) ) ;
#37291 = CARTESIAN_POINT ( 'NONE',  ( 0.7495606340400177148, 0.1264236179284866091, 1.774114173174582643 ) ) ;
#37292 = CARTESIAN_POINT ( 'NONE',  ( -0.1264236179284866091, -0.7140748030958424808, -0.1264236179284866091 ) ) ;
#37293 = EDGE_LOOP ( 'NONE', ( #33708, #27549, #16807, #34274 ) ) ;
#37294 = CARTESIAN_POINT ( 'NONE',  ( -0.7185039370078739607, 1.928577636452523993E-17, 0.8562992125984251190 ) ) ;
#37295 = CARTESIAN_POINT ( 'NONE',  ( -0.4620708661417322616, 0.9842519685039375910, -0.8759842519685044904 ) ) ;
#37296 = CARTESIAN_POINT ( 'NONE',  ( 0.8759842519685039353, -0.1787899950787401882, 1.154035433017102319 ) ) ;
#37297 = CARTESIAN_POINT ( 'NONE',  ( 0.4330708661417327909, 0.1574803149606300301, 1.186023622047243986 ) ) ;
#37298 = CARTESIAN_POINT ( 'NONE',  ( 0.1113553986120547346, -1.695866141732283561, -0.1113553986120547346 ) ) ;
#37299 = ADVANCED_FACE ( 'NONE', ( #36432 ), #14856, .T. ) ;
#37300 = CARTESIAN_POINT ( 'NONE',  ( 0.2066929133858268486, 0.5419727308409658662, -0.7545416139885202655 ) ) ;
#37301 = ( BOUNDED_CURVE ( )  B_SPLINE_CURVE ( 2, ( #9614, #24234, #12977, #5994, #10080, #6465, #27615, #20615, #42865 ),
 .UNSPECIFIED., .F., .T. ) 
 B_SPLINE_CURVE_WITH_KNOTS ( ( 3, 2, 2, 2, 3 ),
 ( 0.3400000000000000244, 0.3425000000000000266, 0.3449999999999999734, 0.3474999999999999756, 0.3499999999999999778 ),
 .UNSPECIFIED. ) 
 CURVE ( )  GEOMETRIC_REPRESENTATION_ITEM ( )  RATIONAL_B_SPLINE_CURVE ( ( 1.000000000000000000, 0.9238795325112869605, 1.000000000000000000, 0.9238795325112869605, 1.000000000000000000, 0.9238795325112869605, 1.000000000000000000, 0.9238795325112849621, 1.000000000000000000 ) ) 
 REPRESENTATION_ITEM ( '' )  ) ;
#37302 = DIRECTION ( 'NONE',  ( 0.000000000000000000, 0.000000000000000000, -1.000000000000000000 ) ) ;
#37303 = CARTESIAN_POINT ( 'NONE',  ( -1.002407869896990045, 0.1264236179284866091, 0.1845472440407248116 ) ) ;
#37304 = ORIENTED_EDGE ( 'NONE', *, *, #31995, .T. ) ;
#37305 = CARTESIAN_POINT ( 'NONE',  ( 0.1574803149606300301, 0.1077755905511812162, 0.06523048226347956391 ) ) ;
#37306 = ORIENTED_EDGE ( 'NONE', *, *, #20257, .T. ) ;
#37307 = CARTESIAN_POINT ( 'NONE',  ( -0.1787899950787401604, -1.459645669237573884, 0.07405724077823318263 ) ) ;
#37308 = CARTESIAN_POINT ( 'NONE',  ( -0.7495606340400177148, 0.1264236179284866091, 1.887303149552535420 ) ) ;
#37309 = CARTESIAN_POINT ( 'NONE',  ( -0.8019270111902716547, 0.1787899950787401604, 0.9399606298674970661 ) ) ;
#37310 = CARTESIAN_POINT ( 'NONE',  ( -1.054774247047244096, 0.000000000000000000, 0.4601377952218267953 ) ) ;
#37311 = LINE ( 'NONE', #15291, #3079 ) ;
#37312 = VECTOR ( 'NONE', #14733, 39.37007874015748854 ) ;
#37313 = FACE_OUTER_BOUND ( 'NONE', #39316, .T. ) ;
#37314 = CARTESIAN_POINT ( 'NONE',  ( 0.1439410204707495533, 0.1277165727045734556, -0.08101594287816436812 ) ) ;
#37315 = CARTESIAN_POINT ( 'NONE',  ( 1.054774247047244540, -0.07405724077823318263, 0.05905511805647267048 ) ) ;
#37316 = CARTESIAN_POINT ( 'NONE',  ( -0.2665307357296560209, 0.1584585643853064219, -0.8211671128013016130 ) ) ;
#37317 = CARTESIAN_POINT ( 'NONE',  ( 0.1264236179284866091, -0.5921515272843562716, 0.1264236179284866091 ) ) ;
#37318 = CARTESIAN_POINT ( 'NONE',  ( -0.1577829598938297606, -0.08955953743824469904, -0.1904640068750519943 ) ) ;
#37319 = DIRECTION ( 'NONE',  ( -1.000000000000000000, 3.469446951953614189E-15, 0.000000000000000000 ) ) ;
#37320 = CARTESIAN_POINT ( 'NONE',  ( -0.1377952755905511861, 0.1574803149606320007, 0.9074803149606294195 ) ) ;
#37321 = CIRCLE ( 'NONE', #23597, 0.1377952755905511861 ) ;
#37322 = ( BOUNDED_CURVE ( )  B_SPLINE_CURVE ( 2, ( #23704, #37852, #27568, #23480, #41878, #5006, #16289, #5484, #30919 ),
 .UNSPECIFIED., .F., .T. ) 
 B_SPLINE_CURVE_WITH_KNOTS ( ( 3, 2, 2, 2, 3 ),
 ( 0.4500000000000000111, 0.4525000000000000133, 0.4550000000000000155, 0.4575000000000000178, 0.4600000000000000200 ),
 .UNSPECIFIED. ) 
 CURVE ( )  GEOMETRIC_REPRESENTATION_ITEM ( )  RATIONAL_B_SPLINE_CURVE ( ( 1.000000000000000000, 0.9238795325112869605, 1.000000000000000000, 0.9238795325112869605, 1.000000000000000000, 0.9238795325112869605, 1.000000000000000000, 0.9238795325112869605, 1.000000000000000000 ) ) 
 REPRESENTATION_ITEM ( '' )  ) ;
#37323 = CARTESIAN_POINT ( 'NONE',  ( -0.7495606340400177148, 0.1264236179284866091, 0.3124999999462365619 ) ) ;
#37324 = FACE_OUTER_BOUND ( 'NONE', #707, .T. ) ;
#37325 = EDGE_CURVE ( 'NONE', #894, #13083, #39989, .T. ) ;
#37326 = ORIENTED_EDGE ( 'NONE', *, *, #7682, .T. ) ;
#37327 = CARTESIAN_POINT ( 'NONE',  ( 0.2471911001155728260, -0.08911307781772316583, 0.05219320342793875439 ) ) ;
#37328 = ORIENTED_EDGE ( 'NONE', *, *, #46234, .T. ) ;
#37329 = CARTESIAN_POINT ( 'NONE',  ( -1.054774247047244540, 0.07405724077823318263, 1.564960629867495845 ) ) ;
#37330 = ORIENTED_EDGE ( 'NONE', *, *, #34866, .T. ) ;
#37331 = ADVANCED_FACE ( 'NONE', ( #21559 ), #29518, .F. ) ;
#37332 = CARTESIAN_POINT ( 'NONE',  ( 0.07405724077823318263, -1.371062992072219489, 0.1787899950787401604 ) ) ;
#37333 = CARTESIAN_POINT ( 'NONE',  ( 0.1787899950787401882, -1.516240157426551161, -2.189545951927503898E-17 ) ) ;
#37334 = DIRECTION ( 'NONE',  ( 1.822029033848725028E-16, 0.000000000000000000, 1.000000000000000000 ) ) ;
#37335 = DIRECTION ( 'NONE',  ( 0.000000000000000000, 1.000000000000000000, 0.000000000000000000 ) ) ;
#37336 = CARTESIAN_POINT ( 'NONE',  ( -1.033464566929133799, 0.000000000000000000, 1.141732283357039357 ) ) ;
#37337 = CARTESIAN_POINT ( 'NONE',  ( 0.8019270111902717657, -0.1787899950787401604, 0.5659448818360001132 ) ) ;
#37338 = CARTESIAN_POINT ( 'NONE',  ( 0.06523048226347956391, -0.2760826771653543954, -0.1574803149606300301 ) ) ;
#37339 = CARTESIAN_POINT ( 'NONE',  ( 0.8107537697050253289, 0.1574803149606300301, 1.980807086506644943 ) ) ;
#37340 = ORIENTED_EDGE ( 'NONE', *, *, #45159, .T. ) ;
#37341 = CARTESIAN_POINT ( 'NONE',  ( 0.3547871005709968273, 4.766607801171850497E-17, 0.000000000000000000 ) ) ;
#37342 = CARTESIAN_POINT ( 'NONE',  ( -0.8019270111902716547, -0.1787899950787401604, 1.038385826717890259 ) ) ;
#37343 = CARTESIAN_POINT ( 'NONE',  ( 0.8759842519685039353, 0.1574803149606299191, 0.9251968503937008093 ) ) ;
#37344 = DIRECTION ( 'NONE',  ( -0.000000000000000000, 1.000000000000000000, -0.000000000000000000 ) ) ;
#37345 = VECTOR ( 'NONE', #15324, 39.37007874015748143 ) ;
#37346 = CARTESIAN_POINT ( 'NONE',  ( 0.7646288533564489232, -0.1113553986120547346, 0.7431102362204724532 ) ) ;
#37347 = CARTESIAN_POINT ( 'NONE',  ( -0.1461630486916919713, -0.08955915398144619066, 0.07502663895056801979 ) ) ;
#37348 = ORIENTED_EDGE ( 'NONE', *, *, #3411, .T. ) ;
#37349 = CARTESIAN_POINT ( 'NONE',  ( 0.1595439659404218613, -0.05486241767500590893, -0.1404716193513352585 ) ) ;
#37350 = EDGE_LOOP ( 'NONE', ( #13353, #16369, #17940, #2336 ) ) ;
#37351 = ORIENTED_EDGE ( 'NONE', *, *, #2146, .T. ) ;
#37352 = CARTESIAN_POINT ( 'NONE',  ( -0.1093692153654682031, 0.09774221684002692978, -0.2222887249338305893 ) ) ;
#37353 = CARTESIAN_POINT ( 'NONE',  ( -0.1574803149606300301, -0.03001968503937006705, -0.06523048226347956391 ) ) ;
#37354 = CARTESIAN_POINT ( 'NONE',  ( -0.07405724077823318263, -1.503937007820251637, -0.1787899950787401604 ) ) ;
#37355 = CARTESIAN_POINT ( 'NONE',  ( 0.1264236179284866091, -0.8961614172690708369, 0.1264236179284866091 ) ) ;
#37357 = CIRCLE ( 'NONE', #3706, 0.2952755905511810774 ) ;
#37356 = CARTESIAN_POINT ( 'NONE',  ( 0.1574803149606300301, -1.225885826771653697, -0.06523048226347956391 ) ) ;
#37358 = CARTESIAN_POINT ( 'NONE',  ( 0.8759842519685039353, -0.1574803149606299191, 1.092519684931842594 ) ) ;
#37359 = PLANE ( 'NONE',  #42787 ) ;
#37360 = UNCERTAINTY_MEASURE_WITH_UNIT (LENGTH_MEASURE( 1.000000000000000082E-05 ), #31442, 'distance_accuracy_value', 'NONE') ;
#37361 = ORIENTED_EDGE ( 'NONE', *, *, #33374, .T. ) ;
#37362 = CARTESIAN_POINT ( 'NONE',  ( -0.9500414927467378812, -0.1787899950787401604, 1.751968503883245765 ) ) ;
#37363 = CARTESIAN_POINT ( 'NONE',  ( 0.8019270111902717657, -0.1787899950787401604, 1.668307086560410157 ) ) ;
#37364 = CARTESIAN_POINT ( 'NONE',  ( 0.1574803149606299191, -1.297244094380661350, -1.928577636452523993E-17 ) ) ;
#37365 = LINE ( 'NONE', #33819, #12651 ) ;
#37366 = CARTESIAN_POINT ( 'NONE',  ( -1.054774247047244096, 0.000000000000000000, 1.360728346402929168 ) ) ;
#37367 = CARTESIAN_POINT ( 'NONE',  ( 0.8759842519685039353, 0.000000000000000000, 4.498031496062992574 ) ) ;
#37368 = CARTESIAN_POINT ( 'NONE',  ( -1.054774247047244540, 0.07405724077823318263, 1.166338582623402731 ) ) ;
#37369 = CARTESIAN_POINT ( 'NONE',  ( -0.7495606340400177148, -0.1264236179284866091, 0.9522637794737952577 ) ) ;
#37370 = CARTESIAN_POINT ( 'NONE',  ( -0.8019270111902717657, 0.1787899950787401604, 0.03937007868639399305 ) ) ;
#37371 = DIRECTION ( 'NONE',  ( 0.000000000000000000, -1.000000000000000000, 0.000000000000000000 ) ) ;
#37372 = EDGE_CURVE ( 'NONE', #28460, #1520, #358, .T. ) ;
#37373 = CARTESIAN_POINT ( 'NONE',  ( -0.9500414927467378812, -0.1787899950787401604, 1.633858267662771313 ) ) ;
#37374 = VERTEX_POINT ( 'NONE', #46710 ) ;
#37375 = CYLINDRICAL_SURFACE ( 'NONE', #28741, 0.1864803149606298893 ) ;
#37376 = CARTESIAN_POINT ( 'NONE',  ( -0.7185039370078739607, 1.928577636452523993E-17, 1.564960629921259949 ) ) ;
#37377 = CARTESIAN_POINT ( 'NONE',  ( 0.1992435948116500766, -0.3638053972758239496, -1.027775237132794173 ) ) ;
#37378 = EDGE_CURVE ( 'NONE', #2629, #16719, #27874, .T. ) ;
#37379 = CARTESIAN_POINT ( 'NONE',  ( 1.002407869896990045, 0.1264236179284866091, 1.646161417269070837 ) ) ;
#37380 = CARTESIAN_POINT ( 'NONE',  ( -0.2340881785939889770, -0.09842519685039370636, -0.07097624971890235945 ) ) ;
#37381 = CARTESIAN_POINT ( 'NONE',  ( 1.033464566929133799, 0.000000000000000000, 1.938976377952756014 ) ) ;
#37382 = ORIENTED_EDGE ( 'NONE', *, *, #9440, .T. ) ;
#37383 = EDGE_CURVE ( 'NONE', #24091, #7448, #7181, .T. ) ;
#37384 = VECTOR ( 'NONE', #3471, 39.37007874015748854 ) ;
#37385 = ORIENTED_EDGE ( 'NONE', *, *, #41363, .T. ) ;
#37386 = AXIS2_PLACEMENT_3D ( 'NONE', #46188, #28015, #42577 ) ;
#37387 = EDGE_LOOP ( 'NONE', ( #8392, #5919 ) ) ;
#37388 = CARTESIAN_POINT ( 'NONE',  ( 0.1787899950787401882, -0.8912401574265511606, -2.189545951927503898E-17 ) ) ;
#37389 = AXIS2_PLACEMENT_3D ( 'NONE', #35692, #417, #37088 ) ;
#37390 = CARTESIAN_POINT ( 'NONE',  ( 0.07405724077823318263, -1.011811023568284451, 0.1787899950787401604 ) ) ;
#37391 = ORIENTED_EDGE ( 'NONE', *, *, #14169, .F. ) ;
#37392 = DIRECTION ( 'NONE',  ( 0.000000000000000000, 0.000000000000000000, 1.000000000000000000 ) ) ;
#37393 = ( NAMED_UNIT ( * ) SI_UNIT ( $, .STERADIAN. ) SOLID_ANGLE_UNIT ( ) ) ;
#37394 = CARTESIAN_POINT ( 'NONE',  ( 0.7495606340400177148, -0.1264236179284866091, 1.818405511757259729 ) ) ;
#37395 = CARTESIAN_POINT ( 'NONE',  ( -0.1797182628040039087, -0.2741579828113920869, 0.07444174185955065859 ) ) ;
#37396 = CARTESIAN_POINT ( 'NONE',  ( 0.1872703683832034893, 0.1873733034532325537, -0.3097625555229955863 ) ) ;
#37397 = CARTESIAN_POINT ( 'NONE',  ( -0.7646288533564489232, -0.1113553986120547346, 0.8907480313885355327 ) ) ;
#37398 = CARTESIAN_POINT ( 'NONE',  ( 0.8019270111902717657, 0.1787899950787401604, 0.8218503936470251681 ) ) ;
#37400 = CARTESIAN_POINT ( 'NONE',  ( 0.7185039370078714072, 0.06523048226347728795, 1.129429133858268708 ) ) ;
#37399 = CARTESIAN_POINT ( 'NONE',  ( -0.9873396505805591694, -0.1113553986120547346, 1.569881889656251861 ) ) ;
#37401 = FACE_OUTER_BOUND ( 'NONE', #10579, .T. ) ;
#37402 = CARTESIAN_POINT ( 'NONE',  ( -0.1574803149606299191, 0.07021257666615010606, -0.1553045758542774823 ) ) ;
#37403 = CARTESIAN_POINT ( 'NONE',  ( 0.8019270111902717657, 0.1787899950787401604, 1.889763779473794258 ) ) ;
#37404 = CARTESIAN_POINT ( 'NONE',  ( 1.033464566929133799, 0.000000000000000000, 0.08858267716535432601 ) ) ;
#37405 = CARTESIAN_POINT ( 'NONE',  ( 0.8759842519685039353, 0.000000000000000000, 4.498031496062992574 ) ) ;
#37407 = CARTESIAN_POINT ( 'NONE',  ( 0.1264236179284866091, -0.2957677164816697180, -0.1264236179284866091 ) ) ;
#37406 = CARTESIAN_POINT ( 'NONE',  ( -0.1574803149606297803, -0.9601377951680625245, 0.06523048226347956391 ) ) ;
#37408 = FACE_OUTER_BOUND ( 'NONE', #24153, .T. ) ;
#37409 = CARTESIAN_POINT ( 'NONE',  ( 0.07405724077823318263, -1.287401574749386768, 0.1787899950787401604 ) ) ;
#37410 = CARTESIAN_POINT ( 'NONE',  ( 1.054774247047244540, -0.07405724077823318263, 0.1820866141194649179 ) ) ;
#37411 = DIRECTION ( 'NONE',  ( -1.000000000000000000, 0.000000000000000000, 0.000000000000000000 ) ) ;
#37412 = CIRCLE ( 'NONE', #42759, 0.1377952755905511861 ) ;
#37413 = CARTESIAN_POINT ( 'NONE',  ( -1.002407869896990045, 0.1264236179284866091, 1.759350393647023614 ) ) ;
#37414 = ORIENTED_EDGE ( 'NONE', *, *, #40264, .T. ) ;
#37415 = CARTESIAN_POINT ( 'NONE',  ( -1.002407869896990045, -0.1264236179284866091, 1.321358267662771757 ) ) ;
#37416 = CARTESIAN_POINT ( 'NONE',  ( -1.033464566929133799, 0.000000000000000000, 1.299212598317669221 ) ) ;
#37417 = CIRCLE ( 'NONE', #8343, 0.5708661417322833387 ) ;
#37418 = CARTESIAN_POINT ( 'NONE',  ( 0.8759842519685039353, 0.1787899950787401882, 1.336122047190330786 ) ) ;
#37419 = CARTESIAN_POINT ( 'NONE',  ( -0.1574803149606299191, -1.198818897530267824, 0.000000000000000000 ) ) ;
#37420 = CARTESIAN_POINT ( 'NONE',  ( -0.8759842519685039353, -0.1787899950787401882, 0.5290354330171024300 ) ) ;
#37421 = CARTESIAN_POINT ( 'NONE',  ( 1.054774247047244540, 0.07405724077823318263, 1.914370078686394860 ) ) ;
#37422 = CARTESIAN_POINT ( 'NONE',  ( -0.9500414927467378812, -0.1787899950787401604, 1.077755905458048113 ) ) ;
#37423 = EDGE_CURVE ( 'NONE', #23816, #9464, #22740, .T. ) ;
#37424 = CARTESIAN_POINT ( 'NONE',  ( 1.033464566929133799, 0.000000000000000000, 0.5610236220472440971 ) ) ;
#37425 = CARTESIAN_POINT ( 'NONE',  ( -0.008273236941784495660, -0.09842493939591641372, -0.1788444388497219262 ) ) ;
#37426 = CYLINDRICAL_SURFACE ( 'NONE', #14757, 0.1574803149606301966 ) ;
#37427 = CARTESIAN_POINT ( 'NONE',  ( 1.002407869896990045, 0.1264236179284866091, 0.4650590550643464716 ) ) ;
#37428 = CARTESIAN_POINT ( 'NONE',  ( -0.6971942568897637749, 2.189545951927499583E-17, 0.3567913385289137596 ) ) ;
#37429 = CARTESIAN_POINT ( 'NONE',  ( -0.8019270111902717657, 0.1787899950787401604, 0.8218503936470251681 ) ) ;
#37430 = CARTESIAN_POINT ( 'NONE',  ( 0.7185039370078746268, 0.06523048226347956391, 1.710137795168064079 ) ) ;
#37431 = ORIENTED_EDGE ( 'NONE', *, *, #38591, .T. ) ;
#37432 = ORIENTED_EDGE ( 'NONE', *, *, #16413, .T. ) ;
#37433 = AXIS2_PLACEMENT_3D ( 'NONE', #6562, #42022, #16658 ) ;
#37434 = CARTESIAN_POINT ( 'NONE',  ( 0.2395294000716133853, -0.1968503937007874127, -0.4921259842519685179 ) ) ;
#37435 = CARTESIAN_POINT ( 'NONE',  ( 1.054774247047244540, -0.07405724077823318263, 0.9301181101824563813 ) ) ;
#37436 = CARTESIAN_POINT ( 'NONE',  ( -0.8107537697050253289, 0.1574803149606300301, 0.1402559055118110520 ) ) ;
#37437 = AXIS2_PLACEMENT_3D ( 'NONE', #33506, #11689, #10986 ) ;
#37438 = EDGE_CURVE ( 'NONE', #17112, #46310, #22499, .T. ) ;
#37439 = CARTESIAN_POINT ( 'NONE',  ( 1.054774247047244540, -0.07405724077823318263, 1.205708661363558365 ) ) ;
#37440 = CARTESIAN_POINT ( 'NONE',  ( -0.9500414927467377701, -0.1787899950787401604, 1.983267716481668108 ) ) ;
#37441 = ORIENTED_EDGE ( 'NONE', *, *, #24705, .T. ) ;
#37442 = CARTESIAN_POINT ( 'NONE',  ( -1.054774247047244540, 0.07405724077823318263, 0.8956692912848198684 ) ) ;
#37443 = ( BOUNDED_CURVE ( )  B_SPLINE_CURVE ( 2, ( #12112, #4653, #29879, #18571, #25784, #22397, #29422, #41290, #37026 ),
 .UNSPECIFIED., .F., .T. ) 
 B_SPLINE_CURVE_WITH_KNOTS ( ( 3, 2, 2, 2, 3 ),
 ( 0.9200000000000000400, 0.9224999999999999867, 0.9250000000000000444, 0.9274999999999999911, 0.9300000000000000488 ),
 .UNSPECIFIED. ) 
 CURVE ( )  GEOMETRIC_REPRESENTATION_ITEM ( )  RATIONAL_B_SPLINE_CURVE ( ( 1.000000000000000000, 0.9238795325112869605, 1.000000000000000000, 0.9238795325112869605, 1.000000000000000000, 0.9238795325112869605, 1.000000000000000000, 0.9238795325112869605, 1.000000000000000000 ) ) 
 REPRESENTATION_ITEM ( '' )  ) ;
#37444 = CARTESIAN_POINT ( 'NONE',  ( 0.1563805530828667190, -0.1352584698612838698, -0.04649480693109527690 ) ) ;
#37445 = CARTESIAN_POINT ( 'NONE',  ( -1.054774247047244540, -0.07405724077823318263, 0.05905511805647267048 ) ) ;
#37446 = CARTESIAN_POINT ( 'NONE',  ( 0.1787899950787401604, -1.495202708386720092, 0.07405724077823318263 ) ) ;
#37447 = ORIENTED_EDGE ( 'NONE', *, *, #315, .T. ) ;
#37448 = DIRECTION ( 'NONE',  ( 0.000000000000000000, -0.000000000000000000, 1.000000000000000000 ) ) ;
#37449 = CARTESIAN_POINT ( 'NONE',  ( 0.1264236179284866091, -0.4187992125446614589, 0.1264236179284866091 ) ) ;
#37450 = FACE_OUTER_BOUND ( 'NONE', #18809, .T. ) ;
#37451 = ORIENTED_EDGE ( 'NONE', *, *, #9215, .F. ) ;
#37452 = CARTESIAN_POINT ( 'NONE',  ( 1.054774247047244096, 0.000000000000000000, 1.321358267662771757 ) ) ;
#37453 = DIRECTION ( 'NONE',  ( -1.000000000000000000, 0.000000000000000000, -0.000000000000000000 ) ) ;
#37454 = LINE ( 'NONE', #772, #19256 ) ;
#37455 = VECTOR ( 'NONE', #25426, 39.37007874015748143 ) ;
#37456 = CARTESIAN_POINT ( 'NONE',  ( 0.000000000000000000, 0.000000000000000000, -0.3149606299212598381 ) ) ;
#37457 = CARTESIAN_POINT ( 'NONE',  ( 0.6971942568897648851, -0.07405724077823297447, 1.540354330654897685 ) ) ;
#37458 = CARTESIAN_POINT ( 'NONE',  ( 1.002407869896990045, -0.1264236179284866091, 0.1353346456155277433 ) ) ;
#37459 = CARTESIAN_POINT ( 'NONE',  ( -0.1264236179284866091, 0.09682485066839900678, -0.1264236179284866091 ) ) ;
#37460 = CARTESIAN_POINT ( 'NONE',  ( -0.1787899950787401604, -1.656496062938362268, -0.07405724077823318263 ) ) ;
#37461 = DIRECTION ( 'NONE',  ( -0.4075214141134388957, 0.000000000000000000, 0.9131956510184348064 ) ) ;
#37462 = CARTESIAN_POINT ( 'NONE',  ( -0.6195511811023656223, 0.9842519685039375910, -0.5511811023622041894 ) ) ;
#37463 = DIMENSIONAL_EXPONENTS ( 1.000000000000000000, 0.000000000000000000, 0.000000000000000000, 0.000000000000000000, 0.000000000000000000, 0.000000000000000000, 0.000000000000000000 ) ;
#37464 = CIRCLE ( 'NONE', #24476, 0.08090551181102362266 ) ;
#37465 = CARTESIAN_POINT ( 'NONE',  ( -0.6971942568897637749, 2.189545951927499583E-17, 0.5979330708123780092 ) ) ;
#37467 = CARTESIAN_POINT ( 'NONE',  ( 0.1822895153388602307, 0.000000000000000000, 0.000000000000000000 ) ) ;
#37466 = CARTESIAN_POINT ( 'NONE',  ( -9.642888182262618425E-18, -0.7066929133858268486, -0.1574803149606299191 ) ) ;
#37468 = CARTESIAN_POINT ( 'NONE',  ( -0.07444174185955065859, -1.371598927693281844, 0.1797182628040039087 ) ) ;
#37469 = DIRECTION ( 'NONE',  ( 1.541976423090495042E-15, 0.4344452574044144755, -0.9006982393225890782 ) ) ;
#37470 = CARTESIAN_POINT ( 'NONE',  ( -0.8759842519685039353, -0.1574803149606299191, 1.604330708553889595 ) ) ;
#37471 = CYLINDRICAL_SURFACE ( 'NONE', #45996, 0.1574803149606299191 ) ;
#37472 = CARTESIAN_POINT ( 'NONE',  ( 0.9500414927467378812, 0.1787899950787401604, 1.373031496009229135 ) ) ;
#37473 = CARTESIAN_POINT ( 'NONE',  ( 1.002407869896990045, 0.1264236179284866091, 1.877460629867496067 ) ) ;
#37475 = ORIENTED_EDGE ( 'NONE', *, *, #8326, .F. ) ;
#37474 = CARTESIAN_POINT ( 'NONE',  ( -0.8759842519685039353, 0.000000000000000000, 0.000000000000000000 ) ) ;
#37476 = CARTESIAN_POINT ( 'NONE',  ( -0.7185039370078746268, 0.06523048226347956391, 1.523129921259841923 ) ) ;
#37477 = LINE ( 'NONE', #23808, #21337 ) ;
#37478 = DIRECTION ( 'NONE',  ( 7.047314121155781188E-15, 0.000000000000000000, 1.000000000000000000 ) ) ;
#37479 = CARTESIAN_POINT ( 'NONE',  ( -1.033464566929134687, 0.06523048226347956391, 1.222933070758614127 ) ) ;
#37480 = CARTESIAN_POINT ( 'NONE',  ( 0.7495606340400177148, -0.1264236179284866091, 0.3223425196312759144 ) ) ;
#37481 = CYLINDRICAL_SURFACE ( 'NONE', #30051, 0.1574803149606299191 ) ;
#37482 = CARTESIAN_POINT ( 'NONE',  ( 0.3551574803149606385, 2.613864355459500179E-17, 0.000000000000000000 ) ) ;
#37483 = CARTESIAN_POINT ( 'NONE',  ( -0.8759842519685039353, 0.000000000000000000, 2.007874015640504162 ) ) ;
#37484 = CARTESIAN_POINT ( 'NONE',  ( 0.9873396505805591694, 0.1113553986120547346, 0.6742125983176693316 ) ) ;
#37485 = ORIENTED_EDGE ( 'NONE', *, *, #27094, .T. ) ;
#37486 = DIRECTION ( 'NONE',  ( 0.000000000000000000, 0.000000000000000000, -1.000000000000000000 ) ) ;
#37487 = CARTESIAN_POINT ( 'NONE',  ( -9.642888182262618425E-18, -0.03740157480314960925, -0.1574803149606299191 ) ) ;
#37488 = ORIENTED_EDGE ( 'NONE', *, *, #17257, .T. ) ;
#37489 = CARTESIAN_POINT ( 'NONE',  ( 0.1797182628040039087, -0.05762254974052589268, -0.07444174185955065859 ) ) ;
#37490 = CARTESIAN_POINT ( 'NONE',  ( -0.07405724077823318263, -1.154527559001354842, -0.1787899950787401604 ) ) ;
#37491 = CARTESIAN_POINT ( 'NONE',  ( 0.000000000000000000, 1.478656101119254046E-17, 0.1377952755905511861 ) ) ;
#37492 = CARTESIAN_POINT ( 'NONE',  ( -0.9412147342319837628, 0.1574803149606300301, 1.198326771653543510 ) ) ;
#37493 = EDGE_CURVE ( 'NONE', #18657, #16796, #46988, .T. ) ;
#37494 = CARTESIAN_POINT ( 'NONE',  ( -1.033464566929133799, 0.000000000000000000, 0.4429133858267716439 ) ) ;
#37496 = CARTESIAN_POINT ( 'NONE',  ( 0.9873396505805591694, 0.1113553986120547346, 1.943897637795275690 ) ) ;
#37495 = CARTESIAN_POINT ( 'NONE',  ( -0.7185039370078739607, 1.928577636452523993E-17, 0.09842519674286673292 ) ) ;
#37497 = ORIENTED_EDGE ( 'NONE', *, *, #10725, .F. ) ;
#37498 = EDGE_CURVE ( 'NONE', #7863, #24526, #31260, .T. ) ;
#37499 = CIRCLE ( 'NONE', #16825, 0.09842519685039370636 ) ;
#37500 = CARTESIAN_POINT ( 'NONE',  ( -0.08392772586492357190, -0.09126532511089867350, -0.2369773207361680067 ) ) ;
#37501 = ADVANCED_FACE ( 'NONE', ( #5350 ), #45838, .T. ) ;
#37502 = CARTESIAN_POINT ( 'NONE',  ( 0.7495606340400177148, 0.1264236179284866091, 0.9867125983714331028 ) ) ;
#37503 = CARTESIAN_POINT ( 'NONE',  ( 0.1113553986120547346, -0.1210629920184572855, 0.1113553986120547346 ) ) ;
#37504 = CARTESIAN_POINT ( 'NONE',  ( -0.7495606340400177148, -0.1264236179284866091, 1.272145669237574772 ) ) ;
#37505 = ORIENTED_EDGE ( 'NONE', *, *, #25382, .F. ) ;
#37506 = EDGE_CURVE ( 'NONE', #44561, #14442, #42870, .T. ) ;
#37507 = AXIS2_PLACEMENT_3D ( 'NONE', #22466, #7390, #37558 ) ;
#37508 = CARTESIAN_POINT ( 'NONE',  ( -0.7495606340400177148, -0.1264236179284866091, 0.3272637794737956463 ) ) ;
#37509 = CARTESIAN_POINT ( 'NONE',  ( 0.000000000000000000, 0.000000000000000000, 0.4921259842519685179 ) ) ;
#37510 = DIRECTION ( 'NONE',  ( -0.5735764363510518216, -0.8191520442889876907, 0.000000000000000000 ) ) ;
#37511 = CARTESIAN_POINT ( 'NONE',  ( -0.1787899950787401882, -1.000616094213490292, 0.000000000000000000 ) ) ;
#37512 = ORIENTED_EDGE ( 'NONE', *, *, #10628, .T. ) ;
#37513 = CARTESIAN_POINT ( 'NONE',  ( 0.07405724077823318263, 0.1053149606836847191, -0.1787899950787401604 ) ) ;
#37514 = ORIENTED_EDGE ( 'NONE', *, *, #40291, .F. ) ;
#37515 = CARTESIAN_POINT ( 'NONE',  ( 1.002407869896990045, -0.1264236179284866091, 1.040846456639149764 ) ) ;
#37516 = CARTESIAN_POINT ( 'NONE',  ( 0.003562681675963810801, -0.04170475804576580930, 0.1377952202815972693 ) ) ;
#37517 = DIRECTION ( 'NONE',  ( 0.000000000000000000, 0.000000000000000000, 1.000000000000000000 ) ) ;
#37518 = DIRECTION ( 'NONE',  ( -2.775557561562890735E-17, 0.6156614753256639538, 0.7880107536067174623 ) ) ;
#37519 = CARTESIAN_POINT ( 'NONE',  ( 0.1264236179284866091, -0.5024606298674960669, 0.1264236179284866091 ) ) ;
#37520 = CIRCLE ( 'NONE', #9239, 0.3100393700787401619 ) ;
#37521 = CARTESIAN_POINT ( 'NONE',  ( -1.054774247047244540, 0.07405724077823318263, 0.2657480314422993595 ) ) ;
#37522 = CARTESIAN_POINT ( 'NONE',  ( -0.7185039370078746268, -0.06523048226347956391, 0.8193897637795271027 ) ) ;
#37523 = FACE_OUTER_BOUND ( 'NONE', #26850, .T. ) ;
#37524 = CARTESIAN_POINT ( 'NONE',  ( 3.301370929368692659E-17, -0.9754375103704467920, 0.1797182628040039365 ) ) ;
#37525 = CARTESIAN_POINT ( 'NONE',  ( 1.033464566929134687, -0.06523048226347956391, 1.109744094488189115 ) ) ;
#37526 = CARTESIAN_POINT ( 'NONE',  ( -0.8759842519685039353, 0.1574803149606299191, 1.545275590443653480 ) ) ;
#37527 = CARTESIAN_POINT ( 'NONE',  ( 1.054774247047244540, 0.07405724077823318263, 0.9744094487651340231 ) ) ;
#37528 = VECTOR ( 'NONE', #21756, 39.37007874015748143 ) ;
#37529 = CARTESIAN_POINT ( 'NONE',  ( 0.9873396505805591694, -0.1113553986120547346, 1.461614173228346525 ) ) ;
#37531 = CARTESIAN_POINT ( 'NONE',  ( -0.1377952755905511861, -1.331775896911328393E-15, -0.7066929133858274037 ) ) ;
#37530 = CARTESIAN_POINT ( 'NONE',  ( 0.7139362040247607677, -0.04189616717365371446, 1.984049518046542504 ) ) ;
#37532 = CARTESIAN_POINT ( 'NONE',  ( -0.2066929133858267931, -0.2237541348899638183, -1.272196386806236701 ) ) ;
#37533 = CARTESIAN_POINT ( 'NONE',  ( -0.3161444924769509779, 0.4457451269443606368, -1.671447902550282194 ) ) ;
#37534 = CARTESIAN_POINT ( 'NONE',  ( 0.6971942568897637749, 2.189545951927499583E-17, 0.8686023621509606496 ) ) ;
#37535 = CARTESIAN_POINT ( 'NONE',  ( 1.002407869896990045, 0.1264236179284866091, 1.803641732229700700 ) ) ;
#37536 = CARTESIAN_POINT ( 'NONE',  ( -0.1264236179284866091, -0.7928149605761574126, -0.1264236179284866091 ) ) ;
#37537 = ORIENTED_EDGE ( 'NONE', *, *, #8886, .T. ) ;
#37538 = DIRECTION ( 'NONE',  ( 1.000000000000000000, 0.000000000000000000, 0.000000000000000000 ) ) ;
#37539 = CARTESIAN_POINT ( 'NONE',  ( -0.7185039370078739607, 0.000000000000000000, -2.869337061179095023E-17 ) ) ;
#37540 = CARTESIAN_POINT ( 'NONE',  ( 0.1113553986120547346, -1.607283464459401401, -0.1113553986120547346 ) ) ;
#37541 = CARTESIAN_POINT ( 'NONE',  ( 0.7495606340400177148, 0.1264236179284866091, 1.218011810969858111 ) ) ;
#37542 = CARTESIAN_POINT ( 'NONE',  ( -0.7185039370078739607, 1.928577636452523993E-17, 1.053149606299212504 ) ) ;
#37543 = CARTESIAN_POINT ( 'NONE',  ( 0.1113553986120547346, -1.745078740157480546, 0.1113553986120547346 ) ) ;
#37544 = CARTESIAN_POINT ( 'NONE',  ( -0.7646288533564489232, -0.1113553986120547346, 0.5068897637795275468 ) ) ;
#37545 = EDGE_CURVE ( 'NONE', #22479, #40667, #13047, .T. ) ;
#37546 = ORIENTED_EDGE ( 'NONE', *, *, #8756, .T. ) ;
#37547 = CARTESIAN_POINT ( 'NONE',  ( -0.7495606340400177148, 0.1264236179284866091, 0.3124999999462365619 ) ) ;
#37548 = ORIENTED_EDGE ( 'NONE', *, *, #13636, .F. ) ;
#37549 = CARTESIAN_POINT ( 'NONE',  ( 3.127876812047771422E-16, 0.2954942322624074524, -0.3149606299212598381 ) ) ;
#37551 = CARTESIAN_POINT ( 'NONE',  ( 3.284318927891251994E-17, -1.609744094434425232, 0.1787899950787401882 ) ) ;
#37550 = CARTESIAN_POINT ( 'NONE',  ( -0.06523048226347956391, -0.3646653542231817480, 0.1574803149606297803 ) ) ;
#37552 = CARTESIAN_POINT ( 'NONE',  ( -0.8019270111902717657, -0.1787899950787401604, 1.820866141678520789 ) ) ;
#37553 = CARTESIAN_POINT ( 'NONE',  ( -1.054774247047244540, 0.07405724077823318263, 0.8513779527021426707 ) ) ;
#37554 = EDGE_CURVE ( 'NONE', #1893, #2328, #21082, .T. ) ;
#37555 = CARTESIAN_POINT ( 'NONE',  ( -1.002407869896990045, 0.1264236179284866091, 1.129429133804503937 ) ) ;
#37556 = CARTESIAN_POINT ( 'NONE',  ( -0.8019270111902717657, -0.1787899950787401604, 0.5659448818360001132 ) ) ;
#37557 = AXIS2_PLACEMENT_3D ( 'NONE', #9790, #9074, #9557 ) ;
#37558 = DIRECTION ( 'NONE',  ( 0.000000000000000000, -1.000000000000000000, 0.000000000000000000 ) ) ;
#37559 = CARTESIAN_POINT ( 'NONE',  ( 0.3123359580052492146, 4.616380251121755931E-17, 0.000000000000000000 ) ) ;
#37560 = CARTESIAN_POINT ( 'NONE',  ( 0.000000000000000000, 0.000000000000000000, 0.000000000000000000 ) ) ;
#37561 = CARTESIAN_POINT ( 'NONE',  ( -0.3053042314538800817, 0.05494681823601590964, -1.034402892550617459 ) ) ;
#37562 = CARTESIAN_POINT ( 'NONE',  ( 0.1787899950787401882, -0.6266003461819942277, -2.189545951927503898E-17 ) ) ;
#37563 = CARTESIAN_POINT ( 'NONE',  ( -0.1975987513857511702, -0.08955961876119605813, -0.1443798108109194955 ) ) ;
#37564 = CYLINDRICAL_SURFACE ( 'NONE', #11920, 0.1574803149606299191 ) ;
#37565 = CARTESIAN_POINT ( 'NONE',  ( -1.181102362204724310, -0.3937007874015748254, -0.9842519685039370358 ) ) ;
#37566 = PRODUCT_DEFINITION_SHAPE ( 'NONE', 'NONE',  #47469 ) ;
#37567 = DIRECTION ( 'NONE',  ( 0.000000000000000000, 0.000000000000000000, -1.000000000000000000 ) ) ;
#37568 = CARTESIAN_POINT ( 'NONE',  ( -0.6971942568897626646, -0.07405724077823297447, 0.4773622046706456068 ) ) ;
#37569 = LINE ( 'NONE', #33780, #36057 ) ;
#37570 = LINE ( 'NONE', #16026, #8037 ) ;
#37571 = CARTESIAN_POINT ( 'NONE',  ( -0.1787899950787401882, -1.383366141678519678, 0.000000000000000000 ) ) ;
#37572 = ADVANCED_FACE ( 'NONE', ( #35722 ), #2857, .T. ) ;
#37573 = CARTESIAN_POINT ( 'NONE',  ( 0.1787899950787401604, -1.479330708607653699, 0.07405724077823318263 ) ) ;
#37574 = DIRECTION ( 'NONE',  ( -1.000000000000000000, 0.000000000000000000, 0.000000000000000000 ) ) ;
#37575 = CARTESIAN_POINT ( 'NONE',  ( 0.9412147342319837628, -0.1574803149606297803, 0.4749015748031497064 ) ) ;
#37576 = CARTESIAN_POINT ( 'NONE',  ( 0.6195511811023624027, 0.9842519685039365918, -0.7135826771653542844 ) ) ;
#37577 = CARTESIAN_POINT ( 'NONE',  ( -1.033464566929134687, -0.06523048226347956391, 1.099901574695622886 ) ) ;
#37578 = CARTESIAN_POINT ( 'NONE',  ( 1.054774247047244096, 0.000000000000000000, 0.5388779527021417826 ) ) ;
#37580 = DIRECTION ( 'NONE',  ( -0.000000000000000000, 1.000000000000000000, -0.000000000000000000 ) ) ;
#37579 = CARTESIAN_POINT ( 'NONE',  ( 0.06523048226347956391, -0.3154527559055120278, -0.1574803149606300301 ) ) ;
#37581 = ORIENTED_EDGE ( 'NONE', *, *, #21530, .T. ) ;
#37582 = CARTESIAN_POINT ( 'NONE',  ( 1.033464566929134687, 0.06523048226347956391, 1.931594488081448180 ) ) ;
#37583 = ORIENTED_EDGE ( 'NONE', *, *, #13909, .T. ) ;
#37584 = DIRECTION ( 'NONE',  ( 0.000000000000000000, -0.2432573283306646017, 0.9699617890481189164 ) ) ;
#37585 = CARTESIAN_POINT ( 'NONE',  ( -0.9500414927467377701, 0.1787899950787401604, 1.058070866087969186 ) ) ;
#37586 = CARTESIAN_POINT ( 'NONE',  ( 0.7646288533564489232, 0.1113553986120547346, 0.8907480314960629642 ) ) ;
#37587 = DIRECTION ( 'NONE',  ( 0.000000000000000000, 1.000000000000000000, 0.000000000000000000 ) ) ;
#37588 = ( BOUNDED_CURVE ( )  B_SPLINE_CURVE ( 2, ( #40194, #7609, #18631, #19104, #22225, #7850, #7391, #26078, #22467 ),
 .UNSPECIFIED., .F., .T. ) 
 B_SPLINE_CURVE_WITH_KNOTS ( ( 3, 2, 2, 2, 3 ),
 ( 0.4899999999999999911, 0.4924999999999999933, 0.4949999999999999956, 0.4974999999999999978, 0.5000000000000000000 ),
 .UNSPECIFIED. ) 
 CURVE ( )  GEOMETRIC_REPRESENTATION_ITEM ( )  RATIONAL_B_SPLINE_CURVE ( ( 1.000000000000000000, 0.9238795325112869605, 1.000000000000000000, 0.9238795325112869605, 1.000000000000000000, 0.9238795325112869605, 1.000000000000000000, 0.9238795325112869605, 1.000000000000000000 ) ) 
 REPRESENTATION_ITEM ( '' )  ) ;
#37589 = VECTOR ( 'NONE', #45110, 39.37007874015748143 ) ;
#37590 = DIRECTION ( 'NONE',  ( -3.469446951953614189E-15, -1.000000000000000000, -1.118797478067273468E-31 ) ) ;
#37591 = LINE ( 'NONE', #19379, #17010 ) ;
#37592 = CARTESIAN_POINT ( 'NONE',  ( -0.1481685473978694711, -0.08955954485027488310, 0.07164615537806104384 ) ) ;
#37593 = ORIENTED_EDGE ( 'NONE', *, *, #32611, .F. ) ;
#37594 = CARTESIAN_POINT ( 'NONE',  ( 0.3547871005709968273, -0.09842519685039370636, 1.205361022782828805E-17 ) ) ;
#37595 = VECTOR ( 'NONE', #1316, 39.37007874015748143 ) ;
#37596 = AXIS2_PLACEMENT_3D ( 'NONE', #28316, #21101, #32145 ) ;
#37597 = CARTESIAN_POINT ( 'NONE',  ( 1.054774247047244540, -0.07405724077823318263, 0.7283464566391493200 ) ) ;
#37598 = ORIENTED_EDGE ( 'NONE', *, *, #7618, .F. ) ;
#37599 = CARTESIAN_POINT ( 'NONE',  ( -0.08994717584591646609, 0.09317026862874071280, -0.2335020446786553738 ) ) ;
#37600 = CARTESIAN_POINT ( 'NONE',  ( -0.8759842519685039353, 0.1574803149606299191, 0.4429133857192448787 ) ) ;
#37601 = CARTESIAN_POINT ( 'NONE',  ( 0.1787899950787401604, -1.671259842465922407, -0.07405724077823318263 ) ) ;
#37602 = CARTESIAN_POINT ( 'NONE',  ( -0.1264236179284866091, -0.8764763778989921317, -0.1264236179284866091 ) ) ;
#37603 = AXIS2_PLACEMENT_3D ( 'NONE', #33264, #15266, #30384 ) ;
#37604 = CARTESIAN_POINT ( 'NONE',  ( 0.1574803149606299191, -1.267716535433070835, -1.928577636452523993E-17 ) ) ;
#37605 = CARTESIAN_POINT ( 'NONE',  ( 0.8759842519685039353, -0.1574803149606299191, 1.171259842412157637 ) ) ;
#37606 = CARTESIAN_POINT ( 'NONE',  ( -0.4330708661417356775, 0.000000000000000000, -1.186023622047243986 ) ) ;
#37607 = EDGE_CURVE ( 'NONE', #31834, #9930, #13355, .T. ) ;
#37608 = VERTEX_POINT ( 'NONE', #46716 ) ;
#37609 = ORIENTED_EDGE ( 'NONE', *, *, #19244, .F. ) ;
#37610 = CARTESIAN_POINT ( 'NONE',  ( -0.9500414927467378812, 0.1787899950787401604, 1.806102362150961316 ) ) ;
#37611 = CARTESIAN_POINT ( 'NONE',  ( 0.8759842519685039353, 0.1787899950787401882, 1.769192913332062966 ) ) ;
#37612 = CARTESIAN_POINT ( 'NONE',  ( -0.1113553986120547346, -1.312007873908220379, 0.1113553986120547346 ) ) ;
#37613 = CARTESIAN_POINT ( 'NONE',  ( -0.09272654090491234957, -0.2419614285902609574, -0.3131151337379051713 ) ) ;
#37614 = CARTESIAN_POINT ( 'NONE',  ( 0.6971942568897626646, 0.07405724077823318263, 0.3592519684501735977 ) ) ;
#37615 = CARTESIAN_POINT ( 'NONE',  ( -0.6971942568897648851, -0.07405724077823297447, 1.382874015694268044 ) ) ;
#37616 = DIRECTION ( 'NONE',  ( 0.000000000000000000, -1.000000000000000000, 0.000000000000000000 ) ) ;
#37617 = CARTESIAN_POINT ( 'NONE',  ( -0.8019270111902716547, 0.1787899950787401604, 1.176181102308441195 ) ) ;
#37618 = CARTESIAN_POINT ( 'NONE',  ( -1.054774247047244540, 0.07405724077823318263, 0.9301181101824563813 ) ) ;
#37619 = CARTESIAN_POINT ( 'NONE',  ( -1.002407869896990045, 0.1264236179284866091, 0.03198818892261445085 ) ) ;
#37620 = ( BOUNDED_CURVE ( )  B_SPLINE_CURVE ( 2, ( #38219, #5379, #16192, #34180, #15964, #26992, #31057, #45622, #12839 ),
 .UNSPECIFIED., .F., .F. ) 
 B_SPLINE_CURVE_WITH_KNOTS ( ( 3, 2, 2, 2, 3 ),
 ( 0.9200000000000000400, 0.9224999999999999867, 0.9250000000000000444, 0.9274999999999999911, 0.9300000000000000488 ),
 .UNSPECIFIED. ) 
 CURVE ( )  GEOMETRIC_REPRESENTATION_ITEM ( )  RATIONAL_B_SPLINE_CURVE ( ( 1.000000000000000000, 0.9238795325112869605, 1.000000000000000000, 0.9238795325112869605, 1.000000000000000000, 0.9238795325112869605, 1.000000000000000000, 0.9238795325112829637, 1.000000000000000000 ) ) 
 REPRESENTATION_ITEM ( '' )  ) ;
#37621 = CARTESIAN_POINT ( 'NONE',  ( 0.03894127257533385594, 0.06746187776217156540, 0.2629503166621862120 ) ) ;
#37622 = CARTESIAN_POINT ( 'NONE',  ( -1.054774247047244540, 0.07405724077823318263, 1.722440944828125930 ) ) ;
#37623 = CARTESIAN_POINT ( 'NONE',  ( -1.054774247047244096, 0.000000000000000000, 0.1058070865604096300 ) ) ;
#37624 = CARTESIAN_POINT ( 'NONE',  ( 0.1574803149606300023, 1.126631386849005878, -3.440787370833236380 ) ) ;
#37626 = ( BOUNDED_CURVE ( )  B_SPLINE_CURVE ( 2, ( #19577, #34222, #27036, #5426, #20045, #34685, #16700, #23891, #9512 ),
 .UNSPECIFIED., .F., .F. ) 
 B_SPLINE_CURVE_WITH_KNOTS ( ( 3, 2, 2, 2, 3 ),
 ( 0.1199999999999999956, 0.1224999999999999978, 0.1250000000000000000, 0.1275000000000000022, 0.1300000000000000044 ),
 .UNSPECIFIED. ) 
 CURVE ( )  GEOMETRIC_REPRESENTATION_ITEM ( )  RATIONAL_B_SPLINE_CURVE ( ( 1.000000000000000000, 0.9238795325112869605, 1.000000000000000000, 0.9238795325112869605, 1.000000000000000000, 0.9238795325112869605, 1.000000000000000000, 0.9238795325112869605, 1.000000000000000000 ) ) 
 REPRESENTATION_ITEM ( '' )  ) ;
#37625 = CARTESIAN_POINT ( 'NONE',  ( -0.8759842519685039353, -0.1574803149606299191, 1.614173228346456712 ) ) ;
#37627 = CARTESIAN_POINT ( 'NONE',  ( 0.9500414927467377701, -0.1787899950787401604, 1.633858267662771091 ) ) ;
#37628 = CARTESIAN_POINT ( 'NONE',  ( -0.1459848668369287394, -0.09851383230118682111, 0.08268675942001851853 ) ) ;
#37629 = CARTESIAN_POINT ( 'NONE',  ( 0.8107537697050254399, 0.1574803149606300301, 0.2091535431995598104 ) ) ;
#37630 = DIRECTION ( 'NONE',  ( -0.5735764363510518216, 0.8191520442889876907, 1.003171929053519693E-16 ) ) ;
#37631 = ORIENTED_EDGE ( 'NONE', *, *, #24906, .F. ) ;
#37632 = AXIS2_PLACEMENT_3D ( 'NONE', #17912, #39234, #21022 ) ;
#37633 = ORIENTED_EDGE ( 'NONE', *, *, #39622, .T. ) ;
#37634 = APPLICATION_CONTEXT ( 'automotive_design' ) ;
#37635 = CARTESIAN_POINT ( 'NONE',  ( -1.054774247047244540, 0.07405724077823318263, 1.171259842465921741 ) ) ;
#37636 = ORIENTED_EDGE ( 'NONE', *, *, #25666, .F. ) ;
#37637 = CONICAL_SURFACE ( 'NONE', #42199, 0.1003937007874010356, 0.7853981633978647237 ) ;
#37638 = CARTESIAN_POINT ( 'NONE',  ( -0.1264236179284866091, -0.8371062991588346103, -0.1264236179284866091 ) ) ;
#37639 = CARTESIAN_POINT ( 'NONE',  ( 0.1264236179284866091, -1.078248031442299304, -0.1264236179284866091 ) ) ;
#37640 = ORIENTED_EDGE ( 'NONE', *, *, #19360, .T. ) ;
#37641 = CARTESIAN_POINT ( 'NONE',  ( -1.033464566929133799, 0.000000000000000000, 1.269685039370078705 ) ) ;
#37642 = CARTESIAN_POINT ( 'NONE',  ( 0.1270800023317771588, -0.3012249119452504176, 0.1270800023317771588 ) ) ;
#37643 = CARTESIAN_POINT ( 'NONE',  ( 0.1113553986120547346, -1.804133858160189119, -0.1113553986120547346 ) ) ;
#37644 = CARTESIAN_POINT ( 'NONE',  ( 0.06523048226347956391, 0.1422244094488189503, 0.1574803149606297803 ) ) ;
#37645 = CARTESIAN_POINT ( 'NONE',  ( 0.07405724077823318263, -0.1505905511273389341, 0.1787899950787401604 ) ) ;
#37646 = CARTESIAN_POINT ( 'NONE',  ( -1.033464566929134687, -0.06523048226347956391, 0.9030511809948349455 ) ) ;
#37647 = CARTESIAN_POINT ( 'NONE',  ( 0.6971942568897637749, 2.189545951927499583E-17, 0.7111220471903307860 ) ) ;
#37649 = CARTESIAN_POINT ( 'NONE',  ( -9.642888182262618425E-18, -0.02755905501058318954, -0.1574803149606299191 ) ) ;
#37648 = ( CONVERSION_BASED_UNIT ( 'INCH', #41442 ) LENGTH_UNIT ( ) NAMED_UNIT ( #24668 ) ) ;
#37650 = DIRECTION ( 'NONE',  ( -1.000000000000000000, 0.000000000000000000, 6.123233995736769734E-17 ) ) ;
#37651 = CARTESIAN_POINT ( 'NONE',  ( -0.3980944881889721398, 1.332209862199693839, -0.06082000038405668829 ) ) ;
#37652 = CARTESIAN_POINT ( 'NONE',  ( 0.9500414927467378812, 0.1787899950787401604, 1.845472440891119392 ) ) ;
#37653 = EDGE_CURVE ( 'NONE', #46488, #8877, #34613, .T. ) ;
#37654 = ORIENTED_EDGE ( 'NONE', *, *, #18826, .F. ) ;
#37655 = MECHANICAL_DESIGN_GEOMETRIC_PRESENTATION_REPRESENTATION (  '', ( #25436 ), #45297 ) ;
#37656 = CARTESIAN_POINT ( 'NONE',  ( 0.7646288533564489232, -0.1113553986120547346, 0.07381889763779526936 ) ) ;
#37657 = CARTESIAN_POINT ( 'NONE',  ( 0.1864803149606299171, 1.086379535891623949, -0.03715491745706173132 ) ) ;
#37658 = CARTESIAN_POINT ( 'NONE',  ( -0.07405724077823318263, -0.4458661416785199560, -0.1787899950787401604 ) ) ;
#37659 = CARTESIAN_POINT ( 'NONE',  ( 0.8107537697050234415, -0.1574803149606297803, 0.1156496062992125873 ) ) ;
#37660 = CARTESIAN_POINT ( 'NONE',  ( -0.07405724077823318263, -1.228346456639149542, -0.1787899950787401604 ) ) ;
#37661 = CARTESIAN_POINT ( 'NONE',  ( 1.054774247047244540, -0.07405724077823318263, 0.2214566928596220785 ) ) ;
#37662 = EDGE_CURVE ( 'NONE', #13298, #45388, #24572, .T. ) ;
#37663 = CARTESIAN_POINT ( 'NONE',  ( -0.6971942568897637749, 2.189545951927499583E-17, 1.695374015694267822 ) ) ;
#37664 = ORIENTED_EDGE ( 'NONE', *, *, #3086, .T. ) ;
#37665 = CARTESIAN_POINT ( 'NONE',  ( -0.6971942568897648851, -0.07405724077823297447, 1.309055118056472899 ) ) ;
#37666 = CARTESIAN_POINT ( 'NONE',  ( -0.8759842519685039353, 0.1574803149606299191, 1.318897637795275690 ) ) ;
#37667 = CARTESIAN_POINT ( 'NONE',  ( 0.8019270111902717657, 0.1787899950787401604, 1.259842519631276359 ) ) ;
#37668 = CARTESIAN_POINT ( 'NONE',  ( -0.8759842519685039353, 0.1787899950787401882, 0.5487204723871811352 ) ) ;
#37669 = VECTOR ( 'NONE', #6498, 39.37007874015748143 ) ;
#37670 = VECTOR ( 'NONE', #13272, 39.37007874015748143 ) ;
#37671 = CARTESIAN_POINT ( 'NONE',  ( -1.054774247047244540, -0.07405724077823318263, 1.200787401521039355 ) ) ;
#37672 = FACE_OUTER_BOUND ( 'NONE', #22151, .T. ) ;
#37673 = CARTESIAN_POINT ( 'NONE',  ( -0.1360271360007213048, -0.09844179429577380736, -0.1161711393741745174 ) ) ;
#37674 = CARTESIAN_POINT ( 'NONE',  ( 0.7185039370078746268, 0.06523048226347956391, 0.05659448808144944970 ) ) ;
#37675 = CARTESIAN_POINT ( 'NONE',  ( 1.054774247047244540, -0.07405724077823318263, 0.5364173227808820554 ) ) ;
#37676 = CARTESIAN_POINT ( 'NONE',  ( -0.8759842519685039353, -0.1787899950787401882, 0.4453740156942677664 ) ) ;
#37677 = EDGE_CURVE ( 'NONE', #35796, #15079, #4878, .T. ) ;
#37678 = DIRECTION ( 'NONE',  ( 0.000000000000000000, -1.000000000000000000, 0.000000000000000000 ) ) ;
#37679 = ORIENTED_EDGE ( 'NONE', *, *, #41029, .F. ) ;
#37680 = ORIENTED_EDGE ( 'NONE', *, *, #4417, .F. ) ;
#37681 = CARTESIAN_POINT ( 'NONE',  ( -0.8759842519685039353, 0.1574803149606299191, 0.1771653543307086520 ) ) ;
#37682 = CARTESIAN_POINT ( 'NONE',  ( 0.6971942568897637749, 2.189545951927499583E-17, 1.149114173174582643 ) ) ;
#37683 = CARTESIAN_POINT ( 'NONE',  ( 0.9412147342319837628, 0.1574803149606300301, 1.936515747923967412 ) ) ;
#37684 = CARTESIAN_POINT ( 'NONE',  ( -0.2559055118110235560, -0.04381123493339342950, -0.03538144886923444421 ) ) ;
#37685 = EDGE_LOOP ( 'NONE', ( #42617, #33463, #42128, #34070, #36690 ) ) ;
#37686 = DIRECTION ( 'NONE',  ( 0.000000000000000000, 0.000000000000000000, 1.000000000000000000 ) ) ;
#37687 = CYLINDRICAL_SURFACE ( 'NONE', #18884, 0.1574803149606299191 ) ;
#37688 = CARTESIAN_POINT ( 'NONE',  ( 0.7646288533564489232, -0.1113553986120547346, 0.3100393700787401619 ) ) ;
#37689 = CARTESIAN_POINT ( 'NONE',  ( -1.094772975963752103E-17, -1.404159401300104415, -0.1787899950787401882 ) ) ;
#37690 = VERTEX_POINT ( 'NONE', #34857 ) ;
#37691 = CARTESIAN_POINT ( 'NONE',  ( -1.094772975963752103E-17, -0.4827755904974173617, -0.1787899950787401882 ) ) ;
#37692 = CARTESIAN_POINT ( 'NONE',  ( -0.3100393700787401619, -2.714815113292586694E-26, 1.043307086614172707 ) ) ;
#37693 = ORIENTED_EDGE ( 'NONE', *, *, #3786, .T. ) ;
#37694 = CARTESIAN_POINT ( 'NONE',  ( 0.7495606340400177148, -0.1264236179284866091, 1.306594488135212728 ) ) ;
#37695 = CARTESIAN_POINT ( 'NONE',  ( -0.1171060910373939445, 0.2278812977176828125, -0.3148284977848753718 ) ) ;
#37696 = CARTESIAN_POINT ( 'NONE',  ( 1.033464566929134687, -0.06523048226347956391, 0.7455708660342049710 ) ) ;
#37697 = AXIS2_PLACEMENT_3D ( 'NONE', #24532, #27697, #9460 ) ;
#37698 = CARTESIAN_POINT ( 'NONE',  ( 0.9500414927467378812, 0.1787899950787401604, 1.564960629867495845 ) ) ;
#37699 = CARTESIAN_POINT ( 'NONE',  ( 0.9500414927467378812, -0.1787899950787401604, 0.1328740156942679607 ) ) ;
#37700 = CONICAL_SURFACE ( 'NONE', #30861, 0.1574803149606299191, 0.9599310885968735940 ) ;
#37701 = CARTESIAN_POINT ( 'NONE',  ( -0.1787899950787401882, -1.816437007820251859, 0.000000000000000000 ) ) ;
#37702 = CARTESIAN_POINT ( 'NONE',  ( 0.1787899950787401604, -1.794291338528913426, 0.07405724077823318263 ) ) ;
#37703 = EDGE_CURVE ( 'NONE', #11244, #26454, #14785, .T. ) ;
#37704 = DIRECTION ( 'NONE',  ( 0.000000000000000000, 1.000000000000000000, 0.000000000000000000 ) ) ;
#37705 = CARTESIAN_POINT ( 'NONE',  ( -0.6971942568897648851, -0.07405724077823297447, 0.6791338582139527791 ) ) ;
#37706 = ADVANCED_FACE ( 'NONE', ( #1514 ), #10337, .F. ) ;
#37707 = CARTESIAN_POINT ( 'NONE',  ( -0.1574803149606299191, -0.6968503937007873850, 0.000000000000000000 ) ) ;
#37708 = CARTESIAN_POINT ( 'NONE',  ( 0.1797182628040039365, -1.398665856827139731, -2.200913952912460540E-17 ) ) ;
#37709 = CARTESIAN_POINT ( 'NONE',  ( -0.7185039370078766252, -0.06523048226348168721, 1.596948818790109970 ) ) ;
#37710 = CARTESIAN_POINT ( 'NONE',  ( -9.642888182262618425E-18, -0.4606299211523149362, -0.1574803149606299191 ) ) ;
#37711 = CIRCLE ( 'NONE', #21710, 0.7874015748031496509 ) ;
#37712 = LINE ( 'NONE', #33911, #13887 ) ;
#37713 = CARTESIAN_POINT ( 'NONE',  ( 0.8759842519685039353, -0.1787899950787401882, 1.395177165300567124 ) ) ;
#37714 = CARTESIAN_POINT ( 'NONE',  ( 0.6971942568897637749, 2.189545951927499583E-17, 1.813484251914740053 ) ) ;
#37715 = CARTESIAN_POINT ( 'NONE',  ( 1.054774247047244096, 0.000000000000000000, 0.2977362204186775885 ) ) ;
#37716 = ADVANCED_FACE ( 'NONE', ( #3106 ), #39752, .F. ) ;
#37718 = EDGE_LOOP ( 'NONE', ( #34750, #3911, #24363, #26486 ) ) ;
#37717 = LINE ( 'NONE', #4868, #23746 ) ;
#37720 = CARTESIAN_POINT ( 'NONE',  ( -0.7466676322263418042, 0.09839106858983247272, 1.981216915731769612 ) ) ;
#37719 = CARTESIAN_POINT ( 'NONE',  ( 0.8759842519685039353, 0.000000000000000000, 4.498031496062992574 ) ) ;
#37721 = DIRECTION ( 'NONE',  ( 1.822029033848725028E-16, 0.000000000000000000, 1.000000000000000000 ) ) ;
#37722 = CARTESIAN_POINT ( 'NONE',  ( -0.07405724077823318263, -0.03740157474938609478, 0.1787899950787401604 ) ) ;
#37723 = CARTESIAN_POINT ( 'NONE',  ( 0.6971942568897626646, -0.07405724077823297447, 0.3592519684501735977 ) ) ;
#37724 = CARTESIAN_POINT ( 'NONE',  ( 0.9412147342319837628, 0.1574803149606300301, 1.975885826664125711 ) ) ;
#37725 = CARTESIAN_POINT ( 'NONE',  ( 0.7185039370078746268, 0.06523048226347956391, 0.8538385826771661691 ) ) ;
#37726 = CARTESIAN_POINT ( 'NONE',  ( 0.1377952755905510751, 0.000000000000000000, -0.3149606299212598381 ) ) ;
#37727 = CARTESIAN_POINT ( 'NONE',  ( -0.6971942568897648851, -0.07405724077823297447, 1.304133858213953667 ) ) ;
#37728 = CARTESIAN_POINT ( 'NONE',  ( 0.7646288533564489232, -0.1113553986120547346, 0.7332677164279054471 ) ) ;
#37729 = ORIENTED_EDGE ( 'NONE', *, *, #14079, .F. ) ;
#37730 = CARTESIAN_POINT ( 'NONE',  ( 0.8432997816974205918, 0.1735131131385767855, 0.03937007914154261323 ) ) ;
#37731 = ORIENTED_EDGE ( 'NONE', *, *, #623, .T. ) ;
#37732 = CARTESIAN_POINT ( 'NONE',  ( -0.1797182628040039087, -0.03793751037044712504, 0.07444174185955065859 ) ) ;
#37733 = CARTESIAN_POINT ( 'NONE',  ( 0.1264236179284866091, -1.250492125930488196, 0.1264236179284866091 ) ) ;
#37734 = CARTESIAN_POINT ( 'NONE',  ( -0.8759842519685039353, 0.1574803149606299191, 0.8070866141732283561 ) ) ;
#37735 = CARTESIAN_POINT ( 'NONE',  ( 0.8759842519685039353, -0.1787899950787401882, 1.547736220418677089 ) ) ;
#37736 = CARTESIAN_POINT ( 'NONE',  ( -0.8107537697050253289, 0.1574803149606300301, 1.203248031496062520 ) ) ;
#37737 = DIRECTION ( 'NONE',  ( 0.000000000000000000, 0.000000000000000000, 1.000000000000000000 ) ) ;
#37739 = CARTESIAN_POINT ( 'NONE',  ( -2.458663194297838277E-15, -0.2954942322624074524, -0.1122047244094488277 ) ) ;
#37738 = DIRECTION ( 'NONE',  ( 0.000000000000000000, 0.000000000000000000, 1.000000000000000000 ) ) ;
#37740 = CARTESIAN_POINT ( 'NONE',  ( -0.1574803149606299191, 1.117014023967196401, -3.442880580079819008 ) ) ;
#37741 = ORIENTED_EDGE ( 'NONE', *, *, #37772, .F. ) ;
#37742 = ORIENTED_EDGE ( 'NONE', *, *, #8812, .F. ) ;
#37743 = ( BOUNDED_CURVE ( )  B_SPLINE_CURVE ( 2, ( #7110, #21734, #22612, #39451, #37225, #4371, #36994, #35871, #19001 ),
 .UNSPECIFIED., .F., .T. ) 
 B_SPLINE_CURVE_WITH_KNOTS ( ( 3, 2, 2, 2, 3 ),
 ( 0.6700000000000000400, 0.6724999999999999867, 0.6750000000000000444, 0.6774999999999999911, 0.6800000000000000488 ),
 .UNSPECIFIED. ) 
 CURVE ( )  GEOMETRIC_REPRESENTATION_ITEM ( )  RATIONAL_B_SPLINE_CURVE ( ( 1.000000000000000000, 0.9238795325112869605, 1.000000000000000000, 0.9238795325112869605, 1.000000000000000000, 0.9238795325112869605, 1.000000000000000000, 0.9238795325112869605, 1.000000000000000000 ) ) 
 REPRESENTATION_ITEM ( '' )  ) ;
#37744 = AXIS2_PLACEMENT_3D ( 'NONE', #37467, #41260, #19249 ) ;
#37745 = CARTESIAN_POINT ( 'NONE',  ( -0.1574803149606300301, -0.05954724398696115140, -0.06523048226347956391 ) ) ;
#37746 = CARTESIAN_POINT ( 'NONE',  ( -1.054774247047244540, -0.07405724077823318263, 1.245078740103716886 ) ) ;
#37747 = PRODUCT_DEFINITION_FORMATION_WITH_SPECIFIED_SOURCE ( 'ANY', '', #24326, .NOT_KNOWN. ) ;
#37748 = CIRCLE ( 'NONE', #17065, 0.1574803149606299191 ) ;
#37749 = ORIENTED_EDGE ( 'NONE', *, *, #13004, .T. ) ;
#37750 = CIRCLE ( 'NONE', #41649, 0.08090551181102362266 ) ;
#37751 = CYLINDRICAL_SURFACE ( 'NONE', #13828, 0.1574803149606299191 ) ;
#37752 = CARTESIAN_POINT ( 'NONE',  ( -1.002407869896990045, 0.1264236179284866091, 0.3075787401037169411 ) ) ;
#37753 = CARTESIAN_POINT ( 'NONE',  ( 0.1574803149606299746, 0.1473293504822046074, -0.5595480905233950475 ) ) ;
#37754 = CARTESIAN_POINT ( 'NONE',  ( -0.7185039370078739607, 1.928577636452523993E-17, 1.210629921259842590 ) ) ;
#37755 = CARTESIAN_POINT ( 'NONE',  ( -0.1264236179284866091, -0.9169546768906554624, 0.1264236179284866091 ) ) ;
#37756 = ORIENTED_EDGE ( 'NONE', *, *, #27723, .F. ) ;
#37757 = CARTESIAN_POINT ( 'NONE',  ( -0.1787899950787401604, -0.002952755851748307785, -0.07405724077823318263 ) ) ;
#37758 = ORIENTED_EDGE ( 'NONE', *, *, #16832, .T. ) ;
#37759 = EDGE_LOOP ( 'NONE', ( #45684, #30175, #45653, #4658 ) ) ;
#37760 = CARTESIAN_POINT ( 'NONE',  ( 0.008612976559017233164, -0.06611238040515819703, 0.1377923257425126835 ) ) ;
#37761 = DIRECTION ( 'NONE',  ( 0.000000000000000000, 0.000000000000000000, -1.000000000000000000 ) ) ;
#37762 = CYLINDRICAL_SURFACE ( 'NONE', #17838, 0.1574803149606299191 ) ;
#37763 = CARTESIAN_POINT ( 'NONE',  ( 0.1787899950787401604, -0.6968503936470246130, 0.07405724077823318263 ) ) ;
#37764 = EDGE_CURVE ( 'NONE', #4939, #43211, #26411, .T. ) ;
#37765 = ADVANCED_FACE ( 'NONE', ( #43359 ), #32620, .T. ) ;
#37766 = CARTESIAN_POINT ( 'NONE',  ( -0.9412147342319837628, -0.1574803149606297803, 0.8686023622047237547 ) ) ;
#37767 = DIRECTION ( 'NONE',  ( 0.000000000000000000, -1.000000000000000000, 0.000000000000000000 ) ) ;
#37768 = CARTESIAN_POINT ( 'NONE',  ( -0.1797182628040039365, -1.024650108795643666, 0.000000000000000000 ) ) ;
#37769 = DIRECTION ( 'NONE',  ( -1.000000000000000000, 0.000000000000000000, 0.000000000000000000 ) ) ;
#37770 = CARTESIAN_POINT ( 'NONE',  ( 0.8759842519685039353, -0.1787899950787401882, 1.001476377898992132 ) ) ;
#37771 = CARTESIAN_POINT ( 'NONE',  ( 0.8759842519685039353, -0.1787899950787401882, 1.390255905458047447 ) ) ;
#37772 = EDGE_CURVE ( 'NONE', #15853, #26252, #24129, .T. ) ;
#37773 = VECTOR ( 'NONE', #16032, 39.37007874015748143 ) ;
#37774 = EDGE_CURVE ( 'NONE', #15018, #38595, #15681, .T. ) ;
#37775 = DIRECTION ( 'NONE',  ( 0.000000000000000000, 0.000000000000000000, -1.000000000000000000 ) ) ;
#37776 = CARTESIAN_POINT ( 'NONE',  ( 0.9873396505805591694, -0.1113553986120547346, 1.500984251968503935 ) ) ;
#37777 = CARTESIAN_POINT ( 'NONE',  ( 0.7100468655899934145, 0.001942326053023950760, 1.983232204919558761 ) ) ;
#37778 = CARTESIAN_POINT ( 'NONE',  ( 0.1476377952755906220, -0.4075443641102559078, -0.9311509272141712534 ) ) ;
#37779 = CARTESIAN_POINT ( 'NONE',  ( 0.1574803149606300301, -0.6697834644594027331, 0.06523048226347956391 ) ) ;
#37780 = CARTESIAN_POINT ( 'NONE',  ( 0.07405724077823318263, 0.1053149606836847191, -0.1787899950787401604 ) ) ;
#37781 = DIRECTION ( 'NONE',  ( 1.000000000000000000, -0.000000000000000000, -0.000000000000000000 ) ) ;
#37783 = CARTESIAN_POINT ( 'NONE',  ( 1.033464566929133799, 1.928577636452524610E-17, 4.498031496062992574 ) ) ;
#37782 = CARTESIAN_POINT ( 'NONE',  ( 0.8019270111902716547, 0.1787899950787401604, 1.018700787347811110 ) ) ;
#37784 = CARTESIAN_POINT ( 'NONE',  ( 1.054774247047244096, 0.000000000000000000, 1.798720472387181024 ) ) ;
#37785 = CARTESIAN_POINT ( 'NONE',  ( -0.07405724077823318263, -0.9379921259304876413, 0.1787899950787401604 ) ) ;
#37786 = CARTESIAN_POINT ( 'NONE',  ( -0.1377952755905513804, 0.000000000000000000, -0.3001770169643759867 ) ) ;
#37787 = ORIENTED_EDGE ( 'NONE', *, *, #22998, .T. ) ;
#37788 = CARTESIAN_POINT ( 'NONE',  ( 0.8107537697050254399, 0.1574803149606300301, 1.085137795275590955 ) ) ;
#37789 = CARTESIAN_POINT ( 'NONE',  ( 0.3302522695077432791, -3.032960542342102697E-32, 0.09842519685039370636 ) ) ;
#37790 = CARTESIAN_POINT ( 'NONE',  ( -9.642888182262618425E-18, -1.759842519577511810, -0.1574803149606299191 ) ) ;
#37791 = CARTESIAN_POINT ( 'NONE',  ( -0.7646288533564489232, 0.1113553986120547346, 0.09350393690034704275 ) ) ;
#37792 = CARTESIAN_POINT ( 'NONE',  ( -8.354793841626791791E-17, -0.09842519685039370636, -0.2854330708661417804 ) ) ;
#37793 = CARTESIAN_POINT ( 'NONE',  ( 0.6971942568897648851, 0.07405724077823318263, 1.102362204670646495 ) ) ;
#37794 = CARTESIAN_POINT ( 'NONE',  ( 0.1574803149606299191, 0.000000000000000000, 0.000000000000000000 ) ) ;
#37795 = CARTESIAN_POINT ( 'NONE',  ( 0.1574803149606300301, -1.619586614173227579, -0.06523048226347956391 ) ) ;
#37796 = CARTESIAN_POINT ( 'NONE',  ( 0.1555687797274980522, 0.09281549603114055969, -0.1148293963254594513 ) ) ;
#37797 = DIRECTION ( 'NONE',  ( 1.000000000000000000, 0.000000000000000000, 0.000000000000000000 ) ) ;
#37798 = CARTESIAN_POINT ( 'NONE',  ( -0.7495606340400177148, 0.1264236179284866091, 0.2337598424659216578 ) ) ;
#37800 = CARTESIAN_POINT ( 'NONE',  ( -0.1264236179284866091, -1.545767716481669218, -0.1264236179284866091 ) ) ;
#37799 = CARTESIAN_POINT ( 'NONE',  ( -0.1113553986120547346, -0.3375984250893232508, -0.1113553986120547346 ) ) ;
#37801 = CARTESIAN_POINT ( 'NONE',  ( -0.9500414927467378812, 0.1787899950787401604, 1.879921259788756016 ) ) ;
#37802 = CARTESIAN_POINT ( 'NONE',  ( -1.054774247047244096, 0.000000000000000000, 0.9670275590013542866 ) ) ;
#37803 = ADVANCED_FACE ( 'NONE', ( #28550 ), #18439, .T. ) ;
#37804 = CARTESIAN_POINT ( 'NONE',  ( -1.054774247047244096, 0.000000000000000000, 0.4995078739619842612 ) ) ;
#37805 = DIRECTION ( 'NONE',  ( -1.000000000000000000, 0.000000000000000000, 0.000000000000000000 ) ) ;
#37806 = CARTESIAN_POINT ( 'NONE',  ( 0.1377952755905511861, 0.1574803149606299191, 0.9084645669291339098 ) ) ;
#37807 = DIRECTION ( 'NONE',  ( -1.000000000000000000, 0.000000000000000000, 0.000000000000000000 ) ) ;
#37808 = CARTESIAN_POINT ( 'NONE',  ( -0.7646288533564489232, 0.1113553986120547346, 1.678149606299212726 ) ) ;
#37809 = CARTESIAN_POINT ( 'NONE',  ( -0.1787899950787401604, -0.5306357792528606510, -0.07405724077823318263 ) ) ;
#37810 = CARTESIAN_POINT ( 'NONE',  ( 0.08588050461400061064, -0.08956016273386613324, 0.1986011934319732164 ) ) ;
#37811 = CARTESIAN_POINT ( 'NONE',  ( -9.642888182262618425E-18, 0.05118110246973173183, -0.1574803149606299191 ) ) ;
#37812 = CARTESIAN_POINT ( 'NONE',  ( 0.8759842519685039353, 0.1574803149606299191, 1.791338582677165281 ) ) ;
#37813 = CARTESIAN_POINT ( 'NONE',  ( 0.7185039370078739607, 0.000000000000000000, 4.498031496062992574 ) ) ;
#37814 = CARTESIAN_POINT ( 'NONE',  ( -0.7185039370078766252, -0.06523048226348168721, 1.163877952648377567 ) ) ;
#37815 = CARTESIAN_POINT ( 'NONE',  ( -0.8759842519685039353, -0.1787899950787401882, 0.4453740156942677664 ) ) ;
#37816 = CARTESIAN_POINT ( 'NONE',  ( 0.9412147342319837628, 0.1574803149606300301, 1.188484251860977503 ) ) ;
#37817 = VERTEX_POINT ( 'NONE', #11037 ) ;
#37818 = CARTESIAN_POINT ( 'NONE',  ( 0.2471922963015218966, -0.09312803950197923175, 0.03901180619690218510 ) ) ;
#37819 = AXIS2_PLACEMENT_3D ( 'NONE', #42850, #35246, #2840 ) ;
#37820 = CARTESIAN_POINT ( 'NONE',  ( -0.6971942568897648851, -0.07405724077823297447, 1.584645669237574994 ) ) ;
#37821 = CARTESIAN_POINT ( 'NONE',  ( -0.07405724077823318263, -1.508858267662772867, -0.1787899950787401604 ) ) ;
#37822 = CARTESIAN_POINT ( 'NONE',  ( -0.1787899950787401882, -1.535925196796629866, 0.000000000000000000 ) ) ;
#37823 = EDGE_CURVE ( 'NONE', #752, #21809, #17198, .T. ) ;
#37824 = CARTESIAN_POINT ( 'NONE',  ( 0.1476377952755906220, 1.126631386849005878, -3.440787370833236380 ) ) ;
#37825 = CARTESIAN_POINT ( 'NONE',  ( 0.1619802298358933301, -0.07975797990935330761, 0.1381390393564600749 ) ) ;
#37826 = ORIENTED_EDGE ( 'NONE', *, *, #14578, .F. ) ;
#37827 = CARTESIAN_POINT ( 'NONE',  ( 0.7646288533564489232, 0.1113553986120547346, 0.4970472440944882497 ) ) ;
#37828 = LINE ( 'NONE', #1375, #18665 ) ;
#37829 = CARTESIAN_POINT ( 'NONE',  ( -0.8759842519685039353, 0.1574803149606299191, 1.269685039262551163 ) ) ;
#37830 = CARTESIAN_POINT ( 'NONE',  ( 0.9500414927467378812, -0.1787899950787401604, 0.5708661416785201226 ) ) ;
#37832 = CARTESIAN_POINT ( 'NONE',  ( 0.8107537697050254399, -0.1574803149606297803, 1.759350393593260842 ) ) ;
#37831 = CARTESIAN_POINT ( 'NONE',  ( 0.1574803149606299191, -0.2440944881889763884, -1.928577636452523993E-17 ) ) ;
#37833 = CARTESIAN_POINT ( 'NONE',  ( 0.9412147342319837628, 0.1574803149606300301, 1.897145669183811778 ) ) ;
#37834 = ORIENTED_EDGE ( 'NONE', *, *, #23762, .T. ) ;
#37835 = EDGE_CURVE ( 'NONE', #10222, #43268, #12673, .T. ) ;
#37836 = CARTESIAN_POINT ( 'NONE',  ( -0.1267356318029559670, -0.09168894753733079772, -0.1261112482890841824 ) ) ;
#37837 = CARTESIAN_POINT ( 'NONE',  ( -1.054774247047244540, 0.07405724077823318263, 1.053149606245450176 ) ) ;
#37838 = CARTESIAN_POINT ( 'NONE',  ( 0.7646288533564489232, 0.1113553986120547346, 1.166338582677165281 ) ) ;
#37839 = CARTESIAN_POINT ( 'NONE',  ( -0.7646288533564489232, 0.1113553986120547346, 0.7234251967428662056 ) ) ;
#37840 = DIRECTION ( 'NONE',  ( -0.000000000000000000, 0.000000000000000000, 1.000000000000000000 ) ) ;
#37841 = FACE_OUTER_BOUND ( 'NONE', #30817, .T. ) ;
#37842 = CARTESIAN_POINT ( 'NONE',  ( -0.09445526594068323623, -0.08956264882496832447, 0.1283258905068025424 ) ) ;
#37844 = AXIS2_PLACEMENT_3D ( 'NONE', #5687, #20299, #2087 ) ;
#37843 = CARTESIAN_POINT ( 'NONE',  ( -0.1787899950787401604, -0.5098425196312756924, 0.07405724077823318263 ) ) ;
#37845 = VERTEX_POINT ( 'NONE', #10806 ) ;
#37846 = DIRECTION ( 'NONE',  ( 1.000000000000000000, 0.000000000000000000, 0.000000000000000000 ) ) ;
#37847 = VECTOR ( 'NONE', #17604, 39.37007874015748143 ) ;
#37848 = AXIS2_PLACEMENT_3D ( 'NONE', #46708, #39520, #21312 ) ;
#37849 = CARTESIAN_POINT ( 'NONE',  ( 0.9412147342319837628, 0.1574803149606300301, 1.158956692913385655 ) ) ;
#37850 = EDGE_LOOP ( 'NONE', ( #40699, #38487, #46550, #11399, #29360 ) ) ;
#37851 = CARTESIAN_POINT ( 'NONE',  ( -0.7185039370078714072, 0.06523048226347728795, 1.788877952648379122 ) ) ;
#37852 = CARTESIAN_POINT ( 'NONE',  ( 0.7185039370078746268, -0.06523048226347956391, 0.8981299212598432558 ) ) ;
#37853 = CARTESIAN_POINT ( 'NONE',  ( -0.1264236179284866091, -0.8666338582139527791, 0.1264236179284866091 ) ) ;
#37854 = CARTESIAN_POINT ( 'NONE',  ( -0.1574803149606299191, -1.169291338582677309, 0.000000000000000000 ) ) ;
#37855 = CARTESIAN_POINT ( 'NONE',  ( 1.033464566929134687, -0.06523048226347956391, 1.139271653435780962 ) ) ;
#37856 = CARTESIAN_POINT ( 'NONE',  ( 0.2698848154395015464, 4.466152701071653354E-17, 0.000000000000000000 ) ) ;
#37857 = ORIENTED_EDGE ( 'NONE', *, *, #8571, .F. ) ;
#37858 = ORIENTED_EDGE ( 'NONE', *, *, #34649, .T. ) ;
#37859 = AXIS2_PLACEMENT_3D ( 'NONE', #38200, #34621, #1771 ) ;
#37860 = CARTESIAN_POINT ( 'NONE',  ( -0.9500414927467378812, -0.1787899950787401604, 1.791338582623401177 ) ) ;
#37861 = CARTESIAN_POINT ( 'NONE',  ( 1.002407869896990045, 0.1264236179284866091, 1.803641732229700700 ) ) ;
#37862 = ORIENTED_EDGE ( 'NONE', *, *, #23048, .T. ) ;
#37863 = CARTESIAN_POINT ( 'NONE',  ( -0.06523048226347956391, -1.388287401467275917, 0.1574803149606297803 ) ) ;
#37864 = CARTESIAN_POINT ( 'NONE',  ( -0.8759842519685039353, -0.1787899950787401882, 0.8833661416785196785 ) ) ;
#37865 = CARTESIAN_POINT ( 'NONE',  ( -0.5555748031496052786, 0.4370297686271554238, 0.6367018223237034258 ) ) ;
#37866 = CARTESIAN_POINT ( 'NONE',  ( 1.002407869896990045, 0.1264236179284866091, 0.3863188975840318173 ) ) ;
#37867 = CARTESIAN_POINT ( 'NONE',  ( -1.002407869896990045, 0.1264236179284866091, 1.365649606245448844 ) ) ;
#37868 = CARTESIAN_POINT ( 'NONE',  ( 0.8070866141732283561, -0.0009842519685049383633, -0.7574803149606299524 ) ) ;
#37869 = CARTESIAN_POINT ( 'NONE',  ( -0.7495606340400177148, 0.1264236179284866091, 1.257381889710015743 ) ) ;
#37870 = CARTESIAN_POINT ( 'NONE',  ( -0.8759842519685039353, -0.1787899950787401882, 0.1353346456155279653 ) ) ;
#37871 = CARTESIAN_POINT ( 'NONE',  ( -0.8107537697050254399, 0.1574803149606300301, 0.5733267716535435099 ) ) ;
#37872 = CARTESIAN_POINT ( 'NONE',  ( -0.8759842519685039353, 0.1787899950787401882, 1.808562992072220377 ) ) ;
#37873 = CARTESIAN_POINT ( 'NONE',  ( -0.8019270111902717657, -0.1787899950787401604, 0.09350393695411057804 ) ) ;
#37874 = LINE ( 'NONE', #19649, #39387 ) ;
#37875 = CARTESIAN_POINT ( 'NONE',  ( -1.033464566929133799, 0.000000000000000000, 1.781496062992125928 ) ) ;
#37876 = CARTESIAN_POINT ( 'NONE',  ( -0.9873396505805591694, 0.1113553986120547346, 0.2903543307086614012 ) ) ;
#37877 = CARTESIAN_POINT ( 'NONE',  ( 0.6971942568897637749, 2.189545951927499583E-17, 1.542814960576157413 ) ) ;
#37878 = CARTESIAN_POINT ( 'NONE',  ( -0.1097920307064556983, -0.09842519685039370636, -0.2293370477459909240 ) ) ;
#37879 = CARTESIAN_POINT ( 'NONE',  ( 0.7185039370078739607, 1.928577636452523993E-17, 0.2165354329633393804 ) ) ;
#37880 = ORIENTED_EDGE ( 'NONE', *, *, #12646, .T. ) ;
#37881 = CONICAL_SURFACE ( 'NONE', #34847, 0.09842519685039370636, 0.9599310885968824758 ) ;
#37882 = VECTOR ( 'NONE', #35650, 39.37007874015748143 ) ;
#37883 = CARTESIAN_POINT ( 'NONE',  ( -0.1264236179284866091, -0.9453740156942677109, 0.1264236179284866091 ) ) ;
#37884 = CARTESIAN_POINT ( 'NONE',  ( 0.1264236179284866091, -0.9995078739619842612, -0.1264236179284866091 ) ) ;
#37885 = EDGE_CURVE ( 'NONE', #32335, #8877, #45682, .T. ) ;
#37886 = CARTESIAN_POINT ( 'NONE',  ( 0.1797182628040039087, -0.3332131009216283135, -0.07444174185955065859 ) ) ;
#37887 = CARTESIAN_POINT ( 'NONE',  ( -0.1113553986120547346, -1.794291338475149766, -0.1113553986120547346 ) ) ;
#37888 = CARTESIAN_POINT ( 'NONE',  ( -9.642888182262618425E-18, 0.1594488188976377896, -0.1574803149606299191 ) ) ;
#37889 = CARTESIAN_POINT ( 'NONE',  ( 0.07405724077823318263, -0.1751968503399373434, -0.1787899950787401604 ) ) ;
#37890 = EDGE_CURVE ( 'NONE', #43867, #11471, #44429, .T. ) ;
#37891 = CARTESIAN_POINT ( 'NONE',  ( -0.8759842519685039353, -0.1574803149606299191, 0.8956692912310552090 ) ) ;
#37892 = CARTESIAN_POINT ( 'NONE',  ( 0.8759842519685039353, 0.1787899950787401882, 0.7012795275052913224 ) ) ;
#37894 = CARTESIAN_POINT ( 'NONE',  ( 0.7185039370078739607, 1.928577636452523993E-17, 1.210629921259842590 ) ) ;
#37893 = DIRECTION ( 'NONE',  ( -0.5735764363510518216, -0.8191520442889876907, 0.000000000000000000 ) ) ;
#37895 = CARTESIAN_POINT ( 'NONE',  ( 1.033464566929133799, 0.000000000000000000, 0.4429133858267716439 ) ) ;
#37896 = CARTESIAN_POINT ( 'NONE',  ( 0.8019270111902717657, 0.1787899950787401604, 1.968503936954110189 ) ) ;
#37897 = CARTESIAN_POINT ( 'NONE',  ( 0.9873396505805591694, -0.1113553986120547346, 0.04429133858267716300 ) ) ;
#37898 = CARTESIAN_POINT ( 'NONE',  ( 0.000000000000000000, 0.000000000000000000, -0.0009999999999999347518 ) ) ;
#37899 = CARTESIAN_POINT ( 'NONE',  ( -0.1787899950787401604, -0.3622047243556850704, -0.07405724077823318263 ) ) ;
#37900 = CARTESIAN_POINT ( 'NONE',  ( 1.033464566929134687, -0.06523048226347956391, 0.1254921259842521064 ) ) ;
#37901 = CARTESIAN_POINT ( 'NONE',  ( -0.1787899950787401882, -1.181594488135212506, 0.000000000000000000 ) ) ;
#37902 = ( BOUNDED_CURVE ( )  B_SPLINE_CURVE ( 2, ( #38641, #31232, #45810, #44922, #27659, #8279, #8517, #833, #11668 ),
 .UNSPECIFIED., .F., .F. ) 
 B_SPLINE_CURVE_WITH_KNOTS ( ( 3, 2, 2, 2, 3 ),
 ( 0.9000000000000000222, 0.9024999999999999689, 0.9050000000000000266, 0.9074999999999999734, 0.9100000000000000311 ),
 .UNSPECIFIED. ) 
 CURVE ( )  GEOMETRIC_REPRESENTATION_ITEM ( )  RATIONAL_B_SPLINE_CURVE ( ( 1.000000000000000000, 0.9238795325112869605, 1.000000000000000000, 0.9238795325112869605, 1.000000000000000000, 0.9238795325112869605, 1.000000000000000000, 0.9238795325112829637, 1.000000000000000000 ) ) 
 REPRESENTATION_ITEM ( '' )  ) ;
#37903 = CARTESIAN_POINT ( 'NONE',  ( 0.9500414927467378812, -0.1787899950787401604, 0.2165354330171024577 ) ) ;
#37904 = CARTESIAN_POINT ( 'NONE',  ( -0.8759842519685039353, -0.1787899950787401882, 1.705216535379307174 ) ) ;
#37905 = ORIENTED_EDGE ( 'NONE', *, *, #43280, .F. ) ;
#37906 = VECTOR ( 'NONE', #17239, 39.37007874015748143 ) ;
#37907 = CARTESIAN_POINT ( 'NONE',  ( -0.9500414927467378812, -0.1787899950787401604, 1.318897637741511364 ) ) ;
#37908 = CARTESIAN_POINT ( 'NONE',  ( -1.033464566929133799, 0.000000000000000000, 1.309055118110236338 ) ) ;
#37909 = CARTESIAN_POINT ( 'NONE',  ( 0.6971942568897648851, 0.07405724077823318263, 1.461614173174583753 ) ) ;
#37910 = AXIS2_PLACEMENT_3D ( 'NONE', #5813, #35298, #20422 ) ;
#37911 = AXIS2_PLACEMENT_3D ( 'NONE', #11411, #37040, #11657 ) ;
#37912 = CARTESIAN_POINT ( 'NONE',  ( -0.8759842519685039353, -0.1787899950787401882, 1.193405511757259951 ) ) ;
#37913 = DIRECTION ( 'NONE',  ( 0.000000000000000000, 0.000000000000000000, -1.000000000000000000 ) ) ;
#37914 = CARTESIAN_POINT ( 'NONE',  ( 0.03838706947536870556, -0.09842268942605733595, -0.1746209144150240034 ) ) ;
#37915 = CARTESIAN_POINT ( 'NONE',  ( 0.8759842519685039353, 0.1574803149606299191, 0.04921259831766984505 ) ) ;
#37916 = CARTESIAN_POINT ( 'NONE',  ( 0.9500414927467377701, -0.1787899950787401604, 0.4921259841982049132 ) ) ;
#37917 = CARTESIAN_POINT ( 'NONE',  ( -0.9500414927467377701, -0.1787899950787401604, 0.3297244093950555954 ) ) ;
#37918 = EDGE_CURVE ( 'NONE', #41944, #13298, #19670, .T. ) ;
#37919 = PLANE ( 'NONE',  #2265 ) ;
#37920 = ORIENTED_EDGE ( 'NONE', *, *, #20125, .T. ) ;
#37921 = CARTESIAN_POINT ( 'NONE',  ( -0.7185039370078746268, -0.06523048226347956391, 0.3075787401574804347 ) ) ;
#37922 = CARTESIAN_POINT ( 'NONE',  ( 1.054774247047244540, 0.07405724077823318263, 1.210629921206079818 ) ) ;
#37923 = CARTESIAN_POINT ( 'NONE',  ( -0.8759842519685039353, 0.1787899950787401882, 1.961122047190330786 ) ) ;
#37924 = CARTESIAN_POINT ( 'NONE',  ( -0.2559055118110236116, -4.908314874579054539E-16, -0.02740704184215039460 ) ) ;
#37925 = ORIENTED_EDGE ( 'NONE', *, *, #19900, .F. ) ;
#37926 = FACE_OUTER_BOUND ( 'NONE', #24083, .T. ) ;
#37927 = CARTESIAN_POINT ( 'NONE',  ( -1.002407869896990045, -0.1264236179284866091, 0.9276574802611967652 ) ) ;
#37928 = CARTESIAN_POINT ( 'NONE',  ( 0.1595442748538421218, -0.1490840454108204871, -0.02272210951951406099 ) ) ;
#37929 = CARTESIAN_POINT ( 'NONE',  ( 0.1574803149606300023, 0.09445121742700231249, -0.1242805304366906283 ) ) ;
#37930 = CARTESIAN_POINT ( 'NONE',  ( -0.1787899950787401882, -1.512427117835537516, 0.000000000000000000 ) ) ;
#37931 = EDGE_LOOP ( 'NONE', ( #17894, #5457 ) ) ;
#37932 = CARTESIAN_POINT ( 'NONE',  ( -1.033464566929134687, 0.06523048226347956391, 1.380413385719244435 ) ) ;
#37933 = CARTESIAN_POINT ( 'NONE',  ( 0.1787899950787401882, -0.4138779527021417826, -2.189545951927503898E-17 ) ) ;
#37934 = CARTESIAN_POINT ( 'NONE',  ( -1.033464566929133799, 0.000000000000000000, 0.08858267716535432601 ) ) ;
#37935 = VERTEX_POINT ( 'NONE', #26839 ) ;
#37936 = CARTESIAN_POINT ( 'NONE',  ( 1.054774247047244540, -0.07405724077823318263, 1.318897637741511364 ) ) ;
#37937 = CIRCLE ( 'NONE', #47126, 0.1574803149606299191 ) ;
#37938 = CARTESIAN_POINT ( 'NONE',  ( 0.8107537697050254399, 0.1574803149606300301, 0.8882874015748026819 ) ) ;
#37939 = FACE_OUTER_BOUND ( 'NONE', #23669, .T. ) ;
#37940 = EDGE_CURVE ( 'NONE', #30928, #12054, #3145, .T. ) ;
#37941 = CARTESIAN_POINT ( 'NONE',  ( 1.002407869896990045, 0.1264236179284866091, 1.641240157426551161 ) ) ;
#37942 = VECTOR ( 'NONE', #6910, 39.37007874015748143 ) ;
#37943 = AXIS2_PLACEMENT_3D ( 'NONE', #20996, #2782, #46876 ) ;
#37944 = CARTESIAN_POINT ( 'NONE',  ( -0.1264236179284866091, -1.811515747977732405, 0.1264236179284866091 ) ) ;
#37945 = CARTESIAN_POINT ( 'NONE',  ( -0.1787899950787401604, -1.769685039316315267, 0.07405724077823318263 ) ) ;
#37946 = CARTESIAN_POINT ( 'NONE',  ( 0.1595297091834116943, -0.09842519685039372024, 0.06859577724087914663 ) ) ;
#37947 = EDGE_CURVE ( 'NONE', #41019, #24192, #11909, .T. ) ;
#37948 = CARTESIAN_POINT ( 'NONE',  ( -0.7495606340400177148, -0.1264236179284866091, 0.6815944881352126172 ) ) ;
#37950 = CARTESIAN_POINT ( 'NONE',  ( -1.033464566929133799, 1.928577636452524610E-17, 2.869337061179095023E-17 ) ) ;
#37949 = CARTESIAN_POINT ( 'NONE',  ( 0.1113553986120547346, -0.7903543307086614567, -0.1113553986120547346 ) ) ;
#37951 = CARTESIAN_POINT ( 'NONE',  ( -0.1270800023317771588, -1.610280030055486034, 0.1270800023317771588 ) ) ;
#37952 = CARTESIAN_POINT ( 'NONE',  ( -0.8759842519685039353, 0.000000000000000000, 0.000000000000000000 ) ) ;
#37953 = CARTESIAN_POINT ( 'NONE',  ( -0.8759842519685039353, 0.000000000000000000, 0.000000000000000000 ) ) ;
#37954 = CARTESIAN_POINT ( 'NONE',  ( 1.002407869896990045, 0.1264236179284866091, 1.567421259788755794 ) ) ;
#37955 = CARTESIAN_POINT ( 'NONE',  ( 1.002407869896990045, 0.1264236179284866091, 1.798720472387181024 ) ) ;
#37957 = ORIENTED_EDGE ( 'NONE', *, *, #25911, .T. ) ;
#37956 = PLANE ( 'NONE',  #26855 ) ;
#37959 = CARTESIAN_POINT ( 'NONE',  ( -0.7413037127160185813, 0.09138582755367204158, 1.981387379239460289 ) ) ;
#37958 = DIRECTION ( 'NONE',  ( -1.000000000000000000, 0.000000000000000000, 0.000000000000000000 ) ) ;
#37960 = CARTESIAN_POINT ( 'NONE',  ( 0.2559055118110236116, -0.1477471161312049197, -0.2921040715117803055 ) ) ;
#37961 = CARTESIAN_POINT ( 'NONE',  ( 0.1264236179284866091, 0.05856299217974780119, -0.1264236179284866091 ) ) ;
#37962 = CARTESIAN_POINT ( 'NONE',  ( 1.054774247047244540, 0.07405724077823318263, 0.3789370078202520253 ) ) ;
#37963 = CARTESIAN_POINT ( 'NONE',  ( 0.000000000000000000, -0.5708661417322837828, 2.134496832518260172E-17 ) ) ;
#37964 = CARTESIAN_POINT ( 'NONE',  ( 0.6195511811023595161, 0.1864803149606293620, -1.186023622047243986 ) ) ;
#37965 = CARTESIAN_POINT ( 'NONE',  ( -0.8019270111902717657, 0.1787899950787401604, 1.294291338528912982 ) ) ;
#37966 = CARTESIAN_POINT ( 'NONE',  ( 0.7185039370078746268, -0.06523048226347956391, 0.7701771652468031304 ) ) ;
#37967 = EDGE_LOOP ( 'NONE', ( #43479, #7490, #46158 ) ) ;
#37968 = LINE ( 'NONE', #33452, #32227 ) ;
#37969 = EDGE_LOOP ( 'NONE', ( #16528, #10217, #6244, #22305, #30593 ) ) ;
#37970 = CARTESIAN_POINT ( 'NONE',  ( -1.033464566929133799, 0.000000000000000000, 0.6299212597349921339 ) ) ;
#37971 = CARTESIAN_POINT ( 'NONE',  ( -1.033464566929134687, 0.06523048226347956391, 0.7997047244094481755 ) ) ;
#37972 = CARTESIAN_POINT ( 'NONE',  ( 0.7495606340400177148, 0.1264236179284866091, 1.690452755851748146 ) ) ;
#37973 = CIRCLE ( 'NONE', #26522, 0.1968503937007874405 ) ;
#37974 = DIRECTION ( 'NONE',  ( 0.000000000000000000, 0.000000000000000000, -1.000000000000000000 ) ) ;
#37976 = CARTESIAN_POINT ( 'NONE',  ( 0.5717220857807087109, 4.466152701071653354E-17, 0.000000000000000000 ) ) ;
#37975 = CARTESIAN_POINT ( 'NONE',  ( 0.1658511544268519433, 0.1997399692764126045, -0.3128573757128086941 ) ) ;
#37977 = CARTESIAN_POINT ( 'NONE',  ( -0.8759842519685039353, -0.1574803149606299191, 0.5019685038294811052 ) ) ;
#37978 = CARTESIAN_POINT ( 'NONE',  ( 0.9412147342319837628, -0.1574803149606297803, 1.488681102254677535 ) ) ;
#37979 = VERTEX_POINT ( 'NONE', #19864 ) ;
#37980 = ORIENTED_EDGE ( 'NONE', *, *, #29447, .F. ) ;
#37981 = CARTESIAN_POINT ( 'NONE',  ( -0.05836929678884612144, -0.07899262986803357034, -0.2517335218907394978 ) ) ;
#37982 = ORIENTED_EDGE ( 'NONE', *, *, #39324, .F. ) ;
#37983 = VERTEX_POINT ( 'NONE', #44767 ) ;
#37984 = CARTESIAN_POINT ( 'NONE',  ( -0.1113553986120547346, 0.01673228357209397693, -0.1113553986120547346 ) ) ;
#37985 = CARTESIAN_POINT ( 'NONE',  ( -0.9500414927467378812, 0.1787899950787401604, 1.254921259788757348 ) ) ;
#37986 = EDGE_CURVE ( 'NONE', #5435, #34485, #15104, .T. ) ;
#37987 = CARTESIAN_POINT ( 'NONE',  ( -0.8070866141732283561, -0.0009842519685049383633, -0.7574803149606299524 ) ) ;
#37988 = CARTESIAN_POINT ( 'NONE',  ( 0.07405724077823318263, -0.9489428658670333583, 0.1787899950787401604 ) ) ;
#37989 = EDGE_LOOP ( 'NONE', ( #37756, #34933, #30905, #44553 ) ) ;
#37990 = CARTESIAN_POINT ( 'NONE',  ( 0.1787899950787401882, 0.09793307091990532953, -2.189545951927503898E-17 ) ) ;
#37991 = EDGE_LOOP ( 'NONE', ( #2660, #15614, #40308, #2721, #30457, #27926 ) ) ;
#37992 = ADVANCED_FACE ( 'NONE', ( #679 ), #11983, .F. ) ;
#37993 = ORIENTED_EDGE ( 'NONE', *, *, #36808, .T. ) ;
#37994 = APPLICATION_CONTEXT ( 'automotive_design' ) ;
#37995 = CARTESIAN_POINT ( 'NONE',  ( -0.7185039370078739607, 1.928577636452523993E-17, 1.200787401467275695 ) ) ;
#37996 = CARTESIAN_POINT ( 'NONE',  ( 0.7185039370078739607, 0.000000000000000000, 4.498031496062992574 ) ) ;
#37997 = CARTESIAN_POINT ( 'NONE',  ( 0.1787899950787401604, -0.6181102361667089040, 0.07405724077823318263 ) ) ;
#37998 = EDGE_CURVE ( 'NONE', #33230, #3623, #7888, .T. ) ;
#37999 = CARTESIAN_POINT ( 'NONE',  ( -0.8759842519685039353, 0.1787899950787401882, 0.2731299212060791515 ) ) ;
#38000 = CARTESIAN_POINT ( 'NONE',  ( -0.9412147342319837628, 0.1574803149606300301, 1.040846456692913424 ) ) ;
#38001 = CARTESIAN_POINT ( 'NONE',  ( -0.1270800023317771588, -1.137839085173596443, 0.1270800023317771588 ) ) ;
#38002 = CARTESIAN_POINT ( 'NONE',  ( 0.7185039370078739607, 1.928577636452523993E-17, 0.4232283464566928832 ) ) ;
#38003 = CARTESIAN_POINT ( 'NONE',  ( 0.9500414927467378812, -0.1787899950787401604, 0.9645669290800953366 ) ) ;
#38004 = CARTESIAN_POINT ( 'NONE',  ( 0.6971942568897648851, 0.07405724077823318263, 1.417322834591906444 ) ) ;
#38005 = CARTESIAN_POINT ( 'NONE',  ( -1.033464566929133799, 0.000000000000000000, 0.6299212597349921339 ) ) ;
#38006 = CARTESIAN_POINT ( 'NONE',  ( 0.7185039370078746268, -0.06523048226347956391, 1.606791338582677309 ) ) ;
#38008 = CARTESIAN_POINT ( 'NONE',  ( -1.284448818897637956, 0.000000000000000000, -1.181102362204724310 ) ) ;
#38007 = CARTESIAN_POINT ( 'NONE',  ( 0.7230964962832268084, 0.05970772165639868373, 1.982102096445605310 ) ) ;
#38009 = LINE ( 'NONE', #20025, #23618 ) ;
#38010 = CARTESIAN_POINT ( 'NONE',  ( 0.1787899950787401882, 0.09793307091990532953, -2.189545951927503898E-17 ) ) ;
#38011 = ( BOUNDED_CURVE ( )  B_SPLINE_CURVE ( 2, ( #15419, #11823, #30989, #26446, #45553, #8439, #41234, #12773, #27409 ),
 .UNSPECIFIED., .F., .T. ) 
 B_SPLINE_CURVE_WITH_KNOTS ( ( 3, 2, 2, 2, 3 ),
 ( 0.6500000000000000222, 0.6524999999999999689, 0.6550000000000000266, 0.6574999999999999734, 0.6600000000000000311 ),
 .UNSPECIFIED. ) 
 CURVE ( )  GEOMETRIC_REPRESENTATION_ITEM ( )  RATIONAL_B_SPLINE_CURVE ( ( 1.000000000000000000, 0.9238795325112869605, 1.000000000000000000, 0.9238795325112869605, 1.000000000000000000, 0.9238795325112869605, 1.000000000000000000, 0.9238795325112869605, 1.000000000000000000 ) ) 
 REPRESENTATION_ITEM ( '' )  ) ;
#38012 = CARTESIAN_POINT ( 'NONE',  ( 0.8107537697050254399, -0.1574803149606297803, 0.7849409448818904789 ) ) ;
#38013 = CARTESIAN_POINT ( 'NONE',  ( 0.8019270111902716547, 0.1787899950787401604, 1.058070866087969186 ) ) ;
#38014 = CARTESIAN_POINT ( 'NONE',  ( 0.9500414927467377701, 0.1787899950787401604, 1.884842519631275026 ) ) ;
#38015 = CARTESIAN_POINT ( 'NONE',  ( 0.9873396505805591694, 0.1113553986120547346, 0.3592519683964098820 ) ) ;
#38016 = ORIENTED_EDGE ( 'NONE', *, *, #4855, .T. ) ;
#38017 = DIRECTION ( 'NONE',  ( -1.000000000000000000, 0.000000000000000000, 0.000000000000000000 ) ) ;
#38018 = CARTESIAN_POINT ( 'NONE',  ( 0.7185039370078739607, 1.928577636452523993E-17, 1.879921259842519676 ) ) ;
#38019 = CARTESIAN_POINT ( 'NONE',  ( 0.06523048226347956391, -1.762303149498772425, -0.1574803149606300301 ) ) ;
#38020 = CARTESIAN_POINT ( 'NONE',  ( -0.7646288533564489232, -0.1113553986120547346, 0.2214566928058590567 ) ) ;
#38021 = EDGE_LOOP ( 'NONE', ( #28677, #46566, #2662, #45076 ) ) ;
#38022 = CARTESIAN_POINT ( 'NONE',  ( 1.054774247047244540, 0.07405724077823318263, 1.166338582623402509 ) ) ;
#38023 = LINE ( 'NONE', #27751, #422 ) ;
#38024 = CARTESIAN_POINT ( 'NONE',  ( 0.07405724077823318263, 0.1053149606836847191, -0.1787899950787401604 ) ) ;
#38025 = AXIS2_PLACEMENT_3D ( 'NONE', #25653, #36662, #452 ) ;
#38026 = FACE_OUTER_BOUND ( 'NONE', #37350, .T. ) ;
#38027 = CARTESIAN_POINT ( 'NONE',  ( -0.8019270111902717657, 0.1787899950787401604, 0.5856299212060785964 ) ) ;
#38028 = CARTESIAN_POINT ( 'NONE',  ( -0.9873396505805591694, -0.1113553986120547346, 0.2805118110236220486 ) ) ;
#38029 = DIRECTION ( 'NONE',  ( -1.000000000000000000, 0.000000000000000000, 0.000000000000000000 ) ) ;
#38030 = ORIENTED_EDGE ( 'NONE', *, *, #380, .T. ) ;
#38031 = CARTESIAN_POINT ( 'NONE',  ( -0.1264236179284866091, -1.506397637741511586, -0.1264236179284866091 ) ) ;
#38032 = CARTESIAN_POINT ( 'NONE',  ( -0.7495606340400177148, -0.1264236179284866091, 1.818405511757259729 ) ) ;
#38033 = EDGE_CURVE ( 'NONE', #28644, #18361, #41689, .T. ) ;
#38034 = CARTESIAN_POINT ( 'NONE',  ( -0.9500414927467377701, 0.1787899950787401604, 1.013779527505291878 ) ) ;
#38035 = CARTESIAN_POINT ( 'NONE',  ( -1.054774247047244540, 0.07405724077823318263, 0.5807086613635594752 ) ) ;
#38036 = ( BOUNDED_CURVE ( )  B_SPLINE_CURVE ( 2, ( #4261, #15095, #8113, #29741, #26827 ),
 .UNSPECIFIED., .F., .T. ) 
 B_SPLINE_CURVE_WITH_KNOTS ( ( 3, 2, 3 ),
 ( 0.01499999999999999944, 0.01750000000000000167, 0.02000000000000000042 ),
 .UNSPECIFIED. ) 
 CURVE ( )  GEOMETRIC_REPRESENTATION_ITEM ( )  RATIONAL_B_SPLINE_CURVE ( ( 1.000000000000000000, 0.9238795325112869605, 1.000000000000000000, 0.9238795325112869605, 1.000000000000000000 ) ) 
 REPRESENTATION_ITEM ( '' )  ) ;
#38037 = EDGE_CURVE ( 'NONE', #6061, #31524, #27704, .T. ) ;
#38038 = CARTESIAN_POINT ( 'NONE',  ( -0.2016454051084722587, 0.1790725142611516163, -0.3070225280280141633 ) ) ;
#38039 = CARTESIAN_POINT ( 'NONE',  ( 0.1673228346456693549, 0.09275486626281861935, -0.1104648588920805335 ) ) ;
#38040 = CARTESIAN_POINT ( 'NONE',  ( 0.1264236179284866091, -0.5429389288591598417, -0.1264236179284866091 ) ) ;
#38041 = CARTESIAN_POINT ( 'NONE',  ( 0.1884186337727752070, -0.08956031548849312240, 0.08950290581337028151 ) ) ;
#38042 = DIRECTION ( 'NONE',  ( 0.5735764363510331698, -0.6455006197386610189, 0.5043203561029969695 ) ) ;
#38043 = EDGE_CURVE ( 'NONE', #42894, #28693, #41158, .T. ) ;
#38044 = CARTESIAN_POINT ( 'NONE',  ( -1.033464566929133799, 0.000000000000000000, 0.5216535433070865757 ) ) ;
#38045 = CARTESIAN_POINT ( 'NONE',  ( -1.054774247047244096, 0.000000000000000000, 0.4552165353793071745 ) ) ;
#38046 = CARTESIAN_POINT ( 'NONE',  ( -1.033464566929133799, 1.928577636452524610E-17, 2.869337061179095023E-17 ) ) ;
#38047 = ORIENTED_EDGE ( 'NONE', *, *, #6011, .T. ) ;
#38048 = CARTESIAN_POINT ( 'NONE',  ( 0.2471922904502823481, -0.05170400041210165137, 0.1201839652823721433 ) ) ;
#38049 = CARTESIAN_POINT ( 'NONE',  ( -1.002407869896990045, 0.1264236179284866091, 1.528051181048598384 ) ) ;
#38050 = CARTESIAN_POINT ( 'NONE',  ( 0.1787899950787401882, -1.521161417269070837, -2.189545951927503898E-17 ) ) ;
#38052 = EDGE_CURVE ( 'NONE', #7550, #20344, #27087, .T. ) ;
#38051 = DIRECTION ( 'NONE',  ( 1.541976423090495042E-15, 0.4344452574044150306, -0.9006982393225888561 ) ) ;
#38053 = CIRCLE ( 'NONE', #43376, 0.1377952755905511861 ) ;
#38054 = CARTESIAN_POINT ( 'NONE',  ( -0.1476377952755905387, 0.2573565155132549465, -0.3015174453633734930 ) ) ;
#38055 = DIRECTION ( 'NONE',  ( 0.000000000000000000, 0.7071067811867007835, 0.7071067811863941399 ) ) ;
#38056 = CARTESIAN_POINT ( 'NONE',  ( 1.033464566929133799, 0.000000000000000000, 0.4429133858267716439 ) ) ;
#38057 = DIRECTION ( 'NONE',  ( 1.000000000000000000, 0.000000000000000000, 0.000000000000000000 ) ) ;
#38058 = CARTESIAN_POINT ( 'NONE',  ( -1.033464566929134687, 0.06523048226347956391, 1.262303149498772425 ) ) ;
#38059 = CARTESIAN_POINT ( 'NONE',  ( 1.054774247047244540, -0.07405724077823318263, 0.5757874015210394658 ) ) ;
#38061 = CARTESIAN_POINT ( 'NONE',  ( -0.2066929133858267931, 0.6201712226723911092, -1.113828806122273418 ) ) ;
#38060 = CARTESIAN_POINT ( 'NONE',  ( 0.1113553986120547346, -0.4064960629921260393, 0.1113553986120547346 ) ) ;
#38062 = CARTESIAN_POINT ( 'NONE',  ( 0.000000000000000000, 0.000000000000000000, 0.000000000000000000 ) ) ;
#38063 = ORIENTED_EDGE ( 'NONE', *, *, #41849, .F. ) ;
#38064 = CARTESIAN_POINT ( 'NONE',  ( 0.1113553986120547346, 0.03641732283464567399, -0.1113553986120547346 ) ) ;
#38065 = CARTESIAN_POINT ( 'NONE',  ( -1.054774247047244540, 0.07405724077823318263, 1.092519684985606032 ) ) ;
#38066 = CARTESIAN_POINT ( 'NONE',  ( 1.033464566929134687, -0.06523048226347956391, 1.031003937007875182 ) ) ;
#38067 = DIRECTION ( 'NONE',  ( -1.000000000000000000, 0.000000000000000000, 0.000000000000000000 ) ) ;
#38068 = LINE ( 'NONE', #34029, #601 ) ;
#38069 = CARTESIAN_POINT ( 'NONE',  ( 2.892866454678787531E-17, -0.5590551180027086842, 0.1574803149606299191 ) ) ;
#38071 = DIRECTION ( 'NONE',  ( -1.000000000000000000, 0.000000000000000000, 0.000000000000000000 ) ) ;
#38070 = CYLINDRICAL_SURFACE ( 'NONE', #16166, 0.1574803149606299191 ) ;
#38072 = CARTESIAN_POINT ( 'NONE',  ( 0.9412147342319837628, 0.1574803149606300301, 1.267224409341291436 ) ) ;
#38073 = CARTESIAN_POINT ( 'NONE',  ( -0.1690116988092786321, -0.08956104861086600089, -0.02641944785140138904 ) ) ;
#38074 = CARTESIAN_POINT ( 'NONE',  ( -0.1787899950787401882, -0.5910433070328504623, 0.000000000000000000 ) ) ;
#38075 = VERTEX_POINT ( 'NONE', #37123 ) ;
#38076 = DIRECTION ( 'NONE',  ( 0.000000000000000000, 0.000000000000000000, -1.000000000000000000 ) ) ;
#38077 = CARTESIAN_POINT ( 'NONE',  ( -0.3100393700787402174, 0.01127274112884909044, 0.7086614173228353852 ) ) ;
#38078 = CARTESIAN_POINT ( 'NONE',  ( 0.9500414927467378812, -0.1787899950787401604, 0.7234251967966300878 ) ) ;
#38079 = ORIENTED_EDGE ( 'NONE', *, *, #17149, .T. ) ;
#38080 = CARTESIAN_POINT ( 'NONE',  ( -0.09072581850463902475, 0.09340956239926205551, -0.2330524951300393943 ) ) ;
#38081 = FACE_OUTER_BOUND ( 'NONE', #27387, .T. ) ;
#38082 = CARTESIAN_POINT ( 'NONE',  ( -0.1787899950787401882, -1.732775590497417362, 0.000000000000000000 ) ) ;
#38083 = CARTESIAN_POINT ( 'NONE',  ( 0.1264236179284866091, -0.9650590550643465271, -0.1264236179284866091 ) ) ;
#38084 = CARTESIAN_POINT ( 'NONE',  ( 0.1574803149606300301, -1.348917322834644938, 0.06523048226347956391 ) ) ;
#38085 = CARTESIAN_POINT ( 'NONE',  ( 0.8107537697050253289, 0.1574803149606300301, 1.193405511703496957 ) ) ;
#38086 = CARTESIAN_POINT ( 'NONE',  ( 0.7185039370078739607, 1.928577636452523993E-17, 0.7283464565853858819 ) ) ;
#38087 = ORIENTED_EDGE ( 'NONE', *, *, #37325, .T. ) ;
#38088 = ORIENTED_EDGE ( 'NONE', *, *, #43772, .F. ) ;
#38089 = CARTESIAN_POINT ( 'NONE',  ( -0.8019270111902717657, -0.1787899950787401604, 1.747047244040724312 ) ) ;
#38090 = CARTESIAN_POINT ( 'NONE',  ( 0.7495606340400177148, -0.1264236179284866091, 1.902066929080094448 ) ) ;
#38091 = VERTEX_POINT ( 'NONE', #15582 ) ;
#38092 = CARTESIAN_POINT ( 'NONE',  ( 0.6971942568897626646, 0.07405724077823318263, 0.4379921259304882519 ) ) ;
#38093 = CARTESIAN_POINT ( 'NONE',  ( -0.6971942568897648851, 0.07405724077823318263, 1.456692913332062744 ) ) ;
#38094 = LINE ( 'NONE', #27581, #32047 ) ;
#38095 = EDGE_CURVE ( 'NONE', #3096, #36213, #24789, .T. ) ;
#38096 = CIRCLE ( 'NONE', #31198, 0.09842519685039370636 ) ;
#38097 = CARTESIAN_POINT ( 'NONE',  ( -0.8759842519685039353, 0.1787899950787401882, 0.03690944876513417572 ) ) ;
#38098 = EDGE_CURVE ( 'NONE', #47016, #15855, #24907, .T. ) ;
#38099 = LINE ( 'NONE', #5261, #13794 ) ;
#38100 = CARTESIAN_POINT ( 'NONE',  ( -1.054774247047244096, 0.000000000000000000, 1.680610236166708793 ) ) ;
#38101 = CARTESIAN_POINT ( 'NONE',  ( -1.002407869896990045, 0.1264236179284866091, 0.03198818892261445085 ) ) ;
#38102 = CARTESIAN_POINT ( 'NONE',  ( -0.8759842519685039353, -0.1574803149606299191, 1.732283464566929165 ) ) ;
#38103 = DIRECTION ( 'NONE',  ( -1.000000000000000000, 0.000000000000000000, 0.000000000000000000 ) ) ;
#38104 = CARTESIAN_POINT ( 'NONE',  ( 0.8019270111902716547, -0.1787899950787401604, 1.668307086560410157 ) ) ;
#38105 = CARTESIAN_POINT ( 'NONE',  ( 0.2014288353937744303, -0.09842519685039370636, 0.06137064346568976703 ) ) ;
#38106 = CARTESIAN_POINT ( 'NONE',  ( -0.7185039370078739607, 1.928577636452523993E-17, 1.722440944881889813 ) ) ;
#38107 = EDGE_CURVE ( 'NONE', #11278, #6310, #31055, .T. ) ;
#38108 = CARTESIAN_POINT ( 'NONE',  ( 0.8107537697050254399, 0.1574803149606300301, 0.2878937006798746312 ) ) ;
#38109 = EDGE_CURVE ( 'NONE', #12102, #2430, #23033, .T. ) ;
#38110 = DIMENSIONAL_EXPONENTS ( 1.000000000000000000, 0.000000000000000000, 0.000000000000000000, 0.000000000000000000, 0.000000000000000000, 0.000000000000000000, 0.000000000000000000 ) ;
#38111 = ORIENTED_EDGE ( 'NONE', *, *, #22370, .T. ) ;
#38112 = VERTEX_POINT ( 'NONE', #2119 ) ;
#38113 = EDGE_LOOP ( 'NONE', ( #31089, #32885 ) ) ;
#38114 = CARTESIAN_POINT ( 'NONE',  ( -0.07405724077823318263, -0.9970472440407247561, -0.1787899950787401604 ) ) ;
#38115 = CARTESIAN_POINT ( 'NONE',  ( 3.284318927891251994E-17, -1.132381889710015743, 0.1787899950787401882 ) ) ;
#38116 = CIRCLE ( 'NONE', #29744, 0.1968503937007874127 ) ;
#38117 = DIRECTION ( 'NONE',  ( 0.000000000000000000, 0.2432573283306646017, -0.9699617890481189164 ) ) ;
#38118 = ( NAMED_UNIT ( * ) PLANE_ANGLE_UNIT ( ) SI_UNIT ( $, .RADIAN. ) ) ;
#38119 = CARTESIAN_POINT ( 'NONE',  ( 0.7495606340400177148, -0.1264236179284866091, 1.857775590497417362 ) ) ;
#38120 = CARTESIAN_POINT ( 'NONE',  ( 0.1270800023317771588, -0.4193351481657228152, 0.1270800023317771588 ) ) ;
#38121 = CARTESIAN_POINT ( 'NONE',  ( -0.9412147342319837628, -0.1574803149606297803, 0.8193897636719996713 ) ) ;
#38122 = CARTESIAN_POINT ( 'NONE',  ( 0.1113553986120547346, -0.05216535433070866590, 0.1113553986120547346 ) ) ;
#38123 = CARTESIAN_POINT ( 'NONE',  ( 0.8019270111902717657, 0.1787899950787401604, 0.9005905511273389896 ) ) ;
#38124 = VECTOR ( 'NONE', #47281, 39.37007874015748143 ) ;
#38126 = CARTESIAN_POINT ( 'NONE',  ( 0.003457534521343444064, 0.09882139917205609581, 0.1044452803223061832 ) ) ;
#38125 = CARTESIAN_POINT ( 'NONE',  ( -1.054774247047244540, -0.07405724077823318263, 1.993110236166711013 ) ) ;
#38127 = CYLINDRICAL_SURFACE ( 'NONE', #21584, 0.1574803149606299191 ) ;
#38128 = CARTESIAN_POINT ( 'NONE',  ( 0.8019270111902717657, -0.1787899950787401604, 1.983267716481667886 ) ) ;
#38129 = CARTESIAN_POINT ( 'NONE',  ( 0.1645805237892203066, -0.08067386790044646372, 0.1414080254031224448 ) ) ;
#38130 = CARTESIAN_POINT ( 'NONE',  ( 0.07405724077823318263, -0.4507874015210400209, -0.1787899950787401604 ) ) ;
#38131 = DIRECTION ( 'NONE',  ( 0.5735764363510332808, -0.6455006197386610189, 0.5043203561029969695 ) ) ;
#38132 = CARTESIAN_POINT ( 'NONE',  ( -0.1787899950787401882, -1.339074803095842592, 0.000000000000000000 ) ) ;
#38133 = CARTESIAN_POINT ( 'NONE',  ( -0.7495606340400177148, -0.1264236179284866091, 1.779035433017102319 ) ) ;
#38134 = ORIENTED_EDGE ( 'NONE', *, *, #43280, .T. ) ;
#38135 = CARTESIAN_POINT ( 'NONE',  ( -1.054774247047244096, 0.000000000000000000, 1.326279527505291433 ) ) ;
#38136 = DIRECTION ( 'NONE',  ( -1.000000000000000000, 0.000000000000000000, 0.000000000000000000 ) ) ;
#38137 = CARTESIAN_POINT ( 'NONE',  ( 0.8019270111902717657, 0.1787899950787401604, 1.338582677111590069 ) ) ;
#38138 = CARTESIAN_POINT ( 'NONE',  ( -0.7495606340400177148, 0.1264236179284866091, 1.257381889710015743 ) ) ;
#38139 = CARTESIAN_POINT ( 'NONE',  ( 0.06628613000900354657, -0.09842519684894961152, -0.1660483457538282914 ) ) ;
#38140 = CARTESIAN_POINT ( 'NONE',  ( 1.033464566929133799, 0.000000000000000000, 1.190944881889763884 ) ) ;
#38141 = CARTESIAN_POINT ( 'NONE',  ( 1.054774247047244540, -0.07405724077823318263, 0.6151574802611973203 ) ) ;
#38142 = CARTESIAN_POINT ( 'NONE',  ( -0.9500414927467377701, 0.1787899950787401604, 0.4625984251430869665 ) ) ;
#38143 = ADVANCED_FACE ( 'NONE', ( #20098 ), #31389, .T. ) ;
#38144 = CARTESIAN_POINT ( 'NONE',  ( -0.7185039370078739607, 1.928577636452523993E-17, 1.604330708661417360 ) ) ;
#38145 = ORIENTED_EDGE ( 'NONE', *, *, #23938, .T. ) ;
#38146 = ORIENTED_EDGE ( 'NONE', *, *, #15233, .F. ) ;
#38147 = CARTESIAN_POINT ( 'NONE',  ( -0.8107537697050234415, -0.1574803149606297803, 0.2731299212598424231 ) ) ;
#38148 = CARTESIAN_POINT ( 'NONE',  ( -0.8759842519685039353, -0.1787899950787401882, 1.941437007820252081 ) ) ;
#38149 = CARTESIAN_POINT ( 'NONE',  ( -0.8759842519685039353, 0.1574803149606299191, 0.4822834644594015674 ) ) ;
#38150 = ORIENTED_EDGE ( 'NONE', *, *, #3053, .T. ) ;
#38151 = ADVANCED_FACE ( 'NONE', ( #24408 ), #41877, .T. ) ;
#38152 = CARTESIAN_POINT ( 'NONE',  ( -0.7495606340400177148, 0.1264236179284866091, 0.9079724408911180600 ) ) ;
#38153 = VECTOR ( 'NONE', #5743, 39.37007874015748143 ) ;
#38154 = CARTESIAN_POINT ( 'NONE',  ( -1.033464566929134687, -0.06523048226347956391, 0.2042322834645668717 ) ) ;
#38155 = ORIENTED_EDGE ( 'NONE', *, *, #7219, .F. ) ;
#38156 = CARTESIAN_POINT ( 'NONE',  ( 0.9412147342319837628, 0.1574803149606300301, 1.001476377952755348 ) ) ;
#38157 = CARTESIAN_POINT ( 'NONE',  ( -0.07405724077823318263, -0.3622047243556850704, -0.1787899950787401604 ) ) ;
#38158 = CARTESIAN_POINT ( 'NONE',  ( -0.7185039370078739607, 1.928577636452523993E-17, 0.06889763779527559306 ) ) ;
#38159 = ORIENTED_EDGE ( 'NONE', *, *, #12960, .F. ) ;
#38160 = CARTESIAN_POINT ( 'NONE',  ( 1.111591794296983909E-20, 0.1210185251471166540, 0.06598031696924452905 ) ) ;
#38161 = LINE ( 'NONE', #31932, #46819 ) ;
#38162 = CARTESIAN_POINT ( 'NONE',  ( -1.094772975963752103E-17, -0.2514763778989925203, -0.1787899950787401882 ) ) ;
#38163 = CARTESIAN_POINT ( 'NONE',  ( 0.9412147342319837628, 0.1574803149606300301, 1.867618110236221707 ) ) ;
#38164 = CARTESIAN_POINT ( 'NONE',  ( 0.1787899950787401604, 0.1189705199597376750, 0.07405724077823318263 ) ) ;
#38165 = APPLICATION_PROTOCOL_DEFINITION ( 'draft international standard', 'automotive_design', 1998, #43789 ) ;
#38166 = CARTESIAN_POINT ( 'NONE',  ( 0.5555748031496099415, 0.6449983665207552619, -0.06082000038405668829 ) ) ;
#38167 = CARTESIAN_POINT ( 'NONE',  ( -1.002407869896990045, 0.1264236179284866091, 0.7800196849856062542 ) ) ;
#38168 = VECTOR ( 'NONE', #789, 39.37007874015748143 ) ;
#38170 = LINE ( 'NONE', #30783, #219 ) ;
#38169 = CARTESIAN_POINT ( 'NONE',  ( -0.1113553986120547346, -0.7411417322834646937, -0.1113553986120547346 ) ) ;
#38171 = CARTESIAN_POINT ( 'NONE',  ( 0.1270800023317771588, -1.561067431630289271, 0.1270800023317771588 ) ) ;
#38172 = LINE ( 'NONE', #37231, #10310 ) ;
#38173 = CARTESIAN_POINT ( 'NONE',  ( -0.06523048226347956391, -0.4581692912310550425, -0.1574803149606300301 ) ) ;
#38174 = ( BOUNDED_CURVE ( )  B_SPLINE_CURVE ( 2, ( #30630, #42067, #45193, #12415, #26789, #23651, #38028, #41346, #2071 ),
 .UNSPECIFIED., .F., .F. ) 
 B_SPLINE_CURVE_WITH_KNOTS ( ( 3, 2, 2, 2, 3 ),
 ( 0.1300000000000000044, 0.1325000000000000067, 0.1350000000000000089, 0.1375000000000000111, 0.1400000000000000133 ),
 .UNSPECIFIED. ) 
 CURVE ( )  GEOMETRIC_REPRESENTATION_ITEM ( )  RATIONAL_B_SPLINE_CURVE ( ( 1.000000000000000000, 0.9238795325112869605, 1.000000000000000000, 0.9238795325112869605, 1.000000000000000000, 0.9238795325112869605, 1.000000000000000000, 0.9238795325112869605, 1.000000000000000000 ) ) 
 REPRESENTATION_ITEM ( '' )  ) ;
#38175 = CARTESIAN_POINT ( 'NONE',  ( -0.07405724077823318263, -0.3622047243556850704, -0.1787899950787401604 ) ) ;
#38176 = DIRECTION ( 'NONE',  ( 0.000000000000000000, 0.000000000000000000, 1.000000000000000000 ) ) ;
#38177 = CARTESIAN_POINT ( 'NONE',  ( 0.6971942568897648851, -0.07405724077823297447, 1.545275590497416696 ) ) ;
#38178 = CARTESIAN_POINT ( 'NONE',  ( 0.8019270111902716547, 0.1787899950787401604, 1.845472440891119392 ) ) ;
#38179 = CARTESIAN_POINT ( 'NONE',  ( 1.054774247047244540, -0.07405724077823318263, 0.4527559054580477249 ) ) ;
#38180 = AXIS2_PLACEMENT_3D ( 'NONE', #16736, #21015, #35430 ) ;
#38182 = ORIENTED_EDGE ( 'NONE', *, *, #37890, .T. ) ;
#38181 = CARTESIAN_POINT ( 'NONE',  ( 1.033464566929133799, 0.000000000000000000, 1.072834645669291431 ) ) ;
#38183 = LINE ( 'NONE', #41984, #21242 ) ;
#38184 = DIRECTION ( 'NONE',  ( 0.000000000000000000, 0.000000000000000000, -1.000000000000000000 ) ) ;
#38185 = CARTESIAN_POINT ( 'NONE',  ( -0.1264236179284866091, -0.01033464561552783524, -0.1264236179284866091 ) ) ;
#38186 = CARTESIAN_POINT ( 'NONE',  ( 0.7185039370078739607, 1.928577636452523993E-17, 0.4921259841444416971 ) ) ;
#38187 = VECTOR ( 'NONE', #7154, 39.37007874015748143 ) ;
#38188 = CARTESIAN_POINT ( 'NONE',  ( 0.6971942568897637749, 2.189545951927499583E-17, 0.4749015747493858242 ) ) ;
#38189 = CARTESIAN_POINT ( 'NONE',  ( 0.8759842519685039353, -0.1574803149606299191, 0.07874015748031495954 ) ) ;
#38190 = CARTESIAN_POINT ( 'NONE',  ( 0.000000000000000000, 0.000000000000000000, 0.000000000000000000 ) ) ;
#38191 = DIRECTION ( 'NONE',  ( 1.000000000000000000, 0.000000000000000000, 0.000000000000000000 ) ) ;
#38192 = CARTESIAN_POINT ( 'NONE',  ( 0.8107537697050253289, 0.1574803149606300301, 0.7603346455617647770 ) ) ;
#38193 = ORIENTED_EDGE ( 'NONE', *, *, #47187, .T. ) ;
#38195 = AXIS2_PLACEMENT_3D ( 'NONE', #8539, #9018, #23172 ) ;
#38194 = CARTESIAN_POINT ( 'NONE',  ( -1.033464566929133799, 0.000000000000000000, 0.7874015746956221085 ) ) ;
#38196 = CARTESIAN_POINT ( 'NONE',  ( 1.054774247047244540, 0.07405724077823318263, 0.9744094487651340231 ) ) ;
#38197 = ORIENTED_EDGE ( 'NONE', *, *, #30826, .T. ) ;
#38198 = CARTESIAN_POINT ( 'NONE',  ( -0.1787899950787401604, -1.307086614119465695, -0.07405724077823318263 ) ) ;
#38199 = CARTESIAN_POINT ( 'NONE',  ( -0.7646288533564489232, 0.1113553986120547346, 0.6053149605223937524 ) ) ;
#38200 = CARTESIAN_POINT ( 'NONE',  ( -0.8070866141732283561, 0.000000000000000000, 0.7574803149606299524 ) ) ;
#38201 = CARTESIAN_POINT ( 'NONE',  ( 0.6971942568897637749, 2.189545951927499583E-17, 1.734744094434425232 ) ) ;
#38202 = CARTESIAN_POINT ( 'NONE',  ( -0.7646288533564489232, -0.1113553986120547346, 1.215551181102362266 ) ) ;
#38203 = CARTESIAN_POINT ( 'NONE',  ( 0.9412147342319837628, 0.1574803149606300301, 0.5684055118110233895 ) ) ;
#38205 = CARTESIAN_POINT ( 'NONE',  ( 0.7185039370078739607, 1.928577636452523993E-17, 1.958661417322834719 ) ) ;
#38204 = DIRECTION ( 'NONE',  ( 0.000000000000000000, 0.000000000000000000, 1.000000000000000000 ) ) ;
#38206 = CARTESIAN_POINT ( 'NONE',  ( 0.6971942568897637749, 2.189545951927499583E-17, 0.2042322834108035723 ) ) ;
#38207 = ADVANCED_FACE ( 'NONE', ( #20800 ), #34744, .T. ) ;
#38208 = CARTESIAN_POINT ( 'NONE',  ( 0.7185039370078739607, 1.928577636452523993E-17, 1.476377952648377789 ) ) ;
#38209 = VERTEX_POINT ( 'NONE', #45479 ) ;
#38210 = EDGE_CURVE ( 'NONE', #5993, #23361, #6558, .T. ) ;
#38211 = DIRECTION ( 'NONE',  ( 5.724375810226159034E-16, 0.6156614753256599570, 0.7880107536067207930 ) ) ;
#38212 = CARTESIAN_POINT ( 'NONE',  ( 1.002407869896990045, -0.1264236179284866091, 0.9670275590013542866 ) ) ;
#38213 = CARTESIAN_POINT ( 'NONE',  ( -0.8019270111902716547, 0.1787899950787401604, 1.609251968450173598 ) ) ;
#38214 = CARTESIAN_POINT ( 'NONE',  ( 0.1574803149606300301, -0.07923228335703978720, 0.06523048226347956391 ) ) ;
#38215 = CARTESIAN_POINT ( 'NONE',  ( -0.6971942568897648851, 0.07405724077823318263, 1.422244094434426120 ) ) ;
#38216 = ORIENTED_EDGE ( 'NONE', *, *, #17416, .F. ) ;
#38217 = DIRECTION ( 'NONE',  ( -1.000000000000000000, 0.000000000000000000, 0.000000000000000000 ) ) ;
#38218 = VECTOR ( 'NONE', #43176, 39.37007874015748143 ) ;
#38219 = CARTESIAN_POINT ( 'NONE',  ( 1.033464566929133799, 0.000000000000000000, 1.850393700679873854 ) ) ;
#38220 = CARTESIAN_POINT ( 'NONE',  ( -0.7185039370078739607, 1.928577636452523993E-17, 0.4527559054042842868 ) ) ;
#38221 = CARTESIAN_POINT ( 'NONE',  ( 0.07405724077823318263, -1.209769637520577312, -0.1787899950787401604 ) ) ;
#38222 = VERTEX_POINT ( 'NONE', #21030 ) ;
#38223 = CARTESIAN_POINT ( 'NONE',  ( 3.284318927891251994E-17, -0.03001968498560657339, 0.1787899950787401882 ) ) ;
#38224 = ORIENTED_EDGE ( 'NONE', *, *, #34278, .T. ) ;
#38225 = ORIENTED_EDGE ( 'NONE', *, *, #9828, .F. ) ;
#38226 = CARTESIAN_POINT ( 'NONE',  ( -0.2559082475277629221, -0.04046285581729015118, -0.3131342661657301463 ) ) ;
#38227 = CONICAL_SURFACE ( 'NONE', #23691, 0.1574803149606299191, 1.047197551196598297 ) ;
#38228 = FACE_OUTER_BOUND ( 'NONE', #15368, .T. ) ;
#38229 = EDGE_CURVE ( 'NONE', #40935, #26601, #31149, .T. ) ;
#38230 = CARTESIAN_POINT ( 'NONE',  ( 0.8107537697050253289, -0.1574803149606297803, 1.887303149606301078 ) ) ;
#38231 = AXIS2_PLACEMENT_3D ( 'NONE', #12164, #27515, #23181 ) ;
#38232 = CARTESIAN_POINT ( 'NONE',  ( 0.07405724077823318263, -0.6230314960092281362, 0.1787899950787401604 ) ) ;
#38233 = CARTESIAN_POINT ( 'NONE',  ( -0.6971942568897626646, -0.07405724077823297447, 0.2066929133320631329 ) ) ;
#38234 = CARTESIAN_POINT ( 'NONE',  ( -0.8759842519685039353, -0.1574803149606299191, 1.023622047244094446 ) ) ;
#38235 = CARTESIAN_POINT ( 'NONE',  ( 3.301370929368692659E-17, -1.093547746590919356, 0.1797182628040039365 ) ) ;
#38236 = CARTESIAN_POINT ( 'NONE',  ( 0.1558288391422229802, 0.1299212598425196485, -0.06817221290114469645 ) ) ;
#38237 = CARTESIAN_POINT ( 'NONE',  ( 0.6971942568897637749, 2.189545951927499583E-17, 1.149114173174582643 ) ) ;
#38238 = CARTESIAN_POINT ( 'NONE',  ( 0.8759842519685039353, 0.1787899950787401882, 1.449311023568283341 ) ) ;
#38239 = CARTESIAN_POINT ( 'NONE',  ( 1.002407869896990045, -0.1264236179284866091, 0.1353346456155277433 ) ) ;
#38240 = CARTESIAN_POINT ( 'NONE',  ( 1.033464566929133799, 0.000000000000000000, 1.505905511811023612 ) ) ;
#38242 = CARTESIAN_POINT ( 'NONE',  ( -0.1899652659300057611, -0.1858176586718346124, -0.3092881115734000819 ) ) ;
#38241 = CARTESIAN_POINT ( 'NONE',  ( 0.7902745575623760788, 0.1357881168358097967, 1.980121974491770409 ) ) ;
#38243 = DIRECTION ( 'NONE',  ( -0.000000000000000000, 1.000000000000000000, -0.000000000000000000 ) ) ;
#38244 = CARTESIAN_POINT ( 'NONE',  ( -0.8107537697050253289, 0.1574803149606300301, 1.626476377845228694 ) ) ;
#38245 = FACE_BOUND ( 'NONE', #33469, .T. ) ;
#38246 = CARTESIAN_POINT ( 'NONE',  ( 1.002407869896990045, 0.1264236179284866091, 0.9719488188438739629 ) ) ;
#38247 = CARTESIAN_POINT ( 'NONE',  ( 1.054774247047244540, 0.07405724077823318263, 1.801181102308441861 ) ) ;
#38248 = CARTESIAN_POINT ( 'NONE',  ( 0.7185039370078739607, 1.928577636452523993E-17, 0.3740157479239689664 ) ) ;
#38249 = ORIENTED_EDGE ( 'NONE', *, *, #5256, .F. ) ;
#38250 = EDGE_CURVE ( 'NONE', #31524, #47261, #39255, .T. ) ;
#38251 = DIRECTION ( 'NONE',  ( -0.000000000000000000, 1.000000000000000000, -3.995705278811693553E-31 ) ) ;
#38252 = LINE ( 'NONE', #37539, #12212 ) ;
#38253 = CARTESIAN_POINT ( 'NONE',  ( -0.1574803149606297803, -1.629429133750740721, 0.06523048226347956391 ) ) ;
#38254 = CARTESIAN_POINT ( 'NONE',  ( -1.033464566929133799, 0.000000000000000000, 0.2755905510735752184 ) ) ;
#38255 = CARTESIAN_POINT ( 'NONE',  ( 1.054774247047244540, -0.07405724077823318263, 1.358267716481669662 ) ) ;
#38256 = CYLINDRICAL_SURFACE ( 'NONE', #25703, 0.1574803149606300579 ) ;
#38257 = ADVANCED_FACE ( 'NONE', ( #10025 ), #24645, .T. ) ;
#38258 = CARTESIAN_POINT ( 'NONE',  ( -1.094772975963752103E-17, 0.1471456693451021758, -0.1787899950787401882 ) ) ;
#38259 = CARTESIAN_POINT ( 'NONE',  ( -0.9412147342319837628, -0.1574803149606297803, 1.016240157372787722 ) ) ;
#38260 = EDGE_CURVE ( 'NONE', #18185, #35433, #36612, .T. ) ;
#38261 = CARTESIAN_POINT ( 'NONE',  ( -0.8759842519685039353, 0.1787899950787401882, 0.6225393700249762796 ) ) ;
#38262 = CARTESIAN_POINT ( 'NONE',  ( 0.3100393700787401619, 3.796887221765908018E-17, 0.4921259842519685179 ) ) ;
#38263 = DIRECTION ( 'NONE',  ( -0.6018150231520440485, 0.000000000000000000, -0.7986355100472960489 ) ) ;
#38264 = APPLICATION_CONTEXT ( 'automotive_design' ) ;
#38265 = CARTESIAN_POINT ( 'NONE',  ( -0.1787899950787401604, -1.582677165300567346, -0.07405724077823318263 ) ) ;
#38266 = CARTESIAN_POINT ( 'NONE',  ( -1.054774247047244540, 0.07405724077823318263, 1.053149606245450176 ) ) ;
#38267 = CARTESIAN_POINT ( 'NONE',  ( -0.7495606340400177148, 0.1264236179284866091, 1.847933070812378009 ) ) ;
#38268 = VERTEX_POINT ( 'NONE', #32800 ) ;
#38269 = CARTESIAN_POINT ( 'NONE',  ( -0.9500414927467378812, -0.1787899950787401604, 0.7283464566391493200 ) ) ;
#38270 = ORIENTED_EDGE ( 'NONE', *, *, #42984, .F. ) ;
#38271 = EDGE_CURVE ( 'NONE', #11128, #36578, #37937, .T. ) ;
#38272 = FACE_OUTER_BOUND ( 'NONE', #27976, .T. ) ;
#38273 = CARTESIAN_POINT ( 'NONE',  ( 0.07405724077823318263, -0.5011082201977427042, -0.1787899950787401604 ) ) ;
#38274 = CARTESIAN_POINT ( 'NONE',  ( 0.1082782017465728358, -0.08956058681966397317, -0.1600574421723590657 ) ) ;
#38275 = CARTESIAN_POINT ( 'NONE',  ( -0.3161444924769509779, 1.449372585305505723, -0.3207561694859716317 ) ) ;
#38276 = ORIENTED_EDGE ( 'NONE', *, *, #37918, .T. ) ;
#38277 = CARTESIAN_POINT ( 'NONE',  ( -0.05739891189368035579, -0.09221798112689158500, 0.1474577068024042759 ) ) ;
#38278 = CARTESIAN_POINT ( 'NONE',  ( -0.8759842519685039353, 0.1787899950787401882, 0.5044291338045039375 ) ) ;
#38279 = DIRECTION ( 'NONE',  ( 0.000000000000000000, 1.000000000000000000, 0.000000000000000000 ) ) ;
#38280 = ORIENTED_EDGE ( 'NONE', *, *, #7797, .T. ) ;
#38281 = DIRECTION ( 'NONE',  ( 1.000000000000000000, 0.000000000000000000, 0.000000000000000000 ) ) ;
#38282 = CIRCLE ( 'NONE', #17621, 0.09842519685039310962 ) ;
#38283 = CARTESIAN_POINT ( 'NONE',  ( -0.1787899950787401604, -1.538385826717890703, 0.07405724077823318263 ) ) ;
#38284 = AXIS2_PLACEMENT_3D ( 'NONE', #23724, #16075, #30938 ) ;
#38285 = CARTESIAN_POINT ( 'NONE',  ( 0.000000000000000000, 0.000000000000000000, -0.1183602362204724257 ) ) ;
#38286 = ( BOUNDED_SURFACE ( )  B_SPLINE_SURFACE ( 3, 2, ( 
 ( #20573, #28034, #9806 ),
 ( #35215, #34981, #24414 ),
 ( #27815, #20103, #16295 ),
 ( #30923, #39017, #20806 ),
 ( #23485, #35446, #45484 ),
 ( #2586, #27093, #16755 ) ),
 .UNSPECIFIED., .F., .F., .T. ) 
 B_SPLINE_SURFACE_WITH_KNOTS ( ( 4, 2, 4 ),
 ( 3, 3 ),
 ( 0.01651999345535504898, 0.01858032176739835006, 0.02064065007944164767 ),
 ( 0.000000000000000000, 1.000000000000000000 ),
 .UNSPECIFIED. ) 
 GEOMETRIC_REPRESENTATION_ITEM ( )  RATIONAL_B_SPLINE_SURFACE ( (
 ( 1.000000000000000000, 0.8047781103519390244, 1.000000000000000000),
 ( 1.000000000000000000, 0.8123785825612319655, 1.000000000000000000),
 ( 1.000000000000000000, 0.8190671539777679699, 1.000000000000000000),
 ( 1.000000000000000000, 0.8192352254845469695, 1.000000000000000000),
 ( 1.000000000000000000, 0.8126129677203649537, 1.000000000000000000),
 ( 1.000000000000000000, 0.8047712537969730073, 1.000000000000000000) ) ) 
 REPRESENTATION_ITEM ( '' )  SURFACE ( )  ) ;
#38287 = DIRECTION ( 'NONE',  ( 0.000000000000000000, -1.000000000000000000, 0.000000000000000000 ) ) ;
#38288 = CARTESIAN_POINT ( 'NONE',  ( 0.7185039370078739607, 1.928577636452523993E-17, 0.9744094488188976833 ) ) ;
#38289 = CARTESIAN_POINT ( 'NONE',  ( 0.8107537697050253289, -0.1574803149606297803, 0.5880905511811019837 ) ) ;
#38290 = FACE_OUTER_BOUND ( 'NONE', #4788, .T. ) ;
#38291 = CARTESIAN_POINT ( 'NONE',  ( -0.7646288533564489232, 0.1113553986120547346, 1.195866141624756018 ) ) ;
#38292 = CARTESIAN_POINT ( 'NONE',  ( 1.054774247047244540, 0.07405724077823318263, 0.6594488188438737408 ) ) ;
#38293 = CARTESIAN_POINT ( 'NONE',  ( 0.6971942568897626646, -0.07405724077823297447, 0.08366141726907130871 ) ) ;
#38295 = CARTESIAN_POINT ( 'NONE',  ( 1.033464566929133799, 0.000000000000000000, 1.929133858160188897 ) ) ;
#38294 = CARTESIAN_POINT ( 'NONE',  ( 0.1574803149606300301, -0.3597440944881892810, -0.06523048226347956391 ) ) ;
#38296 = LINE ( 'NONE', #31602, #39121 ) ;
#38297 = ORIENTED_EDGE ( 'NONE', *, *, #40601, .T. ) ;
#38298 = ADVANCED_FACE ( 'NONE', ( #6653 ), #18801, .T. ) ;
#38299 = DIRECTION ( 'NONE',  ( 0.000000000000000000, 0.9699617890481186944, 0.2432573283306645462 ) ) ;
#38300 = CARTESIAN_POINT ( 'NONE',  ( 0.7185039370078746268, -0.06523048226347956391, 1.134350393700787052 ) ) ;
#38301 = FACE_OUTER_BOUND ( 'NONE', #33450, .T. ) ;
#38302 = CARTESIAN_POINT ( 'NONE',  ( -0.7185039370078741827, 0.06523048226347841205, 0.7258858266641272650 ) ) ;
#38304 = DIRECTION ( 'NONE',  ( -0.8191520442889991260, 0.000000000000000000, -0.5735764363510355013 ) ) ;
#38303 = CARTESIAN_POINT ( 'NONE',  ( -0.2559055118110236116, 0.1477471161312047254, -0.2921040715117803055 ) ) ;
#38305 = CARTESIAN_POINT ( 'NONE',  ( 0.5717220857807087109, 4.466152701071653354E-17, 0.000000000000000000 ) ) ;
#38306 = ORIENTED_EDGE ( 'NONE', *, *, #38260, .T. ) ;
#38307 = ADVANCED_FACE ( 'NONE', ( #17918 ), #25365, .F. ) ;
#38308 = CARTESIAN_POINT ( 'NONE',  ( 0.9412147342319837628, -0.1574803149606297803, 0.2780511811023620439 ) ) ;
#38309 = CARTESIAN_POINT ( 'NONE',  ( 1.054774247047244540, -0.07405724077823318263, 0.8464566928596233275 ) ) ;
#38310 = ORIENTED_EDGE ( 'NONE', *, *, #10738, .T. ) ;
#38311 = CARTESIAN_POINT ( 'NONE',  ( -0.06523048226347956391, -0.02017716535433068670, 0.1574803149606297803 ) ) ;
#38312 = CARTESIAN_POINT ( 'NONE',  ( 0.1264236179284866091, -1.747539370024976391, -0.1264236179284866091 ) ) ;
#38313 = CARTESIAN_POINT ( 'NONE',  ( -0.1787899950787401882, -0.9502952755367874982, 0.000000000000000000 ) ) ;
#38314 = CARTESIAN_POINT ( 'NONE',  ( 0.1113553986120547346, -1.312007874015748143, 0.1113553986120547346 ) ) ;
#38315 = ( BOUNDED_CURVE ( )  B_SPLINE_CURVE ( 2, ( #10771, #17459, #36162, #3067, #3316, #17697, #32345, #26329, #33521 ),
 .UNSPECIFIED., .F., .F. ) 
 B_SPLINE_CURVE_WITH_KNOTS ( ( 3, 2, 2, 2, 3 ),
 ( 0.3300000000000000155, 0.3325000000000000178, 0.3350000000000000200, 0.3375000000000000222, 0.3400000000000000244 ),
 .UNSPECIFIED. ) 
 CURVE ( )  GEOMETRIC_REPRESENTATION_ITEM ( )  RATIONAL_B_SPLINE_CURVE ( ( 1.000000000000000000, 0.9238795325112869605, 1.000000000000000000, 0.9238795325112869605, 1.000000000000000000, 0.9238795325112869605, 1.000000000000000000, 0.9238795325112869605, 1.000000000000000000 ) ) 
 REPRESENTATION_ITEM ( '' )  ) ;
#38316 = CARTESIAN_POINT ( 'NONE',  ( 0.7185039370078766252, -0.06523048226348168721, 1.163877952648377567 ) ) ;
#38317 = VECTOR ( 'NONE', #4751, 39.37007874015748143 ) ;
#38318 = VERTEX_POINT ( 'NONE', #14340 ) ;
#38319 = ORIENTED_EDGE ( 'NONE', *, *, #31296, .T. ) ;
#38320 = CARTESIAN_POINT ( 'NONE',  ( -0.6971942568897637749, 2.189545951927499583E-17, 1.857775590497417362 ) ) ;
#38321 = CARTESIAN_POINT ( 'NONE',  ( 0.6971942568897648851, -0.07405724077823297447, 1.820866141678520789 ) ) ;
#38322 = ORIENTED_EDGE ( 'NONE', *, *, #46408, .F. ) ;
#38323 = CARTESIAN_POINT ( 'NONE',  ( 0.8759842519685039353, -0.1574803149606299191, 0.5511811023622047445 ) ) ;
#38324 = CARTESIAN_POINT ( 'NONE',  ( 1.002407869896990045, -0.1264236179284866091, 0.4945866141194645849 ) ) ;
#38325 = COLOUR_RGB ( '', 0.09019608, 0.27058824, 0.51372549) ;
#38326 = CARTESIAN_POINT ( 'NONE',  ( -0.6971942568897648851, -0.07405724077823297447, 1.343503936954111744 ) ) ;
#38327 = CARTESIAN_POINT ( 'NONE',  ( -0.4620708661417322616, 1.354170115732555191, -0.4197102375732078561 ) ) ;
#38328 = VECTOR ( 'NONE', #3887, 39.37007874015748143 ) ;
#38329 = DIRECTION ( 'NONE',  ( 0.000000000000000000, 1.000000000000000000, 0.000000000000000000 ) ) ;
#38330 = CARTESIAN_POINT ( 'NONE',  ( -0.6971942568897637749, 2.189545951927499583E-17, 1.818405511757259729 ) ) ;
#38331 = CARTESIAN_POINT ( 'NONE',  ( -1.054774247047244096, 0.000000000000000000, 0.06643700782025216411 ) ) ;
#38332 = CARTESIAN_POINT ( 'NONE',  ( -0.9412147342319837628, 0.1574803149606300301, 1.710137795275592065 ) ) ;
#38333 = FACE_OUTER_BOUND ( 'NONE', #26664, .T. ) ;
#38334 = CARTESIAN_POINT ( 'NONE',  ( 1.054774247047244540, 0.07405724077823318263, 1.683070866087970074 ) ) ;
#38335 = CARTESIAN_POINT ( 'NONE',  ( 0.0007090829129236239431, -0.09842519685039370636, -0.1903984615526421176 ) ) ;
#38336 = CARTESIAN_POINT ( 'NONE',  ( 0.3849708276051176936, -0.09842519685039370636, 1.205361022782828805E-17 ) ) ;
#38337 = CARTESIAN_POINT ( 'NONE',  ( -0.7185039370078739607, 1.928577636452523993E-17, 1.801181102362204633 ) ) ;
#38338 = EDGE_LOOP ( 'NONE', ( #27023, #36412, #44943, #32544 ) ) ;
#38339 = ORIENTED_EDGE ( 'NONE', *, *, #14890, .T. ) ;
#38340 = CARTESIAN_POINT ( 'NONE',  ( -0.1787899950787401604, -1.070866141678519456, -0.07405724077823318263 ) ) ;
#38341 = CARTESIAN_POINT ( 'NONE',  ( -0.1787899950787401604, -1.184055118056472455, -0.07405724077823318263 ) ) ;
#38342 = AXIS2_PLACEMENT_3D ( 'NONE', #41151, #15812, #12208 ) ;
#38343 = LENGTH_MEASURE_WITH_UNIT ( LENGTH_MEASURE( 0.02539999999999999897 ), #34076 ) ;
#38344 = CARTESIAN_POINT ( 'NONE',  ( 0.1270800023317771588, -0.4980753056460377470, 0.1270800023317771588 ) ) ;
#38345 = CARTESIAN_POINT ( 'NONE',  ( -0.1113553986120547346, -1.784448818790110192, 0.1113553986120547346 ) ) ;
#38346 = CARTESIAN_POINT ( 'NONE',  ( -1.033464566929133799, 0.000000000000000000, 0.7480314959554645871 ) ) ;
#38347 = CARTESIAN_POINT ( 'NONE',  ( -9.642888182262618425E-18, 0.04133858267716535029, -0.1574803149606299191 ) ) ;
#38348 = CIRCLE ( 'NONE', #21518, 0.1574803149606299191 ) ;
#38349 = VECTOR ( 'NONE', #33221, 39.37007874015748143 ) ;
#38350 = EDGE_CURVE ( 'NONE', #34485, #7195, #26496, .T. ) ;
#38351 = CARTESIAN_POINT ( 'NONE',  ( 1.054774247047244540, -0.07405724077823318263, 0.9251968503399374821 ) ) ;
#38352 = VECTOR ( 'NONE', #38993, 39.37007874015748143 ) ;
#38353 = EDGE_CURVE ( 'NONE', #24091, #26106, #5808, .T. ) ;
#38355 = FACE_OUTER_BOUND ( 'NONE', #40315, .T. ) ;
#38354 = DIRECTION ( 'NONE',  ( 1.000000000000000000, 0.000000000000000000, 0.000000000000000000 ) ) ;
#38356 = CARTESIAN_POINT ( 'NONE',  ( 0.7185039370078746268, -0.06523048226347956391, 0.06151574792396910518 ) ) ;
#38357 = ADVANCED_FACE ( 'NONE', ( #32571 ), #28986, .T. ) ;
#38358 = EDGE_CURVE ( 'NONE', #18450, #1893, #18056, .T. ) ;
#38359 = CARTESIAN_POINT ( 'NONE',  ( -0.7859119931880654830, 0.1562117447626044375, 0.03937007874015843040 ) ) ;
#38360 = CARTESIAN_POINT ( 'NONE',  ( 0.1787899950787401604, -0.3818897637257640532, 0.07405724077823318263 ) ) ;
#38361 = CYLINDRICAL_SURFACE ( 'NONE', #15558, 0.1377952755905510751 ) ;
#38362 = CARTESIAN_POINT ( 'NONE',  ( -0.1787899950787401882, -1.417814960576157635, 0.000000000000000000 ) ) ;
#38363 = CARTESIAN_POINT ( 'NONE',  ( -1.002407869896990045, -0.1264236179284866091, 1.867618110182456714 ) ) ;
#38364 = ORIENTED_EDGE ( 'NONE', *, *, #586, .T. ) ;
#38365 = CARTESIAN_POINT ( 'NONE',  ( -0.8759842519685039353, -0.1787899950787401882, 1.395177165300567124 ) ) ;
#38366 = DIRECTION ( 'NONE',  ( 1.822029033848725028E-16, 0.000000000000000000, 1.000000000000000000 ) ) ;
#38367 = CARTESIAN_POINT ( 'NONE',  ( 0.7495606340400177148, -0.1264236179284866091, 1.468996062938362046 ) ) ;
#38368 = CARTESIAN_POINT ( 'NONE',  ( -0.7185039370078739607, 1.928577636452523993E-17, 0.8956692913385826404 ) ) ;
#38369 = CARTESIAN_POINT ( 'NONE',  ( -0.8759842519685039353, 0.1787899950787401882, 0.5093503936470236138 ) ) ;
#38370 = CARTESIAN_POINT ( 'NONE',  ( 1.054774247047244540, -0.07405724077823318263, 0.1033464566391498751 ) ) ;
#38371 = CARTESIAN_POINT ( 'NONE',  ( -1.002407869896990045, -0.1264236179284866091, 1.237696850339937038 ) ) ;
#38372 = DIRECTION ( 'NONE',  ( 0.000000000000000000, 0.000000000000000000, -1.000000000000000000 ) ) ;
#38373 = CARTESIAN_POINT ( 'NONE',  ( 0.4736248074375858375, -0.09842519685039370636, 1.870565676741759775 ) ) ;
#38374 = CARTESIAN_POINT ( 'NONE',  ( 0.8759842519685039353, 0.1787899950787401882, 0.6668307086076534773 ) ) ;
#38375 = CARTESIAN_POINT ( 'NONE',  ( -0.6971942568897648851, -0.07405724077823297447, 0.5954724408911187261 ) ) ;
#38376 = CARTESIAN_POINT ( 'NONE',  ( -0.06756161724086527653, -0.08412760742771717426, 0.2464250160562324043 ) ) ;
#38377 = DIRECTION ( 'NONE',  ( 1.000000000000000000, 0.000000000000000000, 0.000000000000000000 ) ) ;
#38378 = ORIENTED_EDGE ( 'NONE', *, *, #21177, .T. ) ;
#38379 = ORIENTED_EDGE ( 'NONE', *, *, #6936, .T. ) ;
#38380 = CARTESIAN_POINT ( 'NONE',  ( -0.9412147342319837628, 0.1574803149606300301, 0.3715551181102361711 ) ) ;
#38381 = CARTESIAN_POINT ( 'NONE',  ( 1.054774247047244096, 0.000000000000000000, 1.168799212544661348 ) ) ;
#38382 = CARTESIAN_POINT ( 'NONE',  ( 0.05363520799883866180, -0.09851384801570906014, 0.2150731022931543224 ) ) ;
#38383 = DIRECTION ( 'NONE',  ( 1.822029033848725028E-16, 0.000000000000000000, 1.000000000000000000 ) ) ;
#38384 = CONICAL_SURFACE ( 'NONE', #42973, 0.09842519685039370636, 0.9599310885968824758 ) ;
#38385 = ORIENTED_EDGE ( 'NONE', *, *, #34010, .T. ) ;
#38386 = AXIS2_PLACEMENT_3D ( 'NONE', #18153, #28733, #28978 ) ;
#38387 = CARTESIAN_POINT ( 'NONE',  ( -0.8759842519685039353, -0.1574803149606299191, 0.5511811023622047445 ) ) ;
#38388 = VECTOR ( 'NONE', #21745, 39.37007874015748143 ) ;
#38389 = CARTESIAN_POINT ( 'NONE',  ( -1.002407869896990045, -0.1264236179284866091, 0.9670275590013542866 ) ) ;
#38390 = CARTESIAN_POINT ( 'NONE',  ( -1.054774247047244540, -0.07405724077823318263, 0.1377952755367876370 ) ) ;
#38391 = CARTESIAN_POINT ( 'NONE',  ( 0.07405724077823318263, -1.642840503662309493, -0.1787899950787401604 ) ) ;
#38392 = ORIENTED_EDGE ( 'NONE', *, *, #6371, .T. ) ;
#38393 = DIRECTION ( 'NONE',  ( -4.825174235490821143E-17, -0.6156614753256592909, -0.7880107536067212370 ) ) ;
#38394 = CARTESIAN_POINT ( 'NONE',  ( -0.07405724077823318263, -0.5836614172690718361, 0.1787899950787401604 ) ) ;
#38395 = CARTESIAN_POINT ( 'NONE',  ( -0.3042596054108611114, -0.05980719604265498368, 1.032348353801579410 ) ) ;
#38396 = ORIENTED_EDGE ( 'NONE', *, *, #2845, .F. ) ;
#38397 = CARTESIAN_POINT ( 'NONE',  ( 1.054774247047244540, -0.07405724077823318263, 1.358267716481669662 ) ) ;
#38398 = CARTESIAN_POINT ( 'NONE',  ( 0.002794899976025624899, 0.1377744224362131009, 0.03695826049526609869 ) ) ;
#38399 = CARTESIAN_POINT ( 'NONE',  ( -1.181162989532618060E-16, -0.0009842519685041700977, -0.3937007874015748254 ) ) ;
#38400 = CARTESIAN_POINT ( 'NONE',  ( 0.07405724077823318263, -0.8149606298674965110, 0.1787899950787401604 ) ) ;
#38401 = DIRECTION ( 'NONE',  ( 0.000000000000000000, 0.000000000000000000, 1.000000000000000000 ) ) ;
#38402 = CARTESIAN_POINT ( 'NONE',  ( 0.9500414927467378812, -0.1787899950787401604, 1.589566929080094448 ) ) ;
#38403 = CARTESIAN_POINT ( 'NONE',  ( 0.1264236179284866091, -0.04097042492215212384, 0.1264236179284866091 ) ) ;
#38404 = CARTESIAN_POINT ( 'NONE',  ( -0.07405724077823318263, -1.764763779473795813, 0.1787899950787401604 ) ) ;
#38405 = APPLICATION_PROTOCOL_DEFINITION ( 'draft international standard', 'automotive_design', 1998, #6132 ) ;
#38406 = CARTESIAN_POINT ( 'NONE',  ( 0.8759842519685039353, 0.000000000000000000, 4.498031496062992574 ) ) ;
#38407 = PRESENTATION_LAYER_ASSIGNMENT (  '', '', ( #22360 ) ) ;
#38408 = CARTESIAN_POINT ( 'NONE',  ( 0.8759842519685039353, 0.1787899950787401882, 0.4650590550643464716 ) ) ;
#38409 = EDGE_CURVE ( 'NONE', #43867, #13799, #43790, .T. ) ;
#38410 = VECTOR ( 'NONE', #21377, 39.37007874015748143 ) ;
#38411 = CARTESIAN_POINT ( 'NONE',  ( -0.9500414927467377701, -0.1787899950787401604, 0.8464566928596233275 ) ) ;
#38413 = DIRECTION ( 'NONE',  ( 0.000000000000000000, 0.000000000000000000, -1.000000000000000000 ) ) ;
#38412 = CARTESIAN_POINT ( 'NONE',  ( 0.1574803149606300301, -0.9502952755905519355, -0.06523048226347956391 ) ) ;
#38415 = CARTESIAN_POINT ( 'NONE',  ( -0.8475445883371663935, -0.1713140434220985220, 1.987685975326619836 ) ) ;
#38414 = CARTESIAN_POINT ( 'NONE',  ( 0.1797182628040039087, -1.597976880449187398, 0.07444174185955046430 ) ) ;
#38416 = CARTESIAN_POINT ( 'NONE',  ( 0.07405724077823318263, -0.4212598424659216856, 0.1787899950787401604 ) ) ;
#38417 = CARTESIAN_POINT ( 'NONE',  ( -1.033464566929133799, 0.000000000000000000, 1.023622047136567126 ) ) ;
#38418 = CARTESIAN_POINT ( 'NONE',  ( 0.8019270111902717657, -0.1787899950787401604, 1.471456692859622217 ) ) ;
#38419 = CARTESIAN_POINT ( 'NONE',  ( 0.6971942568897648851, 0.07405724077823318263, 1.889763779473794481 ) ) ;
#38420 = CARTESIAN_POINT ( 'NONE',  ( 0.8759842519685039353, 0.1787899950787401882, 0.3863188975840318173 ) ) ;
#38421 = VERTEX_POINT ( 'NONE', #36394 ) ;
#38422 = VECTOR ( 'NONE', #20419, 39.37007874015748854 ) ;
#38423 = CIRCLE ( 'NONE', #17763, 0.3912448816427701037 ) ;
#38424 = VERTEX_POINT ( 'NONE', #14810 ) ;
#38425 = ADVANCED_FACE ( 'NONE', ( #28744 ), #10513, .F. ) ;
#38426 = CARTESIAN_POINT ( 'NONE',  ( 0.5555748031496099415, 0.6449983665207552619, -0.7480314960629921295 ) ) ;
#38427 = DIRECTION ( 'NONE',  ( 0.000000000000000000, 1.000000000000000000, 0.000000000000000000 ) ) ;
#38428 = CARTESIAN_POINT ( 'NONE',  ( 0.1787899950787401604, 0.01673228351833045899, -0.07405724077823318263 ) ) ;
#38429 = CARTESIAN_POINT ( 'NONE',  ( 0.7495606340400177148, -0.1264236179284866091, 0.4798228345919055560 ) ) ;
#38430 = CARTESIAN_POINT ( 'NONE',  ( 0.8019661270514706342, -0.1449744270584123751, 0.03937007223081739893 ) ) ;
#38431 = CARTESIAN_POINT ( 'NONE',  ( 0.9412147342319837628, -0.1574803149606297803, 1.961122047136568014 ) ) ;
#38432 = CARTESIAN_POINT ( 'NONE',  ( -1.033464566929134687, 0.06523048226347956391, 1.577263779420032153 ) ) ;
#38433 = CARTESIAN_POINT ( 'NONE',  ( -0.6971942568897648851, -0.07405724077823297447, 1.422244094434426120 ) ) ;
#38434 = CARTESIAN_POINT ( 'NONE',  ( 1.033464566929134687, 0.06523048226347956391, 0.8292322833570401341 ) ) ;
#38435 = ORIENTED_EDGE ( 'NONE', *, *, #9114, .F. ) ;
#38436 = CARTESIAN_POINT ( 'NONE',  ( -0.7646288533564489232, 0.1113553986120547346, 0.8021653542231811373 ) ) ;
#38437 = CARTESIAN_POINT ( 'NONE',  ( 1.002407869896990045, -0.1264236179284866091, 1.006397637741511808 ) ) ;
#38439 = CARTESIAN_POINT ( 'NONE',  ( -0.1787899950787401604, -1.380905511757260173, 0.07405724077823318263 ) ) ;
#38438 = CARTESIAN_POINT ( 'NONE',  ( 0.1574803149606299191, -1.100393700679874076, -1.928577636452523993E-17 ) ) ;
#38440 = CARTESIAN_POINT ( 'NONE',  ( -0.7646288533564489232, -0.1113553986120547346, 0.5364173227271189504 ) ) ;
#38441 = CARTESIAN_POINT ( 'NONE',  ( -0.8759842519685039353, -0.1574803149606299191, 1.417322834645669216 ) ) ;
#38442 = FACE_OUTER_BOUND ( 'NONE', #10110, .T. ) ;
#38444 = CARTESIAN_POINT ( 'NONE',  ( 1.229559056033039366E-16, -0.0009842519685041700977, 0.4921259842519680183 ) ) ;
#38443 = CARTESIAN_POINT ( 'NONE',  ( -0.7185039370078746268, 0.06523048226347956391, 0.7357283464566919395 ) ) ;
#38445 = CARTESIAN_POINT ( 'NONE',  ( 1.054774247047244096, 0.000000000000000000, 0.1845472440407248116 ) ) ;
#38446 = CARTESIAN_POINT ( 'NONE',  ( 0.9873396505805591694, 0.1113553986120547346, 1.422244094380661572 ) ) ;
#38447 = ORIENTED_EDGE ( 'NONE', *, *, #30191, .T. ) ;
#38448 = ORIENTED_EDGE ( 'NONE', *, *, #8498, .T. ) ;
#38449 = DIRECTION ( 'NONE',  ( 0.000000000000000000, 1.000000000000000000, 0.000000000000000000 ) ) ;
#38450 = ORIENTED_EDGE ( 'NONE', *, *, #11231, .F. ) ;
#38451 = CARTESIAN_POINT ( 'NONE',  ( -0.8759842519685039353, 0.1787899950787401882, 1.764271653489543290 ) ) ;
#38452 = CARTESIAN_POINT ( 'NONE',  ( 0.1113553986120547346, -0.2293307085538901779, -0.1113553986120547346 ) ) ;
#38453 = AXIS2_PLACEMENT_3D ( 'NONE', #13793, #13342, #28440 ) ;
#38454 = FACE_OUTER_BOUND ( 'NONE', #43759, .T. ) ;
#38455 = DIRECTION ( 'NONE',  ( 0.000000000000000000, 1.000000000000000000, 0.000000000000000000 ) ) ;
#38456 = DIRECTION ( 'NONE',  ( -1.739631066775710943E-15, -2.197428715927213823E-15, 1.000000000000000000 ) ) ;
#38457 = CARTESIAN_POINT ( 'NONE',  ( 0.1787899950787401604, -1.219612157205616221, 0.07405724077823318263 ) ) ;
#38458 = VERTEX_POINT ( 'NONE', #29471 ) ;
#38459 = CARTESIAN_POINT ( 'NONE',  ( 0.1787899950787401882, -0.1776574802611972648, -2.189545951927503898E-17 ) ) ;
#38460 = ORIENTED_EDGE ( 'NONE', *, *, #14669, .T. ) ;
#38461 = ORIENTED_EDGE ( 'NONE', *, *, #43540, .T. ) ;
#38462 = VECTOR ( 'NONE', #6771, 39.37007874015748854 ) ;
#38463 = CARTESIAN_POINT ( 'NONE',  ( -0.2559055118110235560, -0.01245242171185129317, -0.3149606299212599492 ) ) ;
#38464 = CARTESIAN_POINT ( 'NONE',  ( 0.3690944881889771101, 0.1864803149606328037, -0.7480314960629921295 ) ) ;
#38465 = PRODUCT ( 'Pivot Shaft', 'Pivot Shaft', '', ( #15200 ) ) ;
#38466 = CARTESIAN_POINT ( 'NONE',  ( 0.7646288533564489232, -0.1113553986120547346, 1.884842519685039353 ) ) ;
#38467 = CARTESIAN_POINT ( 'NONE',  ( -0.1787899950787401604, -0.6771653542769455747, -0.07405724077823318263 ) ) ;
#38468 = VERTEX_POINT ( 'NONE', #28499 ) ;
#38469 = EDGE_CURVE ( 'NONE', #34560, #11282, #34125, .T. ) ;
#38470 = CARTESIAN_POINT ( 'NONE',  ( -0.6971942568897648851, -0.07405724077823297447, 0.4035433070328507954 ) ) ;
#38471 = CARTESIAN_POINT ( 'NONE',  ( -0.8759842519685039353, -0.1574803149606299191, 1.062992125984252079 ) ) ;
#38472 = CARTESIAN_POINT ( 'NONE',  ( -0.07444174185955065859, -1.096008376512180194, 0.1797182628040039087 ) ) ;
#38473 = CARTESIAN_POINT ( 'NONE',  ( -0.7646288533564489232, 0.1113553986120547346, 0.2214566929133858220 ) ) ;
#38474 = CARTESIAN_POINT ( 'NONE',  ( 0.6971942568897626646, 0.07405724077823318263, 0.2362204723871814682 ) ) ;
#38475 = CARTESIAN_POINT ( 'NONE',  ( -0.9412147342319837628, 0.1574803149606300301, 0.6373031494987716483 ) ) ;
#38476 = EDGE_CURVE ( 'NONE', #39669, #46509, #41728, .T. ) ;
#38477 = CARTESIAN_POINT ( 'NONE',  ( 0.7646288533564489232, -0.1113553986120547346, 1.530511811023621993 ) ) ;
#38479 = CARTESIAN_POINT ( 'NONE',  ( -0.1333875707376347142, -0.2184828823904832185, -0.3149606299212598381 ) ) ;
#38478 = CARTESIAN_POINT ( 'NONE',  ( 0.7932464814172374146, 0.1374651347690867276, 1.980054407178728937 ) ) ;
#38480 = CARTESIAN_POINT ( 'NONE',  ( 0.7185039370078746268, -0.06523048226347956391, 0.4552165353255435698 ) ) ;
#38481 = CARTESIAN_POINT ( 'NONE',  ( -0.8759842519685039353, -0.1574803149606299191, 1.643700787294047228 ) ) ;
#38482 = PRESENTATION_LAYER_ASSIGNMENT (  '', '', ( #6313 ) ) ;
#38483 = CARTESIAN_POINT ( 'NONE',  ( -1.033464566929134687, -0.06523048226347956391, 0.7062007872940467834 ) ) ;
#38484 = CARTESIAN_POINT ( 'NONE',  ( 1.054774247047244540, -0.07405724077823318263, 0.9251968503399373711 ) ) ;
#38485 = CARTESIAN_POINT ( 'NONE',  ( 0.9500414927467377701, 0.1787899950787401604, 1.924212598371433325 ) ) ;
#38486 = CARTESIAN_POINT ( 'NONE',  ( 0.8759842519685039353, -0.1574803149606299191, 0.2657480313885358103 ) ) ;
#38487 = ORIENTED_EDGE ( 'NONE', *, *, #5365, .T. ) ;
#38488 = CARTESIAN_POINT ( 'NONE',  ( 0.9412147342319837628, -0.1574803149606297803, 1.252460629813731519 ) ) ;
#38489 = CARTESIAN_POINT ( 'NONE',  ( 0.9873396505805591694, -0.1113553986120547346, 0.2411417322834645827 ) ) ;
#38491 = LINE ( 'NONE', #45654, #5281 ) ;
#38490 = CIRCLE ( 'NONE', #36220, 0.09842519685039370636 ) ;
#38492 = CARTESIAN_POINT ( 'NONE',  ( 0.1574803149606300301, -1.654035432963339103, 0.06523048226347956391 ) ) ;
#38493 = CARTESIAN_POINT ( 'NONE',  ( -1.033464566929134687, -0.06523048226347956391, 0.2731299211523157133 ) ) ;
#38494 = CARTESIAN_POINT ( 'NONE',  ( 1.054774247047244540, -0.07405724077823318263, 1.318897637741511364 ) ) ;
#38495 = CARTESIAN_POINT ( 'NONE',  ( -1.094772975963752103E-17, 0.06840551186478720236, -0.1787899950787401882 ) ) ;
#38496 = CARTESIAN_POINT ( 'NONE',  ( -0.7185039370078739607, 1.928577636452523993E-17, 1.879921259842519676 ) ) ;
#38497 = CARTESIAN_POINT ( 'NONE',  ( -0.9500414927467378812, -0.1787899950787401604, 0.6446850393163160442 ) ) ;
#38498 = LINE ( 'NONE', #24137, #35205 ) ;
#38499 = CARTESIAN_POINT ( 'NONE',  ( -0.05473164110560591739, 0.07681961335491412080, 0.2538337431406300637 ) ) ;
#38501 = EDGE_LOOP ( 'NONE', ( #26614, #6254, #21175, #39730, #22481 ) ) ;
#38500 = AXIS2_PLACEMENT_3D ( 'NONE', #20323, #33611, #3285 ) ;
#38503 = CARTESIAN_POINT ( 'NONE',  ( -0.1787899950787401604, -1.700787401521039355, -0.07405724077823318263 ) ) ;
#38502 = CARTESIAN_POINT ( 'NONE',  ( 0.1113553986120547346, -0.3572834644594020115, 0.1113553986120547346 ) ) ;
#38504 = CARTESIAN_POINT ( 'NONE',  ( -0.6971942568897648851, -0.07405724077823297447, 1.033464566875371027 ) ) ;
#38505 = CARTESIAN_POINT ( 'NONE',  ( -1.002407869896990045, -0.1264236179284866091, 1.906988188922614125 ) ) ;
#38506 = VERTEX_POINT ( 'NONE', #10758 ) ;
#38507 = CARTESIAN_POINT ( 'NONE',  ( -1.054774247047244096, 0.000000000000000000, 0.6569881889226141247 ) ) ;
#38508 = EDGE_CURVE ( 'NONE', #461, #30681, #25832, .T. ) ;
#38509 = ORIENTED_EDGE ( 'NONE', *, *, #26647, .F. ) ;
#38510 = CARTESIAN_POINT ( 'NONE',  ( -0.1951724573785008632, 0.1828112239219657764, -0.3083162604245049954 ) ) ;
#38511 = CARTESIAN_POINT ( 'NONE',  ( -0.9412147342319837628, 0.1574803149606300301, 1.670767716535433545 ) ) ;
#38512 = ORIENTED_EDGE ( 'NONE', *, *, #26554, .T. ) ;
#38513 = CARTESIAN_POINT ( 'NONE',  ( -0.1693402938160395443, -0.08956121756881751939, -0.02606734845562425421 ) ) ;
#38514 = VERTEX_POINT ( 'NONE', #14570 ) ;
#38515 = CARTESIAN_POINT ( 'NONE',  ( 0.4453382816733590377, 4.766607801171850497E-17, 0.000000000000000000 ) ) ;
#38516 = CARTESIAN_POINT ( 'NONE',  ( -0.2471922904502826812, -0.03219022224904098672, -0.1427165354330708902 ) ) ;
#38517 = CARTESIAN_POINT ( 'NONE',  ( -0.7495606340400177148, 0.1264236179284866091, 0.4699803149068661479 ) ) ;
#38518 = CARTESIAN_POINT ( 'NONE',  ( 0.1113553986120547346, 0.06594488188976378729, 0.1113553986120547346 ) ) ;
#38519 = VECTOR ( 'NONE', #8460, 39.37007874015748854 ) ;
#38520 = EDGE_LOOP ( 'NONE', ( #36983, #21704, #7498, #41761, #41763, #17739, #12958, #25650 ) ) ;
#38521 = EDGE_CURVE ( 'NONE', #2430, #8074, #6502, .T. ) ;
#38522 = CARTESIAN_POINT ( 'NONE',  ( -0.8019270111902716547, -0.1787899950787401604, 1.589566929080094226 ) ) ;
#38523 = CARTESIAN_POINT ( 'NONE',  ( 1.054774247047244096, 0.000000000000000000, 0.3026574802611972648 ) ) ;
#38524 = AXIS2_PLACEMENT_3D ( 'NONE', #336, #25769, #22381 ) ;
#38525 = CARTESIAN_POINT ( 'NONE',  ( -0.1264236179284866091, -1.417814960576157635, 0.1264236179284866091 ) ) ;
#38526 = DIRECTION ( 'NONE',  ( 3.478357113474434231E-15, 1.000000000000000000, 0.000000000000000000 ) ) ;
#38527 = EDGE_CURVE ( 'NONE', #28221, #6831, #31076, .T. ) ;
#38528 = CARTESIAN_POINT ( 'NONE',  ( -0.7185039370078739607, 1.928577636452523993E-17, 0.1771653542231816925 ) ) ;
#38529 = CARTESIAN_POINT ( 'NONE',  ( 0.1270800023317771588, -0.6850831796617854463, -0.1270800023317771588 ) ) ;
#38530 = CARTESIAN_POINT ( 'NONE',  ( 1.033464566929133799, 0.000000000000000000, 0.9547244094488189781 ) ) ;
#38531 = CARTESIAN_POINT ( 'NONE',  ( -0.7185039370078739607, 1.928577636452523993E-17, 1.161417322727118284 ) ) ;
#38532 = CARTESIAN_POINT ( 'NONE',  ( 0.8759842519685039353, 0.1787899950787401882, 0.6274606298674959559 ) ) ;
#38534 = CARTESIAN_POINT ( 'NONE',  ( -0.7646288533564489232, 0.1113553986120547346, 0.6840551180027086842 ) ) ;
#38533 = CARTESIAN_POINT ( 'NONE',  ( 0.06523048226347956391, -0.4729330708661419469, -0.1574803149606300301 ) ) ;
#38535 = CARTESIAN_POINT ( 'NONE',  ( 0.000000000000000000, 0.000000000000000000, -0.1377952755905511861 ) ) ;
#38536 = VERTEX_POINT ( 'NONE', #26065 ) ;
#38537 = CARTESIAN_POINT ( 'NONE',  ( -1.033464566929133799, 0.000000000000000000, 0.7874015746956221085 ) ) ;
#38538 = ADVANCED_FACE ( 'NONE', ( #40872 ), #18618, .F. ) ;
#38539 = CARTESIAN_POINT ( 'NONE',  ( -1.054774247047244540, 0.07405724077823318263, 1.131889763725763887 ) ) ;
#38540 = CARTESIAN_POINT ( 'NONE',  ( 0.8759842519685039353, -0.1574803149606299191, 1.062992125984252079 ) ) ;
#38542 = CARTESIAN_POINT ( 'NONE',  ( -0.9129482065544513025, -0.1717787576874445776, 1.988841906250625291 ) ) ;
#38541 = CARTESIAN_POINT ( 'NONE',  ( 0.3123359580052492146, 4.616380251121755931E-17, 0.000000000000000000 ) ) ;
#38543 = FACE_OUTER_BOUND ( 'NONE', #6680, .T. ) ;
#38544 = EDGE_CURVE ( 'NONE', #30859, #894, #41583, .T. ) ;
#38546 = DIRECTION ( 'NONE',  ( 0.000000000000000000, 0.000000000000000000, 1.000000000000000000 ) ) ;
#38545 = CARTESIAN_POINT ( 'NONE',  ( 1.033464566929133799, 0.000000000000000000, 1.299212598317669221 ) ) ;
#38547 = CARTESIAN_POINT ( 'NONE',  ( 0.8107537697050254399, 0.1574803149606300301, 1.272145669183810668 ) ) ;
#38548 = CARTESIAN_POINT ( 'NONE',  ( -0.1684572903745232830, -0.08956285536357470878, -0.03266174313778202887 ) ) ;
#38549 = CARTESIAN_POINT ( 'NONE',  ( 0.07405724077823318263, -0.5639763778989922427, -0.1787899950787401604 ) ) ;
#38550 = VERTEX_POINT ( 'NONE', #8071 ) ;
#38551 = CARTESIAN_POINT ( 'NONE',  ( 0.3100393700787401619, 3.796887221765908018E-17, -0.4921259842519685179 ) ) ;
#38552 = CARTESIAN_POINT ( 'NONE',  ( 1.033464566929134687, -0.06523048226347956391, 0.8735236220472449853 ) ) ;
#38553 = CARTESIAN_POINT ( 'NONE',  ( 1.002407869896990045, 0.1264236179284866091, 0.8144685038832440993 ) ) ;
#38554 = ORIENTED_EDGE ( 'NONE', *, *, #2323, .T. ) ;
#38555 = CARTESIAN_POINT ( 'NONE',  ( 0.7646288533564489232, -0.1113553986120547346, 1.451771653543306950 ) ) ;
#38556 = CARTESIAN_POINT ( 'NONE',  ( 1.737901732061166719E-16, -8.878505979408855953E-16, 0.2933070866141737065 ) ) ;
#38557 = CARTESIAN_POINT ( 'NONE',  ( 0.1264236179284866091, -1.786909448765134023, -0.1264236179284866091 ) ) ;
#38558 = CARTESIAN_POINT ( 'NONE',  ( -0.1264236179284866091, -1.112696850339937038, -0.1264236179284866091 ) ) ;
#38559 = CARTESIAN_POINT ( 'NONE',  ( 0.06523048226347956391, -1.339074803149606474, -0.1574803149606300301 ) ) ;
#38560 = CARTESIAN_POINT ( 'NONE',  ( 0.7646288533564489232, -0.1113553986120547346, 1.205708661309795371 ) ) ;
#38561 = B_SPLINE_CURVE_WITH_KNOTS ( 'NONE', 3,
 ( #9659, #13948, #13485, #21366, #46293, #6510, #31471, #46054, #46528, #28115, #5819, #17539 ),
 .UNSPECIFIED., .F., .F.,
 ( 4, 1, 1, 1, 1, 2, 2, 4 ),
 ( 0.000000000000000000, 0.2500000000000012768, 0.3750000000000018874, 0.4375000000000021094, 0.4687500000000022204, 0.4843750000000023870, 0.5000000000000022204, 1.000000000000000000 ),
 .UNSPECIFIED. ) ;
#38562 = EDGE_LOOP ( 'NONE', ( #15897, #45318, #37497, #43279 ) ) ;
#38563 = ORIENTED_EDGE ( 'NONE', *, *, #28155, .T. ) ;
#38564 = CARTESIAN_POINT ( 'NONE',  ( -0.8019270111902717657, 0.1787899950787401604, 1.850393700733638624 ) ) ;
#38565 = CARTESIAN_POINT ( 'NONE',  ( 1.054774247047244540, 0.07405724077823318263, 1.840551181048599938 ) ) ;
#38566 = VERTEX_POINT ( 'NONE', #41343 ) ;
#38568 = LINE ( 'NONE', #12479, #27191 ) ;
#38567 = VECTOR ( 'NONE', #35477, 39.37007874015748143 ) ;
#38569 = CARTESIAN_POINT ( 'NONE',  ( -1.054774247047244540, -0.07405724077823318263, 1.515748031442299526 ) ) ;
#38570 = CARTESIAN_POINT ( 'NONE',  ( -0.6971942568897637749, 2.189545951927499583E-17, 0.2042322834108035723 ) ) ;
#38571 = CARTESIAN_POINT ( 'NONE',  ( 0.2944196465027555387, 0.09842519685039370636, 0.000000000000000000 ) ) ;
#38572 = CARTESIAN_POINT ( 'NONE',  ( -0.9500414927467378812, 0.1787899950787401604, 1.687992125930489307 ) ) ;
#38573 = CARTESIAN_POINT ( 'NONE',  ( -0.9873396505805591694, -0.1113553986120547346, 1.815944881889763884 ) ) ;
#38574 = PRESENTATION_LAYER_ASSIGNMENT (  '', '', ( #3365 ) ) ;
#38575 = CARTESIAN_POINT ( 'NONE',  ( 0.1377952755905512139, 0.1564960629921262614, -0.9074803149606294195 ) ) ;
#38576 = CARTESIAN_POINT ( 'NONE',  ( 1.002407869896990045, 0.1264236179284866091, 1.724901574749385880 ) ) ;
#38577 = CARTESIAN_POINT ( 'NONE',  ( 0.1778667912632992121, -0.09842519685039370636, 0.1186629878957504020 ) ) ;
#38578 = CARTESIAN_POINT ( 'NONE',  ( -0.06523048226347956391, 0.004429133858267709535, -0.1574803149606300301 ) ) ;
#38579 = ( BOUNDED_CURVE ( )  B_SPLINE_CURVE ( 2, ( #17540, #28601, #15090, #35995, #3154, #47005, #25866, #40448, #29737 ),
 .UNSPECIFIED., .F., .T. ) 
 B_SPLINE_CURVE_WITH_KNOTS ( ( 3, 2, 2, 2, 3 ),
 ( 0.8499999999999999778, 0.8525000000000000355, 0.8549999999999999822, 0.8575000000000000400, 0.8599999999999999867 ),
 .UNSPECIFIED. ) 
 CURVE ( )  GEOMETRIC_REPRESENTATION_ITEM ( )  RATIONAL_B_SPLINE_CURVE ( ( 1.000000000000000000, 0.9238795325112869605, 1.000000000000000000, 0.9238795325112869605, 1.000000000000000000, 0.9238795325112869605, 1.000000000000000000, 0.9238795325112869605, 1.000000000000000000 ) ) 
 REPRESENTATION_ITEM ( '' )  ) ;
#38580 = ORIENTED_EDGE ( 'NONE', *, *, #7959, .T. ) ;
#38581 = EDGE_CURVE ( 'NONE', #23021, #22067, #620, .T. ) ;
#38582 = CARTESIAN_POINT ( 'NONE',  ( -1.002407869896990045, 0.1264236179284866091, 1.291830708607653477 ) ) ;
#38583 = CARTESIAN_POINT ( 'NONE',  ( -1.094772975963752103E-17, -0.9995078739619842612, -0.1787899950787401882 ) ) ;
#38584 = CARTESIAN_POINT ( 'NONE',  ( 0.07405724077823318263, -1.248031496009228913, 0.1787899950787401604 ) ) ;
#38585 = CARTESIAN_POINT ( 'NONE',  ( -1.033464566929133799, 0.000000000000000000, 0.6003937007874016185 ) ) ;
#38586 = CARTESIAN_POINT ( 'NONE',  ( -0.07444174185955065859, -0.4808508961972187135, -0.1797182628040039087 ) ) ;
#38587 = CARTESIAN_POINT ( 'NONE',  ( -0.1113553986120547346, -1.823818897530267602, 0.1113553986120547346 ) ) ;
#38588 = CARTESIAN_POINT ( 'NONE',  ( -0.7646288533564489232, -0.1113553986120547346, 0.8120078739082204899 ) ) ;
#38589 = CARTESIAN_POINT ( 'NONE',  ( -1.033464566929134687, -0.06523048226347956391, 0.7947834645669291653 ) ) ;
#38590 = CARTESIAN_POINT ( 'NONE',  ( 0.1113553986120547346, -0.002952755905511810983, -0.1113553986120547346 ) ) ;
#38591 = EDGE_CURVE ( 'NONE', #18156, #38980, #37070, .T. ) ;
#38592 = CARTESIAN_POINT ( 'NONE',  ( 1.002407869896990045, -0.1264236179284866091, 0.8833661416785196785 ) ) ;
#38593 = ( BOUNDED_CURVE ( )  B_SPLINE_CURVE ( 2, ( #18857, #14574, #18626, #26325, #29247, #37305, #10994, #18400, #43795 ),
 .UNSPECIFIED., .F., .T. ) 
 B_SPLINE_CURVE_WITH_KNOTS ( ( 3, 2, 2, 2, 3 ),
 ( 0.02500000000000000139, 0.02750000000000000014, 0.02999999999999999889, 0.03250000000000000111, 0.03500000000000000333 ),
 .UNSPECIFIED. ) 
 CURVE ( )  GEOMETRIC_REPRESENTATION_ITEM ( )  RATIONAL_B_SPLINE_CURVE ( ( 1.000000000000000000, 0.9238795325112869605, 1.000000000000000000, 0.9238795325112869605, 1.000000000000000000, 0.9238795325112869605, 1.000000000000000000, 0.9238795325112869605, 1.000000000000000000 ) ) 
 REPRESENTATION_ITEM ( '' )  ) ;
#38594 = CARTESIAN_POINT ( 'NONE',  ( 0.7646288533564489232, 0.1113553986120547346, 0.09350393690034704275 ) ) ;
#38595 = VERTEX_POINT ( 'NONE', #37297 ) ;
#38596 = CARTESIAN_POINT ( 'NONE',  ( 0.4934383202099732468, 4.616380251121755931E-17, 0.000000000000000000 ) ) ;
#38598 = CARTESIAN_POINT ( 'NONE',  ( 0.1264236179284866091, -0.4138779527021417826, -0.1264236179284866091 ) ) ;
#38597 = CARTESIAN_POINT ( 'NONE',  ( 0.1113553986120547346, -0.9773622046168818356, -0.1113553986120547346 ) ) ;
#38599 = CARTESIAN_POINT ( 'NONE',  ( 0.000000000000000000, 0.000000000000000000, -0.3149606299212598381 ) ) ;
#38600 = CARTESIAN_POINT ( 'NONE',  ( -0.1787899950787401604, -1.375984251914741163, 0.07405724077823318263 ) ) ;
#38601 = CARTESIAN_POINT ( 'NONE',  ( -0.8759842519685039353, -0.1787899950787401882, 1.862696850339937038 ) ) ;
#38602 = ORIENTED_EDGE ( 'NONE', *, *, #20592, .T. ) ;
#38603 = CARTESIAN_POINT ( 'NONE',  ( -0.7495606340400177148, -0.1264236179284866091, 1.508366141678519678 ) ) ;
#38604 = CARTESIAN_POINT ( 'NONE',  ( 1.002407869896990045, 0.1264236179284866091, 1.370570866087968520 ) ) ;
#38605 = DIRECTION ( 'NONE',  ( 1.000000000000000000, 0.000000000000000000, 0.000000000000000000 ) ) ;
#38606 = CARTESIAN_POINT ( 'NONE',  ( 0.1113553986120547346, -1.252952755797984041, -0.1113553986120547346 ) ) ;
#38607 = CARTESIAN_POINT ( 'NONE',  ( -1.054774247047244096, 0.000000000000000000, 0.6963582676627716461 ) ) ;
#38608 = CARTESIAN_POINT ( 'NONE',  ( 0.6971942568897637749, 2.189545951927499583E-17, 0.1254921259304885850 ) ) ;
#38609 = CARTESIAN_POINT ( 'NONE',  ( -1.054774247047244540, -0.07405724077823318263, 1.279527559001355286 ) ) ;
#38610 = CARTESIAN_POINT ( 'NONE',  ( 0.1623548122380495395, -0.09842494649416595742, -0.07493597120910913678 ) ) ;
#38611 = CARTESIAN_POINT ( 'NONE',  ( 1.054774247047244096, 0.000000000000000000, 0.6569881889226141247 ) ) ;
#38612 = CARTESIAN_POINT ( 'NONE',  ( -0.7495606340400177148, 0.1264236179284866091, 0.5487204723871811352 ) ) ;
#38613 = DIRECTION ( 'NONE',  ( 0.000000000000000000, 1.000000000000000000, 0.000000000000000000 ) ) ;
#38614 = CARTESIAN_POINT ( 'NONE',  ( 1.033464566929133355, 0.06523048226348168721, 1.656003936900346973 ) ) ;
#38615 = ORIENTED_EDGE ( 'NONE', *, *, #28615, .F. ) ;
#38616 = ORIENTED_EDGE ( 'NONE', *, *, #2630, .F. ) ;
#38617 = AXIS2_PLACEMENT_3D ( 'NONE', #45928, #27777, #13140 ) ;
#38618 = CARTESIAN_POINT ( 'NONE',  ( -0.7185039370078746268, -0.06523048226347956391, 0.2288385826771656140 ) ) ;
#38619 = CARTESIAN_POINT ( 'NONE',  ( 0.8019270111902716547, -0.1787899950787401604, 1.274606299158834277 ) ) ;
#38620 = CARTESIAN_POINT ( 'NONE',  ( 0.02849075975873720593, -0.09851384916348070175, 0.2212810442481748241 ) ) ;
#38621 = CARTESIAN_POINT ( 'NONE',  ( -0.9412147342319837628, -0.1574803149606297803, 1.843011810916095783 ) ) ;
#38622 = AXIS2_PLACEMENT_3D ( 'NONE', #39079, #10107, #20876 ) ;
#38623 = AXIS2_PLACEMENT_3D ( 'NONE', #22853, #4617, #19251 ) ;
#38624 = ORIENTED_EDGE ( 'NONE', *, *, #35185, .F. ) ;
#38625 = EDGE_CURVE ( 'NONE', #45189, #43030, #29570, .T. ) ;
#38626 = CARTESIAN_POINT ( 'NONE',  ( -1.002407869896990045, 0.1264236179284866091, 1.016240157426551161 ) ) ;
#38627 = ADVANCED_FACE ( 'NONE', ( #22932 ), #15280, .F. ) ;
#38628 = CARTESIAN_POINT ( 'NONE',  ( -0.1787899950787401882, -1.591167275315852558, 0.000000000000000000 ) ) ;
#38629 = ORIENTED_EDGE ( 'NONE', *, *, #44244, .T. ) ;
#38630 = LINE ( 'NONE', #35049, #18020 ) ;
#38631 = CARTESIAN_POINT ( 'NONE',  ( 0.1787899950787401604, -0.5295275590013543976, -0.07405724077823318263 ) ) ;
#38632 = ADVANCED_FACE ( 'NONE', ( #15053 ), #4448, .F. ) ;
#38633 = CARTESIAN_POINT ( 'NONE',  ( -0.9412147342319837628, -0.1574803149606297803, 0.08120078740157483932 ) ) ;
#38634 = VERTEX_POINT ( 'NONE', #8544 ) ;
#38635 = CARTESIAN_POINT ( 'NONE',  ( 0.8759842519685039353, -0.1787899950787401882, 1.468996062938362046 ) ) ;
#38636 = EDGE_CURVE ( 'NONE', #18185, #8992, #33508, .T. ) ;
#38637 = CARTESIAN_POINT ( 'NONE',  ( -0.08471839801768285549, 0.2465807710546494280, -0.3122165016185723951 ) ) ;
#38638 = CARTESIAN_POINT ( 'NONE',  ( -0.07405724077823318263, -0.3277559054580475584, -0.1787899950787401604 ) ) ;
#38639 = CARTESIAN_POINT ( 'NONE',  ( -0.1787899950787401604, -0.7116141731745821986, -0.07405724077823318263 ) ) ;
#38640 = CARTESIAN_POINT ( 'NONE',  ( -0.8070866141732283561, -0.0009842519685049383633, -0.7574803149606299524 ) ) ;
#38641 = CARTESIAN_POINT ( 'NONE',  ( 1.033464566929133799, 0.000000000000000000, 1.811023621939716444 ) ) ;
#38642 = CARTESIAN_POINT ( 'NONE',  ( 1.054774247047244540, -0.07405724077823318263, 1.594488188922613237 ) ) ;
#38643 = CARTESIAN_POINT ( 'NONE',  ( -0.1787899950787401604, 0.05991540184950147618, -0.07405724077823318263 ) ) ;
#38644 = CONTEXT_DEPENDENT_SHAPE_REPRESENTATION ( #40677, #44811 ) ;
#38645 = DIRECTION ( 'NONE',  ( 0.8191520442889873577, 0.000000000000000000, 0.5735764363510523767 ) ) ;
#38646 = CARTESIAN_POINT ( 'NONE',  ( 0.6971942568897637749, 2.189545951927499583E-17, 0.4749015747493858242 ) ) ;
#38647 = CARTESIAN_POINT ( 'NONE',  ( -0.7495606340400177148, -0.1264236179284866091, 0.8390748030958424808 ) ) ;
#38649 = CARTESIAN_POINT ( 'NONE',  ( 0.7646288533564489232, 0.1113553986120547346, 0.09350393690034704275 ) ) ;
#38648 = CARTESIAN_POINT ( 'NONE',  ( -0.1574803149606300301, -0.8567913385826780859, -0.06523048226347956391 ) ) ;
#38651 = CARTESIAN_POINT ( 'NONE',  ( -0.7299953799755746209, -0.08597721908260566592, 1.984947195527895225 ) ) ;
#38650 = CARTESIAN_POINT ( 'NONE',  ( -0.07444174185955065859, -1.543843022181471847, -0.1797182628040039087 ) ) ;
#38652 = VECTOR ( 'NONE', #12896, 39.37007874015748143 ) ;
#38653 = AXIS2_PLACEMENT_3D ( 'NONE', #16813, #31451, #42431 ) ;
#38654 = CARTESIAN_POINT ( 'NONE',  ( -0.1787899950787401604, -0.3572834645131658382, -0.07405724077823318263 ) ) ;
#38655 = CARTESIAN_POINT ( 'NONE',  ( -0.7646288533564489232, 0.1113553986120547346, 1.038385826664126155 ) ) ;
#38656 = CARTESIAN_POINT ( 'NONE',  ( 0.9500414927467378812, -0.1787899950787401604, 1.515748031442299526 ) ) ;
#38657 = CARTESIAN_POINT ( 'NONE',  ( 0.1572451146043649106, 0.09317026862874189241, -0.1946475616205581294 ) ) ;
#38658 = CARTESIAN_POINT ( 'NONE',  ( 0.8019270111902716547, -0.1787899950787401604, 0.3641732282926931630 ) ) ;
#38659 = AXIS2_PLACEMENT_3D ( 'NONE', #45680, #35172, #41361 ) ;
#38660 = AXIS2_PLACEMENT_3D ( 'NONE', #42565, #13830, #38765 ) ;
#38662 = ORIENTED_EDGE ( 'NONE', *, *, #31937, .T. ) ;
#38661 = LINE ( 'NONE', #45587, #22233 ) ;
#38663 = CARTESIAN_POINT ( 'NONE',  ( -0.8759842519685039353, 0.000000000000000000, 0.000000000000000000 ) ) ;
#38665 = CARTESIAN_POINT ( 'NONE',  ( 0.1787899950787401882, -0.02509842514308689362, -2.189545951927503898E-17 ) ) ;
#38664 = CARTESIAN_POINT ( 'NONE',  ( -0.1574803149606297803, -0.8813976376877487029, 0.06523048226347956391 ) ) ;
#38666 = DIRECTION ( 'NONE',  ( -1.000000000000000000, 0.000000000000000000, 0.000000000000000000 ) ) ;
#38667 = CARTESIAN_POINT ( 'NONE',  ( -1.094772975963752103E-17, -0.04970472435568527164, -0.1787899950787401882 ) ) ;
#38668 = CARTESIAN_POINT ( 'NONE',  ( 1.002407869896990045, -0.1264236179284866091, 0.3715551180564728440 ) ) ;
#38669 = CARTESIAN_POINT ( 'NONE',  ( 0.1264236179284866091, -0.9306102361667086820, 0.1264236179284866091 ) ) ;
#38670 = CARTESIAN_POINT ( 'NONE',  ( 0.8484761801896820721, -0.1575117747672026836, 0.03936098705002191028 ) ) ;
#38672 = CARTESIAN_POINT ( 'NONE',  ( 0.000000000000000000, 0.000000000000000000, -0.07924015748031493223 ) ) ;
#38671 = CARTESIAN_POINT ( 'NONE',  ( 1.054774247047244540, 0.07405724077823318263, 1.323818897584032594 ) ) ;
#38673 = CARTESIAN_POINT ( 'NONE',  ( -0.7495606340400177148, 0.1264236179284866091, 1.414862204670645829 ) ) ;
#38674 = CARTESIAN_POINT ( 'NONE',  ( 0.8759842519685039353, 0.1574803149606299191, 0.7972440943806614611 ) ) ;
#38675 = ORIENTED_EDGE ( 'NONE', *, *, #29563, .T. ) ;
#38676 = DIRECTION ( 'NONE',  ( 0.000000000000000000, 0.000000000000000000, 1.000000000000000000 ) ) ;
#38677 = CARTESIAN_POINT ( 'NONE',  ( 0.8759842519685039353, -0.1787899950787401882, 1.080216535379306952 ) ) ;
#38678 = ORIENTED_EDGE ( 'NONE', *, *, #8615, .F. ) ;
#38680 = ORIENTED_EDGE ( 'NONE', *, *, #40868, .T. ) ;
#38679 = CARTESIAN_POINT ( 'NONE',  ( -0.1787899950787401604, -1.302165354276944242, 0.07405724077823318263 ) ) ;
#38681 = CARTESIAN_POINT ( 'NONE',  ( -0.9873396505805591694, -0.1113553986120547346, 0.5462598424121581919 ) ) ;
#38682 = FACE_OUTER_BOUND ( 'NONE', #26249, .T. ) ;
#38683 = CARTESIAN_POINT ( 'NONE',  ( 0.6971942568897637749, 2.189545951927499583E-17, 1.695374015694267822 ) ) ;
#38684 = CARTESIAN_POINT ( 'NONE',  ( -1.033464566929134687, -0.06523048226347956391, 1.385334645669290987 ) ) ;
#38685 = CARTESIAN_POINT ( 'NONE',  ( 1.033464566929133799, 0.000000000000000000, 1.811023621939716444 ) ) ;
#38686 = DIRECTION ( 'NONE',  ( 0.000000000000000000, 0.000000000000000000, 1.000000000000000000 ) ) ;
#38687 = CARTESIAN_POINT ( 'NONE',  ( 0.8759842519685039353, -0.1787899950787401882, 0.1747047243556852092 ) ) ;
#38688 = CARTESIAN_POINT ( 'NONE',  ( -0.8759842519685039353, -0.1787899950787401882, 0.1304133857730082613 ) ) ;
#38689 = CARTESIAN_POINT ( 'NONE',  ( 1.033464566929134687, 0.06523048226347956391, 1.419783464459402289 ) ) ;
#38690 = ORIENTED_EDGE ( 'NONE', *, *, #19690, .F. ) ;
#38691 = ORIENTED_EDGE ( 'NONE', *, *, #16832, .F. ) ;
#38692 = ORIENTED_EDGE ( 'NONE', *, *, #28549, .T. ) ;
#38693 = LINE ( 'NONE', #17346, #43551 ) ;
#38694 = CARTESIAN_POINT ( 'NONE',  ( -1.002407869896990045, 0.1264236179284866091, 1.759350393647023614 ) ) ;
#38695 = ORIENTED_EDGE ( 'NONE', *, *, #686, .F. ) ;
#38696 = EDGE_CURVE ( 'NONE', #45388, #5152, #19083, .T. ) ;
#38697 = CARTESIAN_POINT ( 'NONE',  ( -0.2471922904502826257, 0.09379707428445145656, -0.03645092102368886755 ) ) ;
#38698 = CARTESIAN_POINT ( 'NONE',  ( 0.3980944881889790787, 0.7681739484881634494, -0.04983111751016747887 ) ) ;
#38699 = CARTESIAN_POINT ( 'NONE',  ( 0.1787899950787401604, -1.135950739882782834, -0.07405724077823318263 ) ) ;
#38700 = VERTEX_POINT ( 'NONE', #16002 ) ;
#38701 = CARTESIAN_POINT ( 'NONE',  ( 0.07405724077823318263, -0.1062992125446616531, 0.1787899950787401604 ) ) ;
#38702 = ORIENTED_EDGE ( 'NONE', *, *, #12586, .F. ) ;
#38703 = EDGE_CURVE ( 'NONE', #24486, #36924, #30624, .T. ) ;
#38704 = EDGE_LOOP ( 'NONE', ( #39560, #6258, #23960, #31697, #37609 ) ) ;
#38705 = ADVANCED_FACE ( 'NONE', ( #15525 ), #44950, .T. ) ;
#38706 = CARTESIAN_POINT ( 'NONE',  ( 1.033464566929133799, 1.928577636452524610E-17, 4.498031496062992574 ) ) ;
#38707 = LINE ( 'NONE', #13531, #41394 ) ;
#38708 = CARTESIAN_POINT ( 'NONE',  ( 1.033464566929133799, 0.000000000000000000, 1.860236220472440971 ) ) ;
#38709 = CARTESIAN_POINT ( 'NONE',  ( 0.1264236179284866091, -0.6599409448281259305, 0.1264236179284866091 ) ) ;
#38710 = ( BOUNDED_CURVE ( )  B_SPLINE_CURVE ( 2, ( #15191, #26453, #40784, #32946, #36752, #43691, #40551, #36525, #41018 ),
 .UNSPECIFIED., .F., .T. ) 
 B_SPLINE_CURVE_WITH_KNOTS ( ( 3, 2, 2, 2, 3 ),
 ( 0.8399999999999999689, 0.8425000000000000266, 0.8449999999999999734, 0.8475000000000000311, 0.8499999999999999778 ),
 .UNSPECIFIED. ) 
 CURVE ( )  GEOMETRIC_REPRESENTATION_ITEM ( )  RATIONAL_B_SPLINE_CURVE ( ( 1.000000000000000000, 0.9238795325112869605, 1.000000000000000000, 0.9238795325112869605, 1.000000000000000000, 0.9238795325112869605, 1.000000000000000000, 0.9238795325112799661, 1.000000000000000000 ) ) 
 REPRESENTATION_ITEM ( '' )  ) ;
#38711 = CARTESIAN_POINT ( 'NONE',  ( -0.8019270111902716547, -0.1787899950787401604, 0.3297244093950555954 ) ) ;
#38712 = CARTESIAN_POINT ( 'NONE',  ( -0.7185039370078746268, 0.06523048226347956391, 1.011318897637796033 ) ) ;
#38713 = CARTESIAN_POINT ( 'NONE',  ( -0.1270800023317771588, -1.098469006433439032, 0.1270800023317771588 ) ) ;
#38714 = CARTESIAN_POINT ( 'NONE',  ( -0.2071276943281862848, 0.1759090021854023134, -0.06129781628412492994 ) ) ;
#38715 = CARTESIAN_POINT ( 'NONE',  ( 0.7495606340400177148, 0.1264236179284866091, 1.144192913332062966 ) ) ;
#38716 = CARTESIAN_POINT ( 'NONE',  ( 1.002407869896990045, -0.1264236179284866091, 1.513287401521039355 ) ) ;
#38717 = CARTESIAN_POINT ( 'NONE',  ( 0.000000000000000000, -0.09842519685039370636, 0.000000000000000000 ) ) ;
#38718 = CARTESIAN_POINT ( 'NONE',  ( 0.7185039370078746268, 0.06523048226347956391, 1.562500000000000000 ) ) ;
#38720 = CARTESIAN_POINT ( 'NONE',  ( 0.7646288533564489232, 0.1113553986120547346, 1.717519685039369914 ) ) ;
#38719 = PLANE ( 'NONE',  #25948 ) ;
#38721 = CARTESIAN_POINT ( 'NONE',  ( 0.4330708661417322913, 4.616380251121755931E-17, 0.000000000000000000 ) ) ;
#38722 = DIRECTION ( 'NONE',  ( 0.000000000000000000, 1.000000000000000000, 8.673617379884034486E-16 ) ) ;
#38723 = DIRECTION ( 'NONE',  ( 1.822029033848725028E-16, 0.000000000000000000, 1.000000000000000000 ) ) ;
#38724 = CARTESIAN_POINT ( 'NONE',  ( 0.6971942568897637749, 2.189545951927499583E-17, 0.9079724408911180600 ) ) ;
#38725 = CARTESIAN_POINT ( 'NONE',  ( 1.002407869896990045, -0.1264236179284866091, 1.951279527505291433 ) ) ;
#38726 = CARTESIAN_POINT ( 'NONE',  ( 0.9873396505805591694, 0.1113553986120547346, 0.2805118109160948947 ) ) ;
#38727 = ORIENTED_EDGE ( 'NONE', *, *, #27375, .T. ) ;
#38728 = LINE ( 'NONE', #12872, #42904 ) ;
#38729 = CARTESIAN_POINT ( 'NONE',  ( 0.1113553986120547346, -1.656496062884598386, 0.1113553986120547346 ) ) ;
#38730 = CARTESIAN_POINT ( 'NONE',  ( -0.7185039370078746268, -0.06523048226347956391, 0.2189960628845991353 ) ) ;
#38731 = CARTESIAN_POINT ( 'NONE',  ( 0.2397010884053811242, 4.466152701071653354E-17, 0.000000000000000000 ) ) ;
#38732 = CARTESIAN_POINT ( 'NONE',  ( 0.9500414927467378812, -0.1787899950787401604, 1.353346456639149986 ) ) ;
#38734 = CARTESIAN_POINT ( 'NONE',  ( -0.8759842519685039353, 0.1574803149606299191, 0.2854330707586145710 ) ) ;
#38733 = CARTESIAN_POINT ( 'NONE',  ( 0.3980944881889770248, 0.1864803149606327204, 0.7480314960629921295 ) ) ;
#38735 = CARTESIAN_POINT ( 'NONE',  ( -0.1574803149606299191, -1.759842519685039353, 0.000000000000000000 ) ) ;
#38736 = DIRECTION ( 'NONE',  ( 0.000000000000000000, 0.000000000000000000, -1.000000000000000000 ) ) ;
#38737 = ADVANCED_BREP_SHAPE_REPRESENTATION ( 'Hook Bracket', ( #3862, #20860 ), #31601 ) ;
#38738 = CARTESIAN_POINT ( 'NONE',  ( -0.7495606340400177148, -0.1264236179284866091, 0.5979330708123780092 ) ) ;
#38739 = DIRECTION ( 'NONE',  ( 0.000000000000000000, -1.000000000000000000, 0.000000000000000000 ) ) ;
#38740 = LINE ( 'NONE', #1831, #30757 ) ;
#38741 = EDGE_LOOP ( 'NONE', ( #29593, #41637, #28956, #32190 ) ) ;
#38742 = EDGE_LOOP ( 'NONE', ( #11980, #35945, #45435, #25137 ) ) ;
#38743 = CARTESIAN_POINT ( 'NONE',  ( -1.054774247047244540, 0.07405724077823318263, 1.363188976324188673 ) ) ;
#38745 = CARTESIAN_POINT ( 'NONE',  ( -0.07405724077823318263, -1.745078740103716886, -0.1787899950787401604 ) ) ;
#38744 = CARTESIAN_POINT ( 'NONE',  ( 0.1574803149606300301, -0.3941929132782996947, 0.06523048226347956391 ) ) ;
#38746 = CARTESIAN_POINT ( 'NONE',  ( -0.9500414927467378812, -0.1787899950787401604, 1.003937007820251193 ) ) ;
#38747 = CARTESIAN_POINT ( 'NONE',  ( -0.8019270111902717657, -0.1787899950787401604, 1.899606299158834943 ) ) ;
#38748 = ORIENTED_EDGE ( 'NONE', *, *, #7618, .T. ) ;
#38749 = CARTESIAN_POINT ( 'NONE',  ( -1.054774247047244540, -0.07405724077823318263, 0.6938976377415123631 ) ) ;
#38750 = EDGE_CURVE ( 'NONE', #25854, #3057, #8329, .T. ) ;
#38751 = DIRECTION ( 'NONE',  ( 1.000000000000000000, 0.000000000000000000, 0.000000000000000000 ) ) ;
#38752 = CARTESIAN_POINT ( 'NONE',  ( -0.8107537697050254399, 0.1574803149606300301, 0.09104330697908723236 ) ) ;
#38753 = ORIENTED_EDGE ( 'NONE', *, *, #23116, .F. ) ;
#38754 = CARTESIAN_POINT ( 'NONE',  ( 0.1577181258794738139, -0.08956002199932618091, 0.1424585403325043520 ) ) ;
#38755 = CARTESIAN_POINT ( 'NONE',  ( -0.7185039370078739607, 1.928577636452523993E-17, 0.6496062991050708391 ) ) ;
#38756 = ORIENTED_EDGE ( 'NONE', *, *, #41511, .T. ) ;
#38757 = CARTESIAN_POINT ( 'NONE',  ( -0.02739131347899105909, -0.09752745740044843625, 0.1550798682808147422 ) ) ;
#38758 = EDGE_CURVE ( 'NONE', #8121, #1697, #36208, .T. ) ;
#38759 = CARTESIAN_POINT ( 'NONE',  ( -0.9412147342319837628, -0.1574803149606297803, 1.764271653435779852 ) ) ;
#38760 = CARTESIAN_POINT ( 'NONE',  ( -0.7495606340400177148, 0.1264236179284866091, 0.6668307086076534773 ) ) ;
#38761 = DIRECTION ( 'NONE',  ( 1.000000000000000000, 0.000000000000000000, 0.000000000000000000 ) ) ;
#38762 = ORIENTED_EDGE ( 'NONE', *, *, #6215, .T. ) ;
#38763 = CARTESIAN_POINT ( 'NONE',  ( -0.9500414927467377701, 0.1787899950787401604, 1.727362204670645385 ) ) ;
#38764 = CARTESIAN_POINT ( 'NONE',  ( 0.1822895153388602307, 0.000000000000000000, 0.000000000000000000 ) ) ;
#38765 = DIRECTION ( 'NONE',  ( 0.000000000000000000, -0.000000000000000000, 1.000000000000000000 ) ) ;
#38766 = CARTESIAN_POINT ( 'NONE',  ( 0.1797182628040039365, -0.7687445969846200544, -2.200913952912460540E-17 ) ) ;
#38767 = CARTESIAN_POINT ( 'NONE',  ( 0.03901279071809810040, -0.09842519685039370636, 1.713085361781127913 ) ) ;
#38768 = CARTESIAN_POINT ( 'NONE',  ( -1.033464566929133799, 0.000000000000000000, 1.259842519577511810 ) ) ;
#38770 = CARTESIAN_POINT ( 'NONE',  ( -0.1738374315028377304, -0.09842519685039370636, 0.01279107473069981266 ) ) ;
#38769 = CARTESIAN_POINT ( 'NONE',  ( -0.1574803149606297803, -0.4581692913385826404, 0.06523048226347956391 ) ) ;
#38771 = CARTESIAN_POINT ( 'NONE',  ( -0.8759842519685039353, 0.1574803149606299191, 0.4133858267716535861 ) ) ;
#38772 = EDGE_LOOP ( 'NONE', ( #9577, #23478 ) ) ;
#38773 = CARTESIAN_POINT ( 'NONE',  ( 0.1574803149606300301, 0.02903543307086614220, 0.06523048226347956391 ) ) ;
#38774 = CARTESIAN_POINT ( 'NONE',  ( 0.8107537697050253289, 0.1574803149606300301, 1.124507874015748810 ) ) ;
#38776 = CARTESIAN_POINT ( 'NONE',  ( 3.060083392313581123E-15, 0.9310112235910578127, -1.064878870394357468 ) ) ;
#38775 = CARTESIAN_POINT ( 'NONE',  ( 0.8070866141732283561, -0.3937007874015746034, 0.6590551181102368705 ) ) ;
#38777 = DIRECTION ( 'NONE',  ( -1.000000000000000000, 0.000000000000000000, 0.000000000000000000 ) ) ;
#38778 = EDGE_CURVE ( 'NONE', #6083, #22780, #1208, .T. ) ;
#38780 = DIRECTION ( 'NONE',  ( -3.469446951953608272E-15, -1.000000000000000000, 0.000000000000000000 ) ) ;
#38779 = CARTESIAN_POINT ( 'NONE',  ( 0.7185039370078746268, 0.06523048226347956391, 0.1845472440944882775 ) ) ;
#38781 = DIRECTION ( 'NONE',  ( -0.000000000000000000, 1.000000000000000000, -0.000000000000000000 ) ) ;
#38782 = CARTESIAN_POINT ( 'NONE',  ( -0.1688295671091639694, -0.08956462757123960505, -0.02832533445597745780 ) ) ;
#38783 = CARTESIAN_POINT ( 'NONE',  ( -0.1787899950787401604, -0.5492125983714331028, 0.07405724077823318263 ) ) ;
#38784 = CARTESIAN_POINT ( 'NONE',  ( 0.2066929133858268486, -0.9875035750853327077, -1.463737590216208861 ) ) ;
#38785 = VERTEX_POINT ( 'NONE', #45428 ) ;
#38786 = CARTESIAN_POINT ( 'NONE',  ( -0.2066929133858267931, -0.3022687907404924545, -1.075852903322848331 ) ) ;
#38787 = CARTESIAN_POINT ( 'NONE',  ( 0.7495606340400177148, 0.1264236179284866091, 0.8243110235682834519 ) ) ;
#38788 = CARTESIAN_POINT ( 'NONE',  ( -0.01993724539793482325, 0.05212746764698077823, -0.2739222968687445303 ) ) ;
#38789 = CARTESIAN_POINT ( 'NONE',  ( 0.9412147342319837628, -0.1574803149606297803, 0.7012795274515276622 ) ) ;
#38790 = CARTESIAN_POINT ( 'NONE',  ( 0.07444174185955046430, 0.06540894632246617435, -0.1797182628040039087 ) ) ;
#38791 = CARTESIAN_POINT ( 'NONE',  ( -0.1787899950787401604, -1.026574803095842370, 0.07405724077823318263 ) ) ;
#38792 = CARTESIAN_POINT ( 'NONE',  ( -0.1574803149606299191, -1.366141732283464583, 0.000000000000000000 ) ) ;
#38793 = CARTESIAN_POINT ( 'NONE',  ( 0.9873396505805591694, 0.1113553986120547346, 1.264763779420031486 ) ) ;
#38794 = ORIENTED_EDGE ( 'NONE', *, *, #39622, .F. ) ;
#38795 = CARTESIAN_POINT ( 'NONE',  ( -0.8759842519685039353, -0.1787899950787401882, 1.985728346402929168 ) ) ;
#38796 = CARTESIAN_POINT ( 'NONE',  ( 0.6971942568897637749, 2.189545951927499583E-17, 1.857775590497417362 ) ) ;
#38797 = ORIENTED_EDGE ( 'NONE', *, *, #5852, .F. ) ;
#38798 = CARTESIAN_POINT ( 'NONE',  ( -0.1574803149606300301, -1.437499999892472013, -0.06523048226347956391 ) ) ;
#38799 = CARTESIAN_POINT ( 'NONE',  ( 0.9873396505805591694, -0.1113553986120547346, 0.5561023622047244208 ) ) ;
#38800 = CARTESIAN_POINT ( 'NONE',  ( -0.6971942568897648851, 0.07405724077823318263, 1.496062992072220821 ) ) ;
#38801 = DIRECTION ( 'NONE',  ( -1.000000000000000000, 0.000000000000000000, 0.000000000000000000 ) ) ;
#38802 = ADVANCED_FACE ( 'NONE', ( #28196, #42535, #1826 ), #16696, .F. ) ;
#38803 = CARTESIAN_POINT ( 'NONE',  ( -1.054774247047244540, 0.07405724077823318263, 0.2263779527021421711 ) ) ;
#38804 = EDGE_CURVE ( 'NONE', #23245, #30756, #38023, .T. ) ;
#38805 = FACE_OUTER_BOUND ( 'NONE', #24941, .T. ) ;
#38806 = CARTESIAN_POINT ( 'NONE',  ( -0.9500414927467378812, 0.1787899950787401604, 1.963582677111591401 ) ) ;
#38807 = DIRECTION ( 'NONE',  ( 1.000000000000000000, 5.372880794957870593E-15, -4.197754538034579871E-15 ) ) ;
#38808 = CARTESIAN_POINT ( 'NONE',  ( -0.9412147342319837628, -0.1574803149606297803, 1.774114173228345859 ) ) ;
#38809 = CARTESIAN_POINT ( 'NONE',  ( 0.2559029816877552155, 0.01435274667127873181, -0.02805003521115247145 ) ) ;
#38810 = CARTESIAN_POINT ( 'NONE',  ( 0.2074171527642326707, -0.09842519685039548272, 0.02027778249552708578 ) ) ;
#38811 = CARTESIAN_POINT ( 'NONE',  ( -0.06523048226347956391, 0.01919291338582680001, 0.1574803149606297803 ) ) ;
#38812 = CARTESIAN_POINT ( 'NONE',  ( -0.7185039370078746268, 0.06523048226347956391, 0.05659448808144944970 ) ) ;
#38813 = EDGE_CURVE ( 'NONE', #42574, #10554, #42521, .T. ) ;
#38814 = AXIS2_PLACEMENT_3D ( 'NONE', #27810, #46909, #16749 ) ;
#38815 = ORIENTED_EDGE ( 'NONE', *, *, #17964, .T. ) ;
#38816 = ORIENTED_EDGE ( 'NONE', *, *, #36848, .F. ) ;
#38817 = CARTESIAN_POINT ( 'NONE',  ( 3.284318927891251994E-17, -1.019192913332062966, 0.1787899950787401882 ) ) ;
#38818 = CARTESIAN_POINT ( 'NONE',  ( 0.1264236179284866091, -1.235728346402928945, -0.1264236179284866091 ) ) ;
#38819 = LINE ( 'NONE', #6449, #32500 ) ;
#38820 = CARTESIAN_POINT ( 'NONE',  ( -0.1270800023317771588, -0.5472879040712346210, 0.1270800023317771588 ) ) ;
#38821 = CARTESIAN_POINT ( 'NONE',  ( 0.4151545546392377273, 4.766607801171850497E-17, 0.000000000000000000 ) ) ;
#38822 = CARTESIAN_POINT ( 'NONE',  ( -1.033464566929134687, 0.06523048226347956391, 0.6815944881889761664 ) ) ;
#38823 = CARTESIAN_POINT ( 'NONE',  ( 0.1113553986120547346, -0.04232283464566929249, -0.1113553986120547346 ) ) ;
#38824 = CARTESIAN_POINT ( 'NONE',  ( 0.9500414927467378812, 0.1787899950787401604, 0.8956692912848198684 ) ) ;
#38825 = CARTESIAN_POINT ( 'NONE',  ( -2.458663194297838277E-15, -0.2954942322624074524, -0.1122047244094488277 ) ) ;
#38826 = ADVANCED_FACE ( 'NONE', ( #20742 ), #28042, .T. ) ;
#38828 = CARTESIAN_POINT ( 'NONE',  ( 0.1564216623530369221, -0.006801955215180027596, 0.1403857474672648431 ) ) ;
#38827 = CARTESIAN_POINT ( 'NONE',  ( 0.4755220087074803481, 4.766607801171850497E-17, 0.000000000000000000 ) ) ;
#38829 = CARTESIAN_POINT ( 'NONE',  ( 0.9873396505805591694, -0.1113553986120547346, 0.07381889753026830980 ) ) ;
#38830 = ORIENTED_EDGE ( 'NONE', *, *, #6046, .T. ) ;
#38831 = CARTESIAN_POINT ( 'NONE',  ( -0.9412147342319837628, -0.1574803149606297803, 1.183562992125983593 ) ) ;
#38832 = CARTESIAN_POINT ( 'NONE',  ( 0.1787899950787401604, -0.6525590550643474153, -0.07405724077823318263 ) ) ;
#38833 = CARTESIAN_POINT ( 'NONE',  ( -1.094772975963752103E-17, -1.467027559001354398, -0.1787899950787401882 ) ) ;
#38834 = CARTESIAN_POINT ( 'NONE',  ( -0.7495606340400177148, 0.1264236179284866091, 1.966043307032850462 ) ) ;
#38835 = ORIENTED_EDGE ( 'NONE', *, *, #11792, .T. ) ;
#38836 = CARTESIAN_POINT ( 'NONE',  ( -0.7495606340400177148, -0.1264236179284866091, 1.429625984198204858 ) ) ;
#38837 = EDGE_CURVE ( 'NONE', #36464, #28863, #43706, .T. ) ;
#38838 = CARTESIAN_POINT ( 'NONE',  ( 0.7495606340400177148, -0.1264236179284866091, 1.390255905458047447 ) ) ;
#38839 = DIRECTION ( 'NONE',  ( 0.000000000000000000, 1.000000000000000000, 0.000000000000000000 ) ) ;
#38840 = CARTESIAN_POINT ( 'NONE',  ( -0.6971942568897637749, 2.189545951927499583E-17, 0.6373031495525354195 ) ) ;
#38841 = CARTESIAN_POINT ( 'NONE',  ( 0.1391909071597861591, -0.09842519806770759494, -0.1123953384983699400 ) ) ;
#38842 = CARTESIAN_POINT ( 'NONE',  ( 0.9500414927467377701, -0.1787899950787401604, 0.6496062991588353874 ) ) ;
#38843 = CARTESIAN_POINT ( 'NONE',  ( -0.9500414927467377701, 0.1787899950787401604, 0.5807086613635594752 ) ) ;
#38844 = CARTESIAN_POINT ( 'NONE',  ( 0.1628039705523879055, -0.09131796649104584329, 0.1914378685689082094 ) ) ;
#38845 = ( BOUNDED_CURVE ( )  B_SPLINE_CURVE ( 2, ( #20545, #10492, #13591, #46887, #24165, #10007, #28004, #13833, #3275 ),
 .UNSPECIFIED., .F., .F. ) 
 B_SPLINE_CURVE_WITH_KNOTS ( ( 3, 2, 2, 2, 3 ),
 ( 0.4799999999999999822, 0.4824999999999999845, 0.4849999999999999867, 0.4874999999999999889, 0.4899999999999999911 ),
 .UNSPECIFIED. ) 
 CURVE ( )  GEOMETRIC_REPRESENTATION_ITEM ( )  RATIONAL_B_SPLINE_CURVE ( ( 1.000000000000000000, 0.9238795325112869605, 1.000000000000000000, 0.9238795325112869605, 1.000000000000000000, 0.9238795325112869605, 1.000000000000000000, 0.9238795325112869605, 1.000000000000000000 ) ) 
 REPRESENTATION_ITEM ( '' )  ) ;
#38846 = ADVANCED_FACE ( 'NONE', ( #12647 ), #38953, .T. ) ;
#38847 = CYLINDRICAL_SURFACE ( 'NONE', #29102, 0.09842519685039370636 ) ;
#38848 = VERTEX_POINT ( 'NONE', #38733 ) ;
#38849 = ORIENTED_EDGE ( 'NONE', *, *, #32209, .F. ) ;
#38850 = CARTESIAN_POINT ( 'NONE',  ( -0.9873396505805591694, -0.1113553986120547346, 0.4773622047244094890 ) ) ;
#38851 = CARTESIAN_POINT ( 'NONE',  ( 1.054774247047244540, -0.07405724077823318263, 1.245078740103716886 ) ) ;
#38852 = CARTESIAN_POINT ( 'NONE',  ( 0.2058001524074047073, -0.09851384666201024043, -0.01602185461346814985 ) ) ;
#38853 = ORIENTED_EDGE ( 'NONE', *, *, #44187, .F. ) ;
#38854 = CARTESIAN_POINT ( 'NONE',  ( -0.7185039370078739607, 1.928577636452523993E-17, 0.9251968502861732668 ) ) ;
#38855 = CARTESIAN_POINT ( 'NONE',  ( -0.8759842519685039353, 0.1787899950787401882, 0.9817913385289134265 ) ) ;
#38856 = ADVANCED_FACE ( 'NONE', ( #2291 ), #38256, .T. ) ;
#38857 = VECTOR ( 'NONE', #5108, 39.37007874015748143 ) ;
#38858 = ORIENTED_EDGE ( 'NONE', *, *, #25159, .F. ) ;
#38859 = CARTESIAN_POINT ( 'NONE',  ( 0.1264236179284866091, -0.6451771653005667906, -0.1264236179284866091 ) ) ;
#38860 = DIRECTION ( 'NONE',  ( 1.000000000000000000, 0.000000000000000000, -1.822029033848725275E-16 ) ) ;
#38861 = VERTEX_POINT ( 'NONE', #31797 ) ;
#38862 = DIRECTION ( 'NONE',  ( 1.822029033848725028E-16, 0.000000000000000000, 1.000000000000000000 ) ) ;
#38863 = VECTOR ( 'NONE', #25672, 39.37007874015748143 ) ;
#38864 = ( BOUNDED_CURVE ( )  B_SPLINE_CURVE ( 2, ( #20893, #13925, #28569, #17986, #2876, #17512, #7209, #17756, #6482 ),
 .UNSPECIFIED., .F., .T. ) 
 B_SPLINE_CURVE_WITH_KNOTS ( ( 3, 2, 2, 2, 3 ),
 ( 0.5200000000000000178, 0.5224999999999999645, 0.5250000000000000222, 0.5274999999999999689, 0.5300000000000000266 ),
 .UNSPECIFIED. ) 
 CURVE ( )  GEOMETRIC_REPRESENTATION_ITEM ( )  RATIONAL_B_SPLINE_CURVE ( ( 1.000000000000000000, 0.9238795325112869605, 1.000000000000000000, 0.9238795325112869605, 1.000000000000000000, 0.9238795325112869605, 1.000000000000000000, 0.9238795325112869605, 1.000000000000000000 ) ) 
 REPRESENTATION_ITEM ( '' )  ) ;
#38865 = CARTESIAN_POINT ( 'NONE',  ( -0.07405724077823318263, -0.7165354330171036512, -0.1787899950787401604 ) ) ;
#38866 = CARTESIAN_POINT ( 'NONE',  ( -0.2471922904502826812, -0.09842519685039370636, 5.914624404477007554E-17 ) ) ;
#38867 = DIRECTION ( 'NONE',  ( -0.000000000000000000, -0.000000000000000000, -1.000000000000000000 ) ) ;
#38868 = CARTESIAN_POINT ( 'NONE',  ( -0.1787899950787401604, 0.02054532310934393743, -0.07405724077823318263 ) ) ;
#38869 = CARTESIAN_POINT ( 'NONE',  ( -0.1787899950787401882, 0.03395669296714932950, 0.000000000000000000 ) ) ;
#38870 = APPLICATION_PROTOCOL_DEFINITION ( 'draft international standard', 'automotive_design', 1998, #1504 ) ;
#38871 = DIRECTION ( 'NONE',  ( 0.7986355100472960489, 0.000000000000000000, -0.6018150231520441595 ) ) ;
#38872 = CARTESIAN_POINT ( 'NONE',  ( 1.054774247047244540, -0.07405724077823318263, 0.4527559054580477249 ) ) ;
#38873 = CARTESIAN_POINT ( 'NONE',  ( -0.7495606340400177148, -0.1264236179284866091, 0.7997047243556849594 ) ) ;
#38875 = DIRECTION ( 'NONE',  ( -1.000000000000000000, 0.000000000000000000, 0.000000000000000000 ) ) ;
#38874 = CARTESIAN_POINT ( 'NONE',  ( 0.1574803149606300301, -0.9109251968503938590, -0.06523048226347956391 ) ) ;
#38877 = CARTESIAN_POINT ( 'NONE',  ( -0.7243157012892635915, -0.07330675423201983565, 1.984682877753522590 ) ) ;
#38876 = CARTESIAN_POINT ( 'NONE',  ( -0.1797182628040039087, -1.534000502496431606, 0.07444174185955065859 ) ) ;
#38878 = CARTESIAN_POINT ( 'NONE',  ( 3.284318927891251994E-17, -0.3449803149068665364, 0.1787899950787401882 ) ) ;
#38879 = CARTESIAN_POINT ( 'NONE',  ( 0.7495606340400177148, -0.1264236179284866091, 1.508366141678519678 ) ) ;
#38881 = CARTESIAN_POINT ( 'NONE',  ( 0.2559055118110236116, 0.1477471161312045311, -0.2921040715117803055 ) ) ;
#38880 = CARTESIAN_POINT ( 'NONE',  ( 0.6971942568897648851, 0.07405724077823318263, 1.929133858213952557 ) ) ;
#38882 = CARTESIAN_POINT ( 'NONE',  ( 0.6971942568897648851, -0.07405724077823297447, 0.4379921259304883074 ) ) ;
#38883 = ORIENTED_EDGE ( 'NONE', *, *, #15099, .F. ) ;
#38886 = ORIENTED_EDGE ( 'NONE', *, *, #23605, .T. ) ;
#38885 = EDGE_CURVE ( 'NONE', #30632, #5872, #46336, .T. ) ;
#38884 = CARTESIAN_POINT ( 'NONE',  ( -0.1628039705528179781, -0.09131796649085367756, -0.1914378685686898007 ) ) ;
#38887 = DIRECTION ( 'NONE',  ( 0.000000000000000000, 0.000000000000000000, 1.000000000000000000 ) ) ;
#38888 = CARTESIAN_POINT ( 'NONE',  ( 0.1977610074737742307, -0.1813162243849978650, -0.3078067560680141090 ) ) ;
#38890 = CARTESIAN_POINT ( 'NONE',  ( 0.1787899950787401604, -0.1013779527021420185, -0.07405724077823318263 ) ) ;
#38889 = CARTESIAN_POINT ( 'NONE',  ( -0.06523048226347956391, -0.8764763778452294707, 0.1574803149606297803 ) ) ;
#38891 = CARTESIAN_POINT ( 'NONE',  ( 1.054774247047244540, 0.07405724077823318263, 0.4183070865604097133 ) ) ;
#38892 = CARTESIAN_POINT ( 'NONE',  ( 3.284318927891251994E-17, -0.9749015747493857686, 0.1787899950787401882 ) ) ;
#38893 = DIRECTION ( 'NONE',  ( 0.000000000000000000, 0.000000000000000000, -1.000000000000000000 ) ) ;
#38894 = DIRECTION ( 'NONE',  ( -1.000000000000000000, 0.000000000000000000, 0.000000000000000000 ) ) ;
#38895 = AXIS2_PLACEMENT_3D ( 'NONE', #27556, #45707, #41869 ) ;
#38896 = CARTESIAN_POINT ( 'NONE',  ( -1.054774247047244096, 0.000000000000000000, 1.478838582623401399 ) ) ;
#38897 = VERTEX_POINT ( 'NONE', #13792 ) ;
#38898 = DIRECTION ( 'NONE',  ( 1.000000000000000000, 0.000000000000000000, -1.822029033848725275E-16 ) ) ;
#38899 = ADVANCED_FACE ( 'NONE', ( #14038 ), #28924, .T. ) ;
#38900 = CARTESIAN_POINT ( 'NONE',  ( 0.9500414927467378812, 0.1787899950787401604, 0.9793307086076531442 ) ) ;
#38901 = CARTESIAN_POINT ( 'NONE',  ( 0.07405724077823318263, -1.356299212544662014, -0.1787899950787401604 ) ) ;
#38902 = CARTESIAN_POINT ( 'NONE',  ( -1.033464566929134687, 0.06523048226347956391, 0.5930118109160945616 ) ) ;
#38903 = CARTESIAN_POINT ( 'NONE',  ( 0.9500414927467378812, -0.1787899950787401604, 1.707677165300566235 ) ) ;
#38904 = CARTESIAN_POINT ( 'NONE',  ( -0.8107537697050253289, -0.1574803149606297803, 1.414862204724410377 ) ) ;
#38905 = CARTESIAN_POINT ( 'NONE',  ( -0.6971942568897637749, 2.189545951927499583E-17, 0.8292322834108031282 ) ) ;
#38906 = CARTESIAN_POINT ( 'NONE',  ( 0.000000000000000000, 0.1591122789105269553, 0.000000000000000000 ) ) ;
#38907 = DIRECTION ( 'NONE',  ( -0.000000000000000000, -1.000000000000000000, -0.000000000000000000 ) ) ;
#38908 = CARTESIAN_POINT ( 'NONE',  ( 0.8759842519685039353, -0.1787899950787401882, 0.09596456687537047170 ) ) ;
#38909 = CARTESIAN_POINT ( 'NONE',  ( 0.7646288533564489232, 0.1113553986120547346, 1.471456692805858113 ) ) ;
#38910 = ORIENTED_EDGE ( 'NONE', *, *, #6572, .F. ) ;
#38911 = AXIS2_PLACEMENT_3D ( 'NONE', #16545, #38103, #19410 ) ;
#38912 = CARTESIAN_POINT ( 'NONE',  ( 0.5839895013123354017, 4.616380251121755931E-17, 0.000000000000000000 ) ) ;
#38913 = CARTESIAN_POINT ( 'NONE',  ( -0.9500414927467377701, 0.1787899950787401604, 1.722440944828126153 ) ) ;
#38914 = ORIENTED_EDGE ( 'NONE', *, *, #36498, .T. ) ;
#38915 = CARTESIAN_POINT ( 'NONE',  ( 0.1574803149606299191, 0.000000000000000000, -0.07924015748031493223 ) ) ;
#38916 = DIRECTION ( 'NONE',  ( -5.934354299241488461E-32, -1.000000000000000000, -8.673617379884034486E-16 ) ) ;
#38917 = CARTESIAN_POINT ( 'NONE',  ( -0.1787899950787401604, -1.076895621772545830, 0.07405724077823318263 ) ) ;
#38918 = ORIENTED_EDGE ( 'NONE', *, *, #3841, .T. ) ;
#38919 = CARTESIAN_POINT ( 'NONE',  ( 0.07405724077823318263, -0.1456692912848192578, 0.1787899950787401604 ) ) ;
#38920 = ORIENTED_EDGE ( 'NONE', *, *, #39785, .T. ) ;
#38921 = ORIENTED_EDGE ( 'NONE', *, *, #36582, .T. ) ;
#38922 = CARTESIAN_POINT ( 'NONE',  ( -0.2559066715754571564, -0.04966882545208399502, -0.3122129920274815951 ) ) ;
#38923 = CARTESIAN_POINT ( 'NONE',  ( -0.7185039370078739607, 1.928577636452523993E-17, 0.4133858266641259882 ) ) ;
#38924 = AXIS2_PLACEMENT_3D ( 'NONE', #612, #18843, #15043 ) ;
#38925 = CARTESIAN_POINT ( 'NONE',  ( 0.7646288533564489232, 0.1113553986120547346, 1.756889763779527547 ) ) ;
#38926 = CONICAL_SURFACE ( 'NONE', #47366, 0.08090551181102362266, 0.9599310885968742602 ) ;
#38927 = CARTESIAN_POINT ( 'NONE',  ( -0.1797182628040039087, -0.2397091639137541308, -0.07444174185955065859 ) ) ;
#38928 = CARTESIAN_POINT ( 'NONE',  ( 0.1787899950787401604, -0.7755905511273385455, 0.07405724077823318263 ) ) ;
#38929 = CARTESIAN_POINT ( 'NONE',  ( -0.7495606340400177148, -0.1264236179284866091, 0.4060039369541102450 ) ) ;
#38930 = CARTESIAN_POINT ( 'NONE',  ( -0.7185039370078746268, 0.06523048226347956391, 1.050688976377951889 ) ) ;
#38931 = CARTESIAN_POINT ( 'NONE',  ( 0.07444174185955046430, -1.233803652102731352, -0.1797182628040039087 ) ) ;
#38932 = CARTESIAN_POINT ( 'NONE',  ( -0.7185039370078739607, 1.928577636452523993E-17, 0.2263779527559055260 ) ) ;
#38933 = CARTESIAN_POINT ( 'NONE',  ( 0.8019270111902717657, 0.1787899950787401604, 1.023622047190330342 ) ) ;
#38934 = CARTESIAN_POINT ( 'NONE',  ( 0.7495606340400177148, -0.1264236179284866091, 1.503444881836000002 ) ) ;
#38935 = CARTESIAN_POINT ( 'NONE',  ( 0.9500414927467377701, 0.1787899950787401604, 0.2263779527021421711 ) ) ;
#38937 = EDGE_CURVE ( 'NONE', #11894, #29244, #26128, .T. ) ;
#38936 = DIRECTION ( 'NONE',  ( -1.000000000000000000, 0.000000000000000000, 0.000000000000000000 ) ) ;
#38939 = FACE_OUTER_BOUND ( 'NONE', #32158, .T. ) ;
#38938 = CARTESIAN_POINT ( 'NONE',  ( 0.7646288533564489232, -0.1113553986120547346, 1.412401574803149540 ) ) ;
#38940 = DIRECTION ( 'NONE',  ( -1.000000000000000000, 0.000000000000000000, 0.000000000000000000 ) ) ;
#38941 = CARTESIAN_POINT ( 'NONE',  ( -0.1787899950787401604, -0.002952755851748307785, -0.07405724077823318263 ) ) ;
#38942 = ADVANCED_FACE ( 'NONE', ( #3234 ), #10453, .F. ) ;
#38943 = CARTESIAN_POINT ( 'NONE',  ( 0.9500414927467377701, -0.1787899950787401604, 1.195866141678520345 ) ) ;
#38944 = CARTESIAN_POINT ( 'NONE',  ( 1.054774247047244540, 0.07405724077823318263, 1.919291338528913649 ) ) ;
#38945 = CARTESIAN_POINT ( 'NONE',  ( 0.8107537697050253289, -0.1574803149606297803, 0.3813976376877488139 ) ) ;
#38946 = ORIENTED_EDGE ( 'NONE', *, *, #34372, .F. ) ;
#38947 = CARTESIAN_POINT ( 'NONE',  ( 1.229559056033039366E-16, -0.0009842519685041700977, 0.3937007874015748254 ) ) ;
#38948 = EDGE_CURVE ( 'NONE', #43205, #44478, #45977, .T. ) ;
#38949 = CARTESIAN_POINT ( 'NONE',  ( -0.7646288533564489232, 0.1113553986120547346, 0.2116141731208196763 ) ) ;
#38950 = ORIENTED_EDGE ( 'NONE', *, *, #46512, .T. ) ;
#38951 = CARTESIAN_POINT ( 'NONE',  ( 0.6971942568897648851, 0.07405724077823318263, 1.299212598371432215 ) ) ;
#38952 = EDGE_CURVE ( 'NONE', #18622, #20854, #32583, .T. ) ;
#38954 = CARTESIAN_POINT ( 'NONE',  ( -0.7185039370078746268, 0.06523048226347956391, 0.2928149605223942520 ) ) ;
#38953 = CYLINDRICAL_SURFACE ( 'NONE', #19551, 0.1574803149606300579 ) ;
#38955 = CARTESIAN_POINT ( 'NONE',  ( -0.1787899950787401604, -0.08169291333206318839, -0.07405724077823318263 ) ) ;
#38956 = CARTESIAN_POINT ( 'NONE',  ( -0.9412147342319837628, 0.1574803149606300301, 1.867618110236221707 ) ) ;
#38957 = CIRCLE ( 'NONE', #20593, 0.1377952755905511861 ) ;
#38958 = CARTESIAN_POINT ( 'NONE',  ( 0.8759842519685039353, -0.1574803149606299191, 1.289370078632629868 ) ) ;
#38959 = CARTESIAN_POINT ( 'NONE',  ( -0.7646288533564489232, 0.1113553986120547346, 0.2116141731208196763 ) ) ;
#38960 = ORIENTED_EDGE ( 'NONE', *, *, #30443, .T. ) ;
#38961 = CARTESIAN_POINT ( 'NONE',  ( -0.8759842519685039353, 0.1787899950787401882, 1.331200787347811110 ) ) ;
#38962 = CARTESIAN_POINT ( 'NONE',  ( 0.07405724077823318263, -1.725393700733637958, 0.1787899950787401604 ) ) ;
#38963 = CARTESIAN_POINT ( 'NONE',  ( -1.054774247047244096, 0.000000000000000000, 0.9719488188438739629 ) ) ;
#38964 = CARTESIAN_POINT ( 'NONE',  ( -0.7646288533564489232, 0.1113553986120547346, 0.02460629921259842659 ) ) ;
#38965 = ORIENTED_EDGE ( 'NONE', *, *, #23313, .F. ) ;
#38966 = CARTESIAN_POINT ( 'NONE',  ( -0.8019270111902716547, -0.1787899950787401604, 0.9940944881352130613 ) ) ;
#38967 = VECTOR ( 'NONE', #38916, 39.37007874015748143 ) ;
#38968 = CARTESIAN_POINT ( 'NONE',  ( -0.6971942568897626646, 0.07405724077823318263, 0.6348425196312760255 ) ) ;
#38969 = CARTESIAN_POINT ( 'NONE',  ( -1.033464566929133799, 0.000000000000000000, 0.07874015737278799998 ) ) ;
#38970 = EDGE_LOOP ( 'NONE', ( #8630, #23442, #32356, #14236 ) ) ;
#38971 = CARTESIAN_POINT ( 'NONE',  ( -0.009204872250209487905, -0.08956057363312637520, -0.1860142604523574716 ) ) ;
#38972 = CONICAL_SURFACE ( 'NONE', #20606, 0.1574803149606299191, 0.9599310885968735940 ) ;
#38973 = CARTESIAN_POINT ( 'NONE',  ( 0.7185039370078739607, 1.928577636452523993E-17, 0.6594488188976378451 ) ) ;
#38974 = ORIENTED_EDGE ( 'NONE', *, *, #43046, .T. ) ;
#38975 = CARTESIAN_POINT ( 'NONE',  ( 0.000000000000000000, 0.000000000000000000, 0.09842519685039370636 ) ) ;
#38976 = CARTESIAN_POINT ( 'NONE',  ( -0.8107537697050254399, -0.1574803149606297803, 1.759350393593260842 ) ) ;
#38977 = CARTESIAN_POINT ( 'NONE',  ( -1.002407869896990045, 0.1264236179284866091, 0.6963582676627716461 ) ) ;
#38978 = ( BOUNDED_CURVE ( )  B_SPLINE_CURVE ( 2, ( #2200, #27880, #13939, #2887, #24491, #35525, #17528, #46992, #28583 ),
 .UNSPECIFIED., .F., .T. ) 
 B_SPLINE_CURVE_WITH_KNOTS ( ( 3, 2, 2, 2, 3 ),
 ( 0.1900000000000000022, 0.1925000000000000044, 0.1950000000000000067, 0.1975000000000000089, 0.2000000000000000111 ),
 .UNSPECIFIED. ) 
 CURVE ( )  GEOMETRIC_REPRESENTATION_ITEM ( )  RATIONAL_B_SPLINE_CURVE ( ( 1.000000000000000000, 0.9238795325112869605, 1.000000000000000000, 0.9238795325112869605, 1.000000000000000000, 0.9238795325112869605, 1.000000000000000000, 0.9238795325112869605, 1.000000000000000000 ) ) 
 REPRESENTATION_ITEM ( '' )  ) ;
#38979 = CARTESIAN_POINT ( 'NONE',  ( 0.1476377952755906220, 0.06851622550196635741, -0.1414889043096673460 ) ) ;
#38980 = VERTEX_POINT ( 'NONE', #3487 ) ;
#38981 = CARTESIAN_POINT ( 'NONE',  ( -0.8019270111902716547, -0.1787899950787401604, 1.707677165300568456 ) ) ;
#38982 = CARTESIAN_POINT ( 'NONE',  ( 0.5555748031496089423, 0.3833307086614172743, 0.7480314960629921295 ) ) ;
#38983 = AXIS2_PLACEMENT_3D ( 'NONE', #23748, #35723, #23998 ) ;
#38984 = CARTESIAN_POINT ( 'NONE',  ( -0.7185039370078739607, 1.928577636452523993E-17, 0.5019685039370078705 ) ) ;
#38985 = CARTESIAN_POINT ( 'NONE',  ( 0.9873396505805591694, 0.1113553986120547346, 0.6053149606299212948 ) ) ;
#38986 = CARTESIAN_POINT ( 'NONE',  ( 0.1270800023317771588, -0.6555556206066672775, 0.1270800023317771588 ) ) ;
#38987 = CARTESIAN_POINT ( 'NONE',  ( 0.1574803149606299191, 0.5360961046428496246, -0.7563373642699310340 ) ) ;
#38988 = CARTESIAN_POINT ( 'NONE',  ( -1.033464566929133799, 0.000000000000000000, 1.417322834538141674 ) ) ;
#38990 = CARTESIAN_POINT ( 'NONE',  ( -0.4620708661417322616, 0.4133858267716533086, 1.186023622047243986 ) ) ;
#38989 = CARTESIAN_POINT ( 'NONE',  ( 0.06523048226347956391, -0.5270669291338577755, 0.1574803149606297803 ) ) ;
#38991 = DIRECTION ( 'NONE',  ( 0.000000000000000000, 0.000000000000000000, 1.000000000000000000 ) ) ;
#38992 = VERTEX_POINT ( 'NONE', #32268 ) ;
#38993 = DIRECTION ( 'NONE',  ( -3.469446951953613794E-15, -1.000000000000000000, 0.000000000000000000 ) ) ;
#38994 = CARTESIAN_POINT ( 'NONE',  ( 0.9873396505805591694, -0.1113553986120547346, 1.186023622047243986 ) ) ;
#38995 = CARTESIAN_POINT ( 'NONE',  ( 0.1113553986120547346, 0.07578740168233012720, 0.1113553986120547346 ) ) ;
#38997 = CARTESIAN_POINT ( 'NONE',  ( -0.9873396505805591694, -0.1113553986120547346, 1.343503937007874072 ) ) ;
#38996 = CARTESIAN_POINT ( 'NONE',  ( -0.8107537697050254399, 0.1574803149606300301, 1.272145669183810668 ) ) ;
#38998 = CIRCLE ( 'NONE', #27555, 0.2114570894355444486 ) ;
#38999 = CARTESIAN_POINT ( 'NONE',  ( 0.8759842519685039353, -0.1574803149606299191, 1.732283464566929165 ) ) ;
#39000 = ADVANCED_FACE ( 'NONE', ( #36560 ), #3721, .T. ) ;
#39002 = CARTESIAN_POINT ( 'NONE',  ( 0.8759842519685039353, -0.1574803149606299191, 1.683070866034204638 ) ) ;
#39001 = CARTESIAN_POINT ( 'NONE',  ( 1.033464566929133799, 0.000000000000000000, 0.5905511809948347235 ) ) ;
#39003 = LINE ( 'NONE', #32561, #27783 ) ;
#39004 = DIRECTION ( 'NONE',  ( 2.943801717310650128E-16, -1.000000000000000000, -2.355041373848520102E-15 ) ) ;
#39005 = DIRECTION ( 'NONE',  ( -1.000000000000000000, 0.000000000000000000, 0.000000000000000000 ) ) ;
#39006 = ORIENTED_EDGE ( 'NONE', *, *, #35455, .F. ) ;
#39007 = CIRCLE ( 'NONE', #6852, 0.02900000000000001882 ) ;
#39008 = CARTESIAN_POINT ( 'NONE',  ( 0.001132063567019381744, 0.1075630933946142148, -0.08929056810493603280 ) ) ;
#39009 = CARTESIAN_POINT ( 'NONE',  ( 0.7495606340400177148, -0.1264236179284866091, 0.8735236219934803259 ) ) ;
#39010 = EDGE_CURVE ( 'NONE', #32371, #12253, #47167, .T. ) ;
#39011 = ORIENTED_EDGE ( 'NONE', *, *, #25927, .T. ) ;
#39012 = DIRECTION ( 'NONE',  ( -1.000000000000000000, -0.000000000000000000, 0.000000000000000000 ) ) ;
#39013 = DIRECTION ( 'NONE',  ( 0.000000000000000000, 1.000000000000000000, 0.000000000000000000 ) ) ;
#39014 = CARTESIAN_POINT ( 'NONE',  ( 0.1797182628040039365, 0.1367672140390017721, -2.200913952912460540E-17 ) ) ;
#39015 = CARTESIAN_POINT ( 'NONE',  ( 0.07405724077823318263, -1.080708661363559919, -0.1787899950787401604 ) ) ;
#39016 = CARTESIAN_POINT ( 'NONE',  ( 0.1113553986120547346, -1.390748031496063186, 0.1113553986120547346 ) ) ;
#39017 = CARTESIAN_POINT ( 'NONE',  ( 0.1554371429169570662, 0.1056204263327887305, -0.09265060645563602537 ) ) ;
#39018 = CARTESIAN_POINT ( 'NONE',  ( -0.8759842519685039353, -0.1787899950787401882, 1.946358267662771757 ) ) ;
#39019 = CARTESIAN_POINT ( 'NONE',  ( 0.8019270111902717657, 0.1787899950787401604, 1.929133858213952335 ) ) ;
#39020 = ORIENTED_EDGE ( 'NONE', *, *, #46745, .T. ) ;
#39021 = CARTESIAN_POINT ( 'NONE',  ( 0.7646288533564489232, -0.1113553986120547346, 0.5462598425196850682 ) ) ;
#39022 = CARTESIAN_POINT ( 'NONE',  ( -0.9500414927467378812, 0.1787899950787401604, 1.564960629867495845 ) ) ;
#39023 = CYLINDRICAL_SURFACE ( 'NONE', #43472, 0.09842519685039370636 ) ;
#39024 = CARTESIAN_POINT ( 'NONE',  ( -0.8019270111902717657, -0.1787899950787401604, 0.2509842519147403861 ) ) ;
#39025 = CIRCLE ( 'NONE', #19903, 0.02900000000000001882 ) ;
#39026 = CARTESIAN_POINT ( 'NONE',  ( -0.2471922904502826535, 0.09142184925109154980, 0.04493454898959751281 ) ) ;
#39027 = CARTESIAN_POINT ( 'NONE',  ( -0.7495606340400177148, 0.1264236179284866091, 1.931594488135212728 ) ) ;
#39028 = CARTESIAN_POINT ( 'NONE',  ( -0.8759842519685039353, -0.1574803149606299191, 1.929133858267716661 ) ) ;
#39029 = DIRECTION ( 'NONE',  ( 1.822029033848725028E-16, 0.000000000000000000, 1.000000000000000000 ) ) ;
#39030 = CARTESIAN_POINT ( 'NONE',  ( -0.1787899950787401604, -0.2550452280717585563, -0.07405724077823318263 ) ) ;
#39031 = CARTESIAN_POINT ( 'NONE',  ( 0.05862610683640598341, -0.09842519685039370636, 0.2134590741261405689 ) ) ;
#39032 = LINE ( 'NONE', #6440, #21835 ) ;
#39033 = CARTESIAN_POINT ( 'NONE',  ( 0.8759842519685039353, -0.1574803149606299191, 1.053149606191685184 ) ) ;
#39034 = CIRCLE ( 'NONE', #37507, 0.09842519685039370636 ) ;
#39035 = EDGE_CURVE ( 'NONE', #9464, #33977, #449, .T. ) ;
#39036 = VERTEX_POINT ( 'NONE', #20970 ) ;
#39037 = ORIENTED_EDGE ( 'NONE', *, *, #23709, .T. ) ;
#39038 = CARTESIAN_POINT ( 'NONE',  ( -0.07405724077823318263, -1.100393700733639069, 0.1787899950787401604 ) ) ;
#39039 = CARTESIAN_POINT ( 'NONE',  ( -0.1264236179284866091, -1.216043307032850462, 0.1264236179284866091 ) ) ;
#39040 = LINE ( 'NONE', #17475, #6436 ) ;
#39041 = ( CONVERSION_BASED_UNIT ( 'INCH', #25144 ) LENGTH_UNIT ( ) NAMED_UNIT ( #32022 ) ) ;
#39042 = CARTESIAN_POINT ( 'NONE',  ( 0.1270800023317771588, -0.5374453843861952684, 0.1270800023317771588 ) ) ;
#39043 = LINE ( 'NONE', #13889, #20144 ) ;
#39044 = CARTESIAN_POINT ( 'NONE',  ( -0.8759842519685039353, -0.1574803149606299191, 0.8562992124908976876 ) ) ;
#39045 = CARTESIAN_POINT ( 'NONE',  ( -0.8759842519685039353, -0.1574803149606299191, 0.7086614173228346081 ) ) ;
#39046 = CARTESIAN_POINT ( 'NONE',  ( -0.1574803149606297803, -0.02509842519685037687, 0.06523048226347956391 ) ) ;
#39047 = CARTESIAN_POINT ( 'NONE',  ( 1.033464566929134687, 0.06523048226347956391, 0.7603346456692923194 ) ) ;
#39048 = CARTESIAN_POINT ( 'NONE',  ( 2.892866454678787531E-17, -0.05708661417322834220, 0.1574803149606299191 ) ) ;
#39049 = EDGE_CURVE ( 'NONE', #45154, #13201, #44154, .T. ) ;
#39050 = VECTOR ( 'NONE', #7874, 39.37007874015748143 ) ;
#39052 = CARTESIAN_POINT ( 'NONE',  ( 0.1573602050224812976, -0.1080344010929237403, -0.09369282772939586945 ) ) ;
#39051 = CARTESIAN_POINT ( 'NONE',  ( 0.1642836037694651863, 0.2006450494026638109, -0.03472289316813669674 ) ) ;
#39053 = CARTESIAN_POINT ( 'NONE',  ( 0.8107537697050234415, -0.1574803149606297803, 0.1845472439869611236 ) ) ;
#39054 = CIRCLE ( 'NONE', #6146, 0.2204724409448818867 ) ;
#39055 = EDGE_LOOP ( 'NONE', ( #4771, #26516, #9709, #10939, #17938, #31333 ) ) ;
#39056 = CARTESIAN_POINT ( 'NONE',  ( -1.033464566929134687, -0.06523048226347956391, 0.7849409447743629364 ) ) ;
#39057 = DIRECTION ( 'NONE',  ( -1.000000000000000000, 0.000000000000000000, 0.000000000000000000 ) ) ;
#39058 = CARTESIAN_POINT ( 'NONE',  ( -0.1787899950787401882, -0.5172244093950552069, 0.000000000000000000 ) ) ;
#39059 = VECTOR ( 'NONE', #23842, 39.37007874015748854 ) ;
#39060 = CARTESIAN_POINT ( 'NONE',  ( -1.094772975963752103E-17, -1.388287401521039355, -0.1787899950787401882 ) ) ;
#39061 = CARTESIAN_POINT ( 'NONE',  ( -0.8759842519685039353, -0.1787899950787401882, 1.980807086560409491 ) ) ;
#39062 = ORIENTED_EDGE ( 'NONE', *, *, #35571, .T. ) ;
#39063 = CARTESIAN_POINT ( 'NONE',  ( 0.6971942568897648851, -0.07405724077823297447, 1.545275590497416696 ) ) ;
#39064 = CARTESIAN_POINT ( 'NONE',  ( 0.7185039370078739607, 1.928577636452523993E-17, 0.9251968502861732668 ) ) ;
#39065 = CARTESIAN_POINT ( 'NONE',  ( -1.054774247047244540, 0.07405724077823318263, 0.6988188975840318173 ) ) ;
#39066 = CARTESIAN_POINT ( 'NONE',  ( 0.4811709046783464450, 4.466152701071653354E-17, 0.000000000000000000 ) ) ;
#39067 = SURFACE_SIDE_STYLE ('',( #34807 ) ) ;
#39068 = CARTESIAN_POINT ( 'NONE',  ( 1.002407869896990045, 0.1264236179284866091, 0.6225393700249762796 ) ) ;
#39069 = CARTESIAN_POINT ( 'NONE',  ( -1.002407869896990045, 0.1264236179284866091, 0.4995078739619842612 ) ) ;
#39070 = CARTESIAN_POINT ( 'NONE',  ( 0.3604359965418638123, -3.032960542342102697E-32, 0.09842519685039370636 ) ) ;
#39071 = DIRECTION ( 'NONE',  ( 0.000000000000000000, 0.000000000000000000, 1.000000000000000000 ) ) ;
#39072 = EDGE_LOOP ( 'NONE', ( #12361, #39558, #11012, #5908 ) ) ;
#39073 = CARTESIAN_POINT ( 'NONE',  ( -0.9500414927467378812, -0.1787899950787401604, 1.358267716481669662 ) ) ;
#39074 = PLANE ( 'NONE',  #31019 ) ;
#39075 = CARTESIAN_POINT ( 'NONE',  ( -1.033464566929134687, -0.06523048226347956391, 0.4404527559055117503 ) ) ;
#39076 = CARTESIAN_POINT ( 'NONE',  ( 0.8759842519685039353, 0.1787899950787401882, 1.375492125930488196 ) ) ;
#39077 = CARTESIAN_POINT ( 'NONE',  ( -0.02315057879874008254, -0.09851384983704390697, 0.2241609000832641696 ) ) ;
#39078 = ORIENTED_EDGE ( 'NONE', *, *, #17173, .T. ) ;
#39079 = CARTESIAN_POINT ( 'NONE',  ( 0.08946752424252854552, 0.3740157480314960647, 1.224299699984021661 ) ) ;
#39080 = AXIS2_PLACEMENT_3D ( 'NONE', #44698, #8533, #36657 ) ;
#39081 = CARTESIAN_POINT ( 'NONE',  ( -0.1787899950787401882, -1.630537354056009969, 0.000000000000000000 ) ) ;
#39082 = ORIENTED_EDGE ( 'NONE', *, *, #321, .T. ) ;
#39083 = CARTESIAN_POINT ( 'NONE',  ( 0.07405724077823318263, -0.6033464566391496531, -0.1787899950787401604 ) ) ;
#39084 = CYLINDRICAL_SURFACE ( 'NONE', #13202, 0.1574803149606299191 ) ;
#39085 = VERTEX_POINT ( 'NONE', #37495 ) ;
#39086 = CARTESIAN_POINT ( 'NONE',  ( 0.6971942568897637749, 2.189545951927499583E-17, 1.380413385773007873 ) ) ;
#39087 = VECTOR ( 'NONE', #11160, 39.37007874015748143 ) ;
#39088 = AXIS2_PLACEMENT_3D ( 'NONE', #17955, #35711, #203 ) ;
#39089 = CARTESIAN_POINT ( 'NONE',  ( 0.1787899950787401604, -0.3375984251430867999, -0.07405724077823318263 ) ) ;
#39090 = CARTESIAN_POINT ( 'NONE',  ( -0.07405724077823318263, -0.7952755904974174728, -0.1787899950787401604 ) ) ;
#39091 = FACE_OUTER_BOUND ( 'NONE', #46694, .T. ) ;
#39092 = CARTESIAN_POINT ( 'NONE',  ( 0.000000000000000000, -0.09842519685039370636, 0.000000000000000000 ) ) ;
#39093 = CARTESIAN_POINT ( 'NONE',  ( 0.8019270111902717657, -0.1787899950787401604, 0.3248031495525355306 ) ) ;
#39094 = EDGE_CURVE ( 'NONE', #38424, #14831, #19594, .T. ) ;
#39095 = CARTESIAN_POINT ( 'NONE',  ( 0.1264236179284866091, -0.03112790523711275736, -0.1264236179284866091 ) ) ;
#39096 = CARTESIAN_POINT ( 'NONE',  ( 0.07405724077823318263, 0.1003937008411650705, -0.1787899950787401604 ) ) ;
#39097 = DIRECTION ( 'NONE',  ( 1.000000000000000000, 0.000000000000000000, -1.822029033848725275E-16 ) ) ;
#39098 = CARTESIAN_POINT ( 'NONE',  ( 0.8759842519685039353, 0.1787899950787401882, 0.5044291338045039375 ) ) ;
#39099 = CARTESIAN_POINT ( 'NONE',  ( -1.002407869896990045, 0.1264236179284866091, 0.7406496062454487328 ) ) ;
#39100 = EDGE_CURVE ( 'NONE', #19773, #31956, #37973, .T. ) ;
#39102 = CARTESIAN_POINT ( 'NONE',  ( 0.7646288533564489232, 0.1113553986120547346, 1.707677165246803241 ) ) ;
#39101 = CARTESIAN_POINT ( 'NONE',  ( 0.1574803149606300301, -0.9552165354330708347, 0.06523048226347956391 ) ) ;
#39104 = CARTESIAN_POINT ( 'NONE',  ( -0.7981378442724675892, -0.1533582279231914536, 1.986711164195015034 ) ) ;
#39103 = CARTESIAN_POINT ( 'NONE',  ( 3.301370929368692659E-17, -1.762839085173596443, 0.1797182628040039365 ) ) ;
#39105 = CARTESIAN_POINT ( 'NONE',  ( -0.1264236179284866091, -0.3499015747493862127, 0.1264236179284866091 ) ) ;
#39106 = CARTESIAN_POINT ( 'NONE',  ( -0.8107537697050254399, -0.1574803149606297803, 1.247539369971212508 ) ) ;
#39107 = CARTESIAN_POINT ( 'NONE',  ( 0.7495606340400177148, 0.1264236179284866091, 1.695374015694267822 ) ) ;
#39109 = CARTESIAN_POINT ( 'NONE',  ( -0.9412147342319837628, -0.1574803149606297803, 1.813484251968503935 ) ) ;
#39108 = DIRECTION ( 'NONE',  ( 0.000000000000000000, 0.000000000000000000, 1.000000000000000000 ) ) ;
#39110 = CARTESIAN_POINT ( 'NONE',  ( 0.8019270111902716547, -0.1787899950787401604, 0.4429133857730084833 ) ) ;
#39111 = ORIENTED_EDGE ( 'NONE', *, *, #17917, .F. ) ;
#39112 = EDGE_CURVE ( 'NONE', #38468, #5617, #37443, .T. ) ;
#39113 = CARTESIAN_POINT ( 'NONE',  ( -0.6195511811023656223, 0.000000000000000000, -1.186023622047243986 ) ) ;
#39114 = CARTESIAN_POINT ( 'NONE',  ( -0.4338976377952755703, -2.656856766417909227E-17, 0.000000000000000000 ) ) ;
#39115 = CARTESIAN_POINT ( 'NONE',  ( -0.1264236179284866091, -0.07923228341080333637, 0.1264236179284866091 ) ) ;
#39116 = CARTESIAN_POINT ( 'NONE',  ( 0.8759842519685039353, 0.1787899950787401882, 0.6225393700249762796 ) ) ;
#39117 = CARTESIAN_POINT ( 'NONE',  ( 0.07405724077823318263, -0.9970472440407247561, -0.1787899950787401604 ) ) ;
#39118 = DIRECTION ( 'NONE',  ( 0.000000000000000000, 0.000000000000000000, 1.000000000000000000 ) ) ;
#39119 = ( BOUNDED_CURVE ( )  B_SPLINE_CURVE ( 2, ( #12698, #19855, #13602, #28242, #39002, #9075, #45953, #27799, #9791 ),
 .UNSPECIFIED., .F., .T. ) 
 B_SPLINE_CURVE_WITH_KNOTS ( ( 3, 2, 2, 2, 3 ),
 ( 0.8299999999999999600, 0.8325000000000000178, 0.8349999999999999645, 0.8375000000000000222, 0.8399999999999999689 ),
 .UNSPECIFIED. ) 
 CURVE ( )  GEOMETRIC_REPRESENTATION_ITEM ( )  RATIONAL_B_SPLINE_CURVE ( ( 1.000000000000000000, 0.9238795325112939549, 1.000000000000000000, 0.9238795325112869605, 1.000000000000000000, 0.9238795325112869605, 1.000000000000000000, 0.9238795325112869605, 1.000000000000000000 ) ) 
 REPRESENTATION_ITEM ( '' )  ) ;
#39120 = CARTESIAN_POINT ( 'NONE',  ( -0.7646288533564489232, -0.1113553986120547346, 0.9301181101286929431 ) ) ;
#39121 = VECTOR ( 'NONE', #16731, 39.37007874015748143 ) ;
#39122 = ADVANCED_FACE ( 'NONE', ( #33227 ), #13475, .F. ) ;
#39123 = CARTESIAN_POINT ( 'NONE',  ( -1.054774247047244540, -0.07405724077823318263, 1.515748031442299526 ) ) ;
#39124 = ORIENTED_EDGE ( 'NONE', *, *, #37169, .T. ) ;
#39125 = DIRECTION ( 'NONE',  ( 0.000000000000000000, -1.000000000000000000, 0.000000000000000000 ) ) ;
#39126 = CARTESIAN_POINT ( 'NONE',  ( 0.8019270111902717657, -0.1787899950787401604, 1.038385826717890259 ) ) ;
#39127 = AXIS2_PLACEMENT_3D ( 'NONE', #9769, #46639, #24156 ) ;
#39128 = CARTESIAN_POINT ( 'NONE',  ( 0.9500414927467378812, -0.1787899950787401604, 1.747047244040724312 ) ) ;
#39129 = CARTESIAN_POINT ( 'NONE',  ( -0.7646288533564489232, -0.1113553986120547346, 1.333661417322834719 ) ) ;
#39130 = CARTESIAN_POINT ( 'NONE',  ( -1.054774247047244096, 0.000000000000000000, 0.9276574802611967652 ) ) ;
#39131 = CARTESIAN_POINT ( 'NONE',  ( -0.4330708661417344563, 1.502516396515352363E-15, 4.927039740520691743E-17 ) ) ;
#39132 = CARTESIAN_POINT ( 'NONE',  ( -0.8484364047846082446, -0.1575219822776003920, 0.03937007874015843040 ) ) ;
#39133 = CARTESIAN_POINT ( 'NONE',  ( 0.8019270111902716547, -0.1787899950787401604, 0.1722440944344256208 ) ) ;
#39134 = CARTESIAN_POINT ( 'NONE',  ( -0.7495606340400177148, 0.1264236179284866091, 0.07627952750529173875 ) ) ;
#39135 = VECTOR ( 'NONE', #20020, 39.37007874015748143 ) ;
#39136 = CARTESIAN_POINT ( 'NONE',  ( 0.8759842519685039353, 0.1574803149606299191, 1.624015747923968522 ) ) ;
#39137 = ORIENTED_EDGE ( 'NONE', *, *, #35178, .T. ) ;
#39138 = CARTESIAN_POINT ( 'NONE',  ( -1.181102362204724310, -0.3937007874015748254, 0.9842519685039370358 ) ) ;
#39139 = CARTESIAN_POINT ( 'NONE',  ( 1.033464566929133799, 0.000000000000000000, 0.6003937007874016185 ) ) ;
#39140 = ORIENTED_EDGE ( 'NONE', *, *, #11878, .F. ) ;
#39141 = ORIENTED_EDGE ( 'NONE', *, *, #41134, .T. ) ;
#39142 = CARTESIAN_POINT ( 'NONE',  ( -0.6971942568897637749, 2.189545951927499583E-17, 1.656003936954110412 ) ) ;
#39143 = ( BOUNDED_CURVE ( )  B_SPLINE_CURVE ( 2, ( #19755, #45138, #19518, #8733, #8019, #27220, #44425, #1059, #33461 ),
 .UNSPECIFIED., .F., .T. ) 
 B_SPLINE_CURVE_WITH_KNOTS ( ( 3, 2, 2, 2, 3 ),
 ( 0.1600000000000000033, 0.1625000000000000056, 0.1650000000000000078, 0.1675000000000000100, 0.1700000000000000122 ),
 .UNSPECIFIED. ) 
 CURVE ( )  GEOMETRIC_REPRESENTATION_ITEM ( )  RATIONAL_B_SPLINE_CURVE ( ( 1.000000000000000000, 0.9238795325112869605, 1.000000000000000000, 0.9238795325112869605, 1.000000000000000000, 0.9238795325112869605, 1.000000000000000000, 0.9238795325112879597, 1.000000000000000000 ) ) 
 REPRESENTATION_ITEM ( '' )  ) ;
#39144 = DIRECTION ( 'NONE',  ( 0.000000000000000000, 0.000000000000000000, 1.000000000000000000 ) ) ;
#39145 = CARTESIAN_POINT ( 'NONE',  ( -0.7646288533564489232, -0.1113553986120547346, 0.7824803149606299746 ) ) ;
#39146 = CARTESIAN_POINT ( 'NONE',  ( 0.1264236179284866091, -1.103962550906403495, 0.1264236179284866091 ) ) ;
#39147 = EDGE_LOOP ( 'NONE', ( #32876, #38063, #751, #38753 ) ) ;
#39148 = CARTESIAN_POINT ( 'NONE',  ( 0.1264236179284866091, -0.05462598419820496182, -0.1264236179284866091 ) ) ;
#39149 = VERTEX_POINT ( 'NONE', #809 ) ;
#39150 = ORIENTED_EDGE ( 'NONE', *, *, #22221, .T. ) ;
#39151 = CARTESIAN_POINT ( 'NONE',  ( 0.8759842519685039353, 0.1787899950787401882, 1.055610236166708793 ) ) ;
#39152 = EDGE_CURVE ( 'NONE', #16719, #2, #34165, .T. ) ;
#39153 = FACE_OUTER_BOUND ( 'NONE', #26343, .T. ) ;
#39154 = CARTESIAN_POINT ( 'NONE',  ( -1.033464566929133799, 0.000000000000000000, 0.9940944881889764995 ) ) ;
#39155 = AXIS2_PLACEMENT_3D ( 'NONE', #42366, #39005, #20794 ) ;
#39156 = EDGE_CURVE ( 'NONE', #40494, #20918, #34657, .T. ) ;
#39157 = CARTESIAN_POINT ( 'NONE',  ( 0.9873396505805591694, 0.1113553986120547346, 1.865157480314960647 ) ) ;
#39158 = EDGE_CURVE ( 'NONE', #35410, #35946, #13521, .T. ) ;
#39159 = CARTESIAN_POINT ( 'NONE',  ( 0.07405724077823318263, -0.7263779527021420046, -0.1787899950787401604 ) ) ;
#39160 = CARTESIAN_POINT ( 'NONE',  ( -0.8019270111902716547, -0.1787899950787401604, 0.3690944881352128393 ) ) ;
#39161 = DIRECTION ( 'NONE',  ( 0.000000000000000000, 0.000000000000000000, 1.000000000000000000 ) ) ;
#39162 = CARTESIAN_POINT ( 'NONE',  ( 0.8019270111902717657, -0.1787899950787401604, 1.117125984198206412 ) ) ;
#39163 = CARTESIAN_POINT ( 'NONE',  ( 1.002407869896990045, -0.1264236179284866091, 1.592027559001354398 ) ) ;
#39164 = CARTESIAN_POINT ( 'NONE',  ( 0.8759842519685039353, 0.1787899950787401882, 0.1894685038832444879 ) ) ;
#39165 = CARTESIAN_POINT ( 'NONE',  ( 0.1574803149606299191, 1.928577636452524918E-17, -0.2357204724409448504 ) ) ;
#39166 = CARTESIAN_POINT ( 'NONE',  ( 1.033464566929133799, 0.000000000000000000, 1.702755905511810885 ) ) ;
#39168 = CARTESIAN_POINT ( 'NONE',  ( -0.8107537697050254399, -0.1574803149606297803, 1.099901574803150650 ) ) ;
#39167 = CARTESIAN_POINT ( 'NONE',  ( 0.7623055800743335775, 0.1150132697384864122, 1.980789724883672998 ) ) ;
#39169 = CARTESIAN_POINT ( 'NONE',  ( 0.06801279071811515420, -0.09842519685039327615, 1.224299699984020107 ) ) ;
#39170 = CARTESIAN_POINT ( 'NONE',  ( -0.7646288533564489232, -0.1113553986120547346, 1.756889763671999782 ) ) ;
#39171 = CARTESIAN_POINT ( 'NONE',  ( 0.8759842519685039353, -0.1787899950787401882, 0.1697834645131655606 ) ) ;
#39172 = DIRECTION ( 'NONE',  ( -4.357234436330879339E-15, 0.9771240687918565371, 0.2126700594527759225 ) ) ;
#39174 = CARTESIAN_POINT ( 'NONE',  ( -0.8759842519685039353, 0.1574803149606299191, 1.820866141624755796 ) ) ;
#39173 = CARTESIAN_POINT ( 'NONE',  ( 1.002407869896990045, -0.1264236179284866091, 1.119586614119464585 ) ) ;
#39175 = CARTESIAN_POINT ( 'NONE',  ( 0.6971942568897648851, 0.07405724077823318263, 1.934055118056471567 ) ) ;
#39176 = CARTESIAN_POINT ( 'NONE',  ( 0.8107537697050253289, -0.1574803149606297803, 0.4207677164279059467 ) ) ;
#39177 = ORIENTED_EDGE ( 'NONE', *, *, #42560, .F. ) ;
#39178 = SURFACE_STYLE_FILL_AREA ( #24811 ) ;
#39179 = CARTESIAN_POINT ( 'NONE',  ( -0.7646288533564489232, 0.1113553986120547346, 0.3297244093412917687 ) ) ;
#39180 = CARTESIAN_POINT ( 'NONE',  ( -0.7185039370078746268, -0.06523048226347956391, 1.528051181102361378 ) ) ;
#39181 = CARTESIAN_POINT ( 'NONE',  ( 0.6971942568897648851, 0.07405724077823318263, 1.338582677111590069 ) ) ;
#39183 = CARTESIAN_POINT ( 'NONE',  ( 1.033464566929133799, 0.000000000000000000, 0.07874015737278799998 ) ) ;
#39182 = DIRECTION ( 'NONE',  ( 1.000000000000000000, -0.000000000000000000, -1.144917494144692682E-16 ) ) ;
#39184 = CARTESIAN_POINT ( 'NONE',  ( 0.1264236179284866091, -0.01525590545804753929, -0.1264236179284866091 ) ) ;
#39185 = DIRECTION ( 'NONE',  ( 0.000000000000000000, 0.000000000000000000, 1.000000000000000000 ) ) ;
#39186 = CIRCLE ( 'NONE', #36173, 0.1013779527559055538 ) ;
#39187 = CARTESIAN_POINT ( 'NONE',  ( 0.8759842519685039353, -0.1574803149606299191, 0.5118110236220472231 ) ) ;
#39188 = ORIENTED_EDGE ( 'NONE', *, *, #40888, .T. ) ;
#39189 = ORIENTED_EDGE ( 'NONE', *, *, #9150, .T. ) ;
#39190 = CARTESIAN_POINT ( 'NONE',  ( -0.9500414927467377701, -0.1787899950787401604, 1.392716535379308285 ) ) ;
#39191 = CARTESIAN_POINT ( 'NONE',  ( 0.07405724077823318263, -1.686023621993479882, 0.1787899950787401604 ) ) ;
#39192 = CARTESIAN_POINT ( 'NONE',  ( -0.9500414927467378812, 0.1787899950787401604, 1.018700787347811110 ) ) ;
#39193 = CONICAL_SURFACE ( 'NONE', #5543, 0.08090551181102362266, 0.9599310885968742602 ) ;
#39194 = CIRCLE ( 'NONE', #18541, 0.1377952755905511861 ) ;
#39195 = CARTESIAN_POINT ( 'NONE',  ( -1.033464566929134687, 0.06523048226347956391, 0.05167322834645668439 ) ) ;
#39196 = CARTESIAN_POINT ( 'NONE',  ( -0.6971942568897637749, 2.189545951927499583E-17, 1.144192913332062966 ) ) ;
#39197 = CARTESIAN_POINT ( 'NONE',  ( -0.8759842519685039353, -0.1787899950787401882, 0.6865157479777322935 ) ) ;
#39198 = CARTESIAN_POINT ( 'NONE',  ( -0.7185039370078746268, -0.06523048226347956391, 0.3469488188976379561 ) ) ;
#39199 = CARTESIAN_POINT ( 'NONE',  ( 0.000000000000000000, 0.000000000000000000, -0.3149606299212598381 ) ) ;
#39200 = CARTESIAN_POINT ( 'NONE',  ( 0.1264236179284866091, -0.6610491650796320728, -0.1264236179284866091 ) ) ;
#39201 = ORIENTED_EDGE ( 'NONE', *, *, #11110, .T. ) ;
#39202 = CARTESIAN_POINT ( 'NONE',  ( -0.1663756747267724490, -0.08956132504751300460, 0.02463664667560858459 ) ) ;
#39203 = ORIENTED_EDGE ( 'NONE', *, *, #29606, .F. ) ;
#39204 = DIRECTION ( 'NONE',  ( 0.000000000000000000, 0.000000000000000000, -1.000000000000000000 ) ) ;
#39205 = ADVANCED_FACE ( 'NONE', ( #31273 ), #34625, .F. ) ;
#39206 = CARTESIAN_POINT ( 'NONE',  ( -0.7185039370078739607, 1.928577636452523993E-17, 0.5708661416247566844 ) ) ;
#39207 = CARTESIAN_POINT ( 'NONE',  ( -0.9500414927467378812, 0.1787899950787401604, 0.5807086613635594752 ) ) ;
#39208 = CARTESIAN_POINT ( 'NONE',  ( 0.1113553986120547346, -0.002952755905511810983, -0.1113553986120547346 ) ) ;
#39209 = ADVANCED_FACE ( 'NONE', ( #5612 ), #13059, .T. ) ;
#39210 = ORIENTED_EDGE ( 'NONE', *, *, #46636, .T. ) ;
#39211 = EDGE_CURVE ( 'NONE', #38222, #27881, #34666, .T. ) ;
#39212 = CARTESIAN_POINT ( 'NONE',  ( -0.9500414927467377701, -0.1787899950787401604, 1.594488188922615457 ) ) ;
#39213 = ADVANCED_FACE ( 'NONE', ( #45609 ), #27696, .T. ) ;
#39214 = DIRECTION ( 'NONE',  ( 0.000000000000000000, 1.000000000000000000, 8.673617379884034486E-16 ) ) ;
#39215 = VECTOR ( 'NONE', #49, 39.37007874015748143 ) ;
#39216 = CARTESIAN_POINT ( 'NONE',  ( -0.9412147342319837628, 0.1574803149606300301, 0.1254921258767249526 ) ) ;
#39217 = ORIENTED_EDGE ( 'NONE', *, *, #29768, .F. ) ;
#39218 = CARTESIAN_POINT ( 'NONE',  ( 0.7185039370078739607, 1.928577636452523993E-17, 0.5413385826771653919 ) ) ;
#39219 = CARTESIAN_POINT ( 'NONE',  ( 0.07444174185955065859, -0.7761264867484009011, 0.1797182628040039087 ) ) ;
#39220 = CARTESIAN_POINT ( 'NONE',  ( 0.2471922904502826812, 0.07821434602336012343, 0.07684457919973788909 ) ) ;
#39221 = CARTESIAN_POINT ( 'NONE',  ( -1.033464566929134687, 0.06523048226347956391, 1.419783464459402289 ) ) ;
#39222 = CARTESIAN_POINT ( 'NONE',  ( 0.6971942568897637749, 2.189545951927499583E-17, 0.6766732282926929409 ) ) ;
#39223 = CARTESIAN_POINT ( 'NONE',  ( -0.06523048226347956391, -0.6500984251968493499, 0.1574803149606297803 ) ) ;
#39224 = ( GEOMETRIC_REPRESENTATION_CONTEXT ( 3 ) GLOBAL_UNCERTAINTY_ASSIGNED_CONTEXT ( ( #7141 ) ) GLOBAL_UNIT_ASSIGNED_CONTEXT ( ( #26155, #36468, #40727 ) ) REPRESENTATION_CONTEXT ( 'NONE', 'WORKASPACE' ) ) ;
#39225 = VECTOR ( 'NONE', #46192, 39.37007874015748143 ) ;
#39226 = CARTESIAN_POINT ( 'NONE',  ( 0.7185039370078739607, 1.928577636452523993E-17, 1.633858267609007875 ) ) ;
#39227 = DIRECTION ( 'NONE',  ( -1.000000000000000000, 0.000000000000000000, 0.000000000000000000 ) ) ;
#39228 = CARTESIAN_POINT ( 'NONE',  ( 0.8107537697050253289, -0.1574803149606297803, 1.257381889763780736 ) ) ;
#39229 = CARTESIAN_POINT ( 'NONE',  ( 0.5555748031496091643, 0.4370297686271512605, 0.6367018223237037589 ) ) ;
#39230 = CARTESIAN_POINT ( 'NONE',  ( 0.000000000000000000, 0.000000000000000000, -0.1966003937007873570 ) ) ;
#39232 = CARTESIAN_POINT ( 'NONE',  ( 1.033464566929133799, 0.000000000000000000, 0.2755905510735752184 ) ) ;
#39231 = CARTESIAN_POINT ( 'NONE',  ( 0.6971942568897637749, 2.189545951927499583E-17, 0.6717519684501732646 ) ) ;
#39233 = CARTESIAN_POINT ( 'NONE',  ( 0.8070866141732283561, 0.000000000000000000, -0.6590551181102368705 ) ) ;
#39234 = DIRECTION ( 'NONE',  ( 0.000000000000000000, 0.000000000000000000, 1.000000000000000000 ) ) ;
#39235 = ORIENTED_EDGE ( 'NONE', *, *, #36334, .T. ) ;
#39236 = VECTOR ( 'NONE', #37174, 39.37007874015748143 ) ;
#39237 = CARTESIAN_POINT ( 'NONE',  ( 0.09009865225413171697, 0.1299212598425196763, 0.1562008126607098424 ) ) ;
#39238 = CARTESIAN_POINT ( 'NONE',  ( 0.9500414927467378812, -0.1787899950787401604, 0.7627952755367881643 ) ) ;
#39239 = CARTESIAN_POINT ( 'NONE',  ( 1.033464566929133799, 0.000000000000000000, 1.466535433070866201 ) ) ;
#39240 = CARTESIAN_POINT ( 'NONE',  ( 1.033464566929133799, 0.000000000000000000, 0.7086614172153071767 ) ) ;
#39241 = CARTESIAN_POINT ( 'NONE',  ( 0.07444174185955065859, 0.09001524553506463910, 0.1797182628040039087 ) ) ;
#39242 = CARTESIAN_POINT ( 'NONE',  ( 0.1264236179284866091, -1.004429133804503937, -0.1264236179284866091 ) ) ;
#39243 = CARTESIAN_POINT ( 'NONE',  ( 2.892866454678787531E-17, -1.474409448818897461, 0.1574803149606299191 ) ) ;
#39244 = CARTESIAN_POINT ( 'NONE',  ( 0.8759842519685039353, -0.1574803149606299191, 1.210629921152315047 ) ) ;
#39245 = CARTESIAN_POINT ( 'NONE',  ( 0.000000000000000000, 0.000000000000000000, 0.000000000000000000 ) ) ;
#39246 = ORIENTED_EDGE ( 'NONE', *, *, #5293, .F. ) ;
#39247 = CARTESIAN_POINT ( 'NONE',  ( -1.054774247047244540, 0.07405724077823318263, 1.919291338528913871 ) ) ;
#39248 = ORIENTED_EDGE ( 'NONE', *, *, #43557, .F. ) ;
#39249 = DIRECTION ( 'NONE',  ( 1.822029033848725028E-16, 0.000000000000000000, 1.000000000000000000 ) ) ;
#39250 = ORIENTED_EDGE ( 'NONE', *, *, #46150, .T. ) ;
#39251 = CARTESIAN_POINT ( 'NONE',  ( -1.054774247047244540, -0.07405724077823318263, 1.914370078686394860 ) ) ;
#39252 = CARTESIAN_POINT ( 'NONE',  ( -1.054774247047244096, 0.000000000000000000, 1.596948818843874074 ) ) ;
#39253 = CARTESIAN_POINT ( 'NONE',  ( 0.8019270111902716547, 0.1787899950787401604, 0.8661417322297002563 ) ) ;
#39254 = CARTESIAN_POINT ( 'NONE',  ( -0.7495606340400177148, 0.1264236179284866091, 0.1993110235682838682 ) ) ;
#39255 = ( BOUNDED_CURVE ( )  B_SPLINE_CURVE ( 2, ( #13610, #6413, #27809, #42369, #28250, #12934, #9567, #9329, #42813 ),
 .UNSPECIFIED., .F., .T. ) 
 B_SPLINE_CURVE_WITH_KNOTS ( ( 3, 2, 2, 2, 3 ),
 ( 0.6500000000000000222, 0.6524999999999999689, 0.6550000000000000266, 0.6574999999999999734, 0.6600000000000000311 ),
 .UNSPECIFIED. ) 
 CURVE ( )  GEOMETRIC_REPRESENTATION_ITEM ( )  RATIONAL_B_SPLINE_CURVE ( ( 1.000000000000000000, 0.9238795325112869605, 1.000000000000000000, 0.9238795325112869605, 1.000000000000000000, 0.9238795325112869605, 1.000000000000000000, 0.9238795325112869605, 1.000000000000000000 ) ) 
 REPRESENTATION_ITEM ( '' )  ) ;
#39256 = AXIS2_PLACEMENT_3D ( 'NONE', #5702, #21914, #46181 ) ;
#39257 = CARTESIAN_POINT ( 'NONE',  ( -0.1350291203833209053, 0.09842519685039377575, -0.2074739718643930364 ) ) ;
#39258 = CARTESIAN_POINT ( 'NONE',  ( -0.7495606340400177148, -0.1264236179284866091, 1.862696850339937038 ) ) ;
#39259 = CARTESIAN_POINT ( 'NONE',  ( -0.8759842519685039353, 0.1574803149606299191, 1.870078740157480324 ) ) ;
#39260 = LINE ( 'NONE', #6671, #30522 ) ;
#39261 = CARTESIAN_POINT ( 'NONE',  ( 0.1264236179284866091, -0.3165609761032547875, 0.1264236179284866091 ) ) ;
#39262 = CARTESIAN_POINT ( 'NONE',  ( 0.7185039370078739607, 1.928577636452523993E-17, 1.909448818790110192 ) ) ;
#39263 = DIRECTION ( 'NONE',  ( 0.000000000000000000, 0.000000000000000000, 1.000000000000000000 ) ) ;
#39264 = AXIS2_PLACEMENT_3D ( 'NONE', #18886, #15310, #29965 ) ;
#39265 = VECTOR ( 'NONE', #9133, 39.37007874015748143 ) ;
#39266 = CARTESIAN_POINT ( 'NONE',  ( -0.6971942568897626646, 0.07405724077823318263, 0.1181102361667090567 ) ) ;
#39268 = CLOSED_SHELL ( 'NONE', ( #44765, #32484, #1244, #13177, #43099, #8303, #3741, #3733, #16821, #2589, #1120, #44007, #3627, #17113, #5574, #29653, #11303, #26549, #1440, #47122, #23353, #4651, #41472, #32716, #32050, #12033, #1382, #39968, #9258, #28498, #28069, #33681, #32824, #16358, #47124, #13227, #43480, #15554, #18081, #32218, #12032, #41456, #4629, #35635, #9177, #46419, #5143, #22660, #44124, #33906, #5690, #24625, #35252, #44295, #36393, #42314, #16143, #46679, #2890, #13582 ) ) ;
#39267 = EDGE_CURVE ( 'NONE', #8850, #580, #15032, .T. ) ;
#39269 = VERTEX_POINT ( 'NONE', #16643 ) ;
#39270 = ORIENTED_EDGE ( 'NONE', *, *, #23008, .T. ) ;
#39271 = EDGE_CURVE ( 'NONE', #42434, #23712, #26973, .T. ) ;
#39272 = CARTESIAN_POINT ( 'NONE',  ( 0.1264236179284866091, -1.122539370024976391, -0.1264236179284866091 ) ) ;
#39273 = CARTESIAN_POINT ( 'NONE',  ( -0.1264236179284866091, -1.186515747977732183, -0.1264236179284866091 ) ) ;
#39274 = DIRECTION ( 'NONE',  ( 0.000000000000000000, 1.000000000000000000, 0.000000000000000000 ) ) ;
#39275 = CARTESIAN_POINT ( 'NONE',  ( 0.1797182628040039365, -0.5718942032838330025, -2.200913952912460540E-17 ) ) ;
#39276 = DIRECTION ( 'NONE',  ( -7.051687499798870116E-15, -1.406820448837680035E-16, -1.000000000000000000 ) ) ;
#39277 = CARTESIAN_POINT ( 'NONE',  ( -1.033464566929133799, 0.000000000000000000, 0.9842519683964094934 ) ) ;
#39278 = CARTESIAN_POINT ( 'NONE',  ( -0.9412147342319837628, 0.1574803149606300301, 0.8046259842519695171 ) ) ;
#39279 = CARTESIAN_POINT ( 'NONE',  ( 0.1574803149606300301, -0.1628937007874015908, -0.06523048226347956391 ) ) ;
#39280 = CARTESIAN_POINT ( 'NONE',  ( 0.7185039370078746268, -0.06523048226347956391, 1.833169291231055542 ) ) ;
#39281 = CARTESIAN_POINT ( 'NONE',  ( 1.033464566929133799, 0.000000000000000000, 0.2362204723334177248 ) ) ;
#39282 = CARTESIAN_POINT ( 'NONE',  ( 0.9412147342319837628, 0.1574803149606300301, 0.8046259842519695171 ) ) ;
#39283 = CARTESIAN_POINT ( 'NONE',  ( 0.1126596235262874585, -0.2304501682927049544, -0.02834147079956455748 ) ) ;
#39284 = DIRECTION ( 'NONE',  ( 1.000000000000000000, -0.000000000000000000, -0.000000000000000000 ) ) ;
#39286 = CARTESIAN_POINT ( 'NONE',  ( 0.1571168540705020489, -0.1349219317375998928, -0.04713923310949922479 ) ) ;
#39285 = CARTESIAN_POINT ( 'NONE',  ( 0.1939037905413676932, 0.1835438265964589033, -0.05114647357130735345 ) ) ;
#39287 = CARTESIAN_POINT ( 'NONE',  ( 0.7185039370078746268, -0.06523048226347956391, 0.1796259841444415029 ) ) ;
#39288 = VECTOR ( 'NONE', #29966, 39.37007874015748143 ) ;
#39289 = EDGE_LOOP ( 'NONE', ( #28703, #8686, #43049, #24605 ) ) ;
#39290 = CARTESIAN_POINT ( 'NONE',  ( -0.8107537697050254399, 0.1574803149606300301, 1.587106299105070839 ) ) ;
#39291 = CARTESIAN_POINT ( 'NONE',  ( 0.9412147342319837628, -0.1574803149606297803, 1.843011810916095783 ) ) ;
#39292 = CARTESIAN_POINT ( 'NONE',  ( -0.7185039370078746268, -0.06523048226347956391, 1.173720472440945350 ) ) ;
#39293 = CARTESIAN_POINT ( 'NONE',  ( -0.1264236179284866091, -0.5516732282926929409, 0.1264236179284866091 ) ) ;
#39294 = CARTESIAN_POINT ( 'NONE',  ( 0.1113553986120547346, -1.105314960629921295, -0.1113553986120547346 ) ) ;
#39295 = CARTESIAN_POINT ( 'NONE',  ( -0.7495606340400177148, -0.1264236179284866091, 1.936515747977732405 ) ) ;
#39296 = EDGE_LOOP ( 'NONE', ( #20288, #14996, #25752, #38680 ) ) ;
#39297 = CARTESIAN_POINT ( 'NONE',  ( -1.054774247047244540, 0.07405724077823318263, 1.446850393647023614 ) ) ;
#39298 = CARTESIAN_POINT ( 'NONE',  ( 1.054774247047244540, 0.07405724077823318263, 1.525590551127340433 ) ) ;
#39299 = CARTESIAN_POINT ( 'NONE',  ( -0.9873396505805591694, -0.1113553986120547346, 0.9104330708661417804 ) ) ;
#39300 = CARTESIAN_POINT ( 'NONE',  ( -0.1113553986120547346, -1.272637795168062746, 0.1113553986120547346 ) ) ;
#39301 = CARTESIAN_POINT ( 'NONE',  ( -0.7495606340400177148, 0.1264236179284866091, 0.5930118109698583329 ) ) ;
#39302 = CARTESIAN_POINT ( 'NONE',  ( 0.6971942568897626646, 0.07405724077823318263, 0.1624015747493861295 ) ) ;
#39303 = CARTESIAN_POINT ( 'NONE',  ( 0.6195511811023621807, 0.9842519685039365918, -1.186023622047243986 ) ) ;
#39304 = CARTESIAN_POINT ( 'NONE',  ( 0.6971942568897648851, -0.07405724077823297447, 0.7972440944344248992 ) ) ;
#39305 = CARTESIAN_POINT ( 'NONE',  ( -1.054774247047244540, -0.07405724077823318263, 0.5708661416785200116 ) ) ;
#39306 = CARTESIAN_POINT ( 'NONE',  ( 0.8107537697050254399, -0.1574803149606297803, 0.6274606299212601712 ) ) ;
#39307 = DIRECTION ( 'NONE',  ( -1.000000000000000000, 0.000000000000000000, 0.000000000000000000 ) ) ;
#39308 = ORIENTED_EDGE ( 'NONE', *, *, #2635, .T. ) ;
#39309 = CARTESIAN_POINT ( 'NONE',  ( -0.06523048226347956391, -0.2613188975302682127, -0.1574803149606300301 ) ) ;
#39310 = CARTESIAN_POINT ( 'NONE',  ( -0.7495606340400177148, 0.1264236179284866091, 1.459153543253322693 ) ) ;
#39311 = EDGE_LOOP ( 'NONE', ( #11172, #12131, #10602, #32851 ) ) ;
#39312 = CARTESIAN_POINT ( 'NONE',  ( -0.7646288533564489232, -0.1113553986120547346, 1.530511811023621993 ) ) ;
#39313 = CARTESIAN_POINT ( 'NONE',  ( -1.033464566929134687, 0.06523048226347956391, 0.4453740157480309270 ) ) ;
#39314 = CARTESIAN_POINT ( 'NONE',  ( 0.7495606340400177148, 0.1264236179284866091, 1.262303149552535420 ) ) ;
#39315 = CARTESIAN_POINT ( 'NONE',  ( 0.07328326258864251153, -0.09851384743134017352, 0.2080889956503677307 ) ) ;
#39316 = EDGE_LOOP ( 'NONE', ( #44527, #36619, #37826 ) ) ;
#39317 = DIRECTION ( 'NONE',  ( 0.000000000000000000, 0.000000000000000000, -1.000000000000000000 ) ) ;
#39318 = EDGE_CURVE ( 'NONE', #4638, #19219, #5048, .T. ) ;
#39319 = EDGE_LOOP ( 'NONE', ( #44502, #45871, #31515, #9280 ) ) ;
#39320 = CARTESIAN_POINT ( 'NONE',  ( -0.1787899950787401604, -0.5935039369541101895, -0.07405724077823318263 ) ) ;
#39321 = PLANE ( 'NONE',  #40746 ) ;
#39322 = VERTEX_POINT ( 'NONE', #8731 ) ;
#39323 = AXIS2_PLACEMENT_3D ( 'NONE', #34018, #41142, #1143 ) ;
#39324 = EDGE_CURVE ( 'NONE', #28102, #39322, #31041, .T. ) ;
#39325 = DIRECTION ( 'NONE',  ( 0.000000000000000000, -1.000000000000000000, -0.000000000000000000 ) ) ;
#39326 = CARTESIAN_POINT ( 'NONE',  ( 0.1787899950787401882, -0.3006889763241893943, -2.189545951927503898E-17 ) ) ;
#39327 = CARTESIAN_POINT ( 'NONE',  ( 0.1787899950787401882, -0.7682086613635590311, -2.189545951927503898E-17 ) ) ;
#39328 = CARTESIAN_POINT ( 'NONE',  ( -0.2471908670705637023, -0.09572725253288329184, -0.02814577918614243404 ) ) ;
#39329 = DIRECTION ( 'NONE',  ( -0.000000000000000000, 1.000000000000000000, -0.000000000000000000 ) ) ;
#39330 = CARTESIAN_POINT ( 'NONE',  ( 0.07405724077823318263, -0.04343105484341201056, 0.1787899950787401604 ) ) ;
#39331 = CARTESIAN_POINT ( 'NONE',  ( 0.1088466229509682248, -0.09842519685039366473, 0.1288475576157622204 ) ) ;
#39332 = CARTESIAN_POINT ( 'NONE',  ( -1.033464566929133799, 0.000000000000000000, 1.496062992018456494 ) ) ;
#39333 = CARTESIAN_POINT ( 'NONE',  ( 1.054774247047244096, 0.000000000000000000, 0.6126968503399370380 ) ) ;
#39334 = DIMENSIONAL_EXPONENTS ( 1.000000000000000000, 0.000000000000000000, 0.000000000000000000, 0.000000000000000000, 0.000000000000000000, 0.000000000000000000, 0.000000000000000000 ) ;
#39335 = CARTESIAN_POINT ( 'NONE',  ( -0.6971942568897648851, 0.07405724077823318263, 1.028543307032851573 ) ) ;
#39337 = CARTESIAN_POINT ( 'NONE',  ( 0.7185039370078739607, 1.928577636452523993E-17, 1.003937007766488199 ) ) ;
#39336 = CARTESIAN_POINT ( 'NONE',  ( 2.892866454678787531E-17, -0.9232283464566929387, 0.1574803149606299191 ) ) ;
#39338 = CARTESIAN_POINT ( 'NONE',  ( -0.1270800023317771588, -1.689020187535801076, 0.1270800023317771588 ) ) ;
#39339 = CARTESIAN_POINT ( 'NONE',  ( 0.8759842519685039353, -0.1787899950787401882, 1.631397637741511808 ) ) ;
#39341 = CARTESIAN_POINT ( 'NONE',  ( 0.2559055118110236671, 0.03078476920768365155, -0.3141842412145660068 ) ) ;
#39340 = CARTESIAN_POINT ( 'NONE',  ( 0.8019270111902716547, -0.1787899950787401604, 1.938976377898990799 ) ) ;
#39342 = CARTESIAN_POINT ( 'NONE',  ( 0.9500414927467377701, -0.1787899950787401604, 0.5265748030958428139 ) ) ;
#39343 = ORIENTED_EDGE ( 'NONE', *, *, #46836, .T. ) ;
#39344 = CARTESIAN_POINT ( 'NONE',  ( -0.1607876024859741237, -0.09201407021827166799, -0.1926022046197118087 ) ) ;
#39345 = CARTESIAN_POINT ( 'NONE',  ( 0.7646288533564489232, 0.1113553986120547346, 0.02460629921259842659 ) ) ;
#39346 = CARTESIAN_POINT ( 'NONE',  ( 0.000000000000000000, 0.000000000000000000, -0.09302377043719921301 ) ) ;
#39347 = CARTESIAN_POINT ( 'NONE',  ( -0.1787899950787401882, -0.1235236219934805202, 0.000000000000000000 ) ) ;
#39348 = CARTESIAN_POINT ( 'NONE',  ( 0.8019270111902717657, -0.1787899950787401604, 0.6397637794737947026 ) ) ;
#39349 = EDGE_CURVE ( 'NONE', #43008, #42075, #31774, .T. ) ;
#39350 = CARTESIAN_POINT ( 'NONE',  ( 0.1787899950787401882, -0.9650590550643465271, -2.189545951927503898E-17 ) ) ;
#39351 = CARTESIAN_POINT ( 'NONE',  ( 1.002407869896990045, -0.1264236179284866091, 0.1008858267178899676 ) ) ;
#39352 = LINE ( 'NONE', #21388, #17792 ) ;
#39353 = DIRECTION ( 'NONE',  ( -1.000000000000000000, 0.000000000000000000, 0.000000000000000000 ) ) ;
#39354 = CARTESIAN_POINT ( 'NONE',  ( -0.6971942568897648851, 0.07405724077823318263, 1.456692913332062744 ) ) ;
#39355 = ORIENTED_EDGE ( 'NONE', *, *, #26289, .T. ) ;
#39356 = CIRCLE ( 'NONE', #39461, 0.09842519685039370636 ) ;
#39357 = CARTESIAN_POINT ( 'NONE',  ( 0.9412147342319837628, -0.1574803149606297803, 0.4355314960629916299 ) ) ;
#39358 = CARTESIAN_POINT ( 'NONE',  ( 0.8759842519685039353, 0.1787899950787401882, 1.178641732229700922 ) ) ;
#39359 = AXIS2_PLACEMENT_3D ( 'NONE', #45164, #41551, #8759 ) ;
#39360 = CIRCLE ( 'NONE', #1880, 0.1870078740157481989 ) ;
#39361 = CARTESIAN_POINT ( 'NONE',  ( -1.033464566929134687, 0.06523048226347956391, 0.6717519683964102706 ) ) ;
#39362 = CARTESIAN_POINT ( 'NONE',  ( 1.033464566929133799, 0.000000000000000000, 1.505905511811023612 ) ) ;
#39363 = CARTESIAN_POINT ( 'NONE',  ( 0.9500414927467378812, 0.1787899950787401604, 1.801181102308441861 ) ) ;
#39364 = CARTESIAN_POINT ( 'NONE',  ( -0.7495606340400177148, -0.1264236179284866091, 0.9522637794737952577 ) ) ;
#39365 = PLANE ( 'NONE',  #7500 ) ;
#39366 = LINE ( 'NONE', #21159, #24694 ) ;
#39367 = CARTESIAN_POINT ( 'NONE',  ( 1.002407869896990045, 0.1264236179284866091, 0.3075787401037169411 ) ) ;
#39368 = PRODUCT_DEFINITION_CONTEXT ( 'detailed design', #46508, 'design' ) ;
#39369 = CARTESIAN_POINT ( 'NONE',  ( 0.7646288533564489232, 0.1113553986120547346, 1.510826771546015523 ) ) ;
#39370 = ORIENTED_EDGE ( 'NONE', *, *, #21541, .T. ) ;
#39371 = CARTESIAN_POINT ( 'NONE',  ( 0.1787899950787401882, 0.01427165359707061217, -2.189545951927503898E-17 ) ) ;
#39372 = CARTESIAN_POINT ( 'NONE',  ( 0.7495606340400177148, -0.1264236179284866091, 0.8390748030958424808 ) ) ;
#39373 = CARTESIAN_POINT ( 'NONE',  ( -0.8759842519685039353, -0.1787899950787401882, 1.626476377898992132 ) ) ;
#39374 = ORIENTED_EDGE ( 'NONE', *, *, #8219, .T. ) ;
#39375 = ADVANCED_FACE ( 'NONE', ( #489 ), #23272, .F. ) ;
#39376 = CARTESIAN_POINT ( 'NONE',  ( 0.08946752424252854552, 0.3740157480314960647, 1.224299699984021661 ) ) ;
#39377 = DIRECTION ( 'NONE',  ( 0.000000000000000000, 0.000000000000000000, 1.000000000000000000 ) ) ;
#39378 = CARTESIAN_POINT ( 'NONE',  ( 0.1264236179284866091, -1.290970424922151638, -0.1264236179284866091 ) ) ;
#39379 = ORIENTED_EDGE ( 'NONE', *, *, #27367, .T. ) ;
#39380 = CARTESIAN_POINT ( 'NONE',  ( 0.1787899950787401604, -0.1358267715997797664, -0.07405724077823318263 ) ) ;
#39381 = ORIENTED_EDGE ( 'NONE', *, *, #12899, .T. ) ;
#39382 = EDGE_CURVE ( 'NONE', #8358, #37845, #15379, .T. ) ;
#39383 = FACE_OUTER_BOUND ( 'NONE', #36638, .T. ) ;
#39384 = CARTESIAN_POINT ( 'NONE',  ( -0.8107537697050254399, -0.1574803149606297803, 0.4207677164279060578 ) ) ;
#39385 = CARTESIAN_POINT ( 'NONE',  ( 1.054774247047244096, 0.000000000000000000, 0.02214566923757503927 ) ) ;
#39386 = VECTOR ( 'NONE', #2357, 39.37007874015748143 ) ;
#39387 = VECTOR ( 'NONE', #44554, 39.37007874015748143 ) ;
#39388 = CARTESIAN_POINT ( 'NONE',  ( 3.284318927891251994E-17, -1.452263779473795369, 0.1787899950787401882 ) ) ;
#39389 = CARTESIAN_POINT ( 'NONE',  ( -0.9500414927467377701, -0.1787899950787401604, 0.3740157479777325711 ) ) ;
#39390 = CARTESIAN_POINT ( 'NONE',  ( -0.1404189863467107946, 0.2144232926957992391, -0.02742975588280811491 ) ) ;
#39391 = CARTESIAN_POINT ( 'NONE',  ( 0.8019270111902717657, 0.1787899950787401604, 1.220472440891118504 ) ) ;
#39392 = CARTESIAN_POINT ( 'NONE',  ( 1.054774247047244096, 0.000000000000000000, 1.557578740103716441 ) ) ;
#39393 = CARTESIAN_POINT ( 'NONE',  ( -0.7185039370078746268, 0.06523048226347956391, 0.6471456691838118891 ) ) ;
#39394 = CARTESIAN_POINT ( 'NONE',  ( 0.7646288533564489232, -0.1113553986120547346, 1.648622047244094668 ) ) ;
#39395 = CARTESIAN_POINT ( 'NONE',  ( 0.6195511811023612925, 0.6102362204724401940, 1.186023622047243986 ) ) ;
#39397 = CARTESIAN_POINT ( 'NONE',  ( 0.8759842519685039353, 0.1574803149606299191, 1.712598425196850238 ) ) ;
#39396 = CARTESIAN_POINT ( 'NONE',  ( -0.8759842519685039353, 0.1574803149606299191, 1.003937007874015741 ) ) ;
#39398 = CARTESIAN_POINT ( 'NONE',  ( 0.7185039370078778465, -0.06523048226348396317, 1.439468503829480772 ) ) ;
#39399 = CARTESIAN_POINT ( 'NONE',  ( 0.1574803149606300023, -0.4008464425712924273, -0.9238935802775078976 ) ) ;
#39400 = CARTESIAN_POINT ( 'NONE',  ( 0.06523048226347956391, -0.7928149605223941965, 0.1574803149606297803 ) ) ;
#39401 = CARTESIAN_POINT ( 'NONE',  ( -1.033464566929133799, 0.000000000000000000, 1.692913385719244213 ) ) ;
#39402 = CARTESIAN_POINT ( 'NONE',  ( 0.6971942568897637749, 2.189545951927499583E-17, 0.1993110235682838682 ) ) ;
#39403 = CARTESIAN_POINT ( 'NONE',  ( 0.7025635012355225806, 0.03299281671818125178, 0.03937034708046514841 ) ) ;
#39405 = CARTESIAN_POINT ( 'NONE',  ( -1.033464566929133799, 0.000000000000000000, 1.811023621939716444 ) ) ;
#39404 = CARTESIAN_POINT ( 'NONE',  ( 0.8759842519685039353, 0.1787899950787401882, 1.173720472387181246 ) ) ;
#39406 = DIRECTION ( 'NONE',  ( -0.000000000000000000, 1.000000000000000000, -0.000000000000000000 ) ) ;
#39407 = CARTESIAN_POINT ( 'NONE',  ( 0.9412147342319837628, -0.1574803149606297803, 0.5437992124908979097 ) ) ;
#39408 = VERTEX_POINT ( 'NONE', #45044 ) ;
#39409 = CARTESIAN_POINT ( 'NONE',  ( -0.8070866141732283561, -0.0009842519685049383633, -0.6590551181102368705 ) ) ;
#39410 = CARTESIAN_POINT ( 'NONE',  ( 0.9755857380299564063, 0.1348144502090965480, 0.03936793015238081866 ) ) ;
#39411 = PRODUCT_DEFINITION_SHAPE ( 'NONE', 'NONE',  #47467 ) ;
#39412 = CARTESIAN_POINT ( 'NONE',  ( -0.7185039370078739607, 1.928577636452523993E-17, 0.3740157479239689664 ) ) ;
#39413 = VERTEX_POINT ( 'NONE', #12022 ) ;
#39414 = CARTESIAN_POINT ( 'NONE',  ( 0.6971942568897637749, 2.189545951927499583E-17, 1.419783464513165505 ) ) ;
#39415 = VECTOR ( 'NONE', #8123, 39.37007874015748854 ) ;
#39417 = FACE_OUTER_BOUND ( 'NONE', #16410, .T. ) ;
#39416 = CARTESIAN_POINT ( 'NONE',  ( -0.7185039370078714072, 0.06523048226347728795, 1.641240157480314377 ) ) ;
#39418 = B_SPLINE_CURVE_WITH_KNOTS ( 'NONE', 3,
 ( #21330, #33760, #25836, #15529, #40639 ),
 .UNSPECIFIED., .F., .F.,
 ( 4, 1, 4 ),
 ( 0.000000000000000000, 0.002020725942163689639, 0.004041451884327379278 ),
 .UNSPECIFIED. ) ;
#39419 = CARTESIAN_POINT ( 'NONE',  ( -0.1787899950787401882, 0.03887795280966901967, 0.000000000000000000 ) ) ;
#39420 = ORIENTED_EDGE ( 'NONE', *, *, #39211, .T. ) ;
#39421 = CARTESIAN_POINT ( 'NONE',  ( -0.8759842519685039353, 0.000000000000000000, 0.000000000000000000 ) ) ;
#39422 = ( BOUNDED_CURVE ( )  B_SPLINE_CURVE ( 2, ( #8683, #5085, #34348, #1479, #1967, #31224, #16136, #27413, #45800 ),
 .UNSPECIFIED., .F., .T. ) 
 B_SPLINE_CURVE_WITH_KNOTS ( ( 3, 2, 2, 2, 3 ),
 ( 0.05999999999999999778, 0.06250000000000000000, 0.06500000000000000222, 0.06750000000000000444, 0.07000000000000000666 ),
 .UNSPECIFIED. ) 
 CURVE ( )  GEOMETRIC_REPRESENTATION_ITEM ( )  RATIONAL_B_SPLINE_CURVE ( ( 1.000000000000000000, 0.9238795325112869605, 1.000000000000000000, 0.9238795325112869605, 1.000000000000000000, 0.9238795325112869605, 1.000000000000000000, 0.9238795325112869605, 1.000000000000000000 ) ) 
 REPRESENTATION_ITEM ( '' )  ) ;
#39423 = ORIENTED_EDGE ( 'NONE', *, *, #40837, .T. ) ;
#39424 = AXIS2_PLACEMENT_3D ( 'NONE', #8801, #19592, #1599 ) ;
#39426 = CARTESIAN_POINT ( 'NONE',  ( 0.1850060400416835837, 0.08128102204193912717, 0.1786197838463692011 ) ) ;
#39425 = VECTOR ( 'NONE', #2607, 39.37007874015748143 ) ;
#39427 = CARTESIAN_POINT ( 'NONE',  ( 0.9500414927467378812, 0.1787899950787401604, 0.6249999999462356737 ) ) ;
#39428 = EDGE_CURVE ( 'NONE', #20344, #5435, #33413, .T. ) ;
#39429 = ORIENTED_EDGE ( 'NONE', *, *, #9641, .F. ) ;
#39430 = CARTESIAN_POINT ( 'NONE',  ( -0.8019270111902716547, -0.1787899950787401604, 1.348425196796630976 ) ) ;
#39431 = CARTESIAN_POINT ( 'NONE',  ( -0.07405724077823318263, -1.666338582623402953, -0.1787899950787401604 ) ) ;
#39432 = CARTESIAN_POINT ( 'NONE',  ( -0.9500414927467378812, 0.1787899950787401604, 1.136811023568283119 ) ) ;
#39433 = CIRCLE ( 'NONE', #40207, 0.1864803149606299171 ) ;
#39434 = AXIS2_PLACEMENT_3D ( 'NONE', #19049, #33717, #12125 ) ;
#39435 = CARTESIAN_POINT ( 'NONE',  ( -0.6971942568897648851, 0.07405724077823318263, 1.968503936954110189 ) ) ;
#39436 = EDGE_LOOP ( 'NONE', ( #32476, #12837, #31121, #26636 ) ) ;
#39437 = CARTESIAN_POINT ( 'NONE',  ( -0.9500414927467377701, 0.1787899950787401604, 1.053149606245450176 ) ) ;
#39438 = DIRECTION ( 'NONE',  ( 0.5000000000000003331, -0.8660254037844384856, 0.000000000000000000 ) ) ;
#39439 = CARTESIAN_POINT ( 'NONE',  ( 0.003620633035317427639, 0.04207376041596044836, -0.1377952987789565764 ) ) ;
#39440 = CARTESIAN_POINT ( 'NONE',  ( -0.1787899950787401604, -0.6881160942134909586, -0.07405724077823318263 ) ) ;
#39441 = VERTEX_POINT ( 'NONE', #15145 ) ;
#39442 = CARTESIAN_POINT ( 'NONE',  ( -0.7185039370078746268, -0.06523048226347956391, 0.6520669290263312323 ) ) ;
#39443 = ORIENTED_EDGE ( 'NONE', *, *, #1721, .T. ) ;
#39444 = CYLINDRICAL_SURFACE ( 'NONE', #16473, 0.1377952755905511029 ) ;
#39445 = CARTESIAN_POINT ( 'NONE',  ( -0.7185039370078746268, 0.06523048226347956391, 0.5684055117034967353 ) ) ;
#39446 = CARTESIAN_POINT ( 'NONE',  ( -0.6971942568897626646, 0.07405724077823318263, 0.7086614172690703928 ) ) ;
#39447 = CARTESIAN_POINT ( 'NONE',  ( 0.06523048226347956391, 0.07824803149606308905, -0.1574803149606300301 ) ) ;
#39448 = VERTEX_POINT ( 'NONE', #30028 ) ;
#39449 = CARTESIAN_POINT ( 'NONE',  ( -0.8759842519685039353, -0.1787899950787401882, 1.670767716481669440 ) ) ;
#39450 = AXIS2_PLACEMENT_3D ( 'NONE', #6177, #27567, #30918 ) ;
#39451 = CARTESIAN_POINT ( 'NONE',  ( 0.8107537697050254399, -0.1574803149606297803, 1.336122047244094446 ) ) ;
#39452 = CARTESIAN_POINT ( 'NONE',  ( 0.7185039370078746268, 0.06523048226347956391, 1.040846456585385882 ) ) ;
#39453 = DIRECTION ( 'NONE',  ( 0.000000000000000000, 0.000000000000000000, 1.000000000000000000 ) ) ;
#39454 = ORIENTED_EDGE ( 'NONE', *, *, #22404, .T. ) ;
#39455 = CARTESIAN_POINT ( 'NONE',  ( 0.07444174185955065859, -0.8942367229688730212, 0.1797182628040039087 ) ) ;
#39456 = CARTESIAN_POINT ( 'NONE',  ( -0.4240551181102362177, 0.2559055118110236116, 3.133938659235354185E-17 ) ) ;
#39457 = CARTESIAN_POINT ( 'NONE',  ( -0.7185039370078746268, 0.06523048226347956391, 1.316437007766489975 ) ) ;
#39458 = CARTESIAN_POINT ( 'NONE',  ( 0.8759842519685039353, -0.1787899950787401882, 0.7652559054580472253 ) ) ;
#39459 = CARTESIAN_POINT ( 'NONE',  ( -0.1574803149606299191, -0.6181102362204724532, 0.000000000000000000 ) ) ;
#39460 = VECTOR ( 'NONE', #13023, 39.37007874015748854 ) ;
#39461 = AXIS2_PLACEMENT_3D ( 'NONE', #31761, #10181, #7045 ) ;
#39462 = DIRECTION ( 'NONE',  ( 0.000000000000000000, 0.000000000000000000, 1.000000000000000000 ) ) ;
#39463 = CARTESIAN_POINT ( 'NONE',  ( -0.2559055118110236116, 0.07922414731028902535, -0.05306965205172459177 ) ) ;
#39464 = CARTESIAN_POINT ( 'NONE',  ( 0.9412147342319837628, -0.1574803149606297803, 1.301673228346455602 ) ) ;
#39466 = LENGTH_MEASURE_WITH_UNIT ( LENGTH_MEASURE( 0.02539999999999999897 ), #17431 ) ;
#39465 = CARTESIAN_POINT ( 'NONE',  ( 0.7498931371579079519, -0.1140439591228732952, 1.985582266786952488 ) ) ;
#39467 = CARTESIAN_POINT ( 'NONE',  ( 0.7646288533564489232, -0.1113553986120547346, 1.727362204724409489 ) ) ;
#39469 = CARTESIAN_POINT ( 'NONE',  ( 0.000000000000000000, 0.000000000000000000, 0.000000000000000000 ) ) ;
#39468 = CARTESIAN_POINT ( 'NONE',  ( 1.054774247047244096, 0.000000000000000000, 0.6126968503399370380 ) ) ;
#39470 = DIRECTION ( 'NONE',  ( 1.000000000000000000, -0.000000000000000000, -0.000000000000000000 ) ) ;
#39471 = CARTESIAN_POINT ( 'NONE',  ( 0.1611065205440928294, 0.07958672989228716965, 0.1378549147581101531 ) ) ;
#39472 = CARTESIAN_POINT ( 'NONE',  ( 0.002094777259473996466, 0.1034000088769234660, -0.09649716854706523461 ) ) ;
#39473 = CARTESIAN_POINT ( 'NONE',  ( 0.8759842519685039353, -0.1787899950787401882, 0.9571850393163149340 ) ) ;
#39474 = ADVANCED_FACE ( 'NONE', ( #1436 ), #30262, .F. ) ;
#39475 = VERTEX_POINT ( 'NONE', #29792 ) ;
#39476 = DIRECTION ( 'NONE',  ( 1.822029033848725028E-16, 0.000000000000000000, 1.000000000000000000 ) ) ;
#39477 = CARTESIAN_POINT ( 'NONE',  ( 1.284448818897637956, -0.3937007874015748254, -1.181102362204724310 ) ) ;
#39478 = CARTESIAN_POINT ( 'NONE',  ( -0.1797182628040039087, 0.1539916234878207224, -0.07444174185955065859 ) ) ;
#39479 = CARTESIAN_POINT ( 'NONE',  ( 0.07405724077823318263, -1.056102362150961982, 0.1787899950787401604 ) ) ;
#39480 = CARTESIAN_POINT ( 'NONE',  ( 0.1574803149606300301, -1.467027559055119168, 0.06523048226347956391 ) ) ;
#39481 = ADVANCED_FACE ( 'NONE', ( #40971 ), #11425, .T. ) ;
#39482 = CARTESIAN_POINT ( 'NONE',  ( 0.1377952755905511861, 0.1574803149606299191, -0.8070866141732283561 ) ) ;
#39483 = CARTESIAN_POINT ( 'NONE',  ( -0.8019270111902717657, 0.1787899950787401604, 0.03444881884387430981 ) ) ;
#39484 = EDGE_CURVE ( 'NONE', #17273, #3953, #24965, .T. ) ;
#39485 = DIRECTION ( 'NONE',  ( -1.000000000000000000, -0.000000000000000000, 0.000000000000000000 ) ) ;
#39486 = EDGE_LOOP ( 'NONE', ( #15081, #5620, #16649, #14760 ) ) ;
#39487 = CARTESIAN_POINT ( 'NONE',  ( 0.06523048226347956391, -1.447342519577512476, -0.1574803149606300301 ) ) ;
#39488 = CARTESIAN_POINT ( 'NONE',  ( -1.054774247047244096, 0.000000000000000000, 1.877460629867496067 ) ) ;
#39489 = CARTESIAN_POINT ( 'NONE',  ( -0.8759842519685039353, -0.1787899950787401882, 1.468996062938362046 ) ) ;
#39490 = AXIS2_PLACEMENT_3D ( 'NONE', #6355, #17865, #10696 ) ;
#39491 = CARTESIAN_POINT ( 'NONE',  ( 1.054774247047244540, -0.07405724077823318263, 0.8513779527021426707 ) ) ;
#39492 = CARTESIAN_POINT ( 'NONE',  ( -1.002407869896990045, 0.1264236179284866091, 1.090059055064346527 ) ) ;
#39493 = CARTESIAN_POINT ( 'NONE',  ( -0.7495606340400177148, -0.1264236179284866091, 0.3666338582139531677 ) ) ;
#39494 = CARTESIAN_POINT ( 'NONE',  ( 0.3649999999999999911, 2.679610302993149545E-17, 0.000000000000000000 ) ) ;
#39495 = CARTESIAN_POINT ( 'NONE',  ( -0.9500414927467378812, 0.1787899950787401604, 1.845472440891119392 ) ) ;
#39496 = CARTESIAN_POINT ( 'NONE',  ( -0.9412147342319837628, 0.1574803149606300301, 1.946358267716538082 ) ) ;
#39497 = CARTESIAN_POINT ( 'NONE',  ( 0.2559046883225459812, 0.07066125644906998127, -0.04784811367750762406 ) ) ;
#39498 = CARTESIAN_POINT ( 'NONE',  ( 3.284318927891251994E-17, -0.2427420784654590602, 0.1787899950787401882 ) ) ;
#39499 = CARTESIAN_POINT ( 'NONE',  ( -0.1150168755148803235, -0.09842519685039370636, 0.1175860779051826899 ) ) ;
#39500 = DIRECTION ( 'NONE',  ( 3.469446951953631938E-15, 1.000000000000000000, 0.000000000000000000 ) ) ;
#39501 = CARTESIAN_POINT ( 'NONE',  ( -1.002407869896990045, -0.1264236179284866091, 0.1747047243556852092 ) ) ;
#39502 = B_SPLINE_CURVE_WITH_KNOTS ( 'NONE', 3,
 ( #10372, #40040, #40509, #7698, #25705, #35999, #22312, #3403, #24979, #3638, #4095, #3157, #40276, #18016, #10856, #32901, #25469, #7463, #17782, #18717, #32430, #47009, #28844, #7237, #21857, #18258, #14670 ),
 .UNSPECIFIED., .F., .F.,
 ( 4, 2, 2, 2, 2, 2, 2, 2, 2, 2, 1, 2, 2, 4 ),
 ( 0.000000000000000000, 0.1249999999999987232, 0.2499999999999974465, 0.3124999999999967804, 0.3749999999999961697, 0.4374999999999955591, 0.4999999999999948930, 0.6249999999999946709, 0.6874999999999952260, 0.7499999999999956701, 0.8124999999999961142, 0.8437499999999963363, 0.8749999999999965583, 1.000000000000000000 ),
 .UNSPECIFIED. ) ;
#39503 = ORIENTED_EDGE ( 'NONE', *, *, #38109, .T. ) ;
#39504 = CARTESIAN_POINT ( 'NONE',  ( -0.8019270111902716547, -0.1787899950787401604, 1.195866141678520345 ) ) ;
#39505 = ORIENTED_EDGE ( 'NONE', *, *, #21130, .F. ) ;
#39506 = CARTESIAN_POINT ( 'NONE',  ( -0.1787899950787401882, -1.186515747977732183, 0.000000000000000000 ) ) ;
#39507 = CARTESIAN_POINT ( 'NONE',  ( -0.07405724077823318263, -1.385826771599779184, -0.1787899950787401604 ) ) ;
#39508 = CARTESIAN_POINT ( 'NONE',  ( -0.8759842519685039353, 0.1574803149606299191, 1.545275590443653480 ) ) ;
#39509 = ( NAMED_UNIT ( * ) PLANE_ANGLE_UNIT ( ) SI_UNIT ( $, .RADIAN. ) ) ;
#39510 = CARTESIAN_POINT ( 'NONE',  ( 0.1797182628040039087, -0.6088036521027303527, -0.07444174185955065859 ) ) ;
#39511 = DIRECTION ( 'NONE',  ( 0.000000000000000000, 0.000000000000000000, 1.000000000000000000 ) ) ;
#39512 = CARTESIAN_POINT ( 'NONE',  ( -0.7185039370078739607, 1.928577636452523993E-17, 0.9645669290263307882 ) ) ;
#39513 = CARTESIAN_POINT ( 'NONE',  ( -0.9873396505805591694, 0.1113553986120547346, 0.7627952755905511584 ) ) ;
#39514 = CARTESIAN_POINT ( 'NONE',  ( -9.642888182262618425E-18, -0.1555118110236220763, -0.1574803149606299191 ) ) ;
#39515 = CARTESIAN_POINT ( 'NONE',  ( 0.7646288533564489232, 0.1113553986120547346, 1.825787401467275473 ) ) ;
#39516 = VERTEX_POINT ( 'NONE', #22795 ) ;
#39517 = CARTESIAN_POINT ( 'NONE',  ( 0.8759842519685039353, -0.1574803149606299191, 0.2263779526483783444 ) ) ;
#39518 = CARTESIAN_POINT ( 'NONE',  ( 1.033464566929134687, 0.06523048226347956391, 0.7209645669291341319 ) ) ;
#39519 = CARTESIAN_POINT ( 'NONE',  ( 0.06699593397070344181, -0.2568141117498130566, -0.04769437235513194345 ) ) ;
#39520 = DIRECTION ( 'NONE',  ( -0.000000000000000000, 1.000000000000000000, -0.000000000000000000 ) ) ;
#39522 = CARTESIAN_POINT ( 'NONE',  ( 0.1582120475477764854, -0.1029568672337116270, -0.1025480767803625959 ) ) ;
#39521 = CARTESIAN_POINT ( 'NONE',  ( 0.000000000000000000, 0.000000000000000000, 0.000000000000000000 ) ) ;
#39523 = CARTESIAN_POINT ( 'NONE',  ( 0.8759842519685039353, 0.1574803149606299191, 0.2460629920184571051 ) ) ;
#39524 = ORIENTED_EDGE ( 'NONE', *, *, #29107, .F. ) ;
#39525 = ADVANCED_FACE ( 'NONE', ( #22555 ), #11796, .T. ) ;
#39526 = DIRECTION ( 'NONE',  ( 0.000000000000000000, 0.000000000000000000, 1.000000000000000000 ) ) ;
#39527 = CARTESIAN_POINT ( 'NONE',  ( 1.033464566929134687, -0.06523048226347956391, 1.847933070758615237 ) ) ;
#39528 = CARTESIAN_POINT ( 'NONE',  ( 0.06523048226347956391, -1.540846456585386548, 0.1574803149606297803 ) ) ;
#39529 = CARTESIAN_POINT ( 'NONE',  ( -0.07405724077823318263, -0.5885826771115909573, 0.1787899950787401604 ) ) ;
#39530 = CARTESIAN_POINT ( 'NONE',  ( 0.06523048226347956391, -0.9847440944881884484, -0.1574803149606300301 ) ) ;
#39531 = CARTESIAN_POINT ( 'NONE',  ( 0.8759842519685039353, 0.1574803149606299191, 1.033464566821606478 ) ) ;
#39532 = ( BOUNDED_CURVE ( )  B_SPLINE_CURVE ( 2, ( #29037, #10807, #25420, #7187, #2396, #46245, #13444, #39056, #42634 ),
 .UNSPECIFIED., .F., .T. ) 
 B_SPLINE_CURVE_WITH_KNOTS ( ( 3, 2, 2, 2, 3 ),
 ( 0.3699999999999999956, 0.3724999999999999978, 0.3750000000000000000, 0.3775000000000000022, 0.3800000000000000044 ),
 .UNSPECIFIED. ) 
 CURVE ( )  GEOMETRIC_REPRESENTATION_ITEM ( )  RATIONAL_B_SPLINE_CURVE ( ( 1.000000000000000000, 0.9238795325112869605, 1.000000000000000000, 0.9238795325112869605, 1.000000000000000000, 0.9238795325112869605, 1.000000000000000000, 0.9238795325112869605, 1.000000000000000000 ) ) 
 REPRESENTATION_ITEM ( '' )  ) ;
#39533 = EDGE_CURVE ( 'NONE', #24250, #20094, #21118, .T. ) ;
#39534 = DIRECTION ( 'NONE',  ( -1.000000000000000000, 0.000000000000000000, 0.000000000000000000 ) ) ;
#39535 = CARTESIAN_POINT ( 'NONE',  ( -1.002407869896990045, 0.1264236179284866091, 0.3420275590013546751 ) ) ;
#39536 = ORIENTED_EDGE ( 'NONE', *, *, #12090, .F. ) ;
#39537 = ORIENTED_EDGE ( 'NONE', *, *, #23872, .F. ) ;
#39538 = CARTESIAN_POINT ( 'NONE',  ( -0.8019270111902717657, -0.1787899950787401604, 1.550196850339937926 ) ) ;
#39539 = ADVANCED_FACE ( 'NONE', ( #37173, #37401 ), #26173, .T. ) ;
#39540 = CARTESIAN_POINT ( 'NONE',  ( 0.6971942568897637749, 2.189545951927499583E-17, 1.582185039316315045 ) ) ;
#39541 = EDGE_LOOP ( 'NONE', ( #27146, #12945, #14336, #21413 ) ) ;
#39542 = CARTESIAN_POINT ( 'NONE',  ( -0.7185039370078739607, 1.928577636452523993E-17, 0.4921259841444416971 ) ) ;
#39543 = CARTESIAN_POINT ( 'NONE',  ( -0.8759842519685039353, 0.1787899950787401882, 0.6668307086076534773 ) ) ;
#39544 = CARTESIAN_POINT ( 'NONE',  ( 0.8019270111902717657, -0.1787899950787401604, 0.2116141731745827814 ) ) ;
#39545 = EDGE_CURVE ( 'NONE', #34176, #33124, #10434, .T. ) ;
#39546 = CARTESIAN_POINT ( 'NONE',  ( -1.033464566929134687, -0.06523048226347956391, 1.690452755797985152 ) ) ;
#39547 = CARTESIAN_POINT ( 'NONE',  ( -0.6971942568897648851, 0.07405724077823318263, 0.6299212597887560161 ) ) ;
#39548 = CARTESIAN_POINT ( 'NONE',  ( 0.1910692666444111232, -0.07766248740297354569, 0.1751191768260063897 ) ) ;
#39549 = CARTESIAN_POINT ( 'NONE',  ( -0.1476377952755905387, 0.7443365962042343131, -3.523993443072799270 ) ) ;
#39550 = CARTESIAN_POINT ( 'NONE',  ( 0.06523048226347956391, -0.2416338581601896740, 0.1574803149606297803 ) ) ;
#39551 = CARTESIAN_POINT ( 'NONE',  ( -0.8759842519685039353, -0.1787899950787401882, 1.434547244040724534 ) ) ;
#39552 = ORIENTED_EDGE ( 'NONE', *, *, #16994, .T. ) ;
#39553 = CARTESIAN_POINT ( 'NONE',  ( -0.8107537697050253289, 0.1574803149606300301, 0.5339566929133855444 ) ) ;
#39554 = CARTESIAN_POINT ( 'NONE',  ( 1.054774247047244540, 0.07405724077823318263, 1.486220472387181912 ) ) ;
#39555 = CARTESIAN_POINT ( 'NONE',  ( 0.1312513784215866286, -0.09851384505487205401, -0.1483491369261773773 ) ) ;
#39556 = CARTESIAN_POINT ( 'NONE',  ( 0.7185039370078739607, 1.928577636452523993E-17, 1.515748031388535200 ) ) ;
#39557 = ORIENTED_EDGE ( 'NONE', *, *, #28163, .T. ) ;
#39558 = ORIENTED_EDGE ( 'NONE', *, *, #47352, .F. ) ;
#39559 = FACE_OUTER_BOUND ( 'NONE', #45509, .T. ) ;
#39560 = ORIENTED_EDGE ( 'NONE', *, *, #25397, .F. ) ;
#39561 = CARTESIAN_POINT ( 'NONE',  ( 0.2821522309711287368, 4.616380251121755931E-17, 0.000000000000000000 ) ) ;
#39562 = CARTESIAN_POINT ( 'NONE',  ( -0.07405724077823318263, -0.3523622046706461619, 0.1787899950787401604 ) ) ;
#39563 = CARTESIAN_POINT ( 'NONE',  ( 3.284318927891251994E-17, -0.9355314960092283583, 0.1787899950787401882 ) ) ;
#39564 = CYLINDRICAL_SURFACE ( 'NONE', #14211, 0.1574803149606299191 ) ;
#39565 = FACE_OUTER_BOUND ( 'NONE', #26156, .T. ) ;
#39566 = CARTESIAN_POINT ( 'NONE',  ( 0.9500414927467378812, -0.1787899950787401604, 0.3690944881352128393 ) ) ;
#39567 = CARTESIAN_POINT ( 'NONE',  ( 0.1264236179284866091, -0.08034050366230964524, 0.1264236179284866091 ) ) ;
#39568 = CARTESIAN_POINT ( 'NONE',  ( -0.1787899950787401604, -0.2736220471903310081, 0.07405724077823318263 ) ) ;
#39569 = CARTESIAN_POINT ( 'NONE',  ( 0.07405724077823318263, 0.02165354336085014916, -0.1787899950787401604 ) ) ;
#39570 = LINE ( 'NONE', #24734, #14251 ) ;
#39571 = DIRECTION ( 'NONE',  ( 0.000000000000000000, -1.000000000000000000, 0.000000000000000000 ) ) ;
#39572 = CARTESIAN_POINT ( 'NONE',  ( 0.7495606340400177148, 0.1264236179284866091, 0.6274606298674959559 ) ) ;
#39573 = CARTESIAN_POINT ( 'NONE',  ( -0.8759842519685039353, 0.1787899950787401882, 0.9817913385289134265 ) ) ;
#39574 = DIRECTION ( 'NONE',  ( -1.000000000000000000, -6.679788269418529283E-17, 0.000000000000000000 ) ) ;
#39575 = CARTESIAN_POINT ( 'NONE',  ( -0.07444174185955065859, -1.780063494622415865, -0.1797182628040039087 ) ) ;
#39576 = CARTESIAN_POINT ( 'NONE',  ( -1.094772975963752103E-17, -0.4434055117572598959, -0.1787899950787401882 ) ) ;
#39577 = CARTESIAN_POINT ( 'NONE',  ( 0.1574803149606299191, 0.5360961046428496246, -0.7563373642699310340 ) ) ;
#39578 = CARTESIAN_POINT ( 'NONE',  ( 0.9500414927467378812, 0.1787899950787401604, 1.609251968450173376 ) ) ;
#39580 = DIRECTION ( 'NONE',  ( 1.822029033848725028E-16, 0.000000000000000000, 1.000000000000000000 ) ) ;
#39579 = FACE_OUTER_BOUND ( 'NONE', #9131, .T. ) ;
#39581 = CARTESIAN_POINT ( 'NONE',  ( 1.054774247047244540, -0.07405724077823318263, 0.5314960629383620461 ) ) ;
#39582 = VERTEX_POINT ( 'NONE', #22314 ) ;
#39584 = VERTEX_POINT ( 'NONE', #32903 ) ;
#39583 = CARTESIAN_POINT ( 'NONE',  ( -0.1986060025687029773, -0.07294156354251685181, -0.1707667409195914865 ) ) ;
#39585 = LINE ( 'NONE', #20200, #38218 ) ;
#39586 = CARTESIAN_POINT ( 'NONE',  ( -0.1264236179284866091, -0.08907480309584270284, -0.1264236179284866091 ) ) ;
#39587 = CARTESIAN_POINT ( 'NONE',  ( 0.8019270111902717657, 0.1787899950787401604, 0.5462598424659214080 ) ) ;
#39588 = CARTESIAN_POINT ( 'NONE',  ( -0.1787899950787401882, -1.142224409395055096, 0.000000000000000000 ) ) ;
#39589 = CARTESIAN_POINT ( 'NONE',  ( 0.8019270111902717657, -0.1787899950787401604, 0.09350393695411057804 ) ) ;
#39590 = EDGE_CURVE ( 'NONE', #26985, #3096, #16557, .T. ) ;
#39591 = DIRECTION ( 'NONE',  ( 0.000000000000000000, -0.6156614753256597350, -0.7880107536067207930 ) ) ;
#39592 = CARTESIAN_POINT ( 'NONE',  ( -0.7495606340400177148, 0.1264236179284866091, 1.532972440891118060 ) ) ;
#39593 = ORIENTED_EDGE ( 'NONE', *, *, #8653, .T. ) ;
#39594 = CARTESIAN_POINT ( 'NONE',  ( 0.9873396505805591694, -0.1113553986120547346, 0.1624015748031496231 ) ) ;
#39595 = CARTESIAN_POINT ( 'NONE',  ( 1.002407869896990045, -0.1264236179284866091, 1.124507873961984261 ) ) ;
#39596 = CARTESIAN_POINT ( 'NONE',  ( -0.9873396505805591694, -0.1113553986120547346, 0.6643700786326299790 ) ) ;
#39597 = CARTESIAN_POINT ( 'NONE',  ( 0.7185039370078739607, 1.928577636452523993E-17, 0.1082677165354330728 ) ) ;
#39598 = CARTESIAN_POINT ( 'NONE',  ( 1.002407869896990045, 0.1264236179284866091, 1.759350393647023614 ) ) ;
#39599 = CARTESIAN_POINT ( 'NONE',  ( -0.9412147342319837628, -0.1574803149606297803, 0.5536417322834641386 ) ) ;
#39600 = CARTESIAN_POINT ( 'NONE',  ( -0.9500414927467378812, 0.1787899950787401604, 0.9350393700249758355 ) ) ;
#39601 = ADVANCED_FACE ( 'NONE', ( #12029 ), #25707, .F. ) ;
#39602 = CARTESIAN_POINT ( 'NONE',  ( -1.033464566929133799, 0.000000000000000000, 0.6299212597349921339 ) ) ;
#39603 = DIRECTION ( 'NONE',  ( -1.000000000000000000, 3.469446951953625627E-15, 0.000000000000000000 ) ) ;
#39604 = CARTESIAN_POINT ( 'NONE',  ( 0.7495606340400177148, -0.1264236179284866091, 0.2878937007336381804 ) ) ;
#39605 = CARTESIAN_POINT ( 'NONE',  ( -0.9500414927467377701, 0.1787899950787401604, 0.1870078739619845110 ) ) ;
#39606 = CARTESIAN_POINT ( 'NONE',  ( -1.054774247047244540, -0.07405724077823318263, 0.6496062991588353874 ) ) ;
#39607 = CARTESIAN_POINT ( 'NONE',  ( 0.8759842519685039353, -0.1574803149606299191, 1.525590551073574774 ) ) ;
#39608 = ORIENTED_EDGE ( 'NONE', *, *, #38052, .F. ) ;
#39609 = AXIS2_PLACEMENT_3D ( 'NONE', #31722, #38887, #20677 ) ;
#39610 = CARTESIAN_POINT ( 'NONE',  ( 0.1787899950787401882, -0.02509842514308689362, -2.189545951927503898E-17 ) ) ;
#39611 = CARTESIAN_POINT ( 'NONE',  ( 0.9500414927467378812, -0.1787899950787401604, 0.8070866141194653620 ) ) ;
#39612 = CARTESIAN_POINT ( 'NONE',  ( -0.6971942568897637749, 2.189545951927499583E-17, 1.852854330654897685 ) ) ;
#39613 = AXIS2_PLACEMENT_3D ( 'NONE', #14636, #24730, #21333 ) ;
#39614 = CYLINDRICAL_SURFACE ( 'NONE', #10780, 0.1574803149606299191 ) ;
#39615 = DIRECTION ( 'NONE',  ( 1.144917494144692682E-16, -5.091027988365947196E-31, 1.000000000000000000 ) ) ;
#39616 = CARTESIAN_POINT ( 'NONE',  ( 0.07405724077823318263, -1.342643653268609460, 0.1787899950787401604 ) ) ;
#39617 = ORIENTED_EDGE ( 'NONE', *, *, #31519, .F. ) ;
#39618 = CARTESIAN_POINT ( 'NONE',  ( 0.07405724077823318263, -0.2883858267178899260, -0.1787899950787401604 ) ) ;
#39619 = DIRECTION ( 'NONE',  ( -0.000000000000000000, 0.000000000000000000, 1.000000000000000000 ) ) ;
#39620 = EDGE_LOOP ( 'NONE', ( #37414, #40405, #22539, #27463 ) ) ;
#39621 = CARTESIAN_POINT ( 'NONE',  ( 0.4509871776442260227, 1.205361022782824954E-17, -0.09842519685039370636 ) ) ;
#39622 = EDGE_CURVE ( 'NONE', #26907, #28221, #22670, .T. ) ;
#39623 = CARTESIAN_POINT ( 'NONE',  ( 1.002407869896990045, 0.1264236179284866091, 0.06643700782025216411 ) ) ;
#39624 = CARTESIAN_POINT ( 'NONE',  ( 0.1264236179284866091, -1.594980314906866203, -0.1264236179284866091 ) ) ;
#39625 = CARTESIAN_POINT ( 'NONE',  ( -0.9500414927467377701, -0.1787899950787401604, 0.4921259841982049132 ) ) ;
#39626 = FACE_OUTER_BOUND ( 'NONE', #41765, .T. ) ;
#39627 = CARTESIAN_POINT ( 'NONE',  ( 1.054774247047244540, -0.07405724077823318263, 1.166338582623402509 ) ) ;
#39628 = CARTESIAN_POINT ( 'NONE',  ( 0.9500414927467377701, -0.1787899950787401604, 1.471456692859622217 ) ) ;
#39629 = CARTESIAN_POINT ( 'NONE',  ( -0.8107537697050254399, 0.1574803149606300301, 0.6028543306011346914 ) ) ;
#39630 = CARTESIAN_POINT ( 'NONE',  ( -0.7185039370078739607, 1.928577636452523993E-17, 1.013779527559055094 ) ) ;
#39631 = DIRECTION ( 'NONE',  ( 0.000000000000000000, 0.000000000000000000, -1.000000000000000000 ) ) ;
#39632 = CARTESIAN_POINT ( 'NONE',  ( -0.9412147342319837628, -0.1574803149606297803, 1.803641732175937484 ) ) ;
#39633 = AXIS2_PLACEMENT_3D ( 'NONE', #44324, #3847, #244 ) ;
#39634 = CARTESIAN_POINT ( 'NONE',  ( 0.8019270111902717657, 0.1787899950787401604, 0.2312992125446618197 ) ) ;
#39635 = CARTESIAN_POINT ( 'NONE',  ( 0.7020141857328450197, -0.007037461325149993799, 0.03936291678462715965 ) ) ;
#39636 = ADVANCED_FACE ( 'NONE', ( #19191 ), #44875, .F. ) ;
#39638 = CARTESIAN_POINT ( 'NONE',  ( -0.7646288533564489232, -0.1113553986120547346, 0.5364173227271189504 ) ) ;
#39637 = CARTESIAN_POINT ( 'NONE',  ( 0.9500414927467377701, -0.1787899950787401604, 1.156496062938362046 ) ) ;
#39639 = PLANE ( 'NONE',  #44162 ) ;
#39640 = CARTESIAN_POINT ( 'NONE',  ( 0.9873396505805591694, 0.1113553986120547346, 0.5167322833570401341 ) ) ;
#39641 = VERTEX_POINT ( 'NONE', #33377 ) ;
#39642 = CARTESIAN_POINT ( 'NONE',  ( -1.707404996040165498E-16, 1.086379535891622172, -0.03715491745705901822 ) ) ;
#39643 = CARTESIAN_POINT ( 'NONE',  ( 0.9858132855136036987, 0.1256053033721491741, 0.03936520543643565878 ) ) ;
#39644 = CARTESIAN_POINT ( 'NONE',  ( -1.033464566929133799, 0.000000000000000000, 0.4330708660342047489 ) ) ;
#39645 = ORIENTED_EDGE ( 'NONE', *, *, #12295, .F. ) ;
#39646 = CARTESIAN_POINT ( 'NONE',  ( 0.8019270111902717657, 0.1787899950787401604, 1.451771653489543290 ) ) ;
#39648 = CYLINDRICAL_SURFACE ( 'NONE', #36921, 0.1574803149606299191 ) ;
#39647 = CARTESIAN_POINT ( 'NONE',  ( -1.033464566929133799, 0.000000000000000000, 1.624015748031496287 ) ) ;
#39649 = CARTESIAN_POINT ( 'NONE',  ( -0.1264236179284866091, -0.08415354325332302654, -0.1264236179284866091 ) ) ;
#39650 = VERTEX_POINT ( 'NONE', #22085 ) ;
#39651 = LENGTH_MEASURE_WITH_UNIT ( LENGTH_MEASURE( 0.02539999999999999897 ), #24823 ) ;
#39652 = EDGE_LOOP ( 'NONE', ( #27644, #27868, #36434, #21762, #35651, #26032 ) ) ;
#39653 = CARTESIAN_POINT ( 'NONE',  ( 0.9500414927467378812, -0.1787899950787401604, 0.5314960629383620461 ) ) ;
#39654 = EDGE_LOOP ( 'NONE', ( #13623, #12015, #14248, #44332 ) ) ;
#39655 = CARTESIAN_POINT ( 'NONE',  ( -1.002407869896990045, -0.1264236179284866091, 1.434547244040724534 ) ) ;
#39656 = CARTESIAN_POINT ( 'NONE',  ( -0.1574803149606299191, 0.1397637796350860440, 0.000000000000000000 ) ) ;
#39657 = CARTESIAN_POINT ( 'NONE',  ( -0.8759842519685039353, -0.1787899950787401882, 1.119586614119464585 ) ) ;
#39658 = CARTESIAN_POINT ( 'NONE',  ( -0.7646288533564489232, -0.1113553986120547346, 0.1919291338582677087 ) ) ;
#39659 = ORIENTED_EDGE ( 'NONE', *, *, #11323, .T. ) ;
#39660 = CARTESIAN_POINT ( 'NONE',  ( -0.9500414927467377701, -0.1787899950787401604, 1.156496062938362046 ) ) ;
#39661 = AXIS2_PLACEMENT_3D ( 'NONE', #10676, #47322, #556 ) ;
#39662 = CARTESIAN_POINT ( 'NONE',  ( -0.8759842519685039353, 0.1787899950787401882, 0.2337598424659216578 ) ) ;
#39663 = LINE ( 'NONE', #33002, #30559 ) ;
#39664 = CARTESIAN_POINT ( 'NONE',  ( -1.094772975963752103E-17, -0.8136082201977422601, -0.1787899950787401882 ) ) ;
#39665 = VERTEX_POINT ( 'NONE', #266 ) ;
#39666 = CARTESIAN_POINT ( 'NONE',  ( -0.8107537697050254399, 0.1574803149606300301, 0.06151574803149608556 ) ) ;
#39667 = CARTESIAN_POINT ( 'NONE',  ( 0.1264236179284866091, 0.1323818898175431191, 0.1264236179284866091 ) ) ;
#39668 = AXIS2_PLACEMENT_3D ( 'NONE', #32066, #46654, #5469 ) ;
#39669 = VERTEX_POINT ( 'NONE', #3873 ) ;
#39670 = CARTESIAN_POINT ( 'NONE',  ( -1.033464566929133799, 0.000000000000000000, 1.742125984251968518 ) ) ;
#39671 = CARTESIAN_POINT ( 'NONE',  ( 0.2204724409448818867, -0.07955613945526357478, -0.1377952755905511861 ) ) ;
#39672 = CIRCLE ( 'NONE', #34370, 0.7874015748031496509 ) ;
#39673 = CARTESIAN_POINT ( 'NONE',  ( -0.8019270111902717657, 0.1787899950787401604, 0.5856299212060785964 ) ) ;
#39674 = DIRECTION ( 'NONE',  ( -1.000000000000000000, 0.000000000000000000, 0.000000000000000000 ) ) ;
#39675 = ORIENTED_EDGE ( 'NONE', *, *, #31027, .F. ) ;
#39676 = CARTESIAN_POINT ( 'NONE',  ( -1.002407869896990045, 0.1264236179284866091, 1.803641732229700700 ) ) ;
#39677 = CARTESIAN_POINT ( 'NONE',  ( 0.001443311806748592266, -0.02661417251542722018, -0.1377865128822150786 ) ) ;
#39678 = ORIENTED_EDGE ( 'NONE', *, *, #20409, .T. ) ;
#39679 = CARTESIAN_POINT ( 'NONE',  ( -1.100456976456230270E-17, -0.7982721560397381122, -0.1797182628040039365 ) ) ;
#39680 = CARTESIAN_POINT ( 'NONE',  ( 1.033464566929134687, 0.06523048226347956391, 0.6323818896562525271 ) ) ;
#39681 = CARTESIAN_POINT ( 'NONE',  ( -0.8107537697050253289, 0.1574803149606300301, 1.350885826664126821 ) ) ;
#39682 = EDGE_CURVE ( 'NONE', #8568, #35682, #494, .T. ) ;
#39683 = CARTESIAN_POINT ( 'NONE',  ( 1.054774247047244540, 0.07405724077823318263, 0.7381889763241898939 ) ) ;
#39684 = CARTESIAN_POINT ( 'NONE',  ( -0.06523048226347956391, -0.5467519685039372579, -0.1574803149606300301 ) ) ;
#39685 = CARTESIAN_POINT ( 'NONE',  ( 0.7185039370078714072, 0.06523048226347728795, 1.631397637687748814 ) ) ;
#39686 = CARTESIAN_POINT ( 'NONE',  ( -0.2559055118110235005, 0.03992503320406630418, -0.03403288757427296030 ) ) ;
#39687 = CARTESIAN_POINT ( 'NONE',  ( 0.7185039370078746268, 0.06523048226347956391, 1.208169291338584417 ) ) ;
#39689 = CYLINDRICAL_SURFACE ( 'NONE', #36960, 0.02900000000000054270 ) ;
#39688 = CARTESIAN_POINT ( 'NONE',  ( 0.9653553125466671769, -0.1534803737003100077, 1.989856878449740352 ) ) ;
#39690 = CARTESIAN_POINT ( 'NONE',  ( 0.9873396505805591694, -0.1113553986120547346, 1.737204724409448842 ) ) ;
#39691 = CARTESIAN_POINT ( 'NONE',  ( 0.06523048226347956391, -0.6205708660342047489, -0.1574803149606300301 ) ) ;
#39692 = ( BOUNDED_CURVE ( )  B_SPLINE_CURVE ( 2, ( #19070, #24340, #2739, #2048, #39397, #20954, #38720, #21193, #42298 ),
 .UNSPECIFIED., .F., .T. ) 
 B_SPLINE_CURVE_WITH_KNOTS ( ( 3, 2, 2, 2, 3 ),
 ( 0.8599999999999999867, 0.8625000000000000444, 0.8649999999999999911, 0.8675000000000000488, 0.8699999999999999956 ),
 .UNSPECIFIED. ) 
 CURVE ( )  GEOMETRIC_REPRESENTATION_ITEM ( )  RATIONAL_B_SPLINE_CURVE ( ( 1.000000000000000000, 0.9238795325112869605, 1.000000000000000000, 0.9238795325112869605, 1.000000000000000000, 0.9238795325112869605, 1.000000000000000000, 0.9238795325112869605, 1.000000000000000000 ) ) 
 REPRESENTATION_ITEM ( '' )  ) ;
#39693 = ADVANCED_FACE ( 'NONE', ( #21859 ), #38926, .T. ) ;
#39695 = CARTESIAN_POINT ( 'NONE',  ( 0.1279527559055118058, -0.2216206741968047289, -0.3149606299212598381 ) ) ;
#39694 = CARTESIAN_POINT ( 'NONE',  ( 0.8019270111902716547, 0.1787899950787401604, 0.7037401574265510495 ) ) ;
#39696 = AXIS2_PLACEMENT_3D ( 'NONE', #1038, #15696, #38184 ) ;
#39697 = DIRECTION ( 'NONE',  ( 0.000000000000000000, -1.000000000000000000, 0.000000000000000000 ) ) ;
#39698 = AXIS2_PLACEMENT_3D ( 'NONE', #37719, #4381, #12335 ) ;
#39699 = CARTESIAN_POINT ( 'NONE',  ( 0.9500414927467378812, -0.1787899950787401604, 0.9596456692375764375 ) ) ;
#39700 = DIRECTION ( 'NONE',  ( 0.000000000000000000, -0.6156614753256566264, -0.7880107536067233465 ) ) ;
#39701 = CARTESIAN_POINT ( 'NONE',  ( -0.07444174185955065859, 0.08509398569254496281, 0.1797182628040039087 ) ) ;
#39702 = CARTESIAN_POINT ( 'NONE',  ( -0.07405724077823318263, -1.179133858213953001, 0.1787899950787401604 ) ) ;
#39704 = CIRCLE ( 'NONE', #45833, 0.09842519685039370636 ) ;
#39703 = CARTESIAN_POINT ( 'NONE',  ( 0.06523048226347956391, -1.590059055118110187, 0.1574803149606297803 ) ) ;
#39705 = CARTESIAN_POINT ( 'NONE',  ( 1.229559056033039366E-16, -0.0009842519685041700977, 0.3937007874015748254 ) ) ;
#39706 = EDGE_CURVE ( 'NONE', #25443, #31526, #970, .T. ) ;
#39707 = EDGE_LOOP ( 'NONE', ( #28830, #7786, #36660, #37073 ) ) ;
#39708 = CARTESIAN_POINT ( 'NONE',  ( -0.6971942568897626646, 0.07405724077823318263, 0.03937007868639404856 ) ) ;
#39709 = VERTEX_POINT ( 'NONE', #40042 ) ;
#39710 = VECTOR ( 'NONE', #401, 39.37007874015748143 ) ;
#39711 = CARTESIAN_POINT ( 'NONE',  ( 0.7495606340400177148, -0.1264236179284866091, 1.980807086560409491 ) ) ;
#39712 = EDGE_LOOP ( 'NONE', ( #3225, #26283, #27160, #15303 ) ) ;
#39713 = CARTESIAN_POINT ( 'NONE',  ( -0.9500414927467377701, 0.1787899950787401604, 1.963582677111591401 ) ) ;
#39714 = CARTESIAN_POINT ( 'NONE',  ( -0.8019270111902717657, -0.1787899950787401604, 1.663385826717890925 ) ) ;
#39715 = CARTESIAN_POINT ( 'NONE',  ( 1.054774247047244540, 0.07405724077823318263, 0.8562992125446617919 ) ) ;
#39716 = CARTESIAN_POINT ( 'NONE',  ( -0.6971942568897637749, 2.189545951927499583E-17, 1.065452755851747924 ) ) ;
#39717 = DIRECTION ( 'NONE',  ( -0.000000000000000000, 1.000000000000000000, -0.000000000000000000 ) ) ;
#39718 = CARTESIAN_POINT ( 'NONE',  ( -0.8019270111902717657, -0.1787899950787401604, 1.865157480261195877 ) ) ;
#39719 = CARTESIAN_POINT ( 'NONE',  ( -0.8759842519685039353, -0.1574803149606299191, 1.968503937007874072 ) ) ;
#39720 = CARTESIAN_POINT ( 'NONE',  ( 0.2559049618366861512, 0.03677276663233821491, -0.03301314027812483204 ) ) ;
#39721 = CARTESIAN_POINT ( 'NONE',  ( -0.07405724077823318263, -0.4568168816150654510, -0.1787899950787401604 ) ) ;
#39722 = CARTESIAN_POINT ( 'NONE',  ( -0.1264082094504824783, -0.09842519685039370636, 0.1067823974213112231 ) ) ;
#39723 = DIRECTION ( 'NONE',  ( 1.822029033848725028E-16, 0.000000000000000000, 1.000000000000000000 ) ) ;
#39724 = CARTESIAN_POINT ( 'NONE',  ( -0.5555748031496030581, 1.061695335278756813, -0.02376411959061705201 ) ) ;
#39725 = CARTESIAN_POINT ( 'NONE',  ( -0.8759842519685039353, 0.1787899950787401882, 0.1500984251430870220 ) ) ;
#39727 = ORIENTED_EDGE ( 'NONE', *, *, #34580, .T. ) ;
#39726 = VECTOR ( 'NONE', #41205, 39.37007874015748143 ) ;
#39728 = ORIENTED_EDGE ( 'NONE', *, *, #33032, .F. ) ;
#39729 = CARTESIAN_POINT ( 'NONE',  ( -0.8019270111902716547, -0.1787899950787401604, 1.353346456639149986 ) ) ;
#39730 = ORIENTED_EDGE ( 'NONE', *, *, #36636, .F. ) ;
#39731 = EDGE_CURVE ( 'NONE', #33099, #21515, #43512, .T. ) ;
#39732 = CARTESIAN_POINT ( 'NONE',  ( -0.07405724077823318263, -1.218503936954111300, 0.1787899950787401604 ) ) ;
#39733 = CARTESIAN_POINT ( 'NONE',  ( -0.1787899950787401604, -1.415354330654897019, 0.07405724077823318263 ) ) ;
#39734 = CARTESIAN_POINT ( 'NONE',  ( 0.1602931993194442739, -0.07955613945526357478, -0.1377952755905511861 ) ) ;
#39735 = ( LENGTH_UNIT ( ) NAMED_UNIT ( * ) SI_UNIT ( $, .METRE. ) ) ;
#39736 = DIRECTION ( 'NONE',  ( 0.000000000000000000, 0.000000000000000000, 1.000000000000000000 ) ) ;
#39737 = CARTESIAN_POINT ( 'NONE',  ( -0.7646288533564489232, -0.1113553986120547346, 0.9694881888688504645 ) ) ;
#39738 = CARTESIAN_POINT ( 'NONE',  ( -1.033464566929134687, 0.06523048226347956391, 0.9178149606299221830 ) ) ;
#39739 = EDGE_CURVE ( 'NONE', #45599, #5246, #44576, .T. ) ;
#39740 = CARTESIAN_POINT ( 'NONE',  ( 0.7495606340400177148, 0.1264236179284866091, 0.4355314960092284138 ) ) ;
#39741 = CARTESIAN_POINT ( 'NONE',  ( 0.1574803149606300301, -0.1678149606299212671, 0.06523048226347956391 ) ) ;
#39742 = CARTESIAN_POINT ( 'NONE',  ( 0.8759842519685039353, -0.1574803149606299191, 1.761811023514519459 ) ) ;
#39743 = ORIENTED_EDGE ( 'NONE', *, *, #13233, .F. ) ;
#39744 = DIRECTION ( 'NONE',  ( 0.000000000000000000, 0.000000000000000000, 1.000000000000000000 ) ) ;
#39745 = CARTESIAN_POINT ( 'NONE',  ( 0.9412147342319837628, -0.1574803149606297803, 0.8686023622047237547 ) ) ;
#39746 = CARTESIAN_POINT ( 'NONE',  ( 1.033464566929133799, 0.000000000000000000, 0.4822834645669291653 ) ) ;
#39747 = PLANE ( 'NONE',  #26401 ) ;
#39749 = CARTESIAN_POINT ( 'NONE',  ( 0.1594510458733890690, -0.1460701887064284055, -0.02793386226024194632 ) ) ;
#39748 = FACE_OUTER_BOUND ( 'NONE', #1895, .T. ) ;
#39750 = CARTESIAN_POINT ( 'NONE',  ( 0.9873396505805591694, -0.1113553986120547346, 0.2312992124908980207 ) ) ;
#39751 = CARTESIAN_POINT ( 'NONE',  ( -0.07405724077823318263, -0.07185039364702389131, 0.1787899950787401604 ) ) ;
#39752 = CYLINDRICAL_SURFACE ( 'NONE', #42454, 0.1673228346456687721 ) ;
#39753 = CARTESIAN_POINT ( 'NONE',  ( 0.1113553986120547346, -1.528543306979086358, -0.1113553986120547346 ) ) ;
#39754 = CARTESIAN_POINT ( 'NONE',  ( 3.284318927891251994E-17, -0.7436023621509606496, 0.1787899950787401882 ) ) ;
#39755 = CARTESIAN_POINT ( 'NONE',  ( -0.06523048226347956391, -1.083169291338583529, 0.1574803149606297803 ) ) ;
#39756 = CARTESIAN_POINT ( 'NONE',  ( 0.7185039370078746268, -0.06523048226347956391, 0.9670275589475911815 ) ) ;
#39757 = CONICAL_SURFACE ( 'NONE', #6863, 0.09842519685039317900, 0.7853981633972921816 ) ;
#39758 = CARTESIAN_POINT ( 'NONE',  ( -1.054774247047244540, -0.07405724077823318263, 0.4527559054580477249 ) ) ;
#39759 = ORIENTED_EDGE ( 'NONE', *, *, #19315, .T. ) ;
#39760 = EDGE_LOOP ( 'NONE', ( #4394, #24964, #4642, #23244, #24057, #18367, #10235, #43739 ) ) ;
#39761 = CARTESIAN_POINT ( 'NONE',  ( -0.6971942568897648851, -0.07405724077823297447, 1.624015747977732849 ) ) ;
#39762 = VERTEX_POINT ( 'NONE', #25930 ) ;
#39763 = CARTESIAN_POINT ( 'NONE',  ( 0.7495606340400177148, 0.1264236179284866091, 1.616633858213952779 ) ) ;
#39764 = VERTEX_POINT ( 'NONE', #40742 ) ;
#39765 = CARTESIAN_POINT ( 'NONE',  ( 0.1574803149606300301, -1.260334645561765221, 0.06523048226347956391 ) ) ;
#39766 = CARTESIAN_POINT ( 'NONE',  ( -1.054774247047244540, 0.07405724077823318263, 0.7775590550643479704 ) ) ;
#39767 = CARTESIAN_POINT ( 'NONE',  ( 1.054774247047244540, -0.07405724077823318263, 0.1427165353793072855 ) ) ;
#39768 = CARTESIAN_POINT ( 'NONE',  ( -0.8107537697050254399, 0.1574803149606300301, 0.2583661417322834497 ) ) ;
#39769 = CARTESIAN_POINT ( 'NONE',  ( 0.8759842519685039353, 0.1787899950787401882, 0.7849409448281259305 ) ) ;
#39770 = CARTESIAN_POINT ( 'NONE',  ( -1.002407869896990045, -0.1264236179284866091, 0.6471456692375747721 ) ) ;
#39771 = CIRCLE ( 'NONE', #11520, 0.1013779527559039162 ) ;
#39772 = FACE_OUTER_BOUND ( 'NONE', #46037, .T. ) ;
#39773 = FACE_OUTER_BOUND ( 'NONE', #43513, .T. ) ;
#39774 = CARTESIAN_POINT ( 'NONE',  ( 0.06523048226347956391, -0.1628937006798744369, 0.1574803149606297803 ) ) ;
#39775 = CARTESIAN_POINT ( 'NONE',  ( -0.6971942568897637749, 2.189545951927499583E-17, 1.464074803095842370 ) ) ;
#39776 = CARTESIAN_POINT ( 'NONE',  ( -0.7646288533564489232, 0.1113553986120547346, 1.520669291338582640 ) ) ;
#39777 = CARTESIAN_POINT ( 'NONE',  ( -1.033464566929133799, 0.000000000000000000, 0.4429133858267716439 ) ) ;
#39778 = CARTESIAN_POINT ( 'NONE',  ( 1.054774247047244096, 0.000000000000000000, 1.444389763725763665 ) ) ;
#39779 = CARTESIAN_POINT ( 'NONE',  ( -0.08758009603785964214, -0.09851383865516692706, -0.1629933310116103984 ) ) ;
#39780 = CARTESIAN_POINT ( 'NONE',  ( -0.3161444924769509779, 0.4457451269443606368, -1.671447902550282194 ) ) ;
#39781 = ORIENTED_EDGE ( 'NONE', *, *, #7511, .F. ) ;
#39782 = CARTESIAN_POINT ( 'NONE',  ( -0.07405724077823318263, -1.677289322559946116, -0.1787899950787401604 ) ) ;
#39783 = VERTEX_POINT ( 'NONE', #40511 ) ;
#39784 = EDGE_LOOP ( 'NONE', ( #41433, #6470, #6607, #17883 ) ) ;
#39785 = EDGE_CURVE ( 'NONE', #1000, #11821, #7938, .T. ) ;
#39786 = DIRECTION ( 'NONE',  ( 1.000000000000000000, 0.000000000000000000, 0.000000000000000000 ) ) ;
#39787 = ADVANCED_FACE ( 'NONE', ( #24174 ), #44277, .T. ) ;
#39788 = CARTESIAN_POINT ( 'NONE',  ( 0.1787899950787401882, -0.8863188975840314843, -2.189545951927503898E-17 ) ) ;
#39789 = AXIS2_PLACEMENT_3D ( 'NONE', #39421, #6358, #43257 ) ;
#39790 = CARTESIAN_POINT ( 'NONE',  ( -0.2471922899045395083, -0.07845124750587918749, -0.07638293795139619591 ) ) ;
#39791 = CARTESIAN_POINT ( 'NONE',  ( 0.000000000000000000, 0.000000000000000000, -0.2610569382242185488 ) ) ;
#39792 = ( CONVERSION_BASED_UNIT ( 'INCH', #28592 ) LENGTH_UNIT ( ) NAMED_UNIT ( #1983 ) ) ;
#39793 = CARTESIAN_POINT ( 'NONE',  ( 0.7495606340400177148, -0.1264236179284866091, 0.2829724408911185041 ) ) ;
#39794 = CARTESIAN_POINT ( 'NONE',  ( -0.07444174185955065859, -0.2052603450161165910, -0.1797182628040039087 ) ) ;
#39795 = EDGE_CURVE ( 'NONE', #16297, #17977, #22858, .T. ) ;
#39796 = CARTESIAN_POINT ( 'NONE',  ( -0.1264236179284866091, -0.1000255430323883782, -0.1264236179284866091 ) ) ;
#39797 = CARTESIAN_POINT ( 'NONE',  ( -0.1264236179284866091, 0.06840551186478720236, -0.1264236179284866091 ) ) ;
#39798 = CARTESIAN_POINT ( 'NONE',  ( 0.2471922026429001218, -0.09209855619650188230, -0.04265916557990739183 ) ) ;
#39799 = EDGE_CURVE ( 'NONE', #4833, #44905, #40447, .T. ) ;
#39800 = CARTESIAN_POINT ( 'NONE',  ( 1.054774247047244540, 0.07405724077823318263, 0.6151574802611965431 ) ) ;
#39801 = AXIS2_PLACEMENT_3D ( 'NONE', #30115, #23117, #29647 ) ;
#39802 = ( BOUNDED_CURVE ( )  B_SPLINE_CURVE ( 2, ( #31798, #35385, #16922, #20515, #31564, #47091, #35150, #24131, #39183 ),
 .UNSPECIFIED., .F., .T. ) 
 B_SPLINE_CURVE_WITH_KNOTS ( ( 3, 2, 2, 2, 3 ),
 ( 0.01000000000000000021, 0.01250000000000000069, 0.01499999999999999944, 0.01750000000000000167, 0.02000000000000000042 ),
 .UNSPECIFIED. ) 
 CURVE ( )  GEOMETRIC_REPRESENTATION_ITEM ( )  RATIONAL_B_SPLINE_CURVE ( ( 1.000000000000000000, 0.9238795325112869605, 1.000000000000000000, 0.9238795325112869605, 1.000000000000000000, 0.9238795325112869605, 1.000000000000000000, 0.9238795325112869605, 1.000000000000000000 ) ) 
 REPRESENTATION_ITEM ( '' )  ) ;
#39803 = CARTESIAN_POINT ( 'NONE',  ( -0.7495606340400177148, 0.1264236179284866091, 0.9079724408911180600 ) ) ;
#39805 = DIRECTION ( 'NONE',  ( 0.000000000000000000, 0.000000000000000000, -1.000000000000000000 ) ) ;
#39804 = CARTESIAN_POINT ( 'NONE',  ( 0.3000685424736224127, 4.466152701071653354E-17, 0.000000000000000000 ) ) ;
#39806 = CARTESIAN_POINT ( 'NONE',  ( 0.07444174185955046430, -1.706244596984621387, -0.1797182628040039087 ) ) ;
#39807 = CARTESIAN_POINT ( 'NONE',  ( 0.8759842519685039353, -0.1574803149606299191, 1.692913385826771533 ) ) ;
#39808 = CARTESIAN_POINT ( 'NONE',  ( 0.9500414927467378812, -0.1787899950787401604, 1.633858267662771313 ) ) ;
#39810 = CARTESIAN_POINT ( 'NONE',  ( 0.2559055118110236116, 0.07425961573522271708, -0.3088661881183391578 ) ) ;
#39809 = CARTESIAN_POINT ( 'NONE',  ( -0.1572356565282391760, -0.09317336072449060314, 0.1946530291195329998 ) ) ;
#39811 = ORIENTED_EDGE ( 'NONE', *, *, #254, .T. ) ;
#39812 = CARTESIAN_POINT ( 'NONE',  ( 0.7185039370078739607, 1.928577636452523993E-17, 0.02952755905511811330 ) ) ;
#39813 = CYLINDRICAL_SURFACE ( 'NONE', #19835, 0.2952755905511806334 ) ;
#39814 = CARTESIAN_POINT ( 'NONE',  ( -0.07405724077823318263, -0.1555118109698585271, 0.1787899950787401604 ) ) ;
#39815 = CARTESIAN_POINT ( 'NONE',  ( -0.8759842519685039353, 0.1787899950787401882, 0.4306102361667086820 ) ) ;
#39816 = CARTESIAN_POINT ( 'NONE',  ( 1.002407869896990045, 0.1264236179284866091, 0.6176181101824566033 ) ) ;
#39817 = CARTESIAN_POINT ( 'NONE',  ( -0.07405724077823318263, -1.070866141678519456, -0.1787899950787401604 ) ) ;
#39818 = CARTESIAN_POINT ( 'NONE',  ( 0.7495606340400177148, 0.1264236179284866091, 0.1599409448281264023 ) ) ;
#39819 = CARTESIAN_POINT ( 'NONE',  ( -1.033464566929134687, -0.06523048226347956391, 1.532972440837355066 ) ) ;
#39820 = CARTESIAN_POINT ( 'NONE',  ( 0.8759842519685039353, -0.1787899950787401882, 0.5634842519147401640 ) ) ;
#39821 = CARTESIAN_POINT ( 'NONE',  ( -1.054774247047244540, 0.07405724077823318263, 1.638779527505292988 ) ) ;
#39822 = EDGE_LOOP ( 'NONE', ( #29068, #13733, #46491, #31581 ) ) ;
#39823 = CARTESIAN_POINT ( 'NONE',  ( -0.6971942568897648851, -0.07405724077823297447, 1.151574803095843036 ) ) ;
#39824 = CARTESIAN_POINT ( 'NONE',  ( -0.2664910633248679939, -0.1585270522231942703, -0.8213382201702412733 ) ) ;
#39825 = CARTESIAN_POINT ( 'NONE',  ( 0.6971942568897648851, 0.07405724077823318263, 1.225393700733637514 ) ) ;
#39826 = CARTESIAN_POINT ( 'NONE',  ( -0.7185039370078746268, 0.06523048226347956391, 0.7258858266641259327 ) ) ;
#39827 = CARTESIAN_POINT ( 'NONE',  ( 0.000000000000000000, -0.09842519685039370636, 0.1574803149606299191 ) ) ;
#39828 = CARTESIAN_POINT ( 'NONE',  ( 0.7495606340400177148, 0.1264236179284866091, 1.887303149552535420 ) ) ;
#39829 = CARTESIAN_POINT ( 'NONE',  ( -0.9412147342319837628, -0.1574803149606297803, 0.5930118110236219930 ) ) ;
#39830 = CARTESIAN_POINT ( 'NONE',  ( -0.8759842519685039353, 0.1787899950787401882, 0.8587598424659212970 ) ) ;
#39831 = CARTESIAN_POINT ( 'NONE',  ( -0.1642836037694702656, -0.2006450494026624509, -0.03472289316814061721 ) ) ;
#39832 = CARTESIAN_POINT ( 'NONE',  ( 0.8019270111902716547, 0.1787899950787401604, 0.2362204723871814682 ) ) ;
#39833 = CARTESIAN_POINT ( 'NONE',  ( -0.8019270111902716547, 0.1787899950787401604, 0.2312992125446618197 ) ) ;
#39834 = UNCERTAINTY_MEASURE_WITH_UNIT (LENGTH_MEASURE( 1.000000000000000082E-05 ), #9122, 'distance_accuracy_value', 'NONE') ;
#39835 = CARTESIAN_POINT ( 'NONE',  ( -0.6971942568897637749, 2.189545951927499583E-17, 0.7111220471903307860 ) ) ;
#39836 = CARTESIAN_POINT ( 'NONE',  ( 0.8759842519685039353, -0.1574803149606299191, 1.604330708553889595 ) ) ;
#39837 = VERTEX_POINT ( 'NONE', #38775 ) ;
#39838 = ( BOUNDED_CURVE ( )  B_SPLINE_CURVE ( 2, ( #17143, #6819, #42993, #24807, #2748, #46838, #43718, #13551, #20961 ),
 .UNSPECIFIED., .F., .T. ) 
 B_SPLINE_CURVE_WITH_KNOTS ( ( 3, 2, 2, 2, 3 ),
 ( 0.9799999999999999822, 0.9825000000000000400, 0.9849999999999999867, 0.9875000000000000444, 0.9899999999999999911 ),
 .UNSPECIFIED. ) 
 CURVE ( )  GEOMETRIC_REPRESENTATION_ITEM ( )  RATIONAL_B_SPLINE_CURVE ( ( 1.000000000000000000, 0.9238795325112869605, 1.000000000000000000, 0.9238795325112869605, 1.000000000000000000, 0.9238795325112869605, 1.000000000000000000, 0.9238795325112869605, 1.000000000000000000 ) ) 
 REPRESENTATION_ITEM ( '' )  ) ;
#39839 = VECTOR ( 'NONE', #30613, 39.37007874015748143 ) ;
#39840 = CARTESIAN_POINT ( 'NONE',  ( -0.07405724077823318263, 0.001968503990771401039, 0.1787899950787401604 ) ) ;
#39841 = CARTESIAN_POINT ( 'NONE',  ( 1.054774247047244540, 0.07405724077823318263, 0.8562992125446617919 ) ) ;
#39842 = CARTESIAN_POINT ( 'NONE',  ( 0.6971942568897648851, 0.07405724077823318263, 0.9891732282926936071 ) ) ;
#39843 = CARTESIAN_POINT ( 'NONE',  ( -0.8019270111902716547, 0.1787899950787401604, 1.806102362150961094 ) ) ;
#39844 = VECTOR ( 'NONE', #37486, 39.37007874015748143 ) ;
#39845 = CARTESIAN_POINT ( 'NONE',  ( 0.9500414927467378812, -0.1787899950787401604, 1.904527559001354398 ) ) ;
#39846 = CIRCLE ( 'NONE', #26087, 0.09842519685039370636 ) ;
#39847 = ORIENTED_EDGE ( 'NONE', *, *, #1349, .F. ) ;
#39848 = CARTESIAN_POINT ( 'NONE',  ( 1.033464566929134687, 0.06523048226347956391, 1.311515748031496509 ) ) ;
#39849 = CARTESIAN_POINT ( 'NONE',  ( -0.07405724077823318263, -1.322958613898530533, -0.1787899950787401604 ) ) ;
#39850 = ORIENTED_EDGE ( 'NONE', *, *, #35976, .F. ) ;
#39851 = CARTESIAN_POINT ( 'NONE',  ( 0.1787899950787401604, -0.2539370078202523584, -0.07405724077823318263 ) ) ;
#39852 = VERTEX_POINT ( 'NONE', #10014 ) ;
#39853 = CARTESIAN_POINT ( 'NONE',  ( 0.9500414927467378812, 0.1787899950787401604, 1.210629921206079818 ) ) ;
#39854 = FACE_OUTER_BOUND ( 'NONE', #24256, .T. ) ;
#39855 = CARTESIAN_POINT ( 'NONE',  ( -0.2471886260750748299, -0.05069887331258201429, 0.1203475566276436537 ) ) ;
#39856 = ADVANCED_FACE ( 'NONE', ( #6403 ), #31373, .T. ) ;
#39857 = CARTESIAN_POINT ( 'NONE',  ( 0.9412147342319837628, -0.1574803149606297803, 1.931594488188976166 ) ) ;
#39858 = CARTESIAN_POINT ( 'NONE',  ( 0.07405724077823318263, -1.567913385773008095, 0.1787899950787401604 ) ) ;
#39859 = CARTESIAN_POINT ( 'NONE',  ( 0.07405724077823318263, -0.7411417322297018107, 0.1787899950787401604 ) ) ;
#39860 = EDGE_CURVE ( 'NONE', #16170, #43692, #45033, .T. ) ;
#39861 = CARTESIAN_POINT ( 'NONE',  ( -0.8019270111902716547, -0.1787899950787401604, 0.4872047243556847929 ) ) ;
#39862 = CARTESIAN_POINT ( 'NONE',  ( 1.033464566929133799, 0.000000000000000000, 0.9448818896562519720 ) ) ;
#39864 = CARTESIAN_POINT ( 'NONE',  ( -0.7226522770000863849, -0.06944897243561021227, 1.984602698732675918 ) ) ;
#39863 = CARTESIAN_POINT ( 'NONE',  ( 0.1797182628040039087, -1.283016250527927893, 0.07444174185955046430 ) ) ;
#39865 = LINE ( 'NONE', #7054, #46233 ) ;
#39866 = CARTESIAN_POINT ( 'NONE',  ( 1.054774247047244096, 0.000000000000000000, 1.247539370024976391 ) ) ;
#39867 = CARTESIAN_POINT ( 'NONE',  ( 0.9500414927467377701, -0.1787899950787401604, 1.747047244040724312 ) ) ;
#39868 = AXIS2_PLACEMENT_3D ( 'NONE', #29446, #33956, #12616 ) ;
#39869 = VECTOR ( 'NONE', #38029, 39.37007874015748143 ) ;
#39870 = CARTESIAN_POINT ( 'NONE',  ( -0.9873396505805591694, 0.1113553986120547346, 1.904527559055118280 ) ) ;
#39871 = CARTESIAN_POINT ( 'NONE',  ( 0.1586958850898451678, 0.05525856355904548017, 0.1377952755905512694 ) ) ;
#39872 = CIRCLE ( 'NONE', #26884, 0.1574803149606299191 ) ;
#39873 = CARTESIAN_POINT ( 'NONE',  ( 0.1555687797274980522, -0.05303742630350904985, -0.1377952755905511861 ) ) ;
#39874 = CARTESIAN_POINT ( 'NONE',  ( -0.9412147342319837628, -0.1574803149606297803, 1.764271653435779630 ) ) ;
#39875 = CARTESIAN_POINT ( 'NONE',  ( -0.1787899950787401882, -0.0004921259304884630223, 0.000000000000000000 ) ) ;
#39876 = CARTESIAN_POINT ( 'NONE',  ( 0.6971942568897626646, 0.07405724077823318263, 0.2362204723871814960 ) ) ;
#39877 = CARTESIAN_POINT ( 'NONE',  ( 0.7020737121823690252, 0.02867620229676474952, 0.03937008399637639128 ) ) ;
#39879 = DIRECTION ( 'NONE',  ( 0.000000000000000000, 0.000000000000000000, -1.000000000000000000 ) ) ;
#39878 = CARTESIAN_POINT ( 'NONE',  ( 0.8019270111902716547, 0.1787899950787401604, 1.097440944828127041 ) ) ;
#39880 = CARTESIAN_POINT ( 'NONE',  ( 0.8107537697050254399, -0.1574803149606297803, 1.218011811023622437 ) ) ;
#39881 = CARTESIAN_POINT ( 'NONE',  ( -1.054774247047244540, 0.07405724077823318263, 1.166338582623402509 ) ) ;
#39882 = CARTESIAN_POINT ( 'NONE',  ( 0.7646288533564489232, -0.1113553986120547346, 0.4183070865066456645 ) ) ;
#39883 = EDGE_LOOP ( 'NONE', ( #17649, #11595, #625, #12374 ) ) ;
#39884 = SURFACE_SIDE_STYLE ('',( #39178 ) ) ;
#39885 = ORIENTED_EDGE ( 'NONE', *, *, #34576, .T. ) ;
#39886 = CARTESIAN_POINT ( 'NONE',  ( -0.7185039370078746268, 0.06523048226347956391, 0.3715551180027090727 ) ) ;
#39887 = ORIENTED_EDGE ( 'NONE', *, *, #22296, .T. ) ;
#39888 = CARTESIAN_POINT ( 'NONE',  ( 0.8019270111902717657, 0.1787899950787401604, 1.491141732229701367 ) ) ;
#39889 = CARTESIAN_POINT ( 'NONE',  ( -0.7185039370078746268, -0.06523048226347956391, 1.134350393700787052 ) ) ;
#39890 = LINE ( 'NONE', #1526, #47253 ) ;
#39892 = CARTESIAN_POINT ( 'NONE',  ( -1.033464566929133799, 0.000000000000000000, 1.387795275590551158 ) ) ;
#39891 = CARTESIAN_POINT ( 'NONE',  ( -0.7185039370078739607, 1.928577636452523993E-17, 1.761811023622047223 ) ) ;
#39893 = CARTESIAN_POINT ( 'NONE',  ( 1.033464566929134687, -0.06523048226347956391, 1.188484251968505268 ) ) ;
#39894 = CARTESIAN_POINT ( 'NONE',  ( 0.1787899950787401604, 0.01673228351833043817, 0.07405724077823318263 ) ) ;
#39895 = ORIENTED_EDGE ( 'NONE', *, *, #24562, .T. ) ;
#39896 = CARTESIAN_POINT ( 'NONE',  ( 0.1564216623530368111, -8.910440797025414093E-13, -0.1403857474672218497 ) ) ;
#39897 = ORIENTED_EDGE ( 'NONE', *, *, #21866, .F. ) ;
#39898 = CARTESIAN_POINT ( 'NONE',  ( 0.8107537697050254399, -0.1574803149606297803, 0.5093503937007877180 ) ) ;
#39899 = CARTESIAN_POINT ( 'NONE',  ( 0.8019270111902717657, -0.1787899950787401604, 0.5265748030958428139 ) ) ;
#39900 = ORIENTED_EDGE ( 'NONE', *, *, #11434, .T. ) ;
#39901 = CARTESIAN_POINT ( 'NONE',  ( -0.1787899950787401604, -1.813976377898992354, 0.07405724077823318263 ) ) ;
#39902 = CARTESIAN_POINT ( 'NONE',  ( -0.7495606340400177148, 0.1264236179284866091, 1.065452755851747924 ) ) ;
#39903 = CARTESIAN_POINT ( 'NONE',  ( -0.8759842519685039353, -0.1574803149606299191, 0.1574803149606299191 ) ) ;
#39904 = ORIENTED_EDGE ( 'NONE', *, *, #7679, .F. ) ;
#39905 = CARTESIAN_POINT ( 'NONE',  ( -0.8019270111902716547, -0.1787899950787401604, 1.033464566875371027 ) ) ;
#39906 = CARTESIAN_POINT ( 'NONE',  ( -1.054774247047244096, 0.000000000000000000, 0.7750984251430865779 ) ) ;
#39907 = CARTESIAN_POINT ( 'NONE',  ( -1.054774247047244540, -0.07405724077823318263, 0.1820866141194649179 ) ) ;
#39908 = FACE_OUTER_BOUND ( 'NONE', #34275, .T. ) ;
#39909 = CARTESIAN_POINT ( 'NONE',  ( -0.1787899950787401604, -0.8062263304339631897, -0.07405724077823318263 ) ) ;
#39910 = ORIENTED_EDGE ( 'NONE', *, *, #41961, .F. ) ;
#39911 = CARTESIAN_POINT ( 'NONE',  ( -0.1694227370586289527, -0.08956103987234979857, 0.004342192889647520510 ) ) ;
#39912 = CARTESIAN_POINT ( 'NONE',  ( -0.1586641775163213364, 2.177585298233989164, -4.122948637049707266 ) ) ;
#39913 = VERTEX_POINT ( 'NONE', #42357 ) ;
#39914 = ORIENTED_EDGE ( 'NONE', *, *, #35611, .F. ) ;
#39915 = CARTESIAN_POINT ( 'NONE',  ( -0.8759842519685039353, -0.1574803149606299191, 0.3444881888688507976 ) ) ;
#39916 = AXIS2_PLACEMENT_3D ( 'NONE', #43391, #29075, #25693 ) ;
#39917 = CONICAL_SURFACE ( 'NONE', #25407, 0.09842519685039370636, 0.9599310885968824758 ) ;
#39918 = DIRECTION ( 'NONE',  ( 2.943801717310650128E-16, -1.000000000000000000, -2.355041373848520102E-15 ) ) ;
#39919 = CARTESIAN_POINT ( 'NONE',  ( -1.002407869896990045, -0.1264236179284866091, 0.8046259841982047467 ) ) ;
#39920 = DIRECTION ( 'NONE',  ( 0.000000000000000000, 0.000000000000000000, 1.000000000000000000 ) ) ;
#39921 = ADVANCED_FACE ( 'NONE', ( #34962 ), #23035, .T. ) ;
#39922 = CARTESIAN_POINT ( 'NONE',  ( -1.002407869896990045, -0.1264236179284866091, 1.793799212544661348 ) ) ;
#39923 = ADVANCED_FACE ( 'NONE', ( #41201 ), #12931, .T. ) ;
#39924 = CARTESIAN_POINT ( 'NONE',  ( -1.033464566929133799, 0.000000000000000000, 1.141732283357039357 ) ) ;
#39925 = CARTESIAN_POINT ( 'NONE',  ( -0.8759842519685039353, -0.1787899950787401882, 0.09596456687537047170 ) ) ;
#39926 = CARTESIAN_POINT ( 'NONE',  ( 0.7185039370078739607, 1.928577636452523993E-17, 0.6200787401574803237 ) ) ;
#39927 = CARTESIAN_POINT ( 'NONE',  ( 0.1270800023317771588, -0.8819335733625728313, -0.1270800023317771588 ) ) ;
#39928 = CARTESIAN_POINT ( 'NONE',  ( 0.000000000000000000, 0.000000000000000000, -0.3149606299212598381 ) ) ;
#39929 = CARTESIAN_POINT ( 'NONE',  ( -0.8759842519685039353, -0.1574803149606299191, 1.407480314853102321 ) ) ;
#39930 = CARTESIAN_POINT ( 'NONE',  ( 0.7495606340400177148, -0.1264236179284866091, 0.7209645668753701386 ) ) ;
#39931 = CARTESIAN_POINT ( 'NONE',  ( -0.1113553986120547346, -0.5442913385826771977, -0.1113553986120547346 ) ) ;
#39932 = CARTESIAN_POINT ( 'NONE',  ( -0.1635024568870425687, 0.1266995851085641056, 0.01633969686776765365 ) ) ;
#39933 = CARTESIAN_POINT ( 'NONE',  ( -0.2559055118110235560, 0.08195668352890772557, -0.05483160856164565750 ) ) ;
#39934 = VECTOR ( 'NONE', #20611, 39.37007874015748143 ) ;
#39935 = CARTESIAN_POINT ( 'NONE',  ( 0.8759842519685039353, 0.1574803149606299191, 1.318897637795275690 ) ) ;
#39937 = DIRECTION ( 'NONE',  ( 0.000000000000000000, 0.000000000000000000, 1.000000000000000000 ) ) ;
#39936 = CARTESIAN_POINT ( 'NONE',  ( 0.9320460955907311495, -0.1671224838594336515, 1.989197504597622679 ) ) ;
#39938 = CARTESIAN_POINT ( 'NONE',  ( 0.8107537697050254399, -0.1574803149606297803, 1.483759842412158747 ) ) ;
#39940 = LINE ( 'NONE', #6645, #40680 ) ;
#39939 = CARTESIAN_POINT ( 'NONE',  ( 0.8019270111902716547, -0.1787899950787401604, 0.7185039369541108556 ) ) ;
#39941 = DIRECTION ( 'NONE',  ( -1.000000000000000000, 3.469446951953626022E-15, 0.000000000000000000 ) ) ;
#39942 = DIRECTION ( 'NONE',  ( 1.822029033848725028E-16, 0.000000000000000000, 1.000000000000000000 ) ) ;
#39943 = VECTOR ( 'NONE', #20883, 39.37007874015748143 ) ;
#39945 = CARTESIAN_POINT ( 'NONE',  ( 0.1582007246420325530, 0.03721045995875260637, -0.1404371117717378159 ) ) ;
#39944 = VECTOR ( 'NONE', #35783, 39.37007874015748143 ) ;
#39946 = CARTESIAN_POINT ( 'NONE',  ( 1.054774247047244540, 0.07405724077823318263, 0.9301181101824563813 ) ) ;
#39947 = DIRECTION ( 'NONE',  ( 0.000000000000000000, 0.000000000000000000, -1.000000000000000000 ) ) ;
#39948 = CARTESIAN_POINT ( 'NONE',  ( -0.1264236179284866091, -1.142224409395055096, 0.1264236179284866091 ) ) ;
#39949 = PLANE ( 'NONE',  #34457 ) ;
#39950 = CARTESIAN_POINT ( 'NONE',  ( -0.7495606340400177148, -0.1264236179284866091, 0.1648622046706460786 ) ) ;
#39951 = AXIS2_PLACEMENT_3D ( 'NONE', #12862, #27495, #42046 ) ;
#39952 = CARTESIAN_POINT ( 'NONE',  ( 0.8759842519685039353, 0.1787899950787401882, 1.966043307032850462 ) ) ;
#39953 = CARTESIAN_POINT ( 'NONE',  ( 0.1113553986120547346, -0.3179133857192444901, 0.1113553986120547346 ) ) ;
#39954 = CARTESIAN_POINT ( 'NONE',  ( -1.054774247047244096, 0.000000000000000000, 1.956200787347811110 ) ) ;
#39955 = CARTESIAN_POINT ( 'NONE',  ( -0.8019270111902717657, 0.1787899950787401604, 1.727362204670645385 ) ) ;
#39956 = CARTESIAN_POINT ( 'NONE',  ( -1.002407869896990045, -0.1264236179284866091, 1.080216535379306952 ) ) ;
#39957 = CARTESIAN_POINT ( 'NONE',  ( -1.054774247047244540, 0.07405724077823318263, 0.4232283464029293896 ) ) ;
#39958 = CYLINDRICAL_SURFACE ( 'NONE', #27618, 0.1574803149606299191 ) ;
#39959 = CARTESIAN_POINT ( 'NONE',  ( 0.1644020957507537628, 0.08115590401245550978, 0.1405661490837558925 ) ) ;
#39960 = CARTESIAN_POINT ( 'NONE',  ( -0.8759842519685039353, 0.1574803149606299191, 1.909448818897637956 ) ) ;
#39961 = CARTESIAN_POINT ( 'NONE',  ( -0.2927386332256519674, 0.1025512834716172661, -0.7433308942907063122 ) ) ;
#39962 = CARTESIAN_POINT ( 'NONE',  ( 0.1264236179284866091, -0.4740412910638843180, 0.1264236179284866091 ) ) ;
#39963 = EDGE_CURVE ( 'NONE', #29530, #28079, #29794, .T. ) ;
#39964 = CARTESIAN_POINT ( 'NONE',  ( 0.02595745220638724302, -0.09842519685039370636, 0.1523733382129854319 ) ) ;
#39965 = CARTESIAN_POINT ( 'NONE',  ( -0.1574803149606299191, 0.2573565155132531146, -0.3015174453633728269 ) ) ;
#39966 = CARTESIAN_POINT ( 'NONE',  ( -0.2066929133858267931, -0.4933358210236690744, -0.8766136318131756422 ) ) ;
#39967 = CARTESIAN_POINT ( 'NONE',  ( -0.8759842519685039353, -0.1787899950787401882, 0.2091535432533232486 ) ) ;
#39968 = ADVANCED_FACE ( 'NONE', ( #12923 ), #16009, .T. ) ;
#39969 = VERTEX_POINT ( 'NONE', #16966 ) ;
#39970 = VERTEX_POINT ( 'NONE', #45705 ) ;
#39971 = CARTESIAN_POINT ( 'NONE',  ( -0.8759842519685039353, -0.1787899950787401882, 1.355807086560409491 ) ) ;
#39972 = VERTEX_POINT ( 'NONE', #6166 ) ;
#39973 = EDGE_CURVE ( 'NONE', #38848, #11301, #19813, .T. ) ;
#39974 = CARTESIAN_POINT ( 'NONE',  ( 0.07405724077823318263, -1.238188976324190005, -0.1787899950787401604 ) ) ;
#39975 = CARTESIAN_POINT ( 'NONE',  ( -1.094772975963752103E-17, -1.309547244040724312, -0.1787899950787401882 ) ) ;
#39976 = DIRECTION ( 'NONE',  ( 0.000000000000000000, 1.000000000000000000, 0.000000000000000000 ) ) ;
#39977 = CARTESIAN_POINT ( 'NONE',  ( -0.7135826771653542844, 0.9842519685039370358, 1.971200000000000075E-07 ) ) ;
#39978 = CARTESIAN_POINT ( 'NONE',  ( -0.07444174185955065859, -0.6235674316302897147, 0.1797182628040039087 ) ) ;
#39979 = CARTESIAN_POINT ( 'NONE',  ( 0.4208034506101054895, 4.466152701071653354E-17, 0.000000000000000000 ) ) ;
#39980 = CARTESIAN_POINT ( 'NONE',  ( -0.7185039370078746268, 0.06523048226347956391, 0.8833661416247557963 ) ) ;
#39981 = AXIS2_PLACEMENT_3D ( 'NONE', #36243, #42673, #24729 ) ;
#39982 = CARTESIAN_POINT ( 'NONE',  ( 1.054774247047244540, 0.07405724077823318263, 0.4232283464029293896 ) ) ;
#39983 = CARTESIAN_POINT ( 'NONE',  ( -0.1574803149606300301, -0.1875000000000000000, -0.06523048226347956391 ) ) ;
#39984 = CARTESIAN_POINT ( 'NONE',  ( 0.9873396505805591694, -0.1113553986120547346, 1.766732283357039135 ) ) ;
#39985 = EDGE_LOOP ( 'NONE', ( #10816, #41864, #34392, #45620, #17153, #15425 ) ) ;
#39986 = LINE ( 'NONE', #3810, #19229 ) ;
#39987 = CARTESIAN_POINT ( 'NONE',  ( 0.8107537697050253289, -0.1574803149606297803, 0.7455708661417325134 ) ) ;
#39988 = DIRECTION ( 'NONE',  ( 0.7071067811865450192, 0.7071067811865500152, 0.000000000000000000 ) ) ;
#39990 = CARTESIAN_POINT ( 'NONE',  ( -1.033464566929133799, 0.000000000000000000, 0.8366141732283465249 ) ) ;
#39989 = LINE ( 'NONE', #17728, #27085 ) ;
#39991 = CARTESIAN_POINT ( 'NONE',  ( 1.033464566929134687, -0.06523048226347956391, 0.2337598424121580809 ) ) ;
#39992 = ORIENTED_EDGE ( 'NONE', *, *, #34580, .F. ) ;
#39993 = ORIENTED_EDGE ( 'NONE', *, *, #16256, .F. ) ;
#39994 = CARTESIAN_POINT ( 'NONE',  ( 0.8107537697050254399, 0.1574803149606300301, 1.902066929026330566 ) ) ;
#39995 = CARTESIAN_POINT ( 'NONE',  ( -0.1113553986120547346, -1.587598425089322696, 0.1113553986120547346 ) ) ;
#39996 = CARTESIAN_POINT ( 'NONE',  ( 0.07405724077823318263, -0.7263779527021420046, -0.1787899950787401604 ) ) ;
#39997 = CARTESIAN_POINT ( 'NONE',  ( -0.9873396505805591694, 0.1113553986120547346, 0.04429133847515007855 ) ) ;
#39998 = CARTESIAN_POINT ( 'NONE',  ( -0.1574803149606300301, -1.132381889763780070, -0.06523048226347956391 ) ) ;
#39999 = CARTESIAN_POINT ( 'NONE',  ( 0.7185039370078739607, 1.928577636452523993E-17, 0.9251968502861732668 ) ) ;
#40000 = LINE ( 'NONE', #32386, #2995 ) ;
#40001 = CONICAL_SURFACE ( 'NONE', #18574, 0.1574803149606299191, 0.9599310885968735940 ) ;
#40002 = CARTESIAN_POINT ( 'NONE',  ( -1.002407869896990045, -0.1264236179284866091, 0.3715551180564728440 ) ) ;
#40003 = VERTEX_POINT ( 'NONE', #39229 ) ;
#40004 = ORIENTED_EDGE ( 'NONE', *, *, #32279, .T. ) ;
#40005 = CARTESIAN_POINT ( 'NONE',  ( -0.6971942568897648851, 0.07405724077823318263, 1.619094488135213838 ) ) ;
#40006 = CARTESIAN_POINT ( 'NONE',  ( 1.002407869896990045, -0.1264236179284866091, 1.518208661363559031 ) ) ;
#40007 = ORIENTED_EDGE ( 'NONE', *, *, #24677, .F. ) ;
#40008 = CARTESIAN_POINT ( 'NONE',  ( -1.054774247047244540, 0.07405724077823318263, 0.7381889763241898939 ) ) ;
#40009 = DIRECTION ( 'NONE',  ( 1.000000000000000000, -3.469446951953614978E-15, -1.144917494144692929E-16 ) ) ;
#40010 = CARTESIAN_POINT ( 'NONE',  ( 0.8019270111902716547, -0.1787899950787401604, 0.7234251967966300878 ) ) ;
#40011 = CARTESIAN_POINT ( 'NONE',  ( -1.054774247047244096, 0.000000000000000000, 0.6914370078202519698 ) ) ;
#40012 = CARTESIAN_POINT ( 'NONE',  ( 0.06523048226347956391, -0.06938976367200050399, -0.1574803149606300301 ) ) ;
#40013 = LINE ( 'NONE', #3125, #45873 ) ;
#40014 = CARTESIAN_POINT ( 'NONE',  ( -0.1113553986120547346, -0.1309055117034966520, 0.1113553986120547346 ) ) ;
#40015 = CARTESIAN_POINT ( 'NONE',  ( -1.033464566929134687, -0.06523048226347956391, 1.847933070758615015 ) ) ;
#40016 = ORIENTED_EDGE ( 'NONE', *, *, #26374, .T. ) ;
#40017 = DIRECTION ( 'NONE',  ( 1.000000000000000000, 0.000000000000000000, -1.822029033848725275E-16 ) ) ;
#40018 = CARTESIAN_POINT ( 'NONE',  ( -0.8107537697050253289, 0.1574803149606300301, 1.478838582677164615 ) ) ;
#40019 = CYLINDRICAL_SURFACE ( 'NONE', #39633, 0.09842519685039370636 ) ;
#40020 = ADVANCED_FACE ( 'NONE', ( #35663 ), #17430, .T. ) ;
#40021 = CARTESIAN_POINT ( 'NONE',  ( -0.1128178969825543304, -0.09851383988190079433, -0.1443091522045568953 ) ) ;
#40022 = CARTESIAN_POINT ( 'NONE',  ( -0.2824199087359778870, 1.411419074098322346, -0.2911036367043326467 ) ) ;
#40023 = ADVANCED_FACE ( 'NONE', ( #27553 ), #45792, .T. ) ;
#40024 = VERTEX_POINT ( 'NONE', #32556 ) ;
#40025 = CARTESIAN_POINT ( 'NONE',  ( -0.07405724077823318263, -1.662525543032388420, 0.1787899950787401604 ) ) ;
#40026 = ORIENTED_EDGE ( 'NONE', *, *, #37378, .T. ) ;
#40027 = ORIENTED_EDGE ( 'NONE', *, *, #37607, .T. ) ;
#40028 = EDGE_CURVE ( 'NONE', #31809, #10459, #16331, .T. ) ;
#40029 = CARTESIAN_POINT ( 'NONE',  ( -0.1264236179284866091, -0.3941929133320630219, 0.1264236179284866091 ) ) ;
#40030 = CARTESIAN_POINT ( 'NONE',  ( 0.07405724077823318263, -0.9330708660879686311, 0.1787899950787401604 ) ) ;
#40031 = CARTESIAN_POINT ( 'NONE',  ( -0.2471922963015220076, -0.09312803950196824054, -0.03901180619694211843 ) ) ;
#40032 = ( LENGTH_UNIT ( ) NAMED_UNIT ( * ) SI_UNIT ( $, .METRE. ) ) ;
#40033 = CARTESIAN_POINT ( 'NONE',  ( 1.002407869896990045, 0.1264236179284866091, 1.719980314906866203 ) ) ;
#40034 = CARTESIAN_POINT ( 'NONE',  ( 0.9500414927467378812, -0.1787899950787401604, 0.2509842519147403861 ) ) ;
#40035 = CARTESIAN_POINT ( 'NONE',  ( 0.07444174185955046430, -0.1314414473783210302, -0.1797182628040039087 ) ) ;
#40036 = AXIS2_PLACEMENT_3D ( 'NONE', #25863, #903, #40213 ) ;
#40037 = CARTESIAN_POINT ( 'NONE',  ( -0.1264236179284866091, -0.09018302334734902559, 0.1264236179284866091 ) ) ;
#40038 = CARTESIAN_POINT ( 'NONE',  ( 0.1787899950787401604, -0.2982283464029296116, 0.07405724077823318263 ) ) ;
#40039 = CARTESIAN_POINT ( 'NONE',  ( 0.6971942568897626646, -0.07405724077823297447, 0.6348425196312760255 ) ) ;
#40041 = CARTESIAN_POINT ( 'NONE',  ( 0.7185039370078692977, 0.06523048226347515077, 1.710137795168064079 ) ) ;
#40040 = CARTESIAN_POINT ( 'NONE',  ( -1.034367163161600489, 0.01381456667479016159, 0.03937007874015843734 ) ) ;
#40042 = CARTESIAN_POINT ( 'NONE',  ( 0.000000000000000000, 0.3883517482604934012, -0.6419475548153109612 ) ) ;
#40043 = CARTESIAN_POINT ( 'NONE',  ( 1.033464566929134687, -0.06523048226347956391, 1.700295275590550936 ) ) ;
#40044 = CARTESIAN_POINT ( 'NONE',  ( 0.7495606340400177148, 0.1264236179284866091, 1.616633858213952779 ) ) ;
#40046 = CARTESIAN_POINT ( 'NONE',  ( 0.4151545546392377273, 4.766607801171850497E-17, 0.000000000000000000 ) ) ;
#40045 = CARTESIAN_POINT ( 'NONE',  ( -0.1377952755905509641, 1.687505431895957030E-17, -0.06545654452343109553 ) ) ;
#40047 = ORIENTED_EDGE ( 'NONE', *, *, #17793, .T. ) ;
#40048 = FACE_OUTER_BOUND ( 'NONE', #45140, .T. ) ;
#40049 = CARTESIAN_POINT ( 'NONE',  ( 0.9412147342319837628, -0.1574803149606297803, 1.331200787294047672 ) ) ;
#40050 = CARTESIAN_POINT ( 'NONE',  ( 0.1787899950787401882, -0.2219488188438744347, -2.189545951927503898E-17 ) ) ;
#40052 = CARTESIAN_POINT ( 'NONE',  ( 0.1582120475477748200, 0.1029568672337303342, 0.1025480767803373799 ) ) ;
#40051 = CARTESIAN_POINT ( 'NONE',  ( -1.054774247047244540, -0.07405724077823318263, 0.4576771653005669016 ) ) ;
#40053 = CARTESIAN_POINT ( 'NONE',  ( -0.07405724077823318263, -1.110236220418677533, -0.1787899950787401604 ) ) ;
#40054 = CARTESIAN_POINT ( 'NONE',  ( 1.054774247047244096, 0.000000000000000000, 0.06643700782025216411 ) ) ;
#40055 = DIRECTION ( 'NONE',  ( 0.000000000000000000, -0.7880107536067184615, 0.6156614753256628436 ) ) ;
#40056 = CARTESIAN_POINT ( 'NONE',  ( 0.9500414927467377701, -0.1787899950787401604, 0.5659448818360001132 ) ) ;
#40057 = CARTESIAN_POINT ( 'NONE',  ( -0.7495606340400177148, -0.1264236179284866091, 1.621555118056472455 ) ) ;
#40058 = ORIENTED_EDGE ( 'NONE', *, *, #37106, .F. ) ;
#40059 = CARTESIAN_POINT ( 'NONE',  ( -0.6971942568897648851, -0.07405724077823297447, 1.190944881836001112 ) ) ;
#40060 = CARTESIAN_POINT ( 'NONE',  ( 1.033464566929133799, 0.000000000000000000, 0.4429133858267716439 ) ) ;
#40061 = ( REPRESENTATION_RELATIONSHIP ('NONE','NONE', #9609, #45408 ) REPRESENTATION_RELATIONSHIP_WITH_TRANSFORMATION ( #28599 )SHAPE_REPRESENTATION_RELATIONSHIP( ) ) ;
#40062 = CARTESIAN_POINT ( 'NONE',  ( 0.9500414927467378812, 0.1787899950787401604, 1.097440944828127041 ) ) ;
#40063 = CARTESIAN_POINT ( 'NONE',  ( -0.1574803149606300301, -1.122539369971214063, -0.06523048226347956391 ) ) ;
#40064 = CARTESIAN_POINT ( 'NONE',  ( 1.002407869896990045, -0.1264236179284866091, 1.788877952702141672 ) ) ;
#40065 = CARTESIAN_POINT ( 'NONE',  ( -0.8107537697050253289, -0.1574803149606297803, 0.5487204724409447953 ) ) ;
#40066 = CARTESIAN_POINT ( 'NONE',  ( -0.8019270111902717657, -0.1787899950787401604, 1.112204724355684959 ) ) ;
#40067 = EDGE_CURVE ( 'NONE', #40994, #31847, #12973, .T. ) ;
#40068 = CARTESIAN_POINT ( 'NONE',  ( 0.1864803149606299171, 0.5288907983920102529, -0.7507079620615728643 ) ) ;
#40069 = CARTESIAN_POINT ( 'NONE',  ( -1.033464566929133799, 1.928577636452524610E-17, 2.869337061179095023E-17 ) ) ;
#40070 = CARTESIAN_POINT ( 'NONE',  ( 1.054774247047244096, 0.000000000000000000, 0.3813976377415121966 ) ) ;
#40071 = CARTESIAN_POINT ( 'NONE',  ( -0.7495606340400177148, -0.1264236179284866091, 0.1648622046706460786 ) ) ;
#40072 = CARTESIAN_POINT ( 'NONE',  ( -0.9500414927467378812, -0.1787899950787401604, 0.7627952755367881643 ) ) ;
#40073 = CARTESIAN_POINT ( 'NONE',  ( 0.9412147342319837628, 0.1574803149606300301, 1.503444881782235232 ) ) ;
#40074 = VERTEX_POINT ( 'NONE', #45887 ) ;
#40075 = ADVANCED_FACE ( 'NONE', ( #24566 ), #38719, .T. ) ;
#40076 = CARTESIAN_POINT ( 'NONE',  ( -0.07405724077823318263, -0.03740157474938609478, 0.1787899950787401604 ) ) ;
#40077 = ORIENTED_EDGE ( 'NONE', *, *, #20714, .T. ) ;
#40078 = CARTESIAN_POINT ( 'NONE',  ( 0.6971942568897626646, 0.07405724077823318263, 0.8710629920722218200 ) ) ;
#40079 = EDGE_CURVE ( 'NONE', #23379, #23076, #34663, .T. ) ;
#40080 = CARTESIAN_POINT ( 'NONE',  ( 0.6971942568897648851, 0.07405724077823318263, 1.028543307032851573 ) ) ;
#40081 = CARTESIAN_POINT ( 'NONE',  ( -0.9500414927467377701, -0.1787899950787401604, 1.786417322780882388 ) ) ;
#40082 = CARTESIAN_POINT ( 'NONE',  ( 1.002407869896990045, -0.1264236179284866091, 1.867618110182456714 ) ) ;
#40083 = CARTESIAN_POINT ( 'NONE',  ( 0.4330708661417291827, 1.006139616066731278E-16, 1.186023622047243986 ) ) ;
#40084 = CARTESIAN_POINT ( 'NONE',  ( -0.1264236179284866091, -1.271285385552072933, 0.1264236179284866091 ) ) ;
#40085 = CIRCLE ( 'NONE', #37819, 0.009842519685039371677 ) ;
#40086 = VERTEX_POINT ( 'NONE', #31547 ) ;
#40087 = CARTESIAN_POINT ( 'NONE',  ( -0.1787899950787401604, -0.3179133857730082058, -0.07405724077823318263 ) ) ;
#40088 = CARTESIAN_POINT ( 'NONE',  ( -0.2741503469832764495, -0.1449524958156370724, 0.7917101702132945951 ) ) ;
#40089 = VERTEX_POINT ( 'NONE', #1811 ) ;
#40090 = CARTESIAN_POINT ( 'NONE',  ( 1.054774247047244540, 0.07405724077823318263, 1.245078740103716886 ) ) ;
#40091 = LINE ( 'NONE', #46581, #24945 ) ;
#40092 = CARTESIAN_POINT ( 'NONE',  ( 0.8759842519685039353, 0.1574803149606299191, 1.387795275483023616 ) ) ;
#40093 = ( BOUNDED_CURVE ( )  B_SPLINE_CURVE ( 2, ( #31042, #19517, #4895, #41291, #20220, #41060, #45137, #30121, #8732 ),
 .UNSPECIFIED., .F., .F. ) 
 B_SPLINE_CURVE_WITH_KNOTS ( ( 3, 2, 2, 2, 3 ),
 ( 0.2099999999999999922, 0.2124999999999999944, 0.2149999999999999967, 0.2174999999999999989, 0.2200000000000000011 ),
 .UNSPECIFIED. ) 
 CURVE ( )  GEOMETRIC_REPRESENTATION_ITEM ( )  RATIONAL_B_SPLINE_CURVE ( ( 1.000000000000000000, 0.9238795325112869605, 1.000000000000000000, 0.9238795325112869605, 1.000000000000000000, 0.9238795325112869605, 1.000000000000000000, 0.9238795325112869605, 1.000000000000000000 ) ) 
 REPRESENTATION_ITEM ( '' )  ) ;
#40094 = CARTESIAN_POINT ( 'NONE',  ( 1.054774247047244540, 0.07405724077823318263, 1.520669291284818758 ) ) ;
#40095 = CARTESIAN_POINT ( 'NONE',  ( 1.002407869896990045, 0.1264236179284866091, 0.02706692908009476414 ) ) ;
#40096 = CARTESIAN_POINT ( 'NONE',  ( 0.1787899950787401604, -1.681102362150960650, 0.07405724077823318263 ) ) ;
#40097 = CARTESIAN_POINT ( 'NONE',  ( 0.07405724077823318263, -1.641732283410802573, 0.1787899950787401604 ) ) ;
#40098 = AXIS2_PLACEMENT_3D ( 'NONE', #1279, #26960, #19974 ) ;
#40099 = CARTESIAN_POINT ( 'NONE',  ( -0.8019270111902716547, 0.1787899950787401604, 0.5511811023084406402 ) ) ;
#40100 = CARTESIAN_POINT ( 'NONE',  ( -0.1730584022666810107, -0.09842519685039369248, -0.02721978519955341527 ) ) ;
#40102 = CARTESIAN_POINT ( 'NONE',  ( -0.7103445921227516946, 0.006968863322258890200, 1.983141774271510727 ) ) ;
#40101 = CARTESIAN_POINT ( 'NONE',  ( -0.1797182628040039087, -1.302701289898007042, -0.07444174185955065859 ) ) ;
#40103 = CARTESIAN_POINT ( 'NONE',  ( -0.7185039370078746268, 0.06523048226347956391, 1.208169291338584417 ) ) ;
#40104 = CARTESIAN_POINT ( 'NONE',  ( 1.002407869896990045, 0.1264236179284866091, 1.213090551127338435 ) ) ;
#40105 = CARTESIAN_POINT ( 'NONE',  ( 1.054774247047244540, 0.07405724077823318263, 1.717519684985606476 ) ) ;
#40106 = AXIS2_PLACEMENT_3D ( 'NONE', #17320, #21627, #3413 ) ;
#40107 = CARTESIAN_POINT ( 'NONE',  ( 0.8759842519685039353, 0.1574803149606299191, 1.505905511703495847 ) ) ;
#40108 = DIRECTION ( 'NONE',  ( 0.000000000000000000, 1.000000000000000000, 0.000000000000000000 ) ) ;
#40109 = CARTESIAN_POINT ( 'NONE',  ( -0.2362204724409468770, 2.422684756221292845E-15, 1.186023622047244208 ) ) ;
#40110 = CARTESIAN_POINT ( 'NONE',  ( -1.033464566929134687, -0.06523048226347956391, 1.031003937007875182 ) ) ;
#40111 = CARTESIAN_POINT ( 'NONE',  ( 0.1476377952755906220, -0.2142072668875215635, -1.269802121763611291 ) ) ;
#40113 = CARTESIAN_POINT ( 'NONE',  ( 0.8019270111902717657, 0.1787899950787401604, 0.1131889763241894359 ) ) ;
#40112 = ( BOUNDED_CURVE ( )  B_SPLINE_CURVE ( 2, ( #13848, #28982, #32324, #18157, #40175, #36609, #29235, #47392, #43541 ),
 .UNSPECIFIED., .F., .T. ) 
 B_SPLINE_CURVE_WITH_KNOTS ( ( 3, 2, 2, 2, 3 ),
 ( 0.2899999999999999800, 0.2924999999999999822, 0.2949999999999999845, 0.2974999999999999867, 0.2999999999999999889 ),
 .UNSPECIFIED. ) 
 CURVE ( )  GEOMETRIC_REPRESENTATION_ITEM ( )  RATIONAL_B_SPLINE_CURVE ( ( 1.000000000000000000, 0.9238795325112869605, 1.000000000000000000, 0.9238795325112869605, 1.000000000000000000, 0.9238795325112869605, 1.000000000000000000, 0.9238795325112869605, 1.000000000000000000 ) ) 
 REPRESENTATION_ITEM ( '' )  ) ;
#40114 = CARTESIAN_POINT ( 'NONE',  ( 0.7129069480552276961, -0.05209332317552755470, 0.03937008009371578687 ) ) ;
#40115 = CARTESIAN_POINT ( 'NONE',  ( -1.033464566929134687, -0.06523048226347956391, 0.5487204723334181411 ) ) ;
#40116 = CARTESIAN_POINT ( 'NONE',  ( 0.6195511811023624027, 0.9842519685039370358, -0.7135826771653542844 ) ) ;
#40117 = CARTESIAN_POINT ( 'NONE',  ( 0.8107537697050253289, -0.1574803149606297803, 0.5388779526483779003 ) ) ;
#40118 = ORIENTED_EDGE ( 'NONE', *, *, #37383, .T. ) ;
#40119 = VECTOR ( 'NONE', #22879, 39.37007874015748143 ) ;
#40120 = CARTESIAN_POINT ( 'NONE',  ( 0.8534778653333370269, 0.1744360945806266716, 0.03937047372765634795 ) ) ;
#40121 = CARTESIAN_POINT ( 'NONE',  ( 0.7646288533564489232, 0.1113553986120547346, 0.8415354329633386588 ) ) ;
#40122 = CARTESIAN_POINT ( 'NONE',  ( -0.9412147342319837628, 0.1574803149606300301, 0.4010826770578274081 ) ) ;
#40123 = CARTESIAN_POINT ( 'NONE',  ( 1.002407869896990045, -0.1264236179284866091, 1.473917322780881722 ) ) ;
#40124 = CARTESIAN_POINT ( 'NONE',  ( -0.8759842519685039353, 0.1574803149606299191, 1.161417322834645605 ) ) ;
#40125 = CARTESIAN_POINT ( 'NONE',  ( 0.8107537697050254399, 0.1574803149606300301, 1.911909448818897017 ) ) ;
#40126 = CARTESIAN_POINT ( 'NONE',  ( 3.284318927891251994E-17, -0.1087598424659214497, 0.1787899950787401882 ) ) ;
#40127 = ORIENTED_EDGE ( 'NONE', *, *, #12957, .T. ) ;
#40128 = CARTESIAN_POINT ( 'NONE',  ( 0.9412147342319837628, 0.1574803149606300301, 0.7258858267716534751 ) ) ;
#40129 = EDGE_CURVE ( 'NONE', #39970, #17877, #16449, .T. ) ;
#40130 = CARTESIAN_POINT ( 'NONE',  ( -0.1574803149606300301, 0.08809055118110237226, -0.06523048226347956391 ) ) ;
#40131 = DIRECTION ( 'NONE',  ( 0.000000000000000000, 0.000000000000000000, 1.000000000000000000 ) ) ;
#40132 = EDGE_LOOP ( 'NONE', ( #20686, #2259, #38918, #39454 ) ) ;
#40133 = CARTESIAN_POINT ( 'NONE',  ( 0.9500414927467378812, -0.1787899950787401604, 0.6102362204186774219 ) ) ;
#40135 = EDGE_CURVE ( 'NONE', #34093, #13680, #25149, .T. ) ;
#40134 = ORIENTED_EDGE ( 'NONE', *, *, #10077, .F. ) ;
#40136 = CARTESIAN_POINT ( 'NONE',  ( -0.1113553986120547346, 0.06594488199729076072, 0.1113553986120547346 ) ) ;
#40137 = CARTESIAN_POINT ( 'NONE',  ( -1.054774247047244540, 0.07405724077823318263, 1.171259842465921741 ) ) ;
#40138 = CARTESIAN_POINT ( 'NONE',  ( -0.6971942568897648851, -0.07405724077823297447, 1.028543307032851573 ) ) ;
#40139 = EDGE_CURVE ( 'NONE', #8724, #9638, #46125, .T. ) ;
#40140 = AXIS2_PLACEMENT_3D ( 'NONE', #18237, #43384, #22064 ) ;
#40141 = CARTESIAN_POINT ( 'NONE',  ( 0.7646288533564489232, -0.1113553986120547346, 1.638779527451527551 ) ) ;
#40142 = CARTESIAN_POINT ( 'NONE',  ( 0.1787899950787401604, -0.8997302674418365953, -0.07405724077823318263 ) ) ;
#40143 = ORIENTED_EDGE ( 'NONE', *, *, #13186, .F. ) ;
#40144 = LINE ( 'NONE', #42777, #22724 ) ;
#40145 = CARTESIAN_POINT ( 'NONE',  ( -0.1787899950787401882, 0.1569881890301415284, 0.000000000000000000 ) ) ;
#40146 = ORIENTED_EDGE ( 'NONE', *, *, #22825, .F. ) ;
#40147 = VECTOR ( 'NONE', #6139, 39.37007874015748143 ) ;
#40148 = AXIS2_PLACEMENT_3D ( 'NONE', #44688, #19549, #37769 ) ;
#40149 = VERTEX_POINT ( 'NONE', #17136 ) ;
#40150 = CARTESIAN_POINT ( 'NONE',  ( 1.054774247047244540, -0.07405724077823318263, 1.043307086560409269 ) ) ;
#40151 = FACE_OUTER_BOUND ( 'NONE', #8900, .T. ) ;
#40152 = CARTESIAN_POINT ( 'NONE',  ( -1.002407869896990045, -0.1264236179284866091, 0.7258858267178898149 ) ) ;
#40153 = ORIENTED_EDGE ( 'NONE', *, *, #28317, .F. ) ;
#40154 = CARTESIAN_POINT ( 'NONE',  ( -0.6971942568897648851, 0.07405724077823318263, 1.737204724355685626 ) ) ;
#40155 = ORIENTED_EDGE ( 'NONE', *, *, #10909, .F. ) ;
#40156 = CARTESIAN_POINT ( 'NONE',  ( 0.4151545546392377273, -0.09842519685039370636, 1.205361022782828805E-17 ) ) ;
#40157 = CARTESIAN_POINT ( 'NONE',  ( 1.033464566929134687, 0.06523048226347956391, 0.6815944881889761664 ) ) ;
#40158 = CARTESIAN_POINT ( 'NONE',  ( 0.07444174185955046430, -0.8401028647011551387, -0.1797182628040039087 ) ) ;
#40159 = CARTESIAN_POINT ( 'NONE',  ( -1.033464566929134687, 0.06523048226347956391, 0.3961614172153076763 ) ) ;
#40160 = CARTESIAN_POINT ( 'NONE',  ( -1.033464566929134687, -0.06523048226347956391, 1.454232283357038691 ) ) ;
#40161 = CARTESIAN_POINT ( 'NONE',  ( 0.6971942568897626646, 0.07405724077823318263, 0.7923228345919055560 ) ) ;
#40162 = CARTESIAN_POINT ( 'NONE',  ( 0.2471922904502826812, 0.08969147984773637172, -0.05033842647028097250 ) ) ;
#40163 = DIRECTION ( 'NONE',  ( -1.000000000000000000, 0.000000000000000000, 0.000000000000000000 ) ) ;
#40164 = CARTESIAN_POINT ( 'NONE',  ( 0.8107537697050253289, 0.1574803149606300301, 1.478838582677164615 ) ) ;
#40166 = CARTESIAN_POINT ( 'NONE',  ( 0.000000000000000000, 0.000000000000000000, -0.1321438491773566926 ) ) ;
#40165 = CARTESIAN_POINT ( 'NONE',  ( 0.8170104114768506065, -0.1622629120985071838, 1.987100449027034088 ) ) ;
#40167 = CARTESIAN_POINT ( 'NONE',  ( 0.7185039370078778465, -0.06523048226348396317, 1.478838582569639071 ) ) ;
#40168 = ORIENTED_EDGE ( 'NONE', *, *, #4049, .F. ) ;
#40170 = DIRECTION ( 'NONE',  ( -1.000000000000000000, 0.000000000000000000, 0.000000000000000000 ) ) ;
#40169 = CARTESIAN_POINT ( 'NONE',  ( 0.7495606340400177148, 0.1264236179284866091, 0.7849409448281259305 ) ) ;
#40172 = AXIS2_PLACEMENT_3D ( 'NONE', #12956, #20361, #28519 ) ;
#40171 = CARTESIAN_POINT ( 'NONE',  ( 0.1787899950787401604, -0.8051181101824581576, -0.07405724077823318263 ) ) ;
#40173 = FACE_OUTER_BOUND ( 'NONE', #3604, .T. ) ;
#40174 = VERTEX_POINT ( 'NONE', #13543 ) ;
#40175 = CARTESIAN_POINT ( 'NONE',  ( 0.8759842519685039353, -0.1574803149606299191, 0.6200787400499527813 ) ) ;
#40176 = VECTOR ( 'NONE', #3310, 39.37007874015748143 ) ;
#40177 = CARTESIAN_POINT ( 'NONE',  ( 0.6195511811023612925, 0.6529540528279703659, 0.4629603087243970849 ) ) ;
#40178 = CARTESIAN_POINT ( 'NONE',  ( 0.9500414927467378812, -0.1787899950787401604, 0.9990157479777320715 ) ) ;
#40179 = CARTESIAN_POINT ( 'NONE',  ( -0.8759842519685039353, 0.000000000000000000, 1.978346456692913646 ) ) ;
#40180 = CARTESIAN_POINT ( 'NONE',  ( 0.1574803149606299191, -1.543307086614173151, -1.928577636452523993E-17 ) ) ;
#40181 = CARTESIAN_POINT ( 'NONE',  ( 0.8759842519685039353, 0.1574803149606299191, 1.240157480314960647 ) ) ;
#40182 = EDGE_CURVE ( 'NONE', #44763, #15464, #31780, .T. ) ;
#40183 = ORIENTED_EDGE ( 'NONE', *, *, #44289, .T. ) ;
#40184 = CARTESIAN_POINT ( 'NONE',  ( -0.9500414927467378812, 0.1787899950787401604, 0.1476377952218271561 ) ) ;
#40185 = CARTESIAN_POINT ( 'NONE',  ( 0.5314960629921260393, 1.928577636452522761E-17, 5.000000000000000000 ) ) ;
#40186 = ORIENTED_EDGE ( 'NONE', *, *, #21920, .T. ) ;
#40187 = CARTESIAN_POINT ( 'NONE',  ( -0.1787899950787401604, -1.420275590497418250, 0.07405724077823318263 ) ) ;
#40188 = CARTESIAN_POINT ( 'NONE',  ( 0.8107537697050234415, -0.1574803149606297803, 0.3420275589475912370 ) ) ;
#40189 = CARTESIAN_POINT ( 'NONE',  ( -0.9500414927467378812, 0.1787899950787401604, 1.604330708607653921 ) ) ;
#40190 = EDGE_CURVE ( 'NONE', #37608, #33104, #14495, .T. ) ;
#40191 = CARTESIAN_POINT ( 'NONE',  ( -0.7495606340400177148, -0.1264236179284866091, 1.109744094434425232 ) ) ;
#40192 = CARTESIAN_POINT ( 'NONE',  ( -0.6971942568897637749, 2.189545951927499583E-17, 0.4404527558517480901 ) ) ;
#40193 = CARTESIAN_POINT ( 'NONE',  ( 0.03901279071809810040, -0.5708661417322835607, 1.713085361781127913 ) ) ;
#40194 = CARTESIAN_POINT ( 'NONE',  ( 0.7185039370078739607, 1.928577636452523993E-17, 0.9744094488188976833 ) ) ;
#40195 = CARTESIAN_POINT ( 'NONE',  ( -0.9873396505805591694, -0.1113553986120547346, 1.973425196850393970 ) ) ;
#40196 = CARTESIAN_POINT ( 'NONE',  ( 0.5962569168439626477, 0.09842519685039370636, 0.000000000000000000 ) ) ;
#40197 = CARTESIAN_POINT ( 'NONE',  ( -0.1787899950787401604, -0.4518956217725454416, -0.07405724077823318263 ) ) ;
#40198 = CARTESIAN_POINT ( 'NONE',  ( -0.08756112481127756308, -0.09842519685039370636, -0.1629625869553541495 ) ) ;
#40199 = DIRECTION ( 'NONE',  ( -1.000000000000000000, 0.000000000000000000, 0.000000000000000000 ) ) ;
#40200 = LINE ( 'NONE', #14362, #23446 ) ;
#40201 = CARTESIAN_POINT ( 'NONE',  ( -0.8759842519685039353, -0.1787899950787401882, 1.040846456639149764 ) ) ;
#40202 = VECTOR ( 'NONE', #33755, 39.37007874015748143 ) ;
#40203 = CARTESIAN_POINT ( 'NONE',  ( -1.002407869896990045, 0.1264236179284866091, 0.3420275590013546751 ) ) ;
#40204 = ORIENTED_EDGE ( 'NONE', *, *, #4131, .T. ) ;
#40205 = CARTESIAN_POINT ( 'NONE',  ( -0.7495606340400177148, -0.1264236179284866091, 1.311515747977732405 ) ) ;
#40206 = ORIENTED_EDGE ( 'NONE', *, *, #29050, .T. ) ;
#40207 = AXIS2_PLACEMENT_3D ( 'NONE', #42909, #31934, #28338 ) ;
#40208 = CARTESIAN_POINT ( 'NONE',  ( 0.1787899950787401604, -1.124999999946237228, -0.07405724077823318263 ) ) ;
#40209 = EDGE_CURVE ( 'NONE', #45828, #19233, #8043, .T. ) ;
#40210 = CARTESIAN_POINT ( 'NONE',  ( -0.1787899950787401604, -1.380905511757260173, -0.07405724077823318263 ) ) ;
#40211 = PLANE ( 'NONE',  #27889 ) ;
#40212 = CARTESIAN_POINT ( 'NONE',  ( 0.000000000000000000, 0.000000000000000000, 0.6196850393700787940 ) ) ;
#40213 = DIRECTION ( 'NONE',  ( 1.000000000000000000, 0.000000000000000000, -1.822029033848725275E-16 ) ) ;
#40214 = CARTESIAN_POINT ( 'NONE',  ( -1.033464566929134687, -0.06523048226347956391, 0.9817913384751510986 ) ) ;
#40215 = CARTESIAN_POINT ( 'NONE',  ( -0.1113553986120547346, -0.1899606299212598659, -0.1113553986120547346 ) ) ;
#40216 = EDGE_LOOP ( 'NONE', ( #41407, #4348, #35315, #45803 ) ) ;
#40217 = CARTESIAN_POINT ( 'NONE',  ( 0.8107537697050253289, -0.1574803149606297803, 1.838090551073574774 ) ) ;
#40218 = ORIENTED_EDGE ( 'NONE', *, *, #28266, .T. ) ;
#40219 = CARTESIAN_POINT ( 'NONE',  ( 0.3123359580052492146, -0.08090551181102362266, 1.098083891755157578E-17 ) ) ;
#40220 = CARTESIAN_POINT ( 'NONE',  ( 0.8107537697050253289, 0.1574803149606300301, 0.9670275590551186129 ) ) ;
#40221 = DIRECTION ( 'NONE',  ( -0.5735764363510518216, 0.8191520442889876907, 1.003171929053519693E-16 ) ) ;
#40223 = CARTESIAN_POINT ( 'NONE',  ( 1.033464566929133799, 0.000000000000000000, 0.7578740157480314821 ) ) ;
#40222 = CARTESIAN_POINT ( 'NONE',  ( 0.2395294000716133853, -0.1968503937007874127, -0.4921259842519685179 ) ) ;
#40224 = DIRECTION ( 'NONE',  ( 0.000000000000000000, -1.000000000000000000, 0.000000000000000000 ) ) ;
#40225 = EDGE_LOOP ( 'NONE', ( #41117, #42009, #23735, #6072 ) ) ;
#40226 = AXIS2_PLACEMENT_3D ( 'NONE', #6828, #39182, #47342 ) ;
#40227 = VERTEX_POINT ( 'NONE', #43468 ) ;
#40228 = DIRECTION ( 'NONE',  ( 0.000000000000000000, 0.000000000000000000, 1.000000000000000000 ) ) ;
#40229 = DIRECTION ( 'NONE',  ( 5.377642775528101993E-15, -1.000000000000000000, 0.000000000000000000 ) ) ;
#40230 = CARTESIAN_POINT ( 'NONE',  ( 3.284318927891251994E-17, -1.486712598371433103, 0.1787899950787401882 ) ) ;
#40231 = CARTESIAN_POINT ( 'NONE',  ( 0.1574803149606300301, -1.570374015640505938, -0.06523048226347956391 ) ) ;
#40232 = CARTESIAN_POINT ( 'NONE',  ( 0.07405724077823318263, -0.7805118109698575557, 0.1787899950787401604 ) ) ;
#40233 = FACE_OUTER_BOUND ( 'NONE', #2009, .T. ) ;
#40234 = EDGE_CURVE ( 'NONE', #36366, #35496, #9807, .T. ) ;
#40235 = CARTESIAN_POINT ( 'NONE',  ( -0.1113553986120547346, -1.056102362204724532, -0.1113553986120547346 ) ) ;
#40236 = CARTESIAN_POINT ( 'NONE',  ( 1.033464566929133799, 0.000000000000000000, 0.9842519683964094934 ) ) ;
#40237 = DIRECTION ( 'NONE',  ( 0.000000000000000000, 0.000000000000000000, -1.000000000000000000 ) ) ;
#40238 = EDGE_CURVE ( 'NONE', #15531, #40961, #25036, .T. ) ;
#40239 = CARTESIAN_POINT ( 'NONE',  ( -1.002407869896990045, -0.1264236179284866091, 0.3321850393163153226 ) ) ;
#40240 = EDGE_LOOP ( 'NONE', ( #13912, #4295, #32887, #24962 ) ) ;
#40241 = ORIENTED_EDGE ( 'NONE', *, *, #19179, .T. ) ;
#40242 = CARTESIAN_POINT ( 'NONE',  ( 0.8019270111902717657, -0.1787899950787401604, 1.747047244040724312 ) ) ;
#40243 = EDGE_LOOP ( 'NONE', ( #19398, #23221, #45968, #8927 ) ) ;
#40244 = TOROIDAL_SURFACE ( 'NONE', #18813, 0.2007874015748031815, 0.01968503937007873988 ) ;
#40245 = CARTESIAN_POINT ( 'NONE',  ( -1.002407869896990045, 0.1264236179284866091, 0.8587598424659212970 ) ) ;
#40246 = CARTESIAN_POINT ( 'NONE',  ( 1.054774247047244540, 0.07405724077823318263, 0.2657480314422993595 ) ) ;
#40247 = CARTESIAN_POINT ( 'NONE',  ( 0.8019270111902716547, 0.1787899950787401604, 0.7874015747493863238 ) ) ;
#40248 = CARTESIAN_POINT ( 'NONE',  ( -0.6971942568897648851, 0.07405724077823318263, 0.6692913385289143147 ) ) ;
#40249 = ADVANCED_FACE ( 'NONE', ( #21684 ), #1604, .F. ) ;
#40250 = LINE ( 'NONE', #21669, #18476 ) ;
#40251 = CARTESIAN_POINT ( 'NONE',  ( 1.033464566929134687, -0.06523048226347956391, 1.149114173228346969 ) ) ;
#40252 = CARTESIAN_POINT ( 'NONE',  ( -0.6971942568897637749, 2.189545951927499583E-17, 1.582185039316315045 ) ) ;
#40253 = CARTESIAN_POINT ( 'NONE',  ( -0.8759842519685039353, 0.1574803149606299191, 1.860236220364913207 ) ) ;
#40254 = VERTEX_POINT ( 'NONE', #17605 ) ;
#40255 = LINE ( 'NONE', #18694, #1400 ) ;
#40256 = CARTESIAN_POINT ( 'NONE',  ( 1.054774247047244540, -0.07405724077823318263, 1.441929133804504604 ) ) ;
#40257 = CARTESIAN_POINT ( 'NONE',  ( 0.06244570574875708824, -0.09851384119049862165, -0.1836092180619330883 ) ) ;
#40258 = DIRECTION ( 'NONE',  ( 0.000000000000000000, -1.000000000000000000, 0.000000000000000000 ) ) ;
#40259 = ORIENTED_EDGE ( 'NONE', *, *, #21093, .F. ) ;
#40260 = ORIENTED_EDGE ( 'NONE', *, *, #2224, .F. ) ;
#40261 = CARTESIAN_POINT ( 'NONE',  ( -1.094772975963752103E-17, -0.6796259841982046357, -0.1787899950787401882 ) ) ;
#40262 = ORIENTED_EDGE ( 'NONE', *, *, #11700, .T. ) ;
#40263 = CYLINDRICAL_SURFACE ( 'NONE', #36883, 0.009842519685039376881 ) ;
#40264 = EDGE_CURVE ( 'NONE', #37935, #29837, #21432, .T. ) ;
#40265 = CARTESIAN_POINT ( 'NONE',  ( -0.1787899950787401882, -0.3991141731745826982, 0.000000000000000000 ) ) ;
#40266 = CARTESIAN_POINT ( 'NONE',  ( 0.1264236179284866091, -0.8420275590013542866, -0.1264236179284866091 ) ) ;
#40267 = EDGE_LOOP ( 'NONE', ( #31054, #45878, #40414, #44677, #21241, #30960 ) ) ;
#40268 = CARTESIAN_POINT ( 'NONE',  ( -0.2471911001155968346, -0.08911307781785425541, -0.05219320342745862457 ) ) ;
#40269 = ( NAMED_UNIT ( * ) SI_UNIT ( $, .STERADIAN. ) SOLID_ANGLE_UNIT ( ) ) ;
#40270 = CARTESIAN_POINT ( 'NONE',  ( 1.054774247047244540, -0.07405724077823318263, 1.712598425143087688 ) ) ;
#40271 = CARTESIAN_POINT ( 'NONE',  ( -1.100456976456230270E-17, -0.2470910536775338395, -0.1797182628040039365 ) ) ;
#40272 = CARTESIAN_POINT ( 'NONE',  ( 0.1264236179284866091, -0.1197105824024671250, 0.1264236179284866091 ) ) ;
#40273 = CARTESIAN_POINT ( 'NONE',  ( -0.07405724077823318263, -0.05216535427694517224, -0.1787899950787401604 ) ) ;
#40274 = CARTESIAN_POINT ( 'NONE',  ( 0.2759478392031617933, -0.09842519685039370636, 1.713085361781125915 ) ) ;
#40275 = CARTESIAN_POINT ( 'NONE',  ( 1.054774247047244540, 0.07405724077823318263, 0.6938976377415123631 ) ) ;
#40277 = CARTESIAN_POINT ( 'NONE',  ( 0.8107537697050254399, -0.1574803149606297803, 1.129429133750740277 ) ) ;
#40276 = CARTESIAN_POINT ( 'NONE',  ( -0.9707163768693443107, 0.1389002614476533559, 0.03937007874015844427 ) ) ;
#40278 = DIRECTION ( 'NONE',  ( 0.000000000000000000, 1.000000000000000000, 0.000000000000000000 ) ) ;
#40279 = CARTESIAN_POINT ( 'NONE',  ( -0.7185039370078739607, 0.000000000000000000, 4.498031496062992574 ) ) ;
#40280 = CARTESIAN_POINT ( 'NONE',  ( 1.054774247047244096, 0.000000000000000000, 1.838090551127338657 ) ) ;
#40282 = DIRECTION ( 'NONE',  ( 0.000000000000000000, -1.000000000000000000, 0.000000000000000000 ) ) ;
#40281 = CARTESIAN_POINT ( 'NONE',  ( -0.1898890638025484690, -0.07836638817766017340, 0.1758005714383346074 ) ) ;
#40283 = CARTESIAN_POINT ( 'NONE',  ( 1.002407869896990045, 0.1264236179284866091, 0.4995078739619842612 ) ) ;
#40284 = EDGE_CURVE ( 'NONE', #39322, #40321, #16775, .T. ) ;
#40285 = CARTESIAN_POINT ( 'NONE',  ( 0.1555213372790489601, -0.1336203177416374344, 0.04415337192907527186 ) ) ;
#40286 = CARTESIAN_POINT ( 'NONE',  ( 0.07405724077823318263, -0.2933070865604095467, -0.1787899950787401604 ) ) ;
#40288 = DIRECTION ( 'NONE',  ( -1.000000000000000000, 0.000000000000000000, 0.000000000000000000 ) ) ;
#40287 = CARTESIAN_POINT ( 'NONE',  ( -0.6971942568897626646, 0.07405724077823318263, 0.4379921259304882519 ) ) ;
#40289 = CARTESIAN_POINT ( 'NONE',  ( -0.1787899950787401604, -1.139763779473794925, 0.07405724077823318263 ) ) ;
#40290 = CARTESIAN_POINT ( 'NONE',  ( 0.8019270111902717657, 0.1787899950787401604, 0.1181102361667090567 ) ) ;
#40291 = EDGE_CURVE ( 'NONE', #44104, #10582, #36315, .T. ) ;
#40292 = CARTESIAN_POINT ( 'NONE',  ( -0.9500414927467378812, -0.1787899950787401604, 1.668307086560410157 ) ) ;
#40293 = ORIENTED_EDGE ( 'NONE', *, *, #26647, .T. ) ;
#40294 = CARTESIAN_POINT ( 'NONE',  ( -0.8019270111902717657, 0.1787899950787401604, 1.181102362150960428 ) ) ;
#40295 = CARTESIAN_POINT ( 'NONE',  ( -0.8759842519685039353, 0.1574803149606299191, 0.3346456692913385988 ) ) ;
#40296 = CARTESIAN_POINT ( 'NONE',  ( 0.8019270111902717657, -0.1787899950787401604, 1.195866141678520345 ) ) ;
#40297 = B_SPLINE_CURVE_WITH_KNOTS ( 'NONE', 3,
 ( #36575, #40839, #15021, #44211, #3966, #592, #30367, #3738, #7561, #14773, #15488, #30131, #18358 ),
 .UNSPECIFIED., .F., .F.,
 ( 4, 2, 2, 1, 2, 2, 4 ),
 ( 0.000000000000000000, 0.2499999999999984457, 0.3749999999999975020, 0.4374999999999972244, 0.4687499999999971134, 0.4999999999999971134, 1.000000000000000000 ),
 .UNSPECIFIED. ) ;
#40298 = CARTESIAN_POINT ( 'NONE',  ( 0.06523048226347956391, -1.186515747923968300, 0.1574803149606297803 ) ) ;
#40299 = CARTESIAN_POINT ( 'NONE',  ( 1.054774247047244540, -0.07405724077823318263, 1.988188976324187562 ) ) ;
#40300 = CARTESIAN_POINT ( 'NONE',  ( -0.7185039370078739607, 1.928577636452523993E-17, 0.5807086614173228023 ) ) ;
#40301 = CARTESIAN_POINT ( 'NONE',  ( -1.054774247047244096, 0.000000000000000000, 1.124507873961984261 ) ) ;
#40302 = CARTESIAN_POINT ( 'NONE',  ( 0.1564256176496426898, 0.1250799318563151907, -0.06412650594350359501 ) ) ;
#40303 = CARTESIAN_POINT ( 'NONE',  ( -0.08916369672655032053, -0.2440155479553919315, -0.03573910814353623705 ) ) ;
#40304 = CARTESIAN_POINT ( 'NONE',  ( 1.002407869896990045, 0.1264236179284866091, 0.2288385826234019815 ) ) ;
#40305 = CARTESIAN_POINT ( 'NONE',  ( -0.8759842519685039353, 0.1787899950787401882, 0.2288385826234019815 ) ) ;
#40306 = UNCERTAINTY_MEASURE_WITH_UNIT (LENGTH_MEASURE( 1.000000000000000082E-05 ), #1681, 'distance_accuracy_value', 'NONE') ;
#40307 = CARTESIAN_POINT ( 'NONE',  ( -0.6971942568897626646, 0.07405724077823318263, 0.7874015747493863238 ) ) ;
#40308 = ORIENTED_EDGE ( 'NONE', *, *, #960, .T. ) ;
#40309 = ADVANCED_FACE ( 'NONE', ( #7058 ), #14267, .T. ) ;
#40310 = PRODUCT_RELATED_PRODUCT_CATEGORY ( 'part', '', ( #29172 ) ) ;
#40311 = CARTESIAN_POINT ( 'NONE',  ( -1.094772975963752103E-17, -0.01525590545804752021, -0.1787899950787401882 ) ) ;
#40312 = CARTESIAN_POINT ( 'NONE',  ( 0.8019270111902717657, -0.1787899950787401604, 0.8021653542769460188 ) ) ;
#40313 = CARTESIAN_POINT ( 'NONE',  ( 1.054774247047244540, 0.07405724077823318263, 1.092519684985606032 ) ) ;
#40314 = CARTESIAN_POINT ( 'NONE',  ( -1.054774247047244096, 0.000000000000000000, 1.793799212544661348 ) ) ;
#40315 = EDGE_LOOP ( 'NONE', ( #13126, #25063, #35052 ) ) ;
#40316 = CARTESIAN_POINT ( 'NONE',  ( -0.7185039370078739607, 1.928577636452523993E-17, 1.594488188868850242 ) ) ;
#40317 = CARTESIAN_POINT ( 'NONE',  ( 3.284318927891251994E-17, -1.345104283189868299, 0.1787899950787401882 ) ) ;
#40318 = ORIENTED_EDGE ( 'NONE', *, *, #13085, .T. ) ;
#40319 = CARTESIAN_POINT ( 'NONE',  ( -0.1264236179284866091, -0.3203740156942680994, -0.1264236179284866091 ) ) ;
#40320 = CARTESIAN_POINT ( 'NONE',  ( -0.7185039370078739607, 1.928577636452523993E-17, 1.092519685039370136 ) ) ;
#40321 = VERTEX_POINT ( 'NONE', #32728 ) ;
#40322 = CARTESIAN_POINT ( 'NONE',  ( 0.6971942568897648851, 0.07405724077823318263, 1.259842519631276359 ) ) ;
#40323 = CARTESIAN_POINT ( 'NONE',  ( -0.1377952755905510751, 1.687505431895957647E-17, -0.3149606299212598381 ) ) ;
#40324 = DIRECTION ( 'NONE',  ( 0.000000000000000000, -9.251858538542971828E-16, 1.000000000000000000 ) ) ;
#40325 = AXIS2_PLACEMENT_3D ( 'NONE', #45083, #8924, #30301 ) ;
#40326 = CARTESIAN_POINT ( 'NONE',  ( 0.8759842519685039353, 0.1787899950787401882, 0.03198818892261445085 ) ) ;
#40327 = CARTESIAN_POINT ( 'NONE',  ( -0.1264236179284866091, -1.727854330654897685, 0.1264236179284866091 ) ) ;
#40328 = EDGE_CURVE ( 'NONE', #8597, #15230, #18326, .T. ) ;
#40329 = CARTESIAN_POINT ( 'NONE',  ( -0.6971942568897648851, -0.07405724077823297447, 0.4429133857730084833 ) ) ;
#40330 = CARTESIAN_POINT ( 'NONE',  ( 0.1797182628040039087, -1.479866644228716055, 0.07444174185955046430 ) ) ;
#40331 = CARTESIAN_POINT ( 'NONE',  ( 0.9412147342319837628, 0.1574803149606300301, 1.434547244094487972 ) ) ;
#40332 = CARTESIAN_POINT ( 'NONE',  ( 1.054774247047244096, 0.000000000000000000, 1.286909448765133801 ) ) ;
#40333 = CARTESIAN_POINT ( 'NONE',  ( 1.002407869896990045, 0.1264236179284866091, 1.641240157426551161 ) ) ;
#40334 = EDGE_CURVE ( 'NONE', #12322, #22163, #16334, .T. ) ;
#40335 = CARTESIAN_POINT ( 'NONE',  ( -1.033464566929136907, -0.06523048226347749612, 1.651082677057827519 ) ) ;
#40336 = DIRECTION ( 'NONE',  ( 0.000000000000000000, 0.9771240687918556489, 0.2126700594527800303 ) ) ;
#40337 = CARTESIAN_POINT ( 'NONE',  ( -0.7646288533564489232, 0.1113553986120547346, 1.008858267716535417 ) ) ;
#40338 = DIRECTION ( 'NONE',  ( 0.000000000000000000, 0.000000000000000000, 1.000000000000000000 ) ) ;
#40339 = CARTESIAN_POINT ( 'NONE',  ( -0.1574803149606299746, -0.4025872315894255538, -0.9257806984251616411 ) ) ;
#40340 = CARTESIAN_POINT ( 'NONE',  ( -0.5555748031496040573, 0.7681739484881665581, -0.04983111751016756213 ) ) ;
#40341 = CARTESIAN_POINT ( 'NONE',  ( 0.7495606340400177148, 0.1264236179284866091, 0.2731299212060791515 ) ) ;
#40342 = CARTESIAN_POINT ( 'NONE',  ( 0.7132025946407314354, -0.05284032427092102274, 0.03937007868462530369 ) ) ;
#40344 = LINE ( 'NONE', #29867, #13170 ) ;
#40343 = CARTESIAN_POINT ( 'NONE',  ( 0.7495606340400177148, 0.1264236179284866091, 1.257381889710015743 ) ) ;
#40345 = LINE ( 'NONE', #11385, #21215 ) ;
#40346 = CARTESIAN_POINT ( 'NONE',  ( 1.033464566929133799, 0.000000000000000000, 1.190944881889763884 ) ) ;
#40347 = CARTESIAN_POINT ( 'NONE',  ( 0.9873396505805591694, 0.1113553986120547346, 0.7135826770578268530 ) ) ;
#40348 = ORIENTED_EDGE ( 'NONE', *, *, #1349, .T. ) ;
#40349 = CARTESIAN_POINT ( 'NONE',  ( 0.8962961640049118550, 0.1721048943457904046, 0.03937035593878661366 ) ) ;
#40350 = CARTESIAN_POINT ( 'NONE',  ( -0.7185039370078746268, 0.06523048226347956391, 1.119586614065702035 ) ) ;
#40351 = CARTESIAN_POINT ( 'NONE',  ( 0.6971942568897648851, 0.07405724077823318263, 1.456692913332062744 ) ) ;
#40352 = CARTESIAN_POINT ( 'NONE',  ( -0.7646288533564489232, -0.1113553986120547346, 1.136811023622047223 ) ) ;
#40353 = CARTESIAN_POINT ( 'NONE',  ( 0.000000000000000000, 0.000000000000000000, 0.000000000000000000 ) ) ;
#40355 = CARTESIAN_POINT ( 'NONE',  ( -9.642888182262618425E-18, 0.1200787401574803237, -0.1574803149606299191 ) ) ;
#40354 = CARTESIAN_POINT ( 'NONE',  ( 0.1564139474901095617, -0.1149079234233351815, 0.08174552760832223819 ) ) ;
#40356 = LINE ( 'NONE', #26014, #9772 ) ;
#40357 = CARTESIAN_POINT ( 'NONE',  ( 0.1787899950787401882, -0.1776574802611972648, -2.189545951927503898E-17 ) ) ;
#40358 = EDGE_LOOP ( 'NONE', ( #21653, #46919, #46804 ) ) ;
#40359 = AXIS2_PLACEMENT_3D ( 'NONE', #20569, #35210, #28251 ) ;
#40360 = CARTESIAN_POINT ( 'NONE',  ( 1.033464566929134687, -0.06523048226347956391, 0.6668307085538908163 ) ) ;
#40361 = CARTESIAN_POINT ( 'NONE',  ( -0.7185039370078739607, 0.000000000000000000, -2.869337061179095023E-17 ) ) ;
#40362 = CARTESIAN_POINT ( 'NONE',  ( -0.03342428880116840584, -0.06208088008896742865, 0.2661310841544294870 ) ) ;
#40363 = CARTESIAN_POINT ( 'NONE',  ( 1.002407869896990045, 0.1264236179284866091, 0.5437992125446614589 ) ) ;
#40364 = ORIENTED_EDGE ( 'NONE', *, *, #27428, .F. ) ;
#40365 = CARTESIAN_POINT ( 'NONE',  ( -0.8759842519685039353, -0.1787899950787401882, 1.468996062938362046 ) ) ;
#40366 = CARTESIAN_POINT ( 'NONE',  ( -0.1264236179284866091, -1.811515747977732405, 0.1264236179284866091 ) ) ;
#40367 = CARTESIAN_POINT ( 'NONE',  ( -1.054774247047244096, 0.000000000000000000, 1.129429133804503937 ) ) ;
#40368 = ORIENTED_EDGE ( 'NONE', *, *, #26641, .F. ) ;
#40369 = CARTESIAN_POINT ( 'NONE',  ( -0.7646288533564489232, -0.1113553986120547346, 1.963582677165354395 ) ) ;
#40370 = CARTESIAN_POINT ( 'NONE',  ( -0.8019270111902717657, -0.1787899950787401604, 0.7627952755367881643 ) ) ;
#40371 = ( BOUNDED_CURVE ( )  B_SPLINE_CURVE ( 2, ( #8174, #22800, #10866, #14446, #29588, #29355, #21874, #43658, #36494 ),
 .UNSPECIFIED., .F., .T. ) 
 B_SPLINE_CURVE_WITH_KNOTS ( ( 3, 2, 2, 2, 3 ),
 ( 0.2200000000000000011, 0.2225000000000000033, 0.2250000000000000056, 0.2275000000000000078, 0.2300000000000000100 ),
 .UNSPECIFIED. ) 
 CURVE ( )  GEOMETRIC_REPRESENTATION_ITEM ( )  RATIONAL_B_SPLINE_CURVE ( ( 1.000000000000000000, 0.9238795325112869605, 1.000000000000000000, 0.9238795325112869605, 1.000000000000000000, 0.9238795325112869605, 1.000000000000000000, 0.9238795325112879597, 1.000000000000000000 ) ) 
 REPRESENTATION_ITEM ( '' )  ) ;
#40372 = CARTESIAN_POINT ( 'NONE',  ( -1.033464566929133799, 0.000000000000000000, 0.6003937007874016185 ) ) ;
#40373 = CARTESIAN_POINT ( 'NONE',  ( -0.6971942568897637749, 2.189545951927499583E-17, 0.1648622046706460786 ) ) ;
#40374 = DIRECTION ( 'NONE',  ( 0.000000000000000000, 0.000000000000000000, 1.000000000000000000 ) ) ;
#40375 = CARTESIAN_POINT ( 'NONE',  ( -0.6195511811023656223, 0.8070866141732282451, 0.5854071585544579071 ) ) ;
#40376 = CARTESIAN_POINT ( 'NONE',  ( -0.1787899950787401882, -0.7643956217725453861, 0.000000000000000000 ) ) ;
#40377 = ORIENTED_EDGE ( 'NONE', *, *, #14788, .F. ) ;
#40378 = CARTESIAN_POINT ( 'NONE',  ( 0.7238228411891962644, 0.09459845738158538520, 0.03936480202592971406 ) ) ;
#40379 = VERTEX_POINT ( 'NONE', #37236 ) ;
#40380 = CARTESIAN_POINT ( 'NONE',  ( 0.01034490908492528144, -0.07275794908485518075, 0.1377952755905511306 ) ) ;
#40381 = CARTESIAN_POINT ( 'NONE',  ( -0.9500414927467378812, 0.1787899950787401604, 0.8169291338045038264 ) ) ;
#40382 = VECTOR ( 'NONE', #19731, 39.37007874015748143 ) ;
#40383 = CARTESIAN_POINT ( 'NONE',  ( -0.6971942568897648851, 0.07405724077823318263, 1.776574803095843702 ) ) ;
#40384 = ADVANCED_FACE ( 'NONE', ( #44175 ), #20489, .F. ) ;
#40385 = AXIS2_PLACEMENT_3D ( 'NONE', #7268, #22104, #29599 ) ;
#40386 = ( BOUNDED_SURFACE ( )  B_SPLINE_SURFACE ( 3, 2, ( 
 ( #19464, #8679, #1245 ),
 ( #15422, #22829, #1475 ),
 ( #44608, #4352, #34117 ),
 ( #4595, #41012, #37444 ),
 ( #8203, #11824, #37928 ),
 ( #16133, #1007, #30764 ) ),
 .UNSPECIFIED., .F., .F., .T. ) 
 B_SPLINE_SURFACE_WITH_KNOTS ( ( 4, 2, 4 ),
 ( 3, 3 ),
 ( 0.01651999345535504898, 0.01858032176739835006, 0.02064065007944164767 ),
 ( 0.000000000000000000, 1.000000000000000000 ),
 .UNSPECIFIED. ) 
 GEOMETRIC_REPRESENTATION_ITEM ( )  RATIONAL_B_SPLINE_SURFACE ( (
 ( 1.000000000000000000, 0.8047781103519390244, 1.000000000000000000),
 ( 1.000000000000000000, 0.8123785825609349809, 1.000000000000000000),
 ( 1.000000000000000000, 0.8190671539781639865, 1.000000000000000000),
 ( 1.000000000000000000, 0.8192352254841480663, 1.000000000000000000),
 ( 1.000000000000000000, 0.8126129677206639368, 1.000000000000000000),
 ( 1.000000000000000000, 0.8047712537969730073, 1.000000000000000000) ) ) 
 REPRESENTATION_ITEM ( '' )  SURFACE ( )  ) ;
#40387 = ADVANCED_FACE ( 'NONE', ( #40570 ), #15211, .T. ) ;
#40388 = CARTESIAN_POINT ( 'NONE',  ( -0.8019270111902716547, 0.1787899950787401604, 0.07874015742655143812 ) ) ;
#40389 = CARTESIAN_POINT ( 'NONE',  ( 0.8107537697050253289, -0.1574803149606297803, 0.6274606299212601712 ) ) ;
#40390 = CARTESIAN_POINT ( 'NONE',  ( 0.1270800023317771588, -0.9311461717877698163, 0.1270800023317771588 ) ) ;
#40391 = DIRECTION ( 'NONE',  ( 0.000000000000000000, 0.000000000000000000, 1.000000000000000000 ) ) ;
#40392 = CARTESIAN_POINT ( 'NONE',  ( -0.7185039370078746268, 0.06523048226347956391, 1.592027558947591848 ) ) ;
#40393 = CARTESIAN_POINT ( 'NONE',  ( 0.6971942568897626646, -0.07405724077823297447, 0.7185039369541108556 ) ) ;
#40394 = CARTESIAN_POINT ( 'NONE',  ( 0.6971942568897637749, 2.189545951927499583E-17, 1.341043307032850462 ) ) ;
#40395 = EDGE_CURVE ( 'NONE', #1067, #46509, #29863, .T. ) ;
#40396 = EDGE_CURVE ( 'NONE', #30681, #36685, #1902, .T. ) ;
#40397 = DIRECTION ( 'NONE',  ( 1.000000000000000000, 0.000000000000000000, 0.000000000000000000 ) ) ;
#40398 = CARTESIAN_POINT ( 'NONE',  ( 0.7185039370078746268, 0.06523048226347956391, 1.405019685039369914 ) ) ;
#40400 = CARTESIAN_POINT ( 'NONE',  ( 0.8107537697050254399, -0.1574803149606297803, 1.562499999892472013 ) ) ;
#40399 = CARTESIAN_POINT ( 'NONE',  ( 0.8118511125780327742, -0.1600945206353099892, 1.986996213762715069 ) ) ;
#40401 = FACE_OUTER_BOUND ( 'NONE', #21039, .T. ) ;
#40403 = CARTESIAN_POINT ( 'NONE',  ( -0.7185039370078739607, 1.928577636452523993E-17, 1.407480314960629864 ) ) ;
#40402 = CARTESIAN_POINT ( 'NONE',  ( 0.9500414927467377701, 0.1787899950787401604, 0.8956692912848198684 ) ) ;
#40404 = CARTESIAN_POINT ( 'NONE',  ( 0.07405724077823318263, -0.7362204723871804690, 0.1787899950787401604 ) ) ;
#40405 = ORIENTED_EDGE ( 'NONE', *, *, #22168, .F. ) ;
#40406 = CARTESIAN_POINT ( 'NONE',  ( 0.1617601974881476001, 0.07970274315509767726, 0.1380562389070501550 ) ) ;
#40407 = CARTESIAN_POINT ( 'NONE',  ( -0.4405986714762811229, 0.2431096003418886098, -0.1899380364129106546 ) ) ;
#40408 = CARTESIAN_POINT ( 'NONE',  ( 0.6971942568897637749, 2.189545951927499583E-17, 1.026082677111590513 ) ) ;
#40409 = DIRECTION ( 'NONE',  ( 1.822029033848725028E-16, 0.000000000000000000, 1.000000000000000000 ) ) ;
#40410 = CARTESIAN_POINT ( 'NONE',  ( -0.06523048226347956391, -1.609744094488189337, -0.1574803149606300301 ) ) ;
#40411 = CARTESIAN_POINT ( 'NONE',  ( 0.3604359965418638123, 0.09842519685039370636, 1.205361022782828805E-17 ) ) ;
#40412 = CIRCLE ( 'NONE', #47313, 0.1377952755905511861 ) ;
#40413 = CARTESIAN_POINT ( 'NONE',  ( -0.8759842519685039353, 0.1787899950787401882, 0.5044291338045039375 ) ) ;
#40414 = ORIENTED_EDGE ( 'NONE', *, *, #18590, .T. ) ;
#40415 = LINE ( 'NONE', #33987, #15286 ) ;
#40416 = CARTESIAN_POINT ( 'NONE',  ( -0.6971942568897626646, 0.07405724077823318263, 0.1181102361667090567 ) ) ;
#40417 = VERTEX_POINT ( 'NONE', #44636 ) ;
#40418 = ORIENTED_EDGE ( 'NONE', *, *, #24783, .F. ) ;
#40419 = CARTESIAN_POINT ( 'NONE',  ( -0.1574803149606299191, 0.06102362215477106361, 0.000000000000000000 ) ) ;
#40420 = CARTESIAN_POINT ( 'NONE',  ( 0.1264236179284866091, -1.447342519631275692, 0.1264236179284866091 ) ) ;
#40421 = CARTESIAN_POINT ( 'NONE',  ( 0.8759842519685039353, -0.1574803149606299191, 0.3444881888688507976 ) ) ;
#40422 = CARTESIAN_POINT ( 'NONE',  ( -0.9500414927467378812, -0.1787899950787401604, 1.747047244040724312 ) ) ;
#40423 = CARTESIAN_POINT ( 'NONE',  ( -0.7495606340400177148, -0.1264236179284866091, 0.8341535432533228045 ) ) ;
#40424 = CARTESIAN_POINT ( 'NONE',  ( -1.002407869896990045, 0.1264236179284866091, 0.3863188975840318173 ) ) ;
#40425 = CARTESIAN_POINT ( 'NONE',  ( -0.7185039370078746268, -0.06523048226347935574, 0.1008858266641264878 ) ) ;
#40426 = CARTESIAN_POINT ( 'NONE',  ( 0.7185039370078739607, 1.928577636452523993E-17, 0.1771653542231816925 ) ) ;
#40427 = DIRECTION ( 'NONE',  ( 1.822029033848725028E-16, 0.000000000000000000, 1.000000000000000000 ) ) ;
#40428 = CARTESIAN_POINT ( 'NONE',  ( -0.9412147342319837628, -0.1574803149606297803, 1.970964566929134021 ) ) ;
#40429 = CARTESIAN_POINT ( 'NONE',  ( -0.2610014219173106831, 0.1673399808196284755, -0.8868260742169717936 ) ) ;
#40430 = CARTESIAN_POINT ( 'NONE',  ( -0.1264236179284866091, -0.4149861729536480914, -0.1264236179284866091 ) ) ;
#40431 = CARTESIAN_POINT ( 'NONE',  ( -0.2387240754188476310, -0.08955950445031535256, -0.009354969050736969619 ) ) ;
#40432 = CONTEXT_DEPENDENT_SHAPE_REPRESENTATION ( #2422, #3077 ) ;
#40433 = CYLINDRICAL_SURFACE ( 'NONE', #7289, 0.09842519685039310962 ) ;
#40434 = DIRECTION ( 'NONE',  ( -1.000000000000000000, -5.372880794957870593E-15, 4.197754538034579871E-15 ) ) ;
#40435 = CARTESIAN_POINT ( 'NONE',  ( -0.9500414927467378812, -0.1787899950787401604, 0.3297244093950552069 ) ) ;
#40436 = ORIENTED_EDGE ( 'NONE', *, *, #40396, .T. ) ;
#40437 = CARTESIAN_POINT ( 'NONE',  ( -0.6971942568897648851, 0.07405724077823318263, 1.382874015694267822 ) ) ;
#40438 = ORIENTED_EDGE ( 'NONE', *, *, #36589, .T. ) ;
#40439 = CARTESIAN_POINT ( 'NONE',  ( 0.1264236179284866091, -1.407972440891118282, 0.1264236179284866091 ) ) ;
#40440 = CARTESIAN_POINT ( 'NONE',  ( 3.284318927891251994E-17, -1.407972440891118282, 0.1787899950787401882 ) ) ;
#40441 = EDGE_CURVE ( 'NONE', #21057, #35279, #41216, .T. ) ;
#40442 = CIRCLE ( 'NONE', #42728, 0.009842519685039376881 ) ;
#40443 = DIRECTION ( 'NONE',  ( -1.000000000000000000, 0.000000000000000000, 0.000000000000000000 ) ) ;
#40444 = CARTESIAN_POINT ( 'NONE',  ( 1.033464566929134687, 0.06523048226347956391, 0.3272637795275589734 ) ) ;
#40445 = CARTESIAN_POINT ( 'NONE',  ( -0.8070866141732283561, -0.0009842519685049383633, -0.7574803149606299524 ) ) ;
#40446 = CARTESIAN_POINT ( 'NONE',  ( -0.8759842519685039353, 0.1574803149606299191, 1.033464566821606478 ) ) ;
#40447 = CIRCLE ( 'NONE', #36647, 0.3912448816427701037 ) ;
#40448 = CARTESIAN_POINT ( 'NONE',  ( -1.033464566929134687, -0.06523048226347956391, 1.700295275590550936 ) ) ;
#40449 = CARTESIAN_POINT ( 'NONE',  ( 0.06523048226347956391, -0.3548228346456690496, -0.1574803149606300301 ) ) ;
#40450 = ORIENTED_EDGE ( 'NONE', *, *, #34073, .F. ) ;
#40451 = LINE ( 'NONE', #18658, #21544 ) ;
#40452 = VERTEX_POINT ( 'NONE', #36771 ) ;
#40453 = ADVANCED_FACE ( 'NONE', ( #26238 ), #43438, .T. ) ;
#40454 = CARTESIAN_POINT ( 'NONE',  ( -0.1264414976123398593, -0.09162967223036785902, -0.1264062623377731343 ) ) ;
#40455 = CARTESIAN_POINT ( 'NONE',  ( 1.033464566929134687, 0.06523048226347956391, 0.9965551181102363376 ) ) ;
#40456 = AXIS2_PLACEMENT_3D ( 'NONE', #24371, #10230, #20531 ) ;
#40457 = DIRECTION ( 'NONE',  ( -0.000000000000000000, 1.000000000000000000, -0.000000000000000000 ) ) ;
#40458 = CARTESIAN_POINT ( 'NONE',  ( -0.06523048226347956391, -0.5221456691838117781, 0.1574803149606297803 ) ) ;
#40459 = DIRECTION ( 'NONE',  ( 1.822029033848725028E-16, 0.000000000000000000, 1.000000000000000000 ) ) ;
#40460 = CARTESIAN_POINT ( 'NONE',  ( -0.1908307771204775238, -0.07780576619187345999, -0.1752568734204362211 ) ) ;
#40461 = ORIENTED_EDGE ( 'NONE', *, *, #6163, .T. ) ;
#40462 = CARTESIAN_POINT ( 'NONE',  ( 1.033464566929133799, 0.000000000000000000, 1.889763779420031486 ) ) ;
#40463 = LINE ( 'NONE', #22507, #28896 ) ;
#40464 = CARTESIAN_POINT ( 'NONE',  ( -0.1787899950787401882, -1.496555118056472677, 0.000000000000000000 ) ) ;
#40465 = CARTESIAN_POINT ( 'NONE',  ( -9.642888182262618425E-18, -1.602362204616881725, -0.1574803149606299191 ) ) ;
#40466 = CARTESIAN_POINT ( 'NONE',  ( -1.094772975963752103E-17, -0.7239173227808818334, -0.1787899950787401882 ) ) ;
#40467 = CARTESIAN_POINT ( 'NONE',  ( 2.892866454678787531E-17, -1.277559055118110187, 0.1574803149606299191 ) ) ;
#40468 = CARTESIAN_POINT ( 'NONE',  ( 1.033464566929134687, 0.06523048226347956391, 1.026082677057828185 ) ) ;
#40469 = CARTESIAN_POINT ( 'NONE',  ( 1.033464566929133799, 0.000000000000000000, 1.820866141732283561 ) ) ;
#40470 = CARTESIAN_POINT ( 'NONE',  ( -0.9500414927467378812, -0.1787899950787401604, 0.3690944881352128393 ) ) ;
#40471 = ORIENTED_EDGE ( 'NONE', *, *, #21087, .T. ) ;
#40472 = ORIENTED_EDGE ( 'NONE', *, *, #28263, .T. ) ;
#40473 = ORIENTED_EDGE ( 'NONE', *, *, #2802, .T. ) ;
#40474 = CARTESIAN_POINT ( 'NONE',  ( -0.6971942568897637749, 2.189545951927499583E-17, 1.621555118056472455 ) ) ;
#40475 = CARTESIAN_POINT ( 'NONE',  ( 1.002407869896990045, -0.1264236179284866091, 1.675688976324189117 ) ) ;
#40476 = CARTESIAN_POINT ( 'NONE',  ( -1.002407869896990045, 0.1264236179284866091, 0.7800196849856062542 ) ) ;
#40477 = CARTESIAN_POINT ( 'NONE',  ( 0.8759842519685039353, 0.000000000000000000, 4.498031496062992574 ) ) ;
#40478 = CARTESIAN_POINT ( 'NONE',  ( 1.002407869896990045, -0.1264236179284866091, 0.2977362204186775885 ) ) ;
#40479 = DIRECTION ( 'NONE',  ( -1.000000000000000000, 5.411399086424350389E-15, -4.275490733183370330E-15 ) ) ;
#40480 = CARTESIAN_POINT ( 'NONE',  ( -0.6971942568897648851, -0.07405724077823297447, 1.225393700733637514 ) ) ;
#40481 = CARTESIAN_POINT ( 'NONE',  ( -0.7495606340400177148, 0.1264236179284866091, 0.6274606298674959559 ) ) ;
#40482 = DIRECTION ( 'NONE',  ( 1.822029033848725028E-16, 0.000000000000000000, 1.000000000000000000 ) ) ;
#40483 = AXIS2_PLACEMENT_3D ( 'NONE', #500, #10623, #25225 ) ;
#40484 = CARTESIAN_POINT ( 'NONE',  ( 0.1864803149606299171, 1.086379535891623949, -0.03715491745706165500 ) ) ;
#40485 = CARTESIAN_POINT ( 'NONE',  ( -1.054774247047244540, 0.07405724077823318263, 1.564960629867495845 ) ) ;
#40486 = CARTESIAN_POINT ( 'NONE',  ( -0.9873396505805591694, 0.1113553986120547346, 1.894685039262551163 ) ) ;
#40487 = ORIENTED_EDGE ( 'NONE', *, *, #46473, .F. ) ;
#40488 = CARTESIAN_POINT ( 'NONE',  ( 0.3649999999999999911, 2.679610302993149545E-17, 0.000000000000000000 ) ) ;
#40489 = CARTESIAN_POINT ( 'NONE',  ( -0.2304022103396637655, -0.09842519685039370636, 0.06210465366844153401 ) ) ;
#40490 = FACE_OUTER_BOUND ( 'NONE', #47334, .T. ) ;
#40491 = ORIENTED_EDGE ( 'NONE', *, *, #18184, .F. ) ;
#40492 = VERTEX_POINT ( 'NONE', #19260 ) ;
#40493 = CONICAL_SURFACE ( 'NONE', #32884, 0.09842519685039370636, 0.9599310885968824758 ) ;
#40494 = VERTEX_POINT ( 'NONE', #12091 ) ;
#40495 = ORIENTED_EDGE ( 'NONE', *, *, #16669, .T. ) ;
#40496 = CARTESIAN_POINT ( 'NONE',  ( -0.1787899950787401882, -0.8321850393163149340, 0.000000000000000000 ) ) ;
#40497 = CARTESIAN_POINT ( 'NONE',  ( 0.07405724077823318263, -0.4507874015210400209, -0.1787899950787401604 ) ) ;
#40498 = SHAPE_REPRESENTATION ( 'Side Bracket', ( #20860 ), #29349 ) ;
#40499 = CARTESIAN_POINT ( 'NONE',  ( -0.1787899950787401882, -0.9060039369541103005, 0.000000000000000000 ) ) ;
#40500 = ORIENTED_EDGE ( 'NONE', *, *, #1727, .F. ) ;
#40501 = EDGE_CURVE ( 'NONE', #3834, #32629, #30103, .T. ) ;
#40502 = DIRECTION ( 'NONE',  ( -1.000000000000000000, 3.469446951953614189E-15, 1.144917494144692682E-16 ) ) ;
#40503 = SHAPE_REPRESENTATION_RELATIONSHIP ( 'NONE' , 'NONE' ,  #17291, #31880 ) ;
#40504 = CARTESIAN_POINT ( 'NONE',  ( -1.100456976456230270E-17, -0.1683508961972187135, -0.1797182628040039365 ) ) ;
#40505 = CARTESIAN_POINT ( 'NONE',  ( 2.892866454678787531E-17, 0.1397637795275590566, 0.1574803149606299191 ) ) ;
#40506 = CARTESIAN_POINT ( 'NONE',  ( -0.1787899950787401882, -0.1235236219934805202, 0.000000000000000000 ) ) ;
#40507 = CARTESIAN_POINT ( 'NONE',  ( 0.2471922711061203815, -0.07744971747249546068, -0.07831899213442956864 ) ) ;
#40508 = CARTESIAN_POINT ( 'NONE',  ( 1.002407869896990045, -0.1264236179284866091, 0.7652559054580472253 ) ) ;
#40510 = CARTESIAN_POINT ( 'NONE',  ( -1.033464566929133799, 0.000000000000000000, 1.417322834538141674 ) ) ;
#40509 = CARTESIAN_POINT ( 'NONE',  ( -1.033507323347888418, 0.02751628197221928779, 0.03937007874015842346 ) ) ;
#40512 = DIRECTION ( 'NONE',  ( -0.5735764363510518216, 0.8191520442889876907, 1.003171929053519693E-16 ) ) ;
#40511 = CARTESIAN_POINT ( 'NONE',  ( -0.1377952755905511861, 1.808041534174241898E-17, -0.05390369169704170571 ) ) ;
#40513 = DIRECTION ( 'NONE',  ( 0.000000000000000000, -1.000000000000000000, 0.000000000000000000 ) ) ;
#40514 = CARTESIAN_POINT ( 'NONE',  ( 1.002407869896990045, -0.1264236179284866091, 1.754429133804503715 ) ) ;
#40515 = CARTESIAN_POINT ( 'NONE',  ( 0.7646288533564489232, -0.1113553986120547346, 1.874999999892472458 ) ) ;
#40516 = CARTESIAN_POINT ( 'NONE',  ( 0.7185039370078739607, 1.928577636452523993E-17, 0.1082677165354330728 ) ) ;
#40517 = DIRECTION ( 'NONE',  ( 1.822029033848725028E-16, 0.000000000000000000, 1.000000000000000000 ) ) ;
#40518 = CARTESIAN_POINT ( 'NONE',  ( 0.1787899950787401604, -0.2244094487651340231, 0.07405724077823318263 ) ) ;
#40519 = CARTESIAN_POINT ( 'NONE',  ( -0.8759842519685039353, 0.000000000000000000, 0.000000000000000000 ) ) ;
#40520 = CARTESIAN_POINT ( 'NONE',  ( 0.07405724077823318263, -1.154527559001354842, -0.1787899950787401604 ) ) ;
#40521 = CARTESIAN_POINT ( 'NONE',  ( 0.7495606340400177148, 0.1264236179284866091, 0.3174212597887562382 ) ) ;
#40522 = CYLINDRICAL_SURFACE ( 'NONE', #42236, 0.009842519685039491373 ) ;
#40523 = CARTESIAN_POINT ( 'NONE',  ( -0.8019270111902717657, -0.1787899950787401604, 1.624015747977732849 ) ) ;
#40524 = ORIENTED_EDGE ( 'NONE', *, *, #24475, .F. ) ;
#40525 = CARTESIAN_POINT ( 'NONE',  ( -1.002407869896990045, 0.1264236179284866091, 1.134350393647023614 ) ) ;
#40527 = AXIS2_PLACEMENT_3D ( 'NONE', #5989, #31661, #32120 ) ;
#40526 = CARTESIAN_POINT ( 'NONE',  ( -1.033464566929134687, 0.06523048226347956391, 0.8784448818897643285 ) ) ;
#40528 = CARTESIAN_POINT ( 'NONE',  ( 1.002407869896990045, -0.1264236179284866091, 1.281988188922614125 ) ) ;
#40529 = CARTESIAN_POINT ( 'NONE',  ( 0.6971942568897637749, 2.189545951927499583E-17, 0.04675196845017354913 ) ) ;
#40530 = CARTESIAN_POINT ( 'NONE',  ( -1.002407869896990045, 0.1264236179284866091, 1.050688976324189117 ) ) ;
#40531 = CARTESIAN_POINT ( 'NONE',  ( 0.1605229034655568932, 0.09306627081908142030, -0.1197794644538782011 ) ) ;
#40532 = CARTESIAN_POINT ( 'NONE',  ( -0.05275478416827693307, -0.2650362434218126451, -0.05809220732313855745 ) ) ;
#40533 = CARTESIAN_POINT ( 'NONE',  ( 1.002407869896990045, 0.1264236179284866091, 0.4256889763241890057 ) ) ;
#40534 = CARTESIAN_POINT ( 'NONE',  ( -1.002407869896990045, 0.1264236179284866091, 0.2632874015210397434 ) ) ;
#40535 = CARTESIAN_POINT ( 'NONE',  ( -1.054774247047244540, 0.07405724077823318263, 0.7726377952218265177 ) ) ;
#40536 = CARTESIAN_POINT ( 'NONE',  ( 0.9873396505805591694, 0.1113553986120547346, 1.658464566821606256 ) ) ;
#40537 = EDGE_LOOP ( 'NONE', ( #42494, #8180, #37157, #41671 ) ) ;
#40538 = EDGE_CURVE ( 'NONE', #13132, #46787, #22030, .T. ) ;
#40539 = CARTESIAN_POINT ( 'NONE',  ( -0.8107537697050254399, 0.1574803149606300301, 0.8784448817822366751 ) ) ;
#40540 = CARTESIAN_POINT ( 'NONE',  ( 0.6971942568897626646, -0.07405724077823297447, 0.9153543306548987957 ) ) ;
#40541 = CARTESIAN_POINT ( 'NONE',  ( -0.6971942568897648851, 0.07405724077823318263, 1.889763779473794481 ) ) ;
#40542 = ORIENTED_EDGE ( 'NONE', *, *, #47057, .F. ) ;
#40543 = CARTESIAN_POINT ( 'NONE',  ( 1.054774247047244540, 0.07405724077823318263, 1.914370078686394860 ) ) ;
#40544 = AXIS2_PLACEMENT_3D ( 'NONE', #39482, #3054, #28989 ) ;
#40545 = FACE_OUTER_BOUND ( 'NONE', #37969, .T. ) ;
#40546 = CARTESIAN_POINT ( 'NONE',  ( 0.1787899950787401882, -1.532112157205616221, -2.189545951927503898E-17 ) ) ;
#40547 = EDGE_LOOP ( 'NONE', ( #14065, #25056, #8157, #7222 ) ) ;
#40548 = FACE_BOUND ( 'NONE', #46373, .T. ) ;
#40549 = CARTESIAN_POINT ( 'NONE',  ( 0.1787899950787401604, -0.3375984251430867999, 0.07405724077823318263 ) ) ;
#40550 = EDGE_CURVE ( 'NONE', #16648, #44831, #44961, .T. ) ;
#40551 = CARTESIAN_POINT ( 'NONE',  ( -0.7646288533564489232, 0.1113553986120547346, 1.707677165246803241 ) ) ;
#40552 = VERTEX_POINT ( 'NONE', #33208 ) ;
#40553 = CARTESIAN_POINT ( 'NONE',  ( 1.054774247047244096, 0.000000000000000000, 1.124507873961984261 ) ) ;
#40554 = LINE ( 'NONE', #18996, #43985 ) ;
#40555 = CARTESIAN_POINT ( 'NONE',  ( 1.033464566929134687, 0.06523048226347956391, 1.380413385719244435 ) ) ;
#40556 = EDGE_CURVE ( 'NONE', #15333, #35268, #12098, .T. ) ;
#40557 = CARTESIAN_POINT ( 'NONE',  ( 0.6971942568897637749, 2.189545951927499583E-17, 1.498523621993480326 ) ) ;
#40558 = CARTESIAN_POINT ( 'NONE',  ( 1.054774247047244540, -0.07405724077823318263, 0.2165354330171024577 ) ) ;
#40559 = CARTESIAN_POINT ( 'NONE',  ( -0.1787899950787401604, -1.661417322780881500, -0.07405724077823318263 ) ) ;
#40560 = CARTESIAN_POINT ( 'NONE',  ( 0.07405724077823318263, -1.720472440891118726, 0.1787899950787401604 ) ) ;
#40561 = SHAPE_DEFINITION_REPRESENTATION ( #8995, #9609 ) ;
#40562 = EDGE_CURVE ( 'NONE', #31929, #36844, #1360, .T. ) ;
#40563 = CARTESIAN_POINT ( 'NONE',  ( -0.6971942568897648851, -0.07405724077823297447, 0.5610236219934807700 ) ) ;
#40564 = CARTESIAN_POINT ( 'NONE',  ( 1.033464566929134687, 0.06523048226347956391, 0.3666338582677165503 ) ) ;
#40565 = CARTESIAN_POINT ( 'NONE',  ( -0.07444174185955065859, -1.346992628480683907, -0.1797182628040039087 ) ) ;
#40566 = CARTESIAN_POINT ( 'NONE',  ( 0.1237557312196567866, 0.6131769916351965666, -0.8165595533554419472 ) ) ;
#40567 = CARTESIAN_POINT ( 'NONE',  ( 1.002407869896990045, 0.1264236179284866091, 1.331200787347811110 ) ) ;
#40568 = CARTESIAN_POINT ( 'NONE',  ( 0.7495606340400177148, -0.1264236179284866091, 1.660925196796630088 ) ) ;
#40569 = LINE ( 'NONE', #32961, #10779 ) ;
#40571 = CARTESIAN_POINT ( 'NONE',  ( -0.7845359159668372495, 0.1324275479413869194, 1.980250702907100369 ) ) ;
#40570 = FACE_OUTER_BOUND ( 'NONE', #15023, .T. ) ;
#40572 = CARTESIAN_POINT ( 'NONE',  ( 0.3906197235759846786, 0.09842519685039370636, 1.205361022782828805E-17 ) ) ;
#40573 = DIRECTION ( 'NONE',  ( -1.000000000000000000, 5.472378587457090550E-15, -4.275490733183370330E-15 ) ) ;
#40574 = CARTESIAN_POINT ( 'NONE',  ( 0.9873396505805591694, 0.1113553986120547346, 0.7529527557979842634 ) ) ;
#40575 = CARTESIAN_POINT ( 'NONE',  ( 0.8019270111902717657, 0.1787899950787401604, 0.3100393700249766682 ) ) ;
#40577 = LINE ( 'NONE', #3935, #10876 ) ;
#40576 = CARTESIAN_POINT ( 'NONE',  ( 0.6971942568897648851, 0.07405724077823318263, 1.220472440891118504 ) ) ;
#40578 = FACE_OUTER_BOUND ( 'NONE', #13989, .T. ) ;
#40579 = CARTESIAN_POINT ( 'NONE',  ( -1.033464566929133799, 0.000000000000000000, 0.9448818896562519720 ) ) ;
#40580 = CARTESIAN_POINT ( 'NONE',  ( -1.054774247047244540, -0.07405724077823318263, 1.200787401521039355 ) ) ;
#40581 = CARTESIAN_POINT ( 'NONE',  ( 0.7185039370078746268, 0.06523048226347956391, 0.6077755904436538126 ) ) ;
#40582 = ORIENTED_EDGE ( 'NONE', *, *, #11167, .F. ) ;
#40583 = CARTESIAN_POINT ( 'NONE',  ( 0.1113553986120547346, -0.04232283464566929249, -0.1113553986120547346 ) ) ;
#40584 = ORIENTED_EDGE ( 'NONE', *, *, #9712, .T. ) ;
#40585 = CARTESIAN_POINT ( 'NONE',  ( 0.07444174185955065859, -0.1068351481657228014, 0.1797182628040039087 ) ) ;
#40586 = PRODUCT_DEFINITION_SHAPE ( 'NONE', 'NONE',  #20410 ) ;
#40587 = CARTESIAN_POINT ( 'NONE',  ( -0.8107537697050253289, 0.1574803149606300301, 0.4847440943806614055 ) ) ;
#40588 = CONICAL_SURFACE ( 'NONE', #35992, 0.08090551181102362266, 0.9599310885968742602 ) ;
#40589 = CARTESIAN_POINT ( 'NONE',  ( 0.001140081640800088593, 0.02362312937809664393, 0.1377990287693362237 ) ) ;
#40590 = CARTESIAN_POINT ( 'NONE',  ( 0.6971942568897637749, 2.189545951927499583E-17, 1.577263779473795369 ) ) ;
#40591 = CARTESIAN_POINT ( 'NONE',  ( 0.1599045142067893333, -0.1486426375326765359, 0.02349808476896642767 ) ) ;
#40593 = AXIS2_PLACEMENT_3D ( 'NONE', #44593, #29814, #7955 ) ;
#40592 = CARTESIAN_POINT ( 'NONE',  ( -0.07405724077823318263, -0.1112204723871813017, 0.1787899950787401604 ) ) ;
#40594 = CARTESIAN_POINT ( 'NONE',  ( 0.9412147342319837628, -0.1574803149606297803, 1.331200787294047672 ) ) ;
#40595 = ORIENTED_EDGE ( 'NONE', *, *, #25154, .T. ) ;
#40596 = CARTESIAN_POINT ( 'NONE',  ( 0.1895013542076671997, -0.07859528327911675938, -0.1760244123199382060 ) ) ;
#40597 = CARTESIAN_POINT ( 'NONE',  ( 0.6971942568897648851, -0.07405724077823297447, 0.9153543306548987957 ) ) ;
#40598 = CARTESIAN_POINT ( 'NONE',  ( 0.06523048226347956391, 0.03395669302091285091, 0.1574803149606297803 ) ) ;
#40599 = CARTESIAN_POINT ( 'NONE',  ( -0.8759842519685039353, 0.1787899950787401882, 1.296751968450173154 ) ) ;
#40600 = EDGE_LOOP ( 'NONE', ( #41294, #29266, #6794, #40631 ) ) ;
#40601 = EDGE_CURVE ( 'NONE', #29380, #7257, #27958, .T. ) ;
#40602 = DIRECTION ( 'NONE',  ( 2.943801717310650128E-16, -1.000000000000000000, -2.355041373848520102E-15 ) ) ;
#40603 = CARTESIAN_POINT ( 'NONE',  ( -0.9500414927467378812, -0.1787899950787401604, 0.1771653542769452139 ) ) ;
#40604 = CYLINDRICAL_SURFACE ( 'NONE', #18772, 0.1574803149606299191 ) ;
#40605 = CARTESIAN_POINT ( 'NONE',  ( 0.000000000000000000, 0.000000000000000000, 0.000000000000000000 ) ) ;
#40606 = CARTESIAN_POINT ( 'NONE',  ( 0.1787899950787401882, -0.8234507398827816127, -2.189545951927503898E-17 ) ) ;
#40607 = ORIENTED_EDGE ( 'NONE', *, *, #16723, .F. ) ;
#40608 = CARTESIAN_POINT ( 'NONE',  ( 1.033464566929133799, 0.000000000000000000, 1.072834645669291431 ) ) ;
#40609 = EDGE_CURVE ( 'NONE', #3381, #5872, #38183, .T. ) ;
#40610 = VERTEX_POINT ( 'NONE', #46314 ) ;
#40611 = CARTESIAN_POINT ( 'NONE',  ( 0.7495606340400177148, 0.1264236179284866091, 1.021161417269070837 ) ) ;
#40612 = CARTESIAN_POINT ( 'NONE',  ( -0.7495606340400177148, -0.1264236179284866091, 0.7554133857730077617 ) ) ;
#40613 = CARTESIAN_POINT ( 'NONE',  ( -1.033464566929133799, 0.000000000000000000, 0.5905511809948347235 ) ) ;
#40614 = AXIS2_PLACEMENT_3D ( 'NONE', #23939, #12697, #13165 ) ;
#40615 = CARTESIAN_POINT ( 'NONE',  ( -1.054774247047244540, 0.07405724077823318263, 1.761811023568284229 ) ) ;
#40616 = CARTESIAN_POINT ( 'NONE',  ( -0.07405724077823318263, -0.5246062991588343882, -0.1787899950787401604 ) ) ;
#40617 = VECTOR ( 'NONE', #26169, 39.37007874015748143 ) ;
#40618 = ( LENGTH_UNIT ( ) NAMED_UNIT ( * ) SI_UNIT ( $, .METRE. ) ) ;
#40619 = CARTESIAN_POINT ( 'NONE',  ( -0.9873396505805591694, -0.1113553986120547346, 0.9498031496062993018 ) ) ;
#40620 = DIRECTION ( 'NONE',  ( 0.000000000000000000, 0.000000000000000000, -1.000000000000000000 ) ) ;
#40621 = CARTESIAN_POINT ( 'NONE',  ( 3.301370929368692659E-17, -1.054177667850761946, 0.1797182628040039365 ) ) ;
#40622 = DIRECTION ( 'NONE',  ( 1.822029033848725028E-16, 0.000000000000000000, 1.000000000000000000 ) ) ;
#40623 = CARTESIAN_POINT ( 'NONE',  ( -0.7646288533564489232, -0.1113553986120547346, 1.520669291231054876 ) ) ;
#40624 = CARTESIAN_POINT ( 'NONE',  ( 0.6971942568897626646, -0.07405724077823297447, 0.9547244093950547628 ) ) ;
#40625 = CARTESIAN_POINT ( 'NONE',  ( 0.8759842519685039353, -0.1574803149606299191, 1.417322834645669216 ) ) ;
#40626 = CARTESIAN_POINT ( 'NONE',  ( 0.7107006069439822937, 0.01204446385459368753, 1.983049284763879427 ) ) ;
#40627 = DIRECTION ( 'NONE',  ( -1.000000000000000000, 0.000000000000000000, 0.000000000000000000 ) ) ;
#40629 = CARTESIAN_POINT ( 'NONE',  ( 0.1526809758745832635, 0.1331472126641763676, 0.04497281396057103281 ) ) ;
#40628 = CARTESIAN_POINT ( 'NONE',  ( 0.6971942568897648851, -0.07405724077823297447, 0.8710629920722218200 ) ) ;
#40630 = CARTESIAN_POINT ( 'NONE',  ( 0.07405724077823318263, -0.7755905511273385455, 0.1787899950787401604 ) ) ;
#40631 = ORIENTED_EDGE ( 'NONE', *, *, #20676, .F. ) ;
#40632 = DIRECTION ( 'NONE',  ( 1.822029033848725028E-16, 0.000000000000000000, 1.000000000000000000 ) ) ;
#40633 = CARTESIAN_POINT ( 'NONE',  ( 0.7495606340400177148, 0.1264236179284866091, 1.178641732229700922 ) ) ;
#40634 = DIRECTION ( 'NONE',  ( 1.000000000000000000, -3.469446951953614583E-15, -1.144917494144684054E-16 ) ) ;
#40635 = CARTESIAN_POINT ( 'NONE',  ( -0.06523048226347956391, -1.688484251968503269, -0.1574803149606300301 ) ) ;
#40636 = DIRECTION ( 'NONE',  ( 0.000000000000000000, 0.000000000000000000, -1.000000000000000000 ) ) ;
#40637 = ( BOUNDED_CURVE ( )  B_SPLINE_CURVE ( 2, ( #36545, #44178, #40574, #3705, #3933, #18554, #90, #15456, #337 ),
 .UNSPECIFIED., .F., .T. ) 
 B_SPLINE_CURVE_WITH_KNOTS ( ( 3, 2, 2, 2, 3 ),
 ( 0.3599999999999999867, 0.3624999999999999889, 0.3649999999999999911, 0.3674999999999999933, 0.3699999999999999956 ),
 .UNSPECIFIED. ) 
 CURVE ( )  GEOMETRIC_REPRESENTATION_ITEM ( )  RATIONAL_B_SPLINE_CURVE ( ( 1.000000000000000000, 0.9238795325112869605, 1.000000000000000000, 0.9238795325112869605, 1.000000000000000000, 0.9238795325112869605, 1.000000000000000000, 0.9238795325112869605, 1.000000000000000000 ) ) 
 REPRESENTATION_ITEM ( '' )  ) ;
#40638 = ORIENTED_EDGE ( 'NONE', *, *, #19536, .T. ) ;
#40639 = CARTESIAN_POINT ( 'NONE',  ( 0.1602931993194444682, -0.1591122789105269553, 0.000000000000000000 ) ) ;
#40640 = CARTESIAN_POINT ( 'NONE',  ( -0.9500414927467378812, -0.1787899950787401604, 0.3297244093950552069 ) ) ;
#40641 = ORIENTED_EDGE ( 'NONE', *, *, #17864, .T. ) ;
#40642 = CARTESIAN_POINT ( 'NONE',  ( -0.7646288533564489232, 0.1113553986120547346, 0.6151574803149606474 ) ) ;
#40643 = CARTESIAN_POINT ( 'NONE',  ( 0.06523048226347956391, -0.3056102361129455214, -0.1574803149606300301 ) ) ;
#40644 = AXIS2_PLACEMENT_3D ( 'NONE', #29901, #44448, #1078 ) ;
#40645 = CARTESIAN_POINT ( 'NONE',  ( -1.002407869896990045, 0.1264236179284866091, 1.680610236166708793 ) ) ;
#40646 = EDGE_CURVE ( 'NONE', #43833, #758, #26643, .T. ) ;
#40647 = CARTESIAN_POINT ( 'NONE',  ( -1.054774247047244096, 0.000000000000000000, 0.9276574802611967652 ) ) ;
#40648 = VECTOR ( 'NONE', #41091, 39.37007874015748143 ) ;
#40649 = CARTESIAN_POINT ( 'NONE',  ( -0.6971942568897626646, 0.07405724077823318263, 0.4773622046706456068 ) ) ;
#40650 = EDGE_CURVE ( 'NONE', #19533, #8469, #8712, .T. ) ;
#40651 = CARTESIAN_POINT ( 'NONE',  ( 0.1574803149606300301, -0.03494094477436274215, -0.06523048226347956391 ) ) ;
#40652 = CARTESIAN_POINT ( 'NONE',  ( -0.9500414927467378812, -0.1787899950787401604, 1.988188976324187562 ) ) ;
#40653 = CARTESIAN_POINT ( 'NONE',  ( 0.1321676148590689159, 0.1299212598425196763, -0.1026092226670043267 ) ) ;
#40654 = CARTESIAN_POINT ( 'NONE',  ( 0.8759842519685039353, 0.1787899950787401882, 0.07135826766277185429 ) ) ;
#40655 = DIRECTION ( 'NONE',  ( -0.000000000000000000, 1.000000000000000000, -0.000000000000000000 ) ) ;
#40656 = CARTESIAN_POINT ( 'NONE',  ( -0.1787899950787401882, -0.3313247556308138164, 0.000000000000000000 ) ) ;
#40657 = CARTESIAN_POINT ( 'NONE',  ( -0.2269653392414791304, -0.08955981648012203977, 0.06100550293770786586 ) ) ;
#40658 = CARTESIAN_POINT ( 'NONE',  ( -0.7646288533564489232, 0.1113553986120547346, 1.904527558947590515 ) ) ;
#40659 = CYLINDRICAL_SURFACE ( 'NONE', #46303, 0.1574803149606299191 ) ;
#40660 = EDGE_CURVE ( 'NONE', #26397, #24855, #12573, .T. ) ;
#40661 = EDGE_CURVE ( 'NONE', #157, #39322, #27200, .T. ) ;
#40662 = CARTESIAN_POINT ( 'NONE',  ( 0.2559055118110236116, -0.1477471161312047254, -0.1122047244094488277 ) ) ;
#40663 = ( BOUNDED_CURVE ( )  B_SPLINE_CURVE ( 2, ( #7343, #32765, #40141, #29895, #25322, #47362, #18585, #22175, #7096 ),
 .UNSPECIFIED., .F., .F. ) 
 B_SPLINE_CURVE_WITH_KNOTS ( ( 3, 2, 2, 2, 3 ),
 ( 0.8100000000000000533, 0.8125000000000000000, 0.8149999999999999467, 0.8175000000000000044, 0.8199999999999999512 ),
 .UNSPECIFIED. ) 
 CURVE ( )  GEOMETRIC_REPRESENTATION_ITEM ( )  RATIONAL_B_SPLINE_CURVE ( ( 1.000000000000000000, 0.9238795325112899581, 1.000000000000000000, 0.9238795325112869605, 1.000000000000000000, 0.9238795325112869605, 1.000000000000000000, 0.9238795325112829637, 1.000000000000000000 ) ) 
 REPRESENTATION_ITEM ( '' )  ) ;
#40664 = CARTESIAN_POINT ( 'NONE',  ( -0.9500414927467378812, 0.1787899950787401604, 0.3838582676627718127 ) ) ;
#40665 = EDGE_LOOP ( 'NONE', ( #31666, #45560, #19236, #26178 ) ) ;
#40666 = CARTESIAN_POINT ( 'NONE',  ( -1.054774247047244540, 0.07405724077823318263, 1.407480314906865981 ) ) ;
#40667 = VERTEX_POINT ( 'NONE', #5343 ) ;
#40668 = CARTESIAN_POINT ( 'NONE',  ( -1.094772975963752103E-17, -1.353838582623401621, -0.1787899950787401882 ) ) ;
#40669 = CARTESIAN_POINT ( 'NONE',  ( 0.07405724077823318263, -1.469488188922614791, -0.1787899950787401604 ) ) ;
#40670 = SURFACE_SIDE_STYLE ('',( #7867 ) ) ;
#40671 = DIRECTION ( 'NONE',  ( -7.000000000000000150E-15, -2.999999999999999839E-15, -1.000000000000000000 ) ) ;
#40672 = CARTESIAN_POINT ( 'NONE',  ( 0.8759842519685039353, -0.1574803149606299191, 0.3937007874015748254 ) ) ;
#40673 = CARTESIAN_POINT ( 'NONE',  ( 0.8759842519685039353, 0.000000000000000000, 4.498031496062992574 ) ) ;
#40674 = CARTESIAN_POINT ( 'NONE',  ( -0.9412147342319837628, 0.1574803149606300301, 1.109744094380661572 ) ) ;
#40675 = CARTESIAN_POINT ( 'NONE',  ( 0.9500414927467378812, 0.1787899950787401604, 0.4675196849856070869 ) ) ;
#40676 = CARTESIAN_POINT ( 'NONE',  ( 0.8759842519685039353, 0.1574803149606299191, 0.5610236219397165547 ) ) ;
#40677 = ( REPRESENTATION_RELATIONSHIP ('NONE','NONE', #9609, #43589 ) REPRESENTATION_RELATIONSHIP_WITH_TRANSFORMATION ( #1738 )SHAPE_REPRESENTATION_RELATIONSHIP( ) ) ;
#40678 = CARTESIAN_POINT ( 'NONE',  ( 0.1113553986120547346, -0.2785433070866141780, -0.1113553986120547346 ) ) ;
#40679 = CIRCLE ( 'NONE', #875, 0.7381889763779526659 ) ;
#40680 = VECTOR ( 'NONE', #35887, 39.37007874015748143 ) ;
#40681 = ORIENTED_EDGE ( 'NONE', *, *, #32698, .T. ) ;
#40682 = CARTESIAN_POINT ( 'NONE',  ( 0.8759842519685039353, 0.1574803149606299191, 1.938976377845228249 ) ) ;
#40683 = ORIENTED_EDGE ( 'NONE', *, *, #20363, .T. ) ;
#40684 = FACE_OUTER_BOUND ( 'NONE', #25136, .T. ) ;
#40685 = CARTESIAN_POINT ( 'NONE',  ( -0.7495606340400177148, -0.1264236179284866091, 0.9965551180564724554 ) ) ;
#40686 = CARTESIAN_POINT ( 'NONE',  ( 1.033464566929133799, 0.000000000000000000, 0.8759842519685039353 ) ) ;
#40687 = DIRECTION ( 'NONE',  ( 3.478357113474434231E-15, 1.000000000000000000, 0.000000000000000000 ) ) ;
#40688 = CARTESIAN_POINT ( 'NONE',  ( -0.7185039370078739607, 1.928577636452523993E-17, 0.6988188976377952555 ) ) ;
#40689 = CARTESIAN_POINT ( 'NONE',  ( -0.7185039370078739607, 1.928577636452523993E-17, 1.003937007766488199 ) ) ;
#40690 = CARTESIAN_POINT ( 'NONE',  ( 0.6971942568897626646, -0.07405724077823297447, 0.5954724408911187261 ) ) ;
#40691 = ORIENTED_EDGE ( 'NONE', *, *, #25617, .F. ) ;
#40692 = CARTESIAN_POINT ( 'NONE',  ( 0.9873396505805591694, 0.1113553986120547346, 1.274606299212598604 ) ) ;
#40693 = CARTESIAN_POINT ( 'NONE',  ( 2.219626494852212756E-16, 0.2954942322624074524, -0.1122047244094488277 ) ) ;
#40694 = CARTESIAN_POINT ( 'NONE',  ( 0.1787899950787401604, -1.518700787347811554, 0.07405724077823318263 ) ) ;
#40695 = CARTESIAN_POINT ( 'NONE',  ( -0.1264236179284866091, -0.7878937007336378473, 0.1264236179284866091 ) ) ;
#40696 = CARTESIAN_POINT ( 'NONE',  ( 0.06523048226347956391, -1.260334645669290321, -0.1574803149606300301 ) ) ;
#40697 = CARTESIAN_POINT ( 'NONE',  ( 0.7185039370078739607, 1.928577636452523993E-17, 1.200787401467275695 ) ) ;
#40698 = FACE_OUTER_BOUND ( 'NONE', #15876, .T. ) ;
#40699 = ORIENTED_EDGE ( 'NONE', *, *, #36313, .F. ) ;
#40700 = ORIENTED_EDGE ( 'NONE', *, *, #20068, .T. ) ;
#40701 = ORIENTED_EDGE ( 'NONE', *, *, #30492, .T. ) ;
#40702 = CARTESIAN_POINT ( 'NONE',  ( -1.002407869896990045, 0.1264236179284866091, 1.803641732229700700 ) ) ;
#40703 = CARTESIAN_POINT ( 'NONE',  ( 0.8759842519685039353, 0.1787899950787401882, 1.729822834591905556 ) ) ;
#40704 = CARTESIAN_POINT ( 'NONE',  ( -0.6971942568897626646, -0.07405724077823297447, 0.8366141731745828647 ) ) ;
#40705 = CARTESIAN_POINT ( 'NONE',  ( -0.06871726393444720082, -0.2558202476623576138, -0.3098131533094798384 ) ) ;
#40706 = CARTESIAN_POINT ( 'NONE',  ( 0.8019270111902717657, 0.1787899950787401604, 0.3543307086076538659 ) ) ;
#40707 = CARTESIAN_POINT ( 'NONE',  ( -0.6971942568897648851, 0.07405724077823318263, 1.299212598371434435 ) ) ;
#40708 = AXIS2_PLACEMENT_3D ( 'NONE', #32902, #19, #29343 ) ;
#40709 = CARTESIAN_POINT ( 'NONE',  ( -0.9500414927467378812, 0.1787899950787401604, 0.8956692912848198684 ) ) ;
#40710 = CARTESIAN_POINT ( 'NONE',  ( 0.9873396505805591694, 0.1113553986120547346, 0.9104330707586141269 ) ) ;
#40711 = EDGE_CURVE ( 'NONE', #1339, #4869, #45359, .T. ) ;
#40712 = VECTOR ( 'NONE', #25302, 39.37007874015748143 ) ;
#40713 = CARTESIAN_POINT ( 'NONE',  ( -1.002407869896990045, -0.1264236179284866091, 1.636318897584031484 ) ) ;
#40714 = CARTESIAN_POINT ( 'NONE',  ( -0.8107537697050253289, -0.1574803149606297803, 1.877460629813732407 ) ) ;
#40715 = EDGE_LOOP ( 'NONE', ( #43988, #10408, #595, #24954 ) ) ;
#40716 = DIRECTION ( 'NONE',  ( -1.000000000000000000, -0.000000000000000000, -0.000000000000000000 ) ) ;
#40717 = CARTESIAN_POINT ( 'NONE',  ( 0.7646288533564489232, -0.1113553986120547346, 0.9694881888688504645 ) ) ;
#40718 = CARTESIAN_POINT ( 'NONE',  ( 0.9500414927467377701, 0.1787899950787401604, 1.609251968450173598 ) ) ;
#40719 = CARTESIAN_POINT ( 'NONE',  ( 0.07340243826527893811, -0.09851382364606299513, 0.1314582435714135855 ) ) ;
#40720 = CARTESIAN_POINT ( 'NONE',  ( 0.7646288533564489232, 0.1113553986120547346, 0.2116141731208196763 ) ) ;
#40721 = EDGE_CURVE ( 'NONE', #7257, #46851, #9189, .T. ) ;
#40722 = AXIS2_PLACEMENT_3D ( 'NONE', #41141, #4482, #19122 ) ;
#40723 = VERTEX_POINT ( 'NONE', #30795 ) ;
#40724 = AXIS2_PLACEMENT_3D ( 'NONE', #31954, #6044, #36005 ) ;
#40725 = EDGE_CURVE ( 'NONE', #7448, #10459, #5953, .T. ) ;
#40726 = ORIENTED_EDGE ( 'NONE', *, *, #4010, .T. ) ;
#40727 = ( NAMED_UNIT ( * ) SI_UNIT ( $, .STERADIAN. ) SOLID_ANGLE_UNIT ( ) ) ;
#40728 = VERTEX_POINT ( 'NONE', #16398 ) ;
#40729 = CARTESIAN_POINT ( 'NONE',  ( 0.1787899950787401604, -0.8543307086076546986, 0.07405724077823318263 ) ) ;
#40730 = CARTESIAN_POINT ( 'NONE',  ( 0.07405724077823318263, -0.4655511810485986057, 0.1787899950787401604 ) ) ;
#40731 = CARTESIAN_POINT ( 'NONE',  ( -0.1787899950787401604, -1.139763779473794925, 0.07405724077823318263 ) ) ;
#40732 = VERTEX_POINT ( 'NONE', #16845 ) ;
#40733 = LENGTH_MEASURE_WITH_UNIT ( LENGTH_MEASURE( 0.02539999999999999897 ), #29789 ) ;
#40734 = CARTESIAN_POINT ( 'NONE',  ( 1.054774247047244540, 0.07405724077823318263, 1.717519684985606476 ) ) ;
#40735 = CARTESIAN_POINT ( 'NONE',  ( 0.1797182628040039365, -0.3356737308428881517, -2.200913952912460540E-17 ) ) ;
#40736 = CARTESIAN_POINT ( 'NONE',  ( 0.000000000000000000, 0.000000000000000000, 0.09842519685039370636 ) ) ;
#40737 = CARTESIAN_POINT ( 'NONE',  ( -0.1787899950787401882, -0.04478346451316559534, 0.000000000000000000 ) ) ;
#40738 = LINE ( 'NONE', #7933, #35294 ) ;
#40739 = CARTESIAN_POINT ( 'NONE',  ( 1.054774247047244096, 0.000000000000000000, 0.8095472440407244230 ) ) ;
#40740 = CIRCLE ( 'NONE', #37697, 0.08090551181102362266 ) ;
#40741 = CARTESIAN_POINT ( 'NONE',  ( -0.7185039370078766252, -0.06523048226348168721, 1.557578740049954558 ) ) ;
#40743 = CARTESIAN_POINT ( 'NONE',  ( 0.000000000000000000, 0.000000000000000000, 0.000000000000000000 ) ) ;
#40742 = CARTESIAN_POINT ( 'NONE',  ( 0.7185039370078739607, 1.928577636452523993E-17, 0.1476377952755905387 ) ) ;
#40744 = CARTESIAN_POINT ( 'NONE',  ( 0.7495606340400177148, -0.1264236179284866091, 1.862696850339937038 ) ) ;
#40745 = CARTESIAN_POINT ( 'NONE',  ( 0.9873396505805591694, -0.1113553986120547346, 1.884842519577511810 ) ) ;
#40746 = AXIS2_PLACEMENT_3D ( 'NONE', #32159, #31460, #35051 ) ;
#40747 = AXIS2_PLACEMENT_3D ( 'NONE', #40519, #7708, #18728 ) ;
#40748 = CARTESIAN_POINT ( 'NONE',  ( 1.033464566929134687, 0.06523048226347956391, 0.09104330708661413640 ) ) ;
#40749 = CARTESIAN_POINT ( 'NONE',  ( 0.8070866141732283561, -0.3937007874015746034, 0.8559055118110230342 ) ) ;
#40750 = CARTESIAN_POINT ( 'NONE',  ( -0.1264236179284866091, -0.2367125983714334636, 0.1264236179284866091 ) ) ;
#40752 = CARTESIAN_POINT ( 'NONE',  ( 0.1605229034655247800, 0.1502651944781876470, 0.02070802253799618881 ) ) ;
#40751 = CARTESIAN_POINT ( 'NONE',  ( -0.7495606340400177148, -0.1264236179284866091, 0.4060039369541102450 ) ) ;
#40753 = CARTESIAN_POINT ( 'NONE',  ( -0.1787899950787401882, -1.220964566875370139, 0.000000000000000000 ) ) ;
#40754 = CARTESIAN_POINT ( 'NONE',  ( 0.7495606340400177148, -0.1264236179284866091, 0.2485236219934806867 ) ) ;
#40755 = CARTESIAN_POINT ( 'NONE',  ( 0.1643592525017875672, 0.08109370453517872335, -0.1404553931991618931 ) ) ;
#40756 = CARTESIAN_POINT ( 'NONE',  ( -0.6971942568897648851, 0.07405724077823318263, 1.811023621993480548 ) ) ;
#40757 = ORIENTED_EDGE ( 'NONE', *, *, #46039, .F. ) ;
#40758 = VECTOR ( 'NONE', #19303, 39.37007874015748143 ) ;
#40759 = CARTESIAN_POINT ( 'NONE',  ( -0.8019270111902717657, 0.1787899950787401604, 1.102362204670646495 ) ) ;
#40760 = DIRECTION ( 'NONE',  ( 0.000000000000000000, 0.9699617890481143645, 0.2432573283306820044 ) ) ;
#40761 = CARTESIAN_POINT ( 'NONE',  ( 0.1113553986120547346, -1.174212598317669221, -0.1113553986120547346 ) ) ;
#40762 = CARTESIAN_POINT ( 'NONE',  ( 0.9500414927467378812, -0.1787899950787401604, 1.943897637741510254 ) ) ;
#40763 = CARTESIAN_POINT ( 'NONE',  ( -0.6971942568897648851, -0.07405724077823297447, 0.9891732282926934960 ) ) ;
#40764 = CARTESIAN_POINT ( 'NONE',  ( -0.09161186067205415173, -0.09842317194137423231, -0.1536306822207036404 ) ) ;
#40765 = CARTESIAN_POINT ( 'NONE',  ( -0.09016091299416130467, -0.2434398048748465382, -0.03531881253561287154 ) ) ;
#40766 = CARTESIAN_POINT ( 'NONE',  ( 1.002407869896990045, 0.1264236179284866091, 0.5044291338045039375 ) ) ;
#40767 = CARTESIAN_POINT ( 'NONE',  ( -0.8019270111902716547, -0.1787899950787401604, 0.4035433070328507954 ) ) ;
#40768 = CARTESIAN_POINT ( 'NONE',  ( -0.9500414927467378812, -0.1787899950787401604, 0.8021653542769460188 ) ) ;
#40769 = ORIENTED_EDGE ( 'NONE', *, *, #41303, .T. ) ;
#40770 = ADVANCED_FACE ( 'NONE', ( #31486 ), #41751, .T. ) ;
#40771 = DIRECTION ( 'NONE',  ( 1.000000000000000000, -3.469446951953614189E-15, 0.000000000000000000 ) ) ;
#40772 = CARTESIAN_POINT ( 'NONE',  ( -0.8107537697050253289, 0.1574803149606300301, 0.2189960629921262614 ) ) ;
#40773 = CARTESIAN_POINT ( 'NONE',  ( 1.002407869896990045, 0.1264236179284866091, 1.094980314906866203 ) ) ;
#40774 = CARTESIAN_POINT ( 'NONE',  ( -0.8019270111902716547, 0.1787899950787401604, 1.963582677111591401 ) ) ;
#40775 = ORIENTED_EDGE ( 'NONE', *, *, #8109, .F. ) ;
#40776 = CONICAL_SURFACE ( 'NONE', #5610, 0.09842519685039370636, 0.9599310885968824758 ) ;
#40777 = EDGE_CURVE ( 'NONE', #39783, #28164, #31023, .T. ) ;
#40778 = ( BOUNDED_CURVE ( )  B_SPLINE_CURVE ( 2, ( #23744, #2625, #42859, #35257, #27610, #34533, #9128, #42165, #5526 ),
 .UNSPECIFIED., .F., .T. ) 
 B_SPLINE_CURVE_WITH_KNOTS ( ( 3, 2, 2, 2, 3 ),
 ( 0.2999999999999999889, 0.3024999999999999911, 0.3049999999999999933, 0.3074999999999999956, 0.3099999999999999978 ),
 .UNSPECIFIED. ) 
 CURVE ( )  GEOMETRIC_REPRESENTATION_ITEM ( )  RATIONAL_B_SPLINE_CURVE ( ( 1.000000000000000000, 0.9238795325112869605, 1.000000000000000000, 0.9238795325112869605, 1.000000000000000000, 0.9238795325112869605, 1.000000000000000000, 0.9238795325112869605, 1.000000000000000000 ) ) 
 REPRESENTATION_ITEM ( '' )  ) ;
#40779 = AXIS2_PLACEMENT_3D ( 'NONE', #24280, #38413, #38875 ) ;
#40780 = CARTESIAN_POINT ( 'NONE',  ( -0.7495606340400177148, 0.1264236179284866091, 0.07627952750529173875 ) ) ;
#40781 = CARTESIAN_POINT ( 'NONE',  ( 0.1787899950787401882, -1.414001920985143768, -2.189545951927503898E-17 ) ) ;
#40782 = ORIENTED_EDGE ( 'NONE', *, *, #43594, .F. ) ;
#40783 = CARTESIAN_POINT ( 'NONE',  ( 0.1787899950787401604, -0.4163385826234020093, 0.07405724077823318263 ) ) ;
#40784 = CARTESIAN_POINT ( 'NONE',  ( -0.9873396505805591694, 0.1113553986120547346, 1.697834645561763889 ) ) ;
#40785 = CARTESIAN_POINT ( 'NONE',  ( 0.8759842519685039353, 0.1787899950787401882, 1.173720472387181246 ) ) ;
#40786 = AXIS2_PLACEMENT_3D ( 'NONE', #29505, #40443, #25861 ) ;
#40787 = VECTOR ( 'NONE', #29020, 39.37007874015748143 ) ;
#40788 = CARTESIAN_POINT ( 'NONE',  ( 1.033464566929133799, 0.000000000000000000, 1.584645669291338654 ) ) ;
#40789 = DIRECTION ( 'NONE',  ( 0.000000000000000000, 0.000000000000000000, 1.000000000000000000 ) ) ;
#40790 = CARTESIAN_POINT ( 'NONE',  ( 0.8759842519685039353, 0.1787899950787401882, 0.2288385826234019815 ) ) ;
#40791 = CARTESIAN_POINT ( 'NONE',  ( 0.1787899950787401882, -1.796751968450173376, -2.189545951927503898E-17 ) ) ;
#40792 = CARTESIAN_POINT ( 'NONE',  ( -0.1264236179284866091, -1.688484251914740275, 0.1264236179284866091 ) ) ;
#40793 = SHAPE_DEFINITION_REPRESENTATION ( #31612, #5950 ) ;
#40794 = CARTESIAN_POINT ( 'NONE',  ( -0.9873396505805591694, -0.1113553986120547346, 1.136811023514519681 ) ) ;
#40795 = ORIENTED_EDGE ( 'NONE', *, *, #9828, .T. ) ;
#40796 = EDGE_CURVE ( 'NONE', #17791, #34943, #23575, .T. ) ;
#40797 = CARTESIAN_POINT ( 'NONE',  ( -0.6971942568897648851, 0.07405724077823318263, 0.6348425196312760255 ) ) ;
#40798 = CARTESIAN_POINT ( 'NONE',  ( -0.1574803149606297803, -0.7731299212598427006, 0.06523048226347956391 ) ) ;
#40799 = CARTESIAN_POINT ( 'NONE',  ( 0.07444174185955046430, -1.430654045803517294, -0.1797182628040039087 ) ) ;
#40800 = CYLINDRICAL_SURFACE ( 'NONE', #7264, 0.1673228346456687721 ) ;
#40801 = CARTESIAN_POINT ( 'NONE',  ( 0.9500414927467378812, -0.1787899950787401604, 1.437007873961985371 ) ) ;
#40802 = CARTESIAN_POINT ( 'NONE',  ( 0.8759842519685039353, -0.1787899950787401882, 1.705216535379307174 ) ) ;
#40803 = DIRECTION ( 'NONE',  ( -1.000000000000000000, 0.000000000000000000, 0.000000000000000000 ) ) ;
#40804 = CARTESIAN_POINT ( 'NONE',  ( 0.7185039370078739607, 0.000000000000000000, 4.498031496062992574 ) ) ;
#40805 = CARTESIAN_POINT ( 'NONE',  ( 0.07405724077823318263, 0.1397637795813224670, -0.1787899950787401604 ) ) ;
#40806 = DIRECTION ( 'NONE',  ( 0.000000000000000000, 0.4344452574044144755, -0.9006982393225890782 ) ) ;
#40808 = CARTESIAN_POINT ( 'NONE',  ( -1.033464566929133799, 0.000000000000000000, 0.1968503935932602311 ) ) ;
#40807 = CARTESIAN_POINT ( 'NONE',  ( 0.8759842519685039353, 0.1787899950787401882, 1.252460629867496067 ) ) ;
#40809 = CARTESIAN_POINT ( 'NONE',  ( 1.033464566929133799, 0.000000000000000000, 0.2854330708661417804 ) ) ;
#40810 = CARTESIAN_POINT ( 'NONE',  ( -0.9500414927467378812, 0.1787899950787401604, 1.210629921206079818 ) ) ;
#40811 = CARTESIAN_POINT ( 'NONE',  ( 0.7185039370078739607, 1.928577636452523993E-17, 0.6102362203649134287 ) ) ;
#40812 = ORIENTED_EDGE ( 'NONE', *, *, #21029, .F. ) ;
#40813 = CARTESIAN_POINT ( 'NONE',  ( -0.2066929133858267931, 0.5257908685547681982, -0.4487896632427120225 ) ) ;
#40814 = ORIENTED_EDGE ( 'NONE', *, *, #21297, .F. ) ;
#40815 = CARTESIAN_POINT ( 'NONE',  ( 0.1270800023317771588, -0.05516191981926597820, -0.1270800023317771588 ) ) ;
#40817 = CARTESIAN_POINT ( 'NONE',  ( -0.9873396505805591694, -0.1113553986120547346, 0.3100393699712130080 ) ) ;
#40816 = VECTOR ( 'NONE', #30660, 39.37007874015748143 ) ;
#40818 = CARTESIAN_POINT ( 'NONE',  ( -0.1787899950787401882, -1.265255905458047225, 0.000000000000000000 ) ) ;
#40819 = CARTESIAN_POINT ( 'NONE',  ( 0.0005771639294482186966, 0.01692329920547855360, 0.1377992204327473935 ) ) ;
#40820 = CARTESIAN_POINT ( 'NONE',  ( 0.7495606340400177148, -0.1264236179284866091, 1.660925196796630088 ) ) ;
#40821 = CARTESIAN_POINT ( 'NONE',  ( -0.7646288533564489232, -0.1113553986120547346, 1.087598425089322918 ) ) ;
#40823 = CARTESIAN_POINT ( 'NONE',  ( -0.9873396505805591694, -0.1113553986120547346, 1.382874015748031704 ) ) ;
#40822 = CARTESIAN_POINT ( 'NONE',  ( 0.1571168540705163430, -0.1082847392565217393, 0.09327620385775631240 ) ) ;
#40824 = CARTESIAN_POINT ( 'NONE',  ( 0.8019270111902716547, -0.1787899950787401604, 0.05413385821395302888 ) ) ;
#40825 = CARTESIAN_POINT ( 'NONE',  ( -1.054774247047244540, -0.07405724077823318263, 0.05905511805647267048 ) ) ;
#40826 = CARTESIAN_POINT ( 'NONE',  ( -0.1264236179284866091, -0.1235236219934805202, -0.1264236179284866091 ) ) ;
#40827 = ORIENTED_EDGE ( 'NONE', *, *, #36465, .T. ) ;
#40828 = ADVANCED_FACE ( 'NONE', ( #23807 ), #45589, .T. ) ;
#40829 = CARTESIAN_POINT ( 'NONE',  ( 0.000000000000000000, 0.000000000000000000, -0.2748405511811023438 ) ) ;
#40830 = FILL_AREA_STYLE ('',( #23767 ) ) ;
#40831 = VERTEX_POINT ( 'NONE', #1507 ) ;
#40832 = CARTESIAN_POINT ( 'NONE',  ( 0.6971942568897626646, -0.07405724077823297447, 0.6791338582139527791 ) ) ;
#40833 = CARTESIAN_POINT ( 'NONE',  ( 0.8019270111902716547, 0.1787899950787401604, 0.8267716534895444003 ) ) ;
#40834 = CARTESIAN_POINT ( 'NONE',  ( -1.054774247047244096, 0.000000000000000000, 1.557578740103716441 ) ) ;
#40835 = CARTESIAN_POINT ( 'NONE',  ( -9.642888182262618425E-18, -0.1062992124908982289, -0.1574803149606299191 ) ) ;
#40836 = CARTESIAN_POINT ( 'NONE',  ( -0.6971942568897648851, 0.07405724077823318263, 1.225393700733637514 ) ) ;
#40837 = EDGE_CURVE ( 'NONE', #42967, #3817, #7492, .T. ) ;
#40838 = CARTESIAN_POINT ( 'NONE',  ( -0.6971942568897626646, -0.07405724077823297447, 0.3248031495525359746 ) ) ;
#40839 = CARTESIAN_POINT ( 'NONE',  ( 0.01035225325193033126, 0.1557259041957147483, -0.005865373059513411674 ) ) ;
#40840 = FACE_OUTER_BOUND ( 'NONE', #39296, .T. ) ;
#40841 = CARTESIAN_POINT ( 'NONE',  ( -0.1787899950787401604, -0.9243365666544370862, -0.07405724077823318263 ) ) ;
#40842 = ORIENTED_EDGE ( 'NONE', *, *, #24157, .T. ) ;
#40843 = CARTESIAN_POINT ( 'NONE',  ( 0.1264236179284866091, 0.06348425202226751218, -0.1264236179284866091 ) ) ;
#40844 = VERTEX_POINT ( 'NONE', #46072 ) ;
#40845 = ORIENTED_EDGE ( 'NONE', *, *, #28893, .T. ) ;
#40846 = CARTESIAN_POINT ( 'NONE',  ( 0.9412147342319837628, -0.1574803149606297803, 1.213090551073575662 ) ) ;
#40847 = FACE_OUTER_BOUND ( 'NONE', #23232, .T. ) ;
#40848 = CARTESIAN_POINT ( 'NONE',  ( 1.033464566929133799, 0.000000000000000000, 1.417322834538141674 ) ) ;
#40849 = CIRCLE ( 'NONE', #302, 0.08090551181102362266 ) ;
#40850 = CARTESIAN_POINT ( 'NONE',  ( -0.9500414927467377701, -0.1787899950787401604, 0.1771653542769452416 ) ) ;
#40851 = CARTESIAN_POINT ( 'NONE',  ( -0.8759842519685039353, 0.1574803149606299191, 0.8464566929133857665 ) ) ;
#40852 = LINE ( 'NONE', #30600, #9564 ) ;
#40853 = CARTESIAN_POINT ( 'NONE',  ( 0.1797182628040039087, -0.9286855418665098671, 0.07444174185955046430 ) ) ;
#40854 = CARTESIAN_POINT ( 'NONE',  ( -0.6195511811023656223, 0.1864803149606299171, 1.186023622047243986 ) ) ;
#40855 = CARTESIAN_POINT ( 'NONE',  ( -0.8107537697050253289, -0.1574803149606297803, 1.523129921152316379 ) ) ;
#40856 = VECTOR ( 'NONE', #41193, 39.37007874015748143 ) ;
#40857 = CARTESIAN_POINT ( 'NONE',  ( 0.6971942568897637749, 2.189545951927499583E-17, 0.9916338582139527791 ) ) ;
#40858 = CARTESIAN_POINT ( 'NONE',  ( 0.7495606340400177148, 0.1264236179284866091, 1.336122047190330786 ) ) ;
#40859 = CARTESIAN_POINT ( 'NONE',  ( 0.1968503937007874682, 0.06245656531175292070, -0.1492449156640645314 ) ) ;
#40860 = CARTESIAN_POINT ( 'NONE',  ( 0.9412147342319837628, -0.1574803149606297803, 1.341043307086615455 ) ) ;
#40862 = CARTESIAN_POINT ( 'NONE',  ( -1.033464566929133799, 0.000000000000000000, 0.04921259842519685318 ) ) ;
#40861 = CARTESIAN_POINT ( 'NONE',  ( 0.7265838559950141828, -0.07822853150185864191, 1.984785922399904701 ) ) ;
#40863 = CARTESIAN_POINT ( 'NONE',  ( -0.1377952755905511861, 0.1564960629921283985, 0.9074803149606294195 ) ) ;
#40865 = CARTESIAN_POINT ( 'NONE',  ( 0.1645760587280559184, 0.08068587895603188120, 0.1413870478498926997 ) ) ;
#40864 = CARTESIAN_POINT ( 'NONE',  ( 1.002407869896990045, -0.1264236179284866091, 0.8046259841982047467 ) ) ;
#40866 = CARTESIAN_POINT ( 'NONE',  ( 0.1787899950787401604, -0.7263779527021420046, -0.07405724077823318263 ) ) ;
#40867 = ORIENTED_EDGE ( 'NONE', *, *, #25526, .F. ) ;
#40868 = EDGE_CURVE ( 'NONE', #5152, #22068, #6790, .T. ) ;
#40869 = CARTESIAN_POINT ( 'NONE',  ( 0.1574803149606299191, 0.1299212598425196763, 0.000000000000000000 ) ) ;
#40870 = CARTESIAN_POINT ( 'NONE',  ( 0.000000000000000000, 0.09842519685039370636, -0.2204724409448818867 ) ) ;
#40871 = CARTESIAN_POINT ( 'NONE',  ( 1.002407869896990045, 0.1264236179284866091, 1.208169291284818980 ) ) ;
#40872 = FACE_OUTER_BOUND ( 'NONE', #30227, .T. ) ;
#40873 = CARTESIAN_POINT ( 'NONE',  ( -0.1574803149606297803, -1.718011811023622881, 0.06523048226347956391 ) ) ;
#40874 = CARTESIAN_POINT ( 'NONE',  ( 0.1498753904841986506, 0.1193342091828950846, -0.06889763779527559306 ) ) ;
#40875 = EDGE_CURVE ( 'NONE', #7744, #19773, #2457, .T. ) ;
#40876 = EDGE_LOOP ( 'NONE', ( #21601, #11934, #24158, #19706, #41104 ) ) ;
#40878 = PLANE ( 'NONE',  #44331 ) ;
#40877 = VECTOR ( 'NONE', #7104, 39.37007874015748854 ) ;
#40879 = CARTESIAN_POINT ( 'NONE',  ( -0.8759842519685039353, 0.1787899950787401882, 0.2682086613635594752 ) ) ;
#40880 = VERTEX_POINT ( 'NONE', #28852 ) ;
#40881 = ORIENTED_EDGE ( 'NONE', *, *, #32097, .T. ) ;
#40882 = CARTESIAN_POINT ( 'NONE',  ( 1.033464566929134687, 0.06523048226347956391, 1.744586614173228245 ) ) ;
#40883 = AXIS2_PLACEMENT_3D ( 'NONE', #17521, #20641, #6494 ) ;
#40885 = CARTESIAN_POINT ( 'NONE',  ( -1.033464566929133799, 0.000000000000000000, 1.860236220472440971 ) ) ;
#40884 = AXIS2_PLACEMENT_3D ( 'NONE', #1087, #33734, #8524 ) ;
#40886 = CARTESIAN_POINT ( 'NONE',  ( -1.002407869896990045, 0.1264236179284866091, 1.877460629867496067 ) ) ;
#40887 = CARTESIAN_POINT ( 'NONE',  ( -1.002407869896990045, -0.1264236179284866091, 0.8833661416785196785 ) ) ;
#40888 = EDGE_CURVE ( 'NONE', #25222, #22261, #37417, .T. ) ;
#40889 = CARTESIAN_POINT ( 'NONE',  ( -0.6971942568897626646, 0.07405724077823318263, 0.5167322834108034613 ) ) ;
#40890 = CARTESIAN_POINT ( 'NONE',  ( -0.9873396505805591694, -0.1113553986120547346, 0.1131889762704257896 ) ) ;
#40891 = FACE_OUTER_BOUND ( 'NONE', #17354, .T. ) ;
#40892 = FACE_BOUND ( 'NONE', #17551, .T. ) ;
#40893 = CARTESIAN_POINT ( 'NONE',  ( 0.009906661468957056113, 0.04209688371799798906, -0.2797134572002689112 ) ) ;
#40894 = CARTESIAN_POINT ( 'NONE',  ( -0.2713383277233170632, 0.1500775187160215962, -0.8012127751235805784 ) ) ;
#40895 = CARTESIAN_POINT ( 'NONE',  ( -0.1787899950787401604, -0.4863444406701833977, 0.07405724077823318263 ) ) ;
#40896 = CARTESIAN_POINT ( 'NONE',  ( -0.2007511360401751932, -0.08955985698252086347, 0.1161810953340854241 ) ) ;
#40897 = CARTESIAN_POINT ( 'NONE',  ( 1.033464566929133799, 0.000000000000000000, 1.781496062992125928 ) ) ;
#40898 = CARTESIAN_POINT ( 'NONE',  ( 0.2559055126074655240, -0.08240829719531699016, -0.05512736142437904552 ) ) ;
#40899 = CARTESIAN_POINT ( 'NONE',  ( -1.054774247047244096, 0.000000000000000000, 0.2977362204186775885 ) ) ;
#40900 = CARTESIAN_POINT ( 'NONE',  ( 0.1264236179284866091, -1.773253889489082580, 0.1264236179284866091 ) ) ;
#40901 = EDGE_LOOP ( 'NONE', ( #44538, #25176, #4474, #21296 ) ) ;
#40902 = CARTESIAN_POINT ( 'NONE',  ( 0.2471922332844968817, -0.07944658092491525825, 0.07441910580888103088 ) ) ;
#40903 = ORIENTED_EDGE ( 'NONE', *, *, #8277, .T. ) ;
#40904 = CARTESIAN_POINT ( 'NONE',  ( 0.1787899950787401604, -1.361220472387181690, -0.07405724077823318263 ) ) ;
#40905 = CARTESIAN_POINT ( 'NONE',  ( -0.07405724077823318263, -1.543307086560409713, -0.1787899950787401604 ) ) ;
#40906 = CARTESIAN_POINT ( 'NONE',  ( 0.5962569168439626477, -0.09842519685039370636, 1.205361022782828805E-17 ) ) ;
#40907 = CARTESIAN_POINT ( 'NONE',  ( 1.033464566929134687, -0.06523048226347956391, 0.4404527559055117503 ) ) ;
#40908 = AXIS2_PLACEMENT_3D ( 'NONE', #23249, #33106, #14876 ) ;
#40909 = CARTESIAN_POINT ( 'NONE',  ( 0.5415383587465882886, -3.032960542342102697E-32, 0.09842519685039370636 ) ) ;
#40910 = CARTESIAN_POINT ( 'NONE',  ( -0.9412147342319837628, -0.1574803149606297803, 1.134350393593259509 ) ) ;
#40911 = CARTESIAN_POINT ( 'NONE',  ( 0.8019270111902717657, -0.1787899950787401604, 0.4872047243556847929 ) ) ;
#40912 = CARTESIAN_POINT ( 'NONE',  ( -7.939671275311751530E-17, -0.03219022224904082713, -0.2854330708661417804 ) ) ;
#40913 = CIRCLE ( 'NONE', #10381, 0.1574803149606299191 ) ;
#40914 = EDGE_LOOP ( 'NONE', ( #30678, #37731, #2763, #19745, #21278 ) ) ;
#40915 = CARTESIAN_POINT ( 'NONE',  ( 0.8107537697050253289, 0.1574803149606300301, 1.941437007766490863 ) ) ;
#40916 = ORIENTED_EDGE ( 'NONE', *, *, #27742, .T. ) ;
#40917 = EDGE_CURVE ( 'NONE', #43186, #29608, #35156, .T. ) ;
#40918 = CARTESIAN_POINT ( 'NONE',  ( -0.1219444983797640936, -0.09073875858372155989, -0.1307555171292179852 ) ) ;
#40919 = CARTESIAN_POINT ( 'NONE',  ( -0.8019270111902716547, -0.1787899950787401604, 0.9202755904974182499 ) ) ;
#40920 = CARTESIAN_POINT ( 'NONE',  ( 1.033464566929134687, 0.06523048226347956391, 0.8784448818897642175 ) ) ;
#40921 = DIRECTION ( 'NONE',  ( 0.000000000000000000, 1.000000000000000000, 0.000000000000000000 ) ) ;
#40922 = CARTESIAN_POINT ( 'NONE',  ( -0.1674689075051689624, -0.08956125648410076523, 0.01721656813326377655 ) ) ;
#40923 = ORIENTED_EDGE ( 'NONE', *, *, #23709, .F. ) ;
#40924 = EDGE_CURVE ( 'NONE', #23361, #5993, #17951, .T. ) ;
#40925 = CARTESIAN_POINT ( 'NONE',  ( 0.1558455157293398008, -0.05538006030750638325, -0.1377952755905511861 ) ) ;
#40926 = ORIENTED_EDGE ( 'NONE', *, *, #35537, .T. ) ;
#40927 = CARTESIAN_POINT ( 'NONE',  ( 0.9412147342319837628, 0.1574803149606300301, 1.277066929133857442 ) ) ;
#40928 = CARTESIAN_POINT ( 'NONE',  ( -1.033464566929133799, 0.000000000000000000, 0.9940944881889764995 ) ) ;
#40929 = CARTESIAN_POINT ( 'NONE',  ( -0.07405724077823318263, -1.543307086560409713, -0.1787899950787401604 ) ) ;
#40930 = CARTESIAN_POINT ( 'NONE',  ( -0.1264236179284866091, -0.9158464566391496531, -0.1264236179284866091 ) ) ;
#40931 = CARTESIAN_POINT ( 'NONE',  ( -0.1113553986120547346, -1.164370078740157632, 0.1113553986120547346 ) ) ;
#40932 = CARTESIAN_POINT ( 'NONE',  ( 0.8759842519685039353, 0.1574803149606299191, 1.112204724301921299 ) ) ;
#40933 = FACE_BOUND ( 'NONE', #37387, .T. ) ;
#40934 = CARTESIAN_POINT ( 'NONE',  ( -1.002407869896990045, 0.1264236179284866091, 0.4601377952218267953 ) ) ;
#40935 = VERTEX_POINT ( 'NONE', #18266 ) ;
#40936 = ORIENTED_EDGE ( 'NONE', *, *, #2376, .F. ) ;
#40937 = CARTESIAN_POINT ( 'NONE',  ( -0.7495606340400177148, -0.1264236179284866091, 1.705216535379307174 ) ) ;
#40938 = CARTESIAN_POINT ( 'NONE',  ( 0.8019270111902717657, 0.1787899950787401604, 1.653543307032850462 ) ) ;
#40939 = CARTESIAN_POINT ( 'NONE',  ( 0.06523048226347956391, -1.343996062884598386, 0.1574803149606297803 ) ) ;
#40940 = CARTESIAN_POINT ( 'NONE',  ( -0.7495606340400177148, -0.1264236179284866091, 0.8784448818360000022 ) ) ;
#40941 = DIRECTION ( 'NONE',  ( 0.000000000000000000, -1.000000000000000000, -0.000000000000000000 ) ) ;
#40942 = CYLINDRICAL_SURFACE ( 'NONE', #26684, 0.009842519685039378616 ) ;
#40943 = CARTESIAN_POINT ( 'NONE',  ( -0.9500414927467377701, -0.1787899950787401604, 1.313976377898992132 ) ) ;
#40944 = CARTESIAN_POINT ( 'NONE',  ( -0.6971942568897637749, 2.189545951927499583E-17, 0.9473425196312755814 ) ) ;
#40945 = CARTESIAN_POINT ( 'NONE',  ( -0.6971942568897626646, 0.07405724077823318263, 0.1624015747493861295 ) ) ;
#40946 = ( BOUNDED_CURVE ( )  B_SPLINE_CURVE ( 2, ( #26753, #23145, #15027, #11666, #44919, #8514, #41079, #19301, #41314 ),
 .UNSPECIFIED., .F., .F. ) 
 B_SPLINE_CURVE_WITH_KNOTS ( ( 3, 2, 2, 2, 3 ),
 ( 0.1100000000000000006, 0.1125000000000000028, 0.1150000000000000050, 0.1174999999999999933, 0.1199999999999999956 ),
 .UNSPECIFIED. ) 
 CURVE ( )  GEOMETRIC_REPRESENTATION_ITEM ( )  RATIONAL_B_SPLINE_CURVE ( ( 1.000000000000000000, 0.9238795325112869605, 1.000000000000000000, 0.9238795325112869605, 1.000000000000000000, 0.9238795325112869605, 1.000000000000000000, 0.9238795325112869605, 1.000000000000000000 ) ) 
 REPRESENTATION_ITEM ( '' )  ) ;
#40947 = DIRECTION ( 'NONE',  ( 0.000000000000000000, 0.9771240687918556489, 0.2126700594527794475 ) ) ;
#40948 = CARTESIAN_POINT ( 'NONE',  ( -0.6971942568897637749, 2.189545951927499583E-17, 1.621555118056472455 ) ) ;
#40949 = CARTESIAN_POINT ( 'NONE',  ( -0.6971942568897626646, 0.07405724077823318263, 0.04429133852891373180 ) ) ;
#40950 = ORIENTED_EDGE ( 'NONE', *, *, #30763, .T. ) ;
#40952 = CARTESIAN_POINT ( 'NONE',  ( -0.8070866141732283561, 0.000000000000000000, 0.8568897637795275246 ) ) ;
#40951 = AXIS2_PLACEMENT_3D ( 'NONE', #7396, #32352, #46930 ) ;
#40954 = ( BOUNDED_CURVE ( )  B_SPLINE_CURVE ( 2, ( #16517, #16052, #34262, #26837, #27328, #12464, #9565, #38552, #5233 ),
 .UNSPECIFIED., .F., .T. ) 
 B_SPLINE_CURVE_WITH_KNOTS ( ( 3, 2, 2, 2, 3 ),
 ( 0.4299999999999999933, 0.4324999999999999956, 0.4349999999999999978, 0.4375000000000000000, 0.4400000000000000022 ),
 .UNSPECIFIED. ) 
 CURVE ( )  GEOMETRIC_REPRESENTATION_ITEM ( )  RATIONAL_B_SPLINE_CURVE ( ( 1.000000000000000000, 0.9238795325112869605, 1.000000000000000000, 0.9238795325112869605, 1.000000000000000000, 0.9238795325112869605, 1.000000000000000000, 0.9238795325112869605, 1.000000000000000000 ) ) 
 REPRESENTATION_ITEM ( '' )  ) ;
#40953 = CARTESIAN_POINT ( 'NONE',  ( -0.9873396505805591694, -0.1113553986120547346, 1.540354330708661568 ) ) ;
#40955 = DIRECTION ( 'NONE',  ( 0.000000000000000000, 0.000000000000000000, -1.000000000000000000 ) ) ;
#40956 = CARTESIAN_POINT ( 'NONE',  ( 1.054774247047244096, 0.000000000000000000, 1.641240157426551161 ) ) ;
#40957 = CARTESIAN_POINT ( 'NONE',  ( -0.1275616080144442999, -0.09842519685039370636, -0.2189039336074421471 ) ) ;
#40958 = DIRECTION ( 'NONE',  ( 8.659560562353054383E-17, 0.7071067811867007835, -0.7071067811863941399 ) ) ;
#40959 = CARTESIAN_POINT ( 'NONE',  ( 0.000000000000000000, 0.1473293504822046074, -0.5595480905233950475 ) ) ;
#40960 = CIRCLE ( 'NONE', #28009, 0.09842519685039370636 ) ;
#40961 = VERTEX_POINT ( 'NONE', #42932 ) ;
#40962 = ORIENTED_EDGE ( 'NONE', *, *, #2794, .T. ) ;
#40963 = EDGE_LOOP ( 'NONE', ( #29555, #18625, #42490, #12871 ) ) ;
#40964 = CARTESIAN_POINT ( 'NONE',  ( 0.07405724077823318263, -0.8592519684501739308, 0.1787899950787401604 ) ) ;
#40965 = CARTESIAN_POINT ( 'NONE',  ( 0.1787899950787401882, -1.043799212544661348, -2.189545951927503898E-17 ) ) ;
#40966 = VERTEX_POINT ( 'NONE', #47262 ) ;
#40967 = DIRECTION ( 'NONE',  ( 1.000000000000000000, -0.000000000000000000, -0.000000000000000000 ) ) ;
#40968 = SHAPE_REPRESENTATION_RELATIONSHIP ( 'NONE' , 'NONE' ,  #40498, #43808 ) ;
#40969 = CARTESIAN_POINT ( 'NONE',  ( 0.8759842519685039353, -0.1787899950787401882, 1.705216535379307174 ) ) ;
#40970 = CARTESIAN_POINT ( 'NONE',  ( 0.1270800023317771588, -0.2913823922602110095, -0.1270800023317771588 ) ) ;
#40971 = FACE_OUTER_BOUND ( 'NONE', #23248, .T. ) ;
#40972 = PRODUCT_DEFINITION_SHAPE ( 'NONE', 'NONE',  #47461 ) ;
#40973 = CARTESIAN_POINT ( 'NONE',  ( 0.1264236179284866091, -0.1874999999462366451, 0.1264236179284866091 ) ) ;
#40974 = AXIS2_PLACEMENT_3D ( 'NONE', #41821, #35149, #31325 ) ;
#40975 = EDGE_CURVE ( 'NONE', #12211, #30513, #19460, .T. ) ;
#40976 = CARTESIAN_POINT ( 'NONE',  ( 0.8759842519685039353, -0.1787899950787401882, 0.8390748030958424808 ) ) ;
#40977 = ADVANCED_FACE ( 'NONE', ( #40048 ), #32530, .T. ) ;
#40979 = FACE_OUTER_BOUND ( 'NONE', #24492, .T. ) ;
#40978 = CARTESIAN_POINT ( 'NONE',  ( -1.054774247047244096, 0.000000000000000000, 1.995570866087968520 ) ) ;
#40980 = DIRECTION ( 'NONE',  ( 1.000000000000000000, 0.000000000000000000, 0.000000000000000000 ) ) ;
#40981 = CARTESIAN_POINT ( 'NONE',  ( -0.8107537697050254399, 0.1574803149606300301, 1.311515747923968744 ) ) ;
#40982 = CARTESIAN_POINT ( 'NONE',  ( 1.054774247047244540, -0.07405724077823318263, 1.756889763725764553 ) ) ;
#40983 = EDGE_CURVE ( 'NONE', #27278, #34093, #9905, .T. ) ;
#40984 = CIRCLE ( 'NONE', #44048, 0.4724409448818899238 ) ;
#40985 = EDGE_CURVE ( 'NONE', #39852, #17493, #21198, .T. ) ;
#40986 = CARTESIAN_POINT ( 'NONE',  ( 1.033464566929133799, 0.000000000000000000, 0.1279527559055118058 ) ) ;
#40987 = CARTESIAN_POINT ( 'NONE',  ( 0.1574803149606300023, 0.07021257666614877380, -0.1553045758542775656 ) ) ;
#40988 = CARTESIAN_POINT ( 'NONE',  ( -0.07405724077823318263, -0.3277559054580475584, -0.1787899950787401604 ) ) ;
#40989 = CARTESIAN_POINT ( 'NONE',  ( 0.1644020957507537628, 0.08115590401245550978, 0.1405661490837558925 ) ) ;
#40990 = CARTESIAN_POINT ( 'NONE',  ( -0.07405724077823318263, -1.252952755851747924, 0.1787899950787401604 ) ) ;
#40991 = CARTESIAN_POINT ( 'NONE',  ( 0.8019270111902717657, 0.1787899950787401604, 0.2755905511273391006 ) ) ;
#40992 = DIRECTION ( 'NONE',  ( 0.000000000000000000, -1.000000000000000000, -0.000000000000000000 ) ) ;
#40993 = CARTESIAN_POINT ( 'NONE',  ( -1.054774247047244540, 0.07405724077823318263, 1.717519684985606476 ) ) ;
#40994 = VERTEX_POINT ( 'NONE', #43118 ) ;
#40995 = CARTESIAN_POINT ( 'NONE',  ( -0.9500414927467378812, -0.1787899950787401604, 1.240157480261197431 ) ) ;
#40996 = LINE ( 'NONE', #33165, #38328 ) ;
#40997 = CARTESIAN_POINT ( 'NONE',  ( -1.002407869896990045, 0.1264236179284866091, 0.5044291338045039375 ) ) ;
#40998 = CARTESIAN_POINT ( 'NONE',  ( -0.8759842519685039353, -0.1787899950787401882, 1.075295275536787276 ) ) ;
#40999 = CARTESIAN_POINT ( 'NONE',  ( -0.1188990808483700867, -0.09842519868841002884, -0.1335248378736948738 ) ) ;
#41000 = CARTESIAN_POINT ( 'NONE',  ( 1.033464566929133799, 1.928577636452524610E-17, 2.007874015640504162 ) ) ;
#41001 = CARTESIAN_POINT ( 'NONE',  ( 0.8759842519685039353, -0.1787899950787401882, 0.4109251967966299213 ) ) ;
#41002 = CARTESIAN_POINT ( 'NONE',  ( -0.6971942568897648851, 0.07405724077823318263, 0.3543307086076538659 ) ) ;
#41003 = CARTESIAN_POINT ( 'NONE',  ( 0.9873396505805591694, -0.1113553986120547346, 1.687992125876724536 ) ) ;
#41004 = ORIENTED_EDGE ( 'NONE', *, *, #11885, .F. ) ;
#41005 = DIRECTION ( 'NONE',  ( 1.822029033848725028E-16, 0.000000000000000000, 1.000000000000000000 ) ) ;
#41006 = CARTESIAN_POINT ( 'NONE',  ( 0.6971942568897626646, 0.07405724077823318263, 0.9104330708123776761 ) ) ;
#41007 = CARTESIAN_POINT ( 'NONE',  ( -0.7185039370078746268, 0.06523048226347956391, 0.1058070866141733041 ) ) ;
#41008 = CARTESIAN_POINT ( 'NONE',  ( 0.9500414927467377701, 0.1787899950787401604, 1.215551181048599272 ) ) ;
#41009 = CARTESIAN_POINT ( 'NONE',  ( -0.6971942568897648851, -0.07405724077823297447, 1.973425196796630088 ) ) ;
#41010 = ORIENTED_EDGE ( 'NONE', *, *, #29238, .F. ) ;
#41011 = DIRECTION ( 'NONE',  ( 0.000000000000000000, 0.000000000000000000, 1.000000000000000000 ) ) ;
#41012 = CARTESIAN_POINT ( 'NONE',  ( 0.1554371429169570384, -0.1330479920330144283, -0.04514466913491271133 ) ) ;
#41013 = CARTESIAN_POINT ( 'NONE',  ( -1.033464566929133799, 0.000000000000000000, 0.2066929133858267931 ) ) ;
#41014 = CARTESIAN_POINT ( 'NONE',  ( 0.1264236179284866091, -1.458293259567820854, 0.1264236179284866091 ) ) ;
#41015 = EDGE_LOOP ( 'NONE', ( #11297, #25737, #30304, #42378 ) ) ;
#41016 = LINE ( 'NONE', #22833, #1938 ) ;
#41017 = CARTESIAN_POINT ( 'NONE',  ( 0.1264236179284866091, -0.4089566928596221063, -0.1264236179284866091 ) ) ;
#41018 = CARTESIAN_POINT ( 'NONE',  ( -0.7185039370078739607, 1.928577636452523993E-17, 1.712598425089322918 ) ) ;
#41019 = VERTEX_POINT ( 'NONE', #6706 ) ;
#41020 = CARTESIAN_POINT ( 'NONE',  ( 1.002407869896990045, -0.1264236179284866091, 1.355807086560409491 ) ) ;
#41021 = DIRECTION ( 'NONE',  ( -1.000000000000000000, 0.000000000000000000, 0.000000000000000000 ) ) ;
#41022 = CARTESIAN_POINT ( 'NONE',  ( -1.033464566929133799, 0.000000000000000000, 0.1279527559055118058 ) ) ;
#41023 = CARTESIAN_POINT ( 'NONE',  ( 0.6971942568897648851, 0.07405724077823318263, 1.535433070812378675 ) ) ;
#41024 = CARTESIAN_POINT ( 'NONE',  ( 1.054774247047244540, 0.07405724077823318263, 0.1033464566391498751 ) ) ;
#41025 = CARTESIAN_POINT ( 'NONE',  ( -0.1787899950787401604, 0.09928548058965885881, -0.07405724077823318263 ) ) ;
#41026 = CARTESIAN_POINT ( 'NONE',  ( -0.1787899950787401882, -1.693405511757259951, 0.000000000000000000 ) ) ;
#41027 = SHAPE_DEFINITION_REPRESENTATION ( #20868, #20643 ) ;
#41028 = DIRECTION ( 'NONE',  ( 1.000000000000000000, -0.000000000000000000, -0.000000000000000000 ) ) ;
#41029 = EDGE_CURVE ( 'NONE', #12184, #39650, #21319, .T. ) ;
#41030 = CARTESIAN_POINT ( 'NONE',  ( -0.9500414927467377701, -0.1787899950787401604, 0.7283464566391492090 ) ) ;
#41032 = DIRECTION ( 'NONE',  ( 0.000000000000000000, 0.000000000000000000, 1.000000000000000000 ) ) ;
#41031 = CARTESIAN_POINT ( 'NONE',  ( 0.1574803149606299191, -0.7165354330708662012, -1.928577636452523993E-17 ) ) ;
#41033 = CARTESIAN_POINT ( 'NONE',  ( -1.100456976456230270E-17, -1.467563494622415421, -0.1797182628040039365 ) ) ;
#41034 = FACE_OUTER_BOUND ( 'NONE', #35407, .T. ) ;
#41035 = DIRECTION ( 'NONE',  ( -1.000000000000000000, 3.469446951953613794E-15, 0.000000000000000000 ) ) ;
#41036 = CARTESIAN_POINT ( 'NONE',  ( 0.7495606340400177148, -0.1264236179284866091, 1.350885826717889815 ) ) ;
#41037 = CARTESIAN_POINT ( 'NONE',  ( 0.8759842519685039353, -0.1787899950787401882, 1.783956692859621995 ) ) ;
#41039 = ORIENTED_EDGE ( 'NONE', *, *, #17399, .F. ) ;
#41038 = CARTESIAN_POINT ( 'NONE',  ( -0.7185039370078739607, 1.928577636452523993E-17, 1.909448818790110192 ) ) ;
#41040 = EDGE_CURVE ( 'NONE', #32014, #18349, #39532, .T. ) ;
#41041 = CARTESIAN_POINT ( 'NONE',  ( 1.284448818897637956, -0.3937007874015748254, 1.181102362204724310 ) ) ;
#41042 = LINE ( 'NONE', #12811, #38168 ) ;
#41043 = CARTESIAN_POINT ( 'NONE',  ( -0.9412147342319837628, -0.1574803149606297803, 1.931594488188976166 ) ) ;
#41044 = CARTESIAN_POINT ( 'NONE',  ( 0.08946752424252873981, -0.5708661417322835607, 1.224299699984019663 ) ) ;
#41045 = CARTESIAN_POINT ( 'NONE',  ( 0.7495606340400177148, -0.1264236179284866091, 0.3617125983714334359 ) ) ;
#41046 = CARTESIAN_POINT ( 'NONE',  ( 0.7411008755701128381, -0.09968592455682778741, 0.03937258286176098521 ) ) ;
#41047 = DIRECTION ( 'NONE',  ( 0.000000000000000000, 0.000000000000000000, 1.000000000000000000 ) ) ;
#41048 = CARTESIAN_POINT ( 'NONE',  ( 0.7185039370078746268, 0.06523048226347956391, 0.6471456691838121111 ) ) ;
#41049 = VERTEX_POINT ( 'NONE', #6225 ) ;
#41050 = CARTESIAN_POINT ( 'NONE',  ( 1.033464566929131356, 0.06523048226348168721, 1.390255905511812218 ) ) ;
#41051 = CARTESIAN_POINT ( 'NONE',  ( 0.7185039370078741827, 0.06523048226347841205, 0.6963582677165353063 ) ) ;
#41052 = ORIENTED_EDGE ( 'NONE', *, *, #21866, .T. ) ;
#41053 = CARTESIAN_POINT ( 'NONE',  ( -0.07444174185955065859, 0.006353828212230052709, 0.1797182628040039087 ) ) ;
#41054 = CARTESIAN_POINT ( 'NONE',  ( -0.1264236179284866091, -1.220964566875370139, 0.1264236179284866091 ) ) ;
#41055 = CARTESIAN_POINT ( 'NONE',  ( -1.033464566929133799, 0.000000000000000000, 1.545275590551181244 ) ) ;
#41056 = CARTESIAN_POINT ( 'NONE',  ( 1.054774247047244540, 0.07405724077823318263, 1.599409448765135133 ) ) ;
#41057 = CARTESIAN_POINT ( 'NONE',  ( -0.8107537697050253289, -0.1574803149606297803, 1.218011811023622437 ) ) ;
#41058 = FACE_OUTER_BOUND ( 'NONE', #2834, .T. ) ;
#41060 = CARTESIAN_POINT ( 'NONE',  ( -0.9412147342319837628, -0.1574803149606297803, 0.4355314960629916299 ) ) ;
#41059 = CARTESIAN_POINT ( 'NONE',  ( -0.1574803149606300301, 0.04872047244094490637, -0.06523048226347956391 ) ) ;
#41061 = CARTESIAN_POINT ( 'NONE',  ( 0.9412147342319837628, -0.1574803149606297803, 1.921751968396409493 ) ) ;
#41062 = CARTESIAN_POINT ( 'NONE',  ( 0.1787899950787401882, -0.09891732278088229136, -2.189545951927503898E-17 ) ) ;
#41063 = CARTESIAN_POINT ( 'NONE',  ( 0.7646288533564489232, 0.1113553986120547346, 1.313976377845228249 ) ) ;
#41064 = ORIENTED_EDGE ( 'NONE', *, *, #7951, .F. ) ;
#41065 = ( BOUNDED_CURVE ( )  B_SPLINE_CURVE ( 3, ( #5924, #20542, #35177, #2325 ),
 .UNSPECIFIED., .F., .T. ) 
 B_SPLINE_CURVE_WITH_KNOTS ( ( 4, 4 ),
 ( 4.712388980384691450, 6.283185307179586232 ),
 .UNSPECIFIED. ) 
 CURVE ( )  GEOMETRIC_REPRESENTATION_ITEM ( )  RATIONAL_B_SPLINE_CURVE ( ( 1.000000000000000000, 0.8047378541243654926, 0.8047378541243654926, 1.000000000000000000 ) ) 
 REPRESENTATION_ITEM ( '' )  ) ;
#41066 = CARTESIAN_POINT ( 'NONE',  ( -0.6971942568897637749, 2.189545951927499583E-17, 1.577263779473795369 ) ) ;
#41067 = CARTESIAN_POINT ( 'NONE',  ( 0.06523048226347956391, 0.009350393808314452077, -0.1574803149606300301 ) ) ;
#41068 = CARTESIAN_POINT ( 'NONE',  ( -0.7495606340400177148, 0.1264236179284866091, 1.301673228292692830 ) ) ;
#41069 = ORIENTED_EDGE ( 'NONE', *, *, #37062, .F. ) ;
#41070 = CIRCLE ( 'NONE', #16613, 0.09842519685039370636 ) ;
#41071 = CARTESIAN_POINT ( 'NONE',  ( -0.6971942568897626646, -0.07405724077823297447, 0.2854330708123783422 ) ) ;
#41072 = CARTESIAN_POINT ( 'NONE',  ( 0.5962569168439626477, 4.766607801171850497E-17, 0.000000000000000000 ) ) ;
#41073 = DIRECTION ( 'NONE',  ( 0.000000000000000000, 0.000000000000000000, 1.000000000000000000 ) ) ;
#41074 = CARTESIAN_POINT ( 'NONE',  ( 0.07405724077823318263, -0.9095727871268751707, 0.1787899950787401604 ) ) ;
#41075 = ORIENTED_EDGE ( 'NONE', *, *, #20175, .T. ) ;
#41076 = CARTESIAN_POINT ( 'NONE',  ( 0.1787899950787401604, 0.01673228351833043817, 0.07405724077823318263 ) ) ;
#41077 = ORIENTED_EDGE ( 'NONE', *, *, #16885, .T. ) ;
#41078 = CARTESIAN_POINT ( 'NONE',  ( 0.9500414927467378812, -0.1787899950787401604, 1.038385826717890259 ) ) ;
#41079 = CARTESIAN_POINT ( 'NONE',  ( -0.9873396505805591694, -0.1113553986120547346, 0.2706692912310554866 ) ) ;
#41080 = CARTESIAN_POINT ( 'NONE',  ( 0.7646288533564489232, -0.1113553986120547346, 0.1033464565853864231 ) ) ;
#41081 = CARTESIAN_POINT ( 'NONE',  ( -1.033464566929133799, 1.928577636452524610E-17, 2.869337061179095023E-17 ) ) ;
#41082 = CARTESIAN_POINT ( 'NONE',  ( -0.07405724077823318263, -0.5098425196312756924, 0.1787899950787401604 ) ) ;
#41083 = ADVANCED_FACE ( 'NONE', ( #9845 ), #25613, .T. ) ;
#41084 = CARTESIAN_POINT ( 'NONE',  ( -0.6971942568897626646, -0.07405724077823297447, 0.2460629920722207653 ) ) ;
#41085 = CARTESIAN_POINT ( 'NONE',  ( -0.9873396505805591694, 0.1113553986120547346, 0.8809055118110236116 ) ) ;
#41086 = CARTESIAN_POINT ( 'NONE',  ( 0.5236220472440944462, 4.616380251121755931E-17, 0.000000000000000000 ) ) ;
#41087 = CARTESIAN_POINT ( 'NONE',  ( 0.1797182628040039087, -1.081244596984620499, -0.07444174185955065859 ) ) ;
#41088 = CARTESIAN_POINT ( 'NONE',  ( 0.9412147342319837628, 0.1574803149606300301, 0.4109251968503938590 ) ) ;
#41089 = CARTESIAN_POINT ( 'NONE',  ( -0.9412147342319837628, 0.1574803149606300301, 1.542814960522393308 ) ) ;
#41090 = CARTESIAN_POINT ( 'NONE',  ( 1.002407869896990045, -0.1264236179284866091, 0.8489173227808819444 ) ) ;
#41091 = DIRECTION ( 'NONE',  ( 0.000000000000000000, 0.000000000000000000, 1.000000000000000000 ) ) ;
#41092 = ADVANCED_FACE ( 'NONE', ( #37523 ), #4204, .T. ) ;
#41093 = CARTESIAN_POINT ( 'NONE',  ( 1.033464566929134687, 0.06523048226347956391, 1.429625984251968074 ) ) ;
#41095 = CARTESIAN_POINT ( 'NONE',  ( -1.033464566929133799, 0.000000000000000000, 1.860236220472440971 ) ) ;
#41094 = CARTESIAN_POINT ( 'NONE',  ( 0.7179901938900657976, 0.04576715322243130046, 1.982392704978442666 ) ) ;
#41096 = CARTESIAN_POINT ( 'NONE',  ( 0.8759842519685039353, 0.000000000000000000, 4.498031496062992574 ) ) ;
#41097 = AXIS2_PLACEMENT_3D ( 'NONE', #37482, #4634, #44886 ) ;
#41098 = CARTESIAN_POINT ( 'NONE',  ( -1.033464566929133799, 0.000000000000000000, 1.545275590551181244 ) ) ;
#41100 = DIRECTION ( 'NONE',  ( 1.000000000000000000, 0.000000000000000000, -1.822029033848725275E-16 ) ) ;
#41099 = CARTESIAN_POINT ( 'NONE',  ( 0.6971942568897648851, -0.07405724077823297447, 0.8316929133320636325 ) ) ;
#41101 = CARTESIAN_POINT ( 'NONE',  ( 0.6971942568897648851, -0.07405724077823297447, 1.781496062938362934 ) ) ;
#41102 = CARTESIAN_POINT ( 'NONE',  ( -0.1787899950787401604, -0.7460629920722210429, 0.07405724077823318263 ) ) ;
#41103 = CARTESIAN_POINT ( 'NONE',  ( 0.7185039370078739607, 1.928577636452523993E-17, 0.7381889763779527769 ) ) ;
#41104 = ORIENTED_EDGE ( 'NONE', *, *, #41843, .F. ) ;
#41105 = DIRECTION ( 'NONE',  ( 1.000000000000000000, 0.000000000000000000, 0.000000000000000000 ) ) ;
#41106 = CARTESIAN_POINT ( 'NONE',  ( 1.033464566929133799, 0.000000000000000000, 1.899606299212598604 ) ) ;
#41107 = CARTESIAN_POINT ( 'NONE',  ( -1.033464566929133799, 0.000000000000000000, 0.03937007863263043694 ) ) ;
#41108 = CARTESIAN_POINT ( 'NONE',  ( 1.054774247047244096, 0.000000000000000000, 1.203248031442299304 ) ) ;
#41109 = CARTESIAN_POINT ( 'NONE',  ( -0.7646288533564489232, 0.1113553986120547346, 1.048228346456692828 ) ) ;
#41110 = CARTESIAN_POINT ( 'NONE',  ( -0.1113553986120547346, -1.636811023622047223, 0.1113553986120547346 ) ) ;
#41111 = LINE ( 'NONE', #37072, #11507 ) ;
#41112 = CARTESIAN_POINT ( 'NONE',  ( -0.6971942568897626646, -0.07405724077823297447, 0.5167322834108034613 ) ) ;
#41113 = ORIENTED_EDGE ( 'NONE', *, *, #27906, .F. ) ;
#41114 = CARTESIAN_POINT ( 'NONE',  ( 0.1574803149606300023, -0.2274162997038010614, -0.9219983537151217323 ) ) ;
#41115 = CARTESIAN_POINT ( 'NONE',  ( -0.9500414927467378812, 0.1787899950787401604, 0.3051181101824569919 ) ) ;
#41116 = ORIENTED_EDGE ( 'NONE', *, *, #14353, .T. ) ;
#41117 = ORIENTED_EDGE ( 'NONE', *, *, #10738, .F. ) ;
#41118 = CARTESIAN_POINT ( 'NONE',  ( -0.1113553986120547346, 0.06594488199729076072, 0.1113553986120547346 ) ) ;
#41119 = CARTESIAN_POINT ( 'NONE',  ( 0.07405724077823318263, -1.528543307032852239, 0.1787899950787401604 ) ) ;
#41120 = CARTESIAN_POINT ( 'NONE',  ( -0.9500414927467378812, 0.1787899950787401604, 1.801181102308441861 ) ) ;
#41121 = CARTESIAN_POINT ( 'NONE',  ( -0.8759842519685039353, -0.1787899950787401882, 0.9571850393163149340 ) ) ;
#41122 = CARTESIAN_POINT ( 'NONE',  ( -0.6971942568897626646, -0.07405724077823297447, 0.5216535432533228045 ) ) ;
#41123 = CARTESIAN_POINT ( 'NONE',  ( -0.1564152455350579229, -0.4043437102334737077, -0.9276840032373354639 ) ) ;
#41124 = CARTESIAN_POINT ( 'NONE',  ( 3.284318927891251994E-17, -0.5970727871268759479, 0.1787899950787401882 ) ) ;
#41125 = CARTESIAN_POINT ( 'NONE',  ( -0.1827272056907964515, -0.08955978927791437283, 0.1407872760489078667 ) ) ;
#41126 = DIRECTION ( 'NONE',  ( 0.000000000000000000, -0.6156614753256598460, -0.7880107536067207930 ) ) ;
#41127 = CARTESIAN_POINT ( 'NONE',  ( 0.9412147342319837628, -0.1574803149606297803, 1.931594488188976166 ) ) ;
#41128 = VECTOR ( 'NONE', #35964, 39.37007874015748143 ) ;
#41129 = CARTESIAN_POINT ( 'NONE',  ( -0.6971942568897637749, 2.189545951927499583E-17, 0.4355314960092284138 ) ) ;
#41130 = CARTESIAN_POINT ( 'NONE',  ( -0.1787899950787401604, -1.790478298937899115, -0.07405724077823318263 ) ) ;
#41131 = ORIENTED_EDGE ( 'NONE', *, *, #10512, .F. ) ;
#41132 = CARTESIAN_POINT ( 'NONE',  ( 0.4811709046783464450, 1.205361022782824954E-17, -0.09842519685039370636 ) ) ;
#41133 = ORIENTED_EDGE ( 'NONE', *, *, #39382, .T. ) ;
#41134 = EDGE_CURVE ( 'NONE', #41392, #36971, #35561, .T. ) ;
#41135 = CARTESIAN_POINT ( 'NONE',  ( -0.8759842519685039353, -0.1787899950787401882, 1.513287401521039355 ) ) ;
#41136 = ORIENTED_EDGE ( 'NONE', *, *, #15157, .F. ) ;
#41137 = CARTESIAN_POINT ( 'NONE',  ( -0.07405724077823318263, -1.351377952702143004, -0.1787899950787401604 ) ) ;
#41138 = CARTESIAN_POINT ( 'NONE',  ( 3.284318927891251994E-17, -1.526082677111590513, 0.1787899950787401882 ) ) ;
#41139 = ADVANCED_FACE ( 'NONE', ( #15261 ), #604, .T. ) ;
#41140 = SURFACE_SIDE_STYLE ('',( #15562 ) ) ;
#41141 = CARTESIAN_POINT ( 'NONE',  ( -0.8759842519685039353, 0.000000000000000000, 0.000000000000000000 ) ) ;
#41142 = DIRECTION ( 'NONE',  ( -1.000000000000000000, 0.000000000000000000, 0.000000000000000000 ) ) ;
#41143 = CARTESIAN_POINT ( 'NONE',  ( -0.8759842519685039353, -0.1574803149606299191, 1.092519684931842594 ) ) ;
#41144 = CARTESIAN_POINT ( 'NONE',  ( 0.8759842519685039353, -0.1574803149606299191, 1.761811023514519459 ) ) ;
#41145 = CARTESIAN_POINT ( 'NONE',  ( 0.7646288533564489232, -0.1113553986120547346, 1.914370078632629868 ) ) ;
#41146 = EDGE_LOOP ( 'NONE', ( #15726, #33781, #32595, #12942, #26544, #20829, #12996, #6733 ) ) ;
#41147 = CARTESIAN_POINT ( 'NONE',  ( 1.033464566929133799, 0.000000000000000000, 1.033464566929133799 ) ) ;
#41148 = CARTESIAN_POINT ( 'NONE',  ( -0.9500414927467377701, -0.1787899950787401604, 1.082677165300567346 ) ) ;
#41149 = CARTESIAN_POINT ( 'NONE',  ( 0.8107537697050253289, 0.1574803149606300301, 0.8882874015748027929 ) ) ;
#41150 = CARTESIAN_POINT ( 'NONE',  ( 0.9412147342319837628, 0.1574803149606300301, 1.355807086614173596 ) ) ;
#41151 = CARTESIAN_POINT ( 'NONE',  ( 0.8759842519685039353, 0.000000000000000000, 4.498031496062992574 ) ) ;
#41152 = VECTOR ( 'NONE', #21261, 39.37007874015748143 ) ;
#41153 = CARTESIAN_POINT ( 'NONE',  ( -0.9873396505805591694, -0.1113553986120547346, 1.264763779527559029 ) ) ;
#41154 = CARTESIAN_POINT ( 'NONE',  ( -0.1307509148717837799, -0.08955578701844334188, 0.09650363397519905184 ) ) ;
#41155 = EDGE_LOOP ( 'NONE', ( #24772, #29533, #17380, #16532 ) ) ;
#41156 = LINE ( 'NONE', #34261, #24540 ) ;
#41157 = VERTEX_POINT ( 'NONE', #44225 ) ;
#41158 = LINE ( 'NONE', #22506, #39415 ) ;
#41159 = DIRECTION ( 'NONE',  ( 1.822029033848725028E-16, 0.000000000000000000, 1.000000000000000000 ) ) ;
#41160 = CARTESIAN_POINT ( 'NONE',  ( -0.1787899950787401882, -1.575295275536787276, 0.000000000000000000 ) ) ;
#41161 = CARTESIAN_POINT ( 'NONE',  ( -0.07405724077823318263, -0.8395669290800948925, -0.1787899950787401604 ) ) ;
#41163 = CIRCLE ( 'NONE', #15976, 0.2362204724409449064 ) ;
#41162 = CARTESIAN_POINT ( 'NONE',  ( 0.1574803149606300301, -1.147145669291337766, -0.06523048226347956391 ) ) ;
#41164 = CARTESIAN_POINT ( 'NONE',  ( 0.9412147342319837628, -0.1574803149606297803, 1.134350393593259509 ) ) ;
#41165 = DIRECTION ( 'NONE',  ( 0.000000000000000000, -0.6156614753256597350, -0.7880107536067206819 ) ) ;
#41166 = ORIENTED_EDGE ( 'NONE', *, *, #10414, .T. ) ;
#41167 = ORIENTED_EDGE ( 'NONE', *, *, #25337, .T. ) ;
#41168 = CARTESIAN_POINT ( 'NONE',  ( -0.8759842519685039353, -0.1787899950787401882, 1.710137795221826851 ) ) ;
#41169 = CARTESIAN_POINT ( 'NONE',  ( 0.7495606340400177148, -0.1264236179284866091, 1.705216535379307174 ) ) ;
#41170 = CARTESIAN_POINT ( 'NONE',  ( 2.892866454678787531E-17, -1.307086614065700703, 0.1574803149606299191 ) ) ;
#41171 = CARTESIAN_POINT ( 'NONE',  ( -0.8019270111902717657, -0.1787899950787401604, 0.8809055117572599514 ) ) ;
#41172 = DIRECTION ( 'NONE',  ( 0.000000000000000000, 0.000000000000000000, 1.000000000000000000 ) ) ;
#41173 = CARTESIAN_POINT ( 'NONE',  ( -1.054774247047244540, 0.07405724077823318263, 1.323818897584032817 ) ) ;
#41174 = DIRECTION ( 'NONE',  ( 0.000000000000000000, 0.000000000000000000, 1.000000000000000000 ) ) ;
#41175 = CARTESIAN_POINT ( 'NONE',  ( -0.7495606340400177148, -0.1264236179284866091, 1.188484251914740275 ) ) ;
#41176 = CARTESIAN_POINT ( 'NONE',  ( -0.7495606340400177148, -0.1264236179284866091, 0.9128937007336377363 ) ) ;
#41177 = CARTESIAN_POINT ( 'NONE',  ( -0.9412147342319837628, 0.1574803149606300301, 1.660925196742867982 ) ) ;
#41178 = CARTESIAN_POINT ( 'NONE',  ( -0.7495606340400177148, -0.1264236179284866091, 1.508366141678519678 ) ) ;
#41179 = CARTESIAN_POINT ( 'NONE',  ( -0.8759842519685039353, 0.1787899950787401882, 0.1156496062454492185 ) ) ;
#41180 = CARTESIAN_POINT ( 'NONE',  ( -0.9873396505805591694, 0.1113553986120547346, 1.589566929133858331 ) ) ;
#41181 = CARTESIAN_POINT ( 'NONE',  ( -1.033464566929134687, -0.06523048226347956391, 0.9522637795275589179 ) ) ;
#41182 = CARTESIAN_POINT ( 'NONE',  ( 0.8019270111902716547, -0.1787899950787401604, 1.550196850339938148 ) ) ;
#41183 = CARTESIAN_POINT ( 'NONE',  ( -0.1397729047152643789, -0.09842519685039370636, 0.1853948292088582472 ) ) ;
#41184 = DIRECTION ( 'NONE',  ( 0.000000000000000000, 0.000000000000000000, 1.000000000000000000 ) ) ;
#41185 = ORIENTED_EDGE ( 'NONE', *, *, #45276, .F. ) ;
#41186 = EDGE_CURVE ( 'NONE', #9479, #40003, #29908, .T. ) ;
#41187 = ORIENTED_EDGE ( 'NONE', *, *, #5867, .T. ) ;
#41188 = EDGE_CURVE ( 'NONE', #33274, #3817, #8753, .T. ) ;
#41189 = ORIENTED_EDGE ( 'NONE', *, *, #13221, .T. ) ;
#41190 = CARTESIAN_POINT ( 'NONE',  ( 0.07405724077823318263, -0.9379921259304876413, 0.1787899950787401604 ) ) ;
#41191 = CIRCLE ( 'NONE', #16753, 0.5905511811023621549 ) ;
#41192 = CARTESIAN_POINT ( 'NONE',  ( -1.094772975963752103E-17, -0.9945866141194644738, -0.1787899950787401882 ) ) ;
#41193 = DIRECTION ( 'NONE',  ( -0.5735764363510518216, -0.8191520442889876907, 0.000000000000000000 ) ) ;
#41194 = CARTESIAN_POINT ( 'NONE',  ( -0.1797182628040039087, -0.3971894788743842164, -0.07444174185955065859 ) ) ;
#41195 = CARTESIAN_POINT ( 'NONE',  ( -0.1574803149606300301, 0.1274606299212597549, -0.06523048226347956391 ) ) ;
#41196 = CARTESIAN_POINT ( 'NONE',  ( -0.1787899950787401882, -0.1628937007336379861, 0.000000000000000000 ) ) ;
#41197 = CARTESIAN_POINT ( 'NONE',  ( -0.8759842519685039353, 0.1574803149606299191, 0.1377952755905511861 ) ) ;
#41198 = CARTESIAN_POINT ( 'NONE',  ( 0.9500414927467378812, -0.1787899950787401604, 0.8415354330171019859 ) ) ;
#41200 = FACE_OUTER_BOUND ( 'NONE', #18847, .T. ) ;
#41199 = CARTESIAN_POINT ( 'NONE',  ( 1.033464566929133799, 1.928577636452524610E-17, 4.498031496062992574 ) ) ;
#41201 = FACE_OUTER_BOUND ( 'NONE', #11579, .T. ) ;
#41202 = DIRECTION ( 'NONE',  ( 0.000000000000000000, 0.000000000000000000, 1.000000000000000000 ) ) ;
#41203 = CARTESIAN_POINT ( 'NONE',  ( 0.9500414927467378812, 0.1787899950787401604, 1.806102362150961316 ) ) ;
#41204 = CARTESIAN_POINT ( 'NONE',  ( 0.8107537697050234415, -0.1574803149606297803, 0.1550196850393702197 ) ) ;
#41205 = DIRECTION ( 'NONE',  ( -1.000000000000000000, -0.000000000000000000, -0.000000000000000000 ) ) ;
#41206 = CARTESIAN_POINT ( 'NONE',  ( -0.07405724077823318263, -0.4852362204186770889, -0.1787899950787401604 ) ) ;
#41207 = CARTESIAN_POINT ( 'NONE',  ( 0.7185039370078739607, 1.928577636452523993E-17, 0.1082677165354330728 ) ) ;
#41208 = CARTESIAN_POINT ( 'NONE',  ( 0.1787899950787401604, -1.159448818843874074, -0.07405724077823318263 ) ) ;
#41209 = ( BOUNDED_CURVE ( )  B_SPLINE_CURVE ( 2, ( #38528, #28225, #2326, #13372, #24161, #20775, #17658, #5697, #42343 ),
 .UNSPECIFIED., .F., .F. ) 
 B_SPLINE_CURVE_WITH_KNOTS ( ( 3, 2, 2, 2, 3 ),
 ( 0.07000000000000000666, 0.07249999999999999500, 0.07499999999999999722, 0.07749999999999999944, 0.08000000000000000167 ),
 .UNSPECIFIED. ) 
 CURVE ( )  GEOMETRIC_REPRESENTATION_ITEM ( )  RATIONAL_B_SPLINE_CURVE ( ( 1.000000000000000000, 0.9238795325112859613, 1.000000000000000000, 0.9238795325112869605, 1.000000000000000000, 0.9238795325112869605, 1.000000000000000000, 0.9238795325112869605, 1.000000000000000000 ) ) 
 REPRESENTATION_ITEM ( '' )  ) ;
#41210 = CARTESIAN_POINT ( 'NONE',  ( 0.8019270111902717657, -0.1787899950787401604, 0.2903543306548980185 ) ) ;
#41211 = VECTOR ( 'NONE', #1757, 39.37007874015748143 ) ;
#41212 = CARTESIAN_POINT ( 'NONE',  ( -1.002407869896990045, -0.1264236179284866091, 1.788877952702141672 ) ) ;
#41213 = ORIENTED_EDGE ( 'NONE', *, *, #28604, .T. ) ;
#41214 = CARTESIAN_POINT ( 'NONE',  ( -1.002407869896990045, -0.1264236179284866091, 1.360728346402929168 ) ) ;
#41215 = CARTESIAN_POINT ( 'NONE',  ( -0.7646288533564489232, 0.1113553986120547346, 0.8907480314960629642 ) ) ;
#41216 = CIRCLE ( 'NONE', #31221, 0.1574803149606300579 ) ;
#41217 = CARTESIAN_POINT ( 'NONE',  ( -0.8019270111902717657, -0.1787899950787401604, 0.5659448818360001132 ) ) ;
#41218 = CARTESIAN_POINT ( 'NONE',  ( 1.054774247047244540, -0.07405724077823318263, 1.948818897584033927 ) ) ;
#41219 = CARTESIAN_POINT ( 'NONE',  ( -0.6971942568897637749, 2.189545951927499583E-17, 1.183562992072220599 ) ) ;
#41220 = CARTESIAN_POINT ( 'NONE',  ( 0.7185039370078739607, 1.928577636452523993E-17, 1.555118110128692832 ) ) ;
#41221 = CARTESIAN_POINT ( 'NONE',  ( -0.1138125304461556353, -0.09842519813797928618, -0.1380434466211696298 ) ) ;
#41222 = DIRECTION ( 'NONE',  ( -1.000000000000000000, 0.000000000000000000, 0.000000000000000000 ) ) ;
#41223 = CARTESIAN_POINT ( 'NONE',  ( 0.9500414927467377701, -0.1787899950787401604, 0.5314960629383620461 ) ) ;
#41224 = CARTESIAN_POINT ( 'NONE',  ( -0.7495606340400177148, 0.1264236179284866091, 0.4306102361667086820 ) ) ;
#41225 = ORIENTED_EDGE ( 'NONE', *, *, #13961, .T. ) ;
#41226 = DIRECTION ( 'NONE',  ( 1.000000000000000000, 0.000000000000000000, 0.000000000000000000 ) ) ;
#41227 = VERTEX_POINT ( 'NONE', #19063 ) ;
#41228 = CARTESIAN_POINT ( 'NONE',  ( 0.9500414927467378812, -0.1787899950787401604, 0.8858267715997791836 ) ) ;
#41229 = CARTESIAN_POINT ( 'NONE',  ( -1.033464566929134687, 0.06523048226347956391, 0.1697834645669291653 ) ) ;
#41230 = CIRCLE ( 'NONE', #37437, 0.1624015748031507056 ) ;
#41231 = DIRECTION ( 'NONE',  ( 0.000000000000000000, 0.000000000000000000, 1.000000000000000000 ) ) ;
#41232 = VERTEX_POINT ( 'NONE', #18833 ) ;
#41233 = EDGE_CURVE ( 'NONE', #33940, #29186, #23152, .T. ) ;
#41234 = CARTESIAN_POINT ( 'NONE',  ( -0.9873396505805591694, -0.1113553986120547346, 1.304133858267716661 ) ) ;
#41235 = EDGE_CURVE ( 'NONE', #31435, #39783, #27007, .T. ) ;
#41236 = PLANE ( 'NONE',  #42615 ) ;
#41237 = DIRECTION ( 'NONE',  ( 2.891205793294680298E-16, -1.000000000000000000, 0.000000000000000000 ) ) ;
#41238 = CARTESIAN_POINT ( 'NONE',  ( -0.07405724077823318263, -1.441068850119002542, -0.1787899950787401604 ) ) ;
#41239 = EDGE_LOOP ( 'NONE', ( #26835, #1673, #7326, #13214 ) ) ;
#41240 = CARTESIAN_POINT ( 'NONE',  ( 0.1787899950787401604, -0.4557086613635593086, 0.07405724077823318263 ) ) ;
#41241 = ADVANCED_FACE ( 'NONE', ( #1322 ), #4924, .T. ) ;
#41242 = CARTESIAN_POINT ( 'NONE',  ( -0.2713569170882992876, -0.1500457819031514040, 0.9508393013034962538 ) ) ;
#41243 = EDGE_LOOP ( 'NONE', ( #23893, #45856, #16572, #34629 ) ) ;
#41244 = CARTESIAN_POINT ( 'NONE',  ( 0.8759842519685039353, 0.1787899950787401882, 1.291830708607653477 ) ) ;
#41245 = EDGE_CURVE ( 'NONE', #18563, #5973, #30255, .T. ) ;
#41246 = CARTESIAN_POINT ( 'NONE',  ( -0.7185039370078741827, 0.06523048226347841205, 0.8439960628845994961 ) ) ;
#41247 = DIRECTION ( 'NONE',  ( 0.000000000000000000, 0.000000000000000000, -1.000000000000000000 ) ) ;
#41248 = CIRCLE ( 'NONE', #23678, 0.08090551181102362266 ) ;
#41249 = CARTESIAN_POINT ( 'NONE',  ( -0.8759842519685039353, 0.1574803149606299191, 1.437007874015747921 ) ) ;
#41250 = CARTESIAN_POINT ( 'NONE',  ( 0.8759842519685039353, -0.1787899950787401882, 1.547736220418677089 ) ) ;
#41251 = CARTESIAN_POINT ( 'NONE',  ( 1.002407869896990045, 0.1264236179284866091, 0.1058070865604098382 ) ) ;
#41252 = CARTESIAN_POINT ( 'NONE',  ( 0.1787899950787401604, -1.794291338528913426, -0.07405724077823318263 ) ) ;
#41253 = CARTESIAN_POINT ( 'NONE',  ( -0.1264236179284866091, -1.767224409395055318, 0.1264236179284866091 ) ) ;
#41254 = APPLICATION_PROTOCOL_DEFINITION ( 'draft international standard', 'automotive_design', 1998, #27872 ) ;
#41255 = CARTESIAN_POINT ( 'NONE',  ( -0.7185039370078739607, 1.928577636452523993E-17, 1.751968503829480106 ) ) ;
#41256 = ORIENTED_EDGE ( 'NONE', *, *, #24253, .F. ) ;
#41257 = AXIS2_PLACEMENT_3D ( 'NONE', #30979, #27402, #9632 ) ;
#41258 = CARTESIAN_POINT ( 'NONE',  ( -1.002407869896990045, 0.1264236179284866091, 0.6225393700249762796 ) ) ;
#41260 = DIRECTION ( 'NONE',  ( 1.000000000000000000, 0.000000000000000000, 0.000000000000000000 ) ) ;
#41259 = CARTESIAN_POINT ( 'NONE',  ( 0.06523048226347956391, -0.6697834645669303866, -0.1574803149606300301 ) ) ;
#41261 = CARTESIAN_POINT ( 'NONE',  ( 0.1270800023317771588, -1.482327274149974450, 0.1270800023317771588 ) ) ;
#41262 = DIRECTION ( 'NONE',  ( 0.000000000000000000, 0.000000000000000000, -1.000000000000000000 ) ) ;
#41263 = CARTESIAN_POINT ( 'NONE',  ( -0.1574803149606300301, -0.4532480313885357548, -0.06523048226347956391 ) ) ;
#41264 = LINE ( 'NONE', #26473, #36096 ) ;
#41265 = CARTESIAN_POINT ( 'NONE',  ( 0.8759842519685039353, 0.1787899950787401882, 1.336122047190330786 ) ) ;
#41266 = AXIS2_PLACEMENT_3D ( 'NONE', #21218, #32513, #35847 ) ;
#41267 = CARTESIAN_POINT ( 'NONE',  ( 0.9500414927467377701, 0.1787899950787401604, 1.919291338528913649 ) ) ;
#41269 = ORIENTED_EDGE ( 'NONE', *, *, #2578, .T. ) ;
#41268 = FACE_OUTER_BOUND ( 'NONE', #31689, .T. ) ;
#41270 = DIRECTION ( 'NONE',  ( 0.000000000000000000, 0.000000000000000000, -1.000000000000000000 ) ) ;
#41271 = DIRECTION ( 'NONE',  ( 1.000000000000000000, 0.000000000000000000, -1.822029033848725275E-16 ) ) ;
#41272 = CARTESIAN_POINT ( 'NONE',  ( 0.07405724077823318263, 0.04625984257344856188, 0.1787899950787401604 ) ) ;
#41273 = CARTESIAN_POINT ( 'NONE',  ( 0.000000000000000000, 0.000000000000000000, -0.0004999999999998990712 ) ) ;
#41274 = CARTESIAN_POINT ( 'NONE',  ( 0.8759842519685039353, 0.1787899950787401882, 0.3075787401037169411 ) ) ;
#41276 = CARTESIAN_POINT ( 'NONE',  ( 1.033464566929133799, 0.000000000000000000, 0.9055118109160944506 ) ) ;
#41275 = CARTESIAN_POINT ( 'NONE',  ( 0.8019270111902716547, 0.1787899950787401604, 1.294291338528913204 ) ) ;
#41277 = CARTESIAN_POINT ( 'NONE',  ( 0.1574803149606300023, 1.571700394971587755, -2.465016072061059660 ) ) ;
#41278 = CARTESIAN_POINT ( 'NONE',  ( -0.9412147342319837628, 0.1574803149606300301, 0.7652559055118115516 ) ) ;
#41279 = CARTESIAN_POINT ( 'NONE',  ( -0.8759842519685039353, 0.1787899950787401882, 1.331200787347811110 ) ) ;
#41280 = CARTESIAN_POINT ( 'NONE',  ( 0.7646288533564489232, 0.1113553986120547346, 0.8415354329633386588 ) ) ;
#41281 = ORIENTED_EDGE ( 'NONE', *, *, #35409, .F. ) ;
#41282 = CARTESIAN_POINT ( 'NONE',  ( -0.2056127690347618886, -0.3270319903728449717, -1.056505771383774661 ) ) ;
#41283 = ORIENTED_EDGE ( 'NONE', *, *, #35409, .T. ) ;
#41284 = CARTESIAN_POINT ( 'NONE',  ( -0.1797182628040039087, 0.001432568369710361233, 0.07444174185955065859 ) ) ;
#41285 = CARTESIAN_POINT ( 'NONE',  ( 0.1787899950787401882, -1.245570866087968520, -2.189545951927503898E-17 ) ) ;
#41286 = CARTESIAN_POINT ( 'NONE',  ( -0.7185039370078746268, -0.06523048226347956391, 1.213090551181103427 ) ) ;
#41287 = CARTESIAN_POINT ( 'NONE',  ( 0.7495606340400177148, -0.1264236179284866091, 1.542814960576157413 ) ) ;
#41288 = CARTESIAN_POINT ( 'NONE',  ( -1.033464566929133799, 0.000000000000000000, 1.230314960629921295 ) ) ;
#41289 = DIRECTION ( 'NONE',  ( 8.659560562358538199E-17, 0.7071067811862530306, -0.7071067811868418929 ) ) ;
#41291 = CARTESIAN_POINT ( 'NONE',  ( -0.8107537697050254399, -0.1574803149606297803, 0.4306102362204725642 ) ) ;
#41290 = CARTESIAN_POINT ( 'NONE',  ( -0.7185039370078746268, 0.06523048226347956391, 1.838090551181102317 ) ) ;
#41292 = CARTESIAN_POINT ( 'NONE',  ( -1.033464566929133799, 0.000000000000000000, 0.8759842519685039353 ) ) ;
#41293 = CARTESIAN_POINT ( 'NONE',  ( 0.8107537697050253289, -0.1574803149606297803, 1.326279527451528661 ) ) ;
#41294 = ORIENTED_EDGE ( 'NONE', *, *, #12367, .T. ) ;
#41295 = CONICAL_SURFACE ( 'NONE', #1533, 0.09842519685039370636, 0.9599310885968824758 ) ;
#41296 = CARTESIAN_POINT ( 'NONE',  ( 0.8759842519685039353, -0.1574803149606299191, 0.5905511811023621549 ) ) ;
#41297 = EDGE_LOOP ( 'NONE', ( #30129, #6797, #28771, #31250 ) ) ;
#41298 = CARTESIAN_POINT ( 'NONE',  ( 0.9500414927467378812, 0.1787899950787401604, 0.6643700786863929730 ) ) ;
#41299 = CARTESIAN_POINT ( 'NONE',  ( 0.8019270111902716547, -0.1787899950787401604, 0.9596456692375763264 ) ) ;
#41300 = CARTESIAN_POINT ( 'NONE',  ( 0.1113553986120547346, -0.08169291327829980576, 0.1113553986120547346 ) ) ;
#41301 = CARTESIAN_POINT ( 'NONE',  ( -0.6971942568897648851, -0.07405724077823297447, 1.309055118056472899 ) ) ;
#41302 = ORIENTED_EDGE ( 'NONE', *, *, #28773, .T. ) ;
#41303 = EDGE_CURVE ( 'NONE', #5973, #4993, #40852, .T. ) ;
#41304 = CARTESIAN_POINT ( 'NONE',  ( -1.054774247047244540, -0.07405724077823318263, 0.3789370078202520253 ) ) ;
#41305 = CARTESIAN_POINT ( 'NONE',  ( -0.4620708661417322616, 0.9842519685039375910, -0.7135826771653542844 ) ) ;
#41306 = CARTESIAN_POINT ( 'NONE',  ( 0.7185039370078746268, 0.06523048226347956391, 0.8833661416247559073 ) ) ;
#41307 = CARTESIAN_POINT ( 'NONE',  ( 0.07405724077823318263, -1.012919243819789594, -0.1787899950787401604 ) ) ;
#41308 = VERTEX_POINT ( 'NONE', #15979 ) ;
#41309 = CARTESIAN_POINT ( 'NONE',  ( 0.1264236179284866091, 0.05364173233722803469, 0.1264236179284866091 ) ) ;
#41310 = ORIENTED_EDGE ( 'NONE', *, *, #36382, .T. ) ;
#41311 = VERTEX_POINT ( 'NONE', #1085 ) ;
#41312 = APPLICATION_CONTEXT ( 'automotive_design' ) ;
#41313 = EDGE_CURVE ( 'NONE', #8358, #6083, #23308, .T. ) ;
#41314 = CARTESIAN_POINT ( 'NONE',  ( -1.033464566929133799, 0.000000000000000000, 0.2755905510735752184 ) ) ;
#41315 = CARTESIAN_POINT ( 'NONE',  ( -0.2362204724409464329, 0.1574803149606323616, 1.186023622047244208 ) ) ;
#41316 = CARTESIAN_POINT ( 'NONE',  ( 0.1787899950787401604, -0.6919291338045056028, -0.07405724077823318263 ) ) ;
#41317 = CONICAL_SURFACE ( 'NONE', #6143, 0.09842519685039310962, 0.7853981633972314524 ) ;
#41318 = CARTESIAN_POINT ( 'NONE',  ( -0.8019270111902716547, -0.1787899950787401604, 0.2509842519147403861 ) ) ;
#41319 = CARTESIAN_POINT ( 'NONE',  ( -1.033464566929133799, 0.000000000000000000, 0.8759842519685039353 ) ) ;
#41320 = DIRECTION ( 'NONE',  ( -1.000000000000000000, 0.000000000000000000, 0.000000000000000000 ) ) ;
#41321 = CARTESIAN_POINT ( 'NONE',  ( 0.07444174185955046430, -0.9582131009216291462, -0.1797182628040039087 ) ) ;
#41322 = CARTESIAN_POINT ( 'NONE',  ( -0.7646288533564489232, 0.1113553986120547346, 1.943897637687747926 ) ) ;
#41323 = CARTESIAN_POINT ( 'NONE',  ( 0.7495606340400177148, -0.1264236179284866091, 0.9965551180564724554 ) ) ;
#41324 = CARTESIAN_POINT ( 'NONE',  ( 1.054774247047244540, 0.07405724077823318263, 1.402559055064346749 ) ) ;
#41325 = CONICAL_SURFACE ( 'NONE', #25298, 0.1673228346456692994, 0.7853981633974532750 ) ;
#41326 = CARTESIAN_POINT ( 'NONE',  ( 0.9873396505805591694, 0.1113553986120547346, 0.5167322833570401341 ) ) ;
#41327 = CARTESIAN_POINT ( 'NONE',  ( 0.7185039370078739607, 1.928577636452523993E-17, 1.643700787401574992 ) ) ;
#41329 = CARTESIAN_POINT ( 'NONE',  ( 1.033464566929133799, 1.928577636452524610E-17, 4.498031496062992574 ) ) ;
#41328 = CARTESIAN_POINT ( 'NONE',  ( 0.7125420959524927378, -0.03489325537972703950, 1.983914969194383371 ) ) ;
#41330 = FACE_OUTER_BOUND ( 'NONE', #39822, .T. ) ;
#41331 = CARTESIAN_POINT ( 'NONE',  ( -0.1787899950787401882, 0.07824803154982658271, 0.000000000000000000 ) ) ;
#41332 = ( BOUNDED_CURVE ( )  B_SPLINE_CURVE ( 2, ( #20190, #8946, #9429, #31476, #27897, #20432, #38649, #34841, #35066 ),
 .UNSPECIFIED., .F., .T. ) 
 B_SPLINE_CURVE_WITH_KNOTS ( ( 3, 2, 2, 2, 3 ),
 ( 0.02000000000000000042, 0.02249999999999999917, 0.02500000000000000139, 0.02750000000000000014, 0.02999999999999999889 ),
 .UNSPECIFIED. ) 
 CURVE ( )  GEOMETRIC_REPRESENTATION_ITEM ( )  RATIONAL_B_SPLINE_CURVE ( ( 1.000000000000000000, 0.9238795325112869605, 1.000000000000000000, 0.9238795325112869605, 1.000000000000000000, 0.9238795325112869605, 1.000000000000000000, 0.9238795325112869605, 1.000000000000000000 ) ) 
 REPRESENTATION_ITEM ( '' )  ) ;
#41333 = FACE_OUTER_BOUND ( 'NONE', #46865, .T. ) ;
#41335 = CARTESIAN_POINT ( 'NONE',  ( -1.033464566929133799, 0.000000000000000000, 1.427165354330708569 ) ) ;
#41334 = CARTESIAN_POINT ( 'NONE',  ( 0.7495606340400177148, 0.1264236179284866091, 0.9817913385289134265 ) ) ;
#41336 = CARTESIAN_POINT ( 'NONE',  ( 0.9500414927467377701, 0.1787899950787401604, 1.806102362150961094 ) ) ;
#41337 = CARTESIAN_POINT ( 'NONE',  ( -0.1264236179284866091, -0.9502952755367874982, -0.1264236179284866091 ) ) ;
#41338 = EDGE_LOOP ( 'NONE', ( #40582, #40903, #36908, #44662 ) ) ;
#41339 = CARTESIAN_POINT ( 'NONE',  ( -0.7185039370078746268, 0.06523048226347956391, 0.8538385826771661691 ) ) ;
#41340 = CARTESIAN_POINT ( 'NONE',  ( 0.1574803149606299191, -1.730314960522393752, -1.928577636452523993E-17 ) ) ;
#41341 = CARTESIAN_POINT ( 'NONE',  ( -0.8759842519685039353, 0.1574803149606299191, 0.04921259831766984505 ) ) ;
#41342 = CARTESIAN_POINT ( 'NONE',  ( 0.9500414927467378812, -0.1787899950787401604, 1.077755905458048113 ) ) ;
#41343 = CARTESIAN_POINT ( 'NONE',  ( 0.1753418932787807749, 0.1299212598425196763, 0.07262899196590184847 ) ) ;
#41344 = CARTESIAN_POINT ( 'NONE',  ( 0.1574803149606300301, -1.742618110236221041, 0.06523048226347956391 ) ) ;
#41345 = CARTESIAN_POINT ( 'NONE',  ( 0.3980944881889786346, 0.6449983665207559280, -0.7480314960629920185 ) ) ;
#41346 = CARTESIAN_POINT ( 'NONE',  ( -1.033464566929134687, -0.06523048226347956391, 0.2829724409448821643 ) ) ;
#41347 = CARTESIAN_POINT ( 'NONE',  ( -0.9500414927467378812, 0.1787899950787401604, 0.2263779527021421711 ) ) ;
#41348 = ORIENTED_EDGE ( 'NONE', *, *, #5999, .T. ) ;
#41349 = CARTESIAN_POINT ( 'NONE',  ( -0.1787899950787401604, -1.464566929080096225, -0.07405724077823318263 ) ) ;
#41350 = CARTESIAN_POINT ( 'NONE',  ( -0.8019270111902717657, -0.1787899950787401604, 1.860236220418677089 ) ) ;
#41351 = CARTESIAN_POINT ( 'NONE',  ( -0.8019270111902716547, -0.1787899950787401604, 0.9547244093950545407 ) ) ;
#41352 = CARTESIAN_POINT ( 'NONE',  ( -0.7495606340400177148, 0.1264236179284866091, 0.5930118109698583329 ) ) ;
#41353 = ( BOUNDED_CURVE ( )  B_SPLINE_CURVE ( 2, ( #3469, #28663, #43229, #25034, #7057, #39629, #6810, #47319, #14494 ),
 .UNSPECIFIED., .F., .T. ) 
 B_SPLINE_CURVE_WITH_KNOTS ( ( 3, 2, 2, 2, 3 ),
 ( 0.2800000000000000266, 0.2824999999999999734, 0.2849999999999999756, 0.2874999999999999778, 0.2899999999999999800 ),
 .UNSPECIFIED. ) 
 CURVE ( )  GEOMETRIC_REPRESENTATION_ITEM ( )  RATIONAL_B_SPLINE_CURVE ( ( 1.000000000000000000, 0.9238795325112869605, 1.000000000000000000, 0.9238795325112869605, 1.000000000000000000, 0.9238795325112869605, 1.000000000000000000, 0.9238795325112869605, 1.000000000000000000 ) ) 
 REPRESENTATION_ITEM ( '' )  ) ;
#41354 = ADVANCED_FACE ( 'NONE', ( #23396 ), #11072, .T. ) ;
#41355 = CIRCLE ( 'NONE', #14611, 0.1624015748031505668 ) ;
#41356 = LINE ( 'NONE', #34230, #10209 ) ;
#41357 = CARTESIAN_POINT ( 'NONE',  ( -0.9873396505805591694, 0.1113553986120547346, 1.668307086614173373 ) ) ;
#41358 = CARTESIAN_POINT ( 'NONE',  ( -1.094772975963752103E-17, -0.6167578264969547641, -0.1787899950787401882 ) ) ;
#41359 = CARTESIAN_POINT ( 'NONE',  ( 0.1048138276931706719, -0.09842519685039370636, 0.1042338764169748050 ) ) ;
#41360 = DIRECTION ( 'NONE',  ( -1.000000000000000000, 0.000000000000000000, 0.000000000000000000 ) ) ;
#41361 = DIRECTION ( 'NONE',  ( 0.000000000000000000, 0.000000000000000000, 1.000000000000000000 ) ) ;
#41362 = ( GEOMETRIC_REPRESENTATION_CONTEXT ( 3 ) GLOBAL_UNCERTAINTY_ASSIGNED_CONTEXT ( ( #8130 ) ) GLOBAL_UNIT_ASSIGNED_CONTEXT ( ( #44890, #29417, #43962 ) ) REPRESENTATION_CONTEXT ( 'NONE', 'WORKASPACE' ) ) ;
#41363 = EDGE_CURVE ( 'NONE', #46267, #33937, #14897, .T. ) ;
#41365 = CARTESIAN_POINT ( 'NONE',  ( 0.2559055108844309201, -0.04382127000173715453, -0.03538492399873669619 ) ) ;
#41364 = AXIS2_PLACEMENT_3D ( 'NONE', #35937, #3097, #17723 ) ;
#41366 = CARTESIAN_POINT ( 'NONE',  ( -0.8019270111902717657, -0.1787899950787401604, 0.4035433070328508509 ) ) ;
#41367 = CARTESIAN_POINT ( 'NONE',  ( -0.1264236179284866091, -1.792938928859161507, -0.1264236179284866091 ) ) ;
#41368 = ORIENTED_EDGE ( 'NONE', *, *, #35882, .T. ) ;
#41369 = CARTESIAN_POINT ( 'NONE',  ( 0.1377952755905511029, 0.000000000000000000, -0.3149606299212598381 ) ) ;
#41370 = CARTESIAN_POINT ( 'NONE',  ( -0.6971942568897637749, 2.189545951927499583E-17, 1.582185039316315045 ) ) ;
#41371 = CARTESIAN_POINT ( 'NONE',  ( 0.1787899950787401604, -1.366141732229700478, 0.07405724077823318263 ) ) ;
#41372 = CARTESIAN_POINT ( 'NONE',  ( 0.07405724077823318263, -1.484251968450174930, 0.1787899950787401604 ) ) ;
#41373 = ( LENGTH_UNIT ( ) NAMED_UNIT ( * ) SI_UNIT ( $, .METRE. ) ) ;
#41374 = CARTESIAN_POINT ( 'NONE',  ( 0.7185039370078739607, 0.000000000000000000, 4.498031496062992574 ) ) ;
#41375 = CARTESIAN_POINT ( 'NONE',  ( 0.8107537697050253289, -0.1574803149606297803, 0.4699803149606304742 ) ) ;
#41376 = DIRECTION ( 'NONE',  ( 0.000000000000000000, -1.073081856240829922E-16, -1.000000000000000000 ) ) ;
#41377 = CARTESIAN_POINT ( 'NONE',  ( -0.7185039370078746268, 0.06523048226347956391, 1.158956692805858113 ) ) ;
#41378 = CARTESIAN_POINT ( 'NONE',  ( 0.7495606340400177148, -0.1264236179284866091, 0.6028543306548976854 ) ) ;
#41380 = DIRECTION ( 'NONE',  ( 0.000000000000000000, 0.000000000000000000, 1.000000000000000000 ) ) ;
#41379 = CARTESIAN_POINT ( 'NONE',  ( -0.1574803149606299191, -0.3425196850393700809, 0.000000000000000000 ) ) ;
#41381 = CARTESIAN_POINT ( 'NONE',  ( 0.7646288533564489232, 0.1113553986120547346, 1.943897637687747926 ) ) ;
#41382 = EDGE_LOOP ( 'NONE', ( #45305, #45922 ) ) ;
#41383 = CARTESIAN_POINT ( 'NONE',  ( -0.8070866141732283561, -0.0009842519685049383633, 0.7574803149606299524 ) ) ;
#41384 = CARTESIAN_POINT ( 'NONE',  ( -1.002407869896990045, 0.1264236179284866091, 1.134350393647023614 ) ) ;
#41385 = CARTESIAN_POINT ( 'NONE',  ( 1.033464566929133799, 0.000000000000000000, 1.033464566929133799 ) ) ;
#41386 = CARTESIAN_POINT ( 'NONE',  ( -1.033464566929133799, 0.000000000000000000, 0.7086614172153071767 ) ) ;
#41387 = CARTESIAN_POINT ( 'NONE',  ( 0.1574803149606300301, -0.5516732282389297248, 0.06523048226347956391 ) ) ;
#41388 = AXIS2_PLACEMENT_3D ( 'NONE', #34599, #1750, #9433 ) ;
#41389 = FACE_OUTER_BOUND ( 'NONE', #11194, .T. ) ;
#41390 = CARTESIAN_POINT ( 'NONE',  ( 0.6195511811023624027, 0.9842519685039365918, -0.7135826771653542844 ) ) ;
#41391 = CARTESIAN_POINT ( 'NONE',  ( -0.1406443466276429688, -0.08955922997629965632, 0.08377781526596418671 ) ) ;
#41392 = VERTEX_POINT ( 'NONE', #35127 ) ;
#41393 = DIRECTION ( 'NONE',  ( 1.000000000000000000, 0.000000000000000000, 0.000000000000000000 ) ) ;
#41394 = VECTOR ( 'NONE', #27479, 39.37007874015748143 ) ;
#41396 = CARTESIAN_POINT ( 'NONE',  ( -0.3010001048904012988, 0.07502508536398720673, 0.7260280747557159575 ) ) ;
#41395 = ( GEOMETRIC_REPRESENTATION_CONTEXT ( 3 ) GLOBAL_UNCERTAINTY_ASSIGNED_CONTEXT ( ( #458 ) ) GLOBAL_UNIT_ASSIGNED_CONTEXT ( ( #21946, #43010, #6605 ) ) REPRESENTATION_CONTEXT ( 'NONE', 'WORKASPACE' ) ) ;
#41397 = CARTESIAN_POINT ( 'NONE',  ( 0.8019270111902717657, 0.1787899950787401604, 0.7431102361667091261 ) ) ;
#41398 = ORIENTED_EDGE ( 'NONE', *, *, #6559, .T. ) ;
#41399 = CARTESIAN_POINT ( 'NONE',  ( -0.7185039370078739607, 1.928577636452523993E-17, 1.791338582569637738 ) ) ;
#41400 = CARTESIAN_POINT ( 'NONE',  ( -0.1113553986120547346, -0.02263779527559055260, 0.1113553986120547346 ) ) ;
#41401 = CARTESIAN_POINT ( 'NONE',  ( 0.1264236179284866091, -1.678641732229700922, 0.1264236179284866091 ) ) ;
#41402 = CARTESIAN_POINT ( 'NONE',  ( 0.1787899950787401882, -0.8912401574265511606, -2.189545951927503898E-17 ) ) ;
#41403 = VECTOR ( 'NONE', #22197, 39.37007874015748854 ) ;
#41404 = CARTESIAN_POINT ( 'NONE',  ( -0.1574803149606297803, -1.166830708661416693, 0.06523048226347956391 ) ) ;
#41405 = CARTESIAN_POINT ( 'NONE',  ( 0.8759842519685039353, 0.1574803149606299191, 1.190944881782236342 ) ) ;
#41406 = DIRECTION ( 'NONE',  ( 1.217491584052838080E-15, 0.6156614753256588468, 0.7880107536067214591 ) ) ;
#41407 = ORIENTED_EDGE ( 'NONE', *, *, #36586, .F. ) ;
#41408 = ORIENTED_EDGE ( 'NONE', *, *, #28056, .F. ) ;
#41409 = CARTESIAN_POINT ( 'NONE',  ( -1.054774247047244096, 0.000000000000000000, 1.759350393647023614 ) ) ;
#41410 = CARTESIAN_POINT ( 'NONE',  ( 0.6971942568897648851, -0.07405724077823297447, 1.781496062938362934 ) ) ;
#41411 = ORIENTED_EDGE ( 'NONE', *, *, #38778, .F. ) ;
#41412 = CARTESIAN_POINT ( 'NONE',  ( 0.1113553986120547346, -1.380905511703496069, 0.1113553986120547346 ) ) ;
#41413 = FACE_BOUND ( 'NONE', #27537, .T. ) ;
#41414 = CARTESIAN_POINT ( 'NONE',  ( 0.6971942568897637749, 2.189545951927499583E-17, 0.4404527558517480901 ) ) ;
#41415 = CARTESIAN_POINT ( 'NONE',  ( -1.054774247047244540, -0.07405724077823318263, 1.358267716481669662 ) ) ;
#41416 = CARTESIAN_POINT ( 'NONE',  ( 0.02156745609636135860, 0.2830359600832316747, -0.2989494884453828272 ) ) ;
#41417 = CARTESIAN_POINT ( 'NONE',  ( -1.054774247047244540, 0.07405724077823318263, 1.284448818843874518 ) ) ;
#41418 = CARTESIAN_POINT ( 'NONE',  ( -0.6971942568897637749, 2.189545951927499583E-17, 0.8686023621509606496 ) ) ;
#41419 = CARTESIAN_POINT ( 'NONE',  ( -1.002407869896990045, -0.1264236179284866091, 0.1008858267178899676 ) ) ;
#41420 = ADVANCED_FACE ( 'NONE', ( #45880 ), #2273, .T. ) ;
#41421 = DIRECTION ( 'NONE',  ( 1.000000000000000000, 0.000000000000000000, 0.000000000000000000 ) ) ;
#41422 = CARTESIAN_POINT ( 'NONE',  ( -0.9500414927467378812, -0.1787899950787401604, 1.791338582623401177 ) ) ;
#41423 = CARTESIAN_POINT ( 'NONE',  ( -0.7495606340400177148, 0.1264236179284866091, 0.04183070860765386589 ) ) ;
#41424 = DIRECTION ( 'NONE',  ( 1.267059173938978811E-30, 3.652049423109077687E-16, -1.000000000000000000 ) ) ;
#41425 = CARTESIAN_POINT ( 'NONE',  ( -0.7185039370078746268, 0.06523048226347956391, 1.759350393700787940 ) ) ;
#41426 = CARTESIAN_POINT ( 'NONE',  ( -1.033464566929133799, 0.000000000000000000, 0.2854330708661417804 ) ) ;
#41427 = CARTESIAN_POINT ( 'NONE',  ( 0.8759842519685039353, 0.1787899950787401882, 1.651082677111590513 ) ) ;
#41428 = CARTESIAN_POINT ( 'NONE',  ( -0.2379070121699287110, -0.09842519685039370636, 0.03196672700780228693 ) ) ;
#41429 = CARTESIAN_POINT ( 'NONE',  ( -0.3100393700787401619, 0.000000000000000000, 1.181102362204724310 ) ) ;
#41430 = ORIENTED_EDGE ( 'NONE', *, *, #43036, .T. ) ;
#41431 = EDGE_CURVE ( 'NONE', #28079, #17196, #15077, .T. ) ;
#41432 = EDGE_CURVE ( 'NONE', #23848, #12702, #1879, .T. ) ;
#41433 = ORIENTED_EDGE ( 'NONE', *, *, #4104, .F. ) ;
#41434 = EDGE_LOOP ( 'NONE', ( #26751, #15835, #14418, #20776 ) ) ;
#41435 = CONICAL_SURFACE ( 'NONE', #16977, 0.1574803149606299191, 0.9599310885968735940 ) ;
#41436 = CARTESIAN_POINT ( 'NONE',  ( 0.1264236179284866091, -0.8961614172690708369, 0.1264236179284866091 ) ) ;
#41437 = CARTESIAN_POINT ( 'NONE',  ( 0.1787899950787401604, -1.124999999946237228, 0.07405724077823318263 ) ) ;
#41438 = CYLINDRICAL_SURFACE ( 'NONE', #15666, 0.09842519685039370636 ) ;
#41439 = CARTESIAN_POINT ( 'NONE',  ( 0.8759842519685039353, 0.1787899950787401882, 1.843011810969858333 ) ) ;
#41440 = CARTESIAN_POINT ( 'NONE',  ( 0.1797182628040039087, -0.2938430221814707366, -0.07444174185955065859 ) ) ;
#41441 = CARTESIAN_POINT ( 'NONE',  ( 0.06523048226347956391, 0.1028543307086613318, 0.1574803149606297803 ) ) ;
#41442 = LENGTH_MEASURE_WITH_UNIT ( LENGTH_MEASURE( 0.02539999999999999897 ), #5051 ) ;
#41443 = CARTESIAN_POINT ( 'NONE',  ( 0.7185039370078746268, -0.06523048226347956391, 0.1008858266641264878 ) ) ;
#41444 = EDGE_CURVE ( 'NONE', #43211, #47206, #11717, .T. ) ;
#41445 = CARTESIAN_POINT ( 'NONE',  ( 0.9412147342319837628, 0.1574803149606300301, 0.1747047244094488694 ) ) ;
#41446 = DIRECTION ( 'NONE',  ( 0.000000000000000000, 1.000000000000000000, 0.000000000000000000 ) ) ;
#41448 = CARTESIAN_POINT ( 'NONE',  ( 0.1264236179284866091, -0.4630905511273386010, 0.1264236179284866091 ) ) ;
#41447 = CARTESIAN_POINT ( 'NONE',  ( 2.892866454678787531E-17, -0.9921259841444409755, 0.1574803149606299191 ) ) ;
#41449 = CARTESIAN_POINT ( 'NONE',  ( 0.2383973256948878072, 0.3740157480314960647, 1.112073044918586717 ) ) ;
#41450 = CARTESIAN_POINT ( 'NONE',  ( -0.1787899950787401604, -1.257874015694269376, 0.07405724077823318263 ) ) ;
#41451 = CARTESIAN_POINT ( 'NONE',  ( 0.9500414927467378812, 0.1787899950787401604, 0.3100393700249766682 ) ) ;
#41452 = DIRECTION ( 'NONE',  ( 1.000000000000000000, 0.000000000000000000, -1.822029033848725275E-16 ) ) ;
#41453 = CARTESIAN_POINT ( 'NONE',  ( -1.054774247047244540, 0.07405724077823318263, 1.678149606245448622 ) ) ;
#41454 = EDGE_LOOP ( 'NONE', ( #41833, #38364, #22455, #18167, #23412, #29995 ) ) ;
#41455 = CARTESIAN_POINT ( 'NONE',  ( -0.7495606340400177148, 0.1264236179284866091, 1.262303149552535420 ) ) ;
#41456 = ADVANCED_FACE ( 'NONE', ( #28481 ), #17201, .F. ) ;
#41457 = CARTESIAN_POINT ( 'NONE',  ( 1.002407869896990045, 0.1264236179284866091, 1.449311023568283341 ) ) ;
#41458 = CARTESIAN_POINT ( 'NONE',  ( -0.06523048226347956391, -1.245570866034205304, -0.1574803149606300301 ) ) ;
#41459 = VECTOR ( 'NONE', #5160, 39.37007874015748143 ) ;
#41460 = CIRCLE ( 'NONE', #6287, 0.09842519685039370636 ) ;
#41461 = CARTESIAN_POINT ( 'NONE',  ( -0.7495606340400177148, -0.1264236179284866091, 1.227854330654897685 ) ) ;
#41462 = CARTESIAN_POINT ( 'NONE',  ( 0.9873396505805591694, -0.1113553986120547346, 0.6643700786326299790 ) ) ;
#41463 = CARTESIAN_POINT ( 'NONE',  ( 0.06474555581190044595, -0.09842519435343592693, -0.1666564064369808196 ) ) ;
#41464 = CARTESIAN_POINT ( 'NONE',  ( -0.7185039370078714072, 0.06523048226347728795, 1.355807086506647829 ) ) ;
#41465 = CARTESIAN_POINT ( 'NONE',  ( 0.8759842519685039353, 0.1787899950787401882, 0.4306102361667086820 ) ) ;
#41466 = CARTESIAN_POINT ( 'NONE',  ( -0.7495606340400177148, -0.1264236179284866091, 0.4010826771115905687 ) ) ;
#41467 = CARTESIAN_POINT ( 'NONE',  ( 1.002407869896990045, -0.1264236179284866091, 0.9276574802611967652 ) ) ;
#41468 = CARTESIAN_POINT ( 'NONE',  ( 0.8759842519685039353, -0.1787899950787401882, 1.158956692859621995 ) ) ;
#41469 = DIRECTION ( 'NONE',  ( -1.000000000000000000, 0.000000000000000000, 0.000000000000000000 ) ) ;
#41470 = CARTESIAN_POINT ( 'NONE',  ( 1.033464566929134687, 0.06523048226347956391, 1.301673228238930502 ) ) ;
#41471 = ORIENTED_EDGE ( 'NONE', *, *, #35190, .F. ) ;
#41472 = ADVANCED_FACE ( 'NONE', ( #14800 ), #25820, .T. ) ;
#41473 = CARTESIAN_POINT ( 'NONE',  ( -1.054774247047244096, 0.000000000000000000, 0.9719488188438739629 ) ) ;
#41474 = CARTESIAN_POINT ( 'NONE',  ( -1.054774247047244096, 0.000000000000000000, 0.02214566923757503927 ) ) ;
#41475 = CARTESIAN_POINT ( 'NONE',  ( 3.284318927891251994E-17, -1.463214519410340531, 0.1787899950787401882 ) ) ;
#41476 = EDGE_LOOP ( 'NONE', ( #23612, #21575, #38134, #46378 ) ) ;
#41477 = FACE_OUTER_BOUND ( 'NONE', #32528, .T. ) ;
#41478 = CARTESIAN_POINT ( 'NONE',  ( 0.1787899950787401882, -0.4926181101824567143, -2.189545951927503898E-17 ) ) ;
#41479 = CARTESIAN_POINT ( 'NONE',  ( 0.7185039370078739607, 1.928577636452523993E-17, 0.6200787401574803237 ) ) ;
#41480 = ORIENTED_EDGE ( 'NONE', *, *, #42061, .T. ) ;
#41481 = CARTESIAN_POINT ( 'NONE',  ( 1.002407869896990045, -0.1264236179284866091, 1.316437007820252081 ) ) ;
#41482 = CARTESIAN_POINT ( 'NONE',  ( 0.9873396505805591694, 0.1113553986120547346, 1.461614173120818760 ) ) ;
#41483 = CARTESIAN_POINT ( 'NONE',  ( -1.033464566929133799, 0.000000000000000000, 1.732283464459401623 ) ) ;
#41484 = CIRCLE ( 'NONE', #22402, 0.1574803149606299191 ) ;
#41485 = CARTESIAN_POINT ( 'NONE',  ( 0.003583035186828842367, -0.09844385435685996943, -0.1050988454126300514 ) ) ;
#41486 = CARTESIAN_POINT ( 'NONE',  ( 0.6971942568897648851, -0.07405724077823297447, 1.619094488135213838 ) ) ;
#41487 = AXIS2_PLACEMENT_3D ( 'NONE', #558, #15214, #44407 ) ;
#41488 = CARTESIAN_POINT ( 'NONE',  ( -0.1264236179284866091, -1.772145669237574994, 0.1264236179284866091 ) ) ;
#41489 = CARTESIAN_POINT ( 'NONE',  ( 0.07405724077823318263, -1.759842519631276581, 0.1787899950787401604 ) ) ;
#41490 = APPLICATION_PROTOCOL_DEFINITION ( 'draft international standard', 'automotive_design', 1998, #12252 ) ;
#41491 = CARTESIAN_POINT ( 'NONE',  ( 0.03901279071809810040, 0.3740157480314960647, 1.224299699984025658 ) ) ;
#41492 = CARTESIAN_POINT ( 'NONE',  ( -0.8019270111902716547, -0.1787899950787401604, 0.6053149605761580787 ) ) ;
#41493 = CARTESIAN_POINT ( 'NONE',  ( -0.8107537697050254399, -0.1574803149606297803, 1.286909448711370585 ) ) ;
#41495 = CARTESIAN_POINT ( 'NONE',  ( 0.4620708661417356478, 0.9842519685039370358, -0.5511811023622036343 ) ) ;
#41494 = CARTESIAN_POINT ( 'NONE',  ( -0.1574803149606300301, -0.7780511811023617108, -0.06523048226347956391 ) ) ;
#41496 = CARTESIAN_POINT ( 'NONE',  ( -0.1797182628040039365, -1.497091053677533479, 0.000000000000000000 ) ) ;
#41497 = DIRECTION ( 'NONE',  ( 0.000000000000000000, 0.000000000000000000, 1.000000000000000000 ) ) ;
#41498 = CARTESIAN_POINT ( 'NONE',  ( 0.1574803149606299191, -0.4704724408373543443, -1.928577636452523993E-17 ) ) ;
#41499 = AXIS2_PLACEMENT_3D ( 'NONE', #44344, #18720, #23690 ) ;
#41500 = CARTESIAN_POINT ( 'NONE',  ( -0.7185039370078739607, 1.928577636452523993E-17, 1.515748031388535200 ) ) ;
#41501 = CARTESIAN_POINT ( 'NONE',  ( 0.9500414927467378812, -0.1787899950787401604, 1.318897637741511364 ) ) ;
#41502 = CARTESIAN_POINT ( 'NONE',  ( 0.8019270111902716547, 0.1787899950787401604, 1.806102362150961094 ) ) ;
#41503 = ORIENTED_EDGE ( 'NONE', *, *, #16935, .F. ) ;
#41505 = EDGE_CURVE ( 'NONE', #35894, #2394, #5355, .T. ) ;
#41504 = CARTESIAN_POINT ( 'NONE',  ( -0.8107537697050234415, -0.1574803149606297803, 0.1451771652468037688 ) ) ;
#41506 = DIRECTION ( 'NONE',  ( -1.000000000000000000, 0.000000000000000000, 0.000000000000000000 ) ) ;
#41507 = DIRECTION ( 'NONE',  ( 0.000000000000000000, 0.000000000000000000, -1.000000000000000000 ) ) ;
#41508 = CARTESIAN_POINT ( 'NONE',  ( 0.1787899950787401604, 0.09547244099864542199, -0.07405724077823318263 ) ) ;
#41509 = CARTESIAN_POINT ( 'NONE',  ( 1.033464566929134687, -0.06523048226347956391, 0.5093503935932608417 ) ) ;
#41510 = CARTESIAN_POINT ( 'NONE',  ( 0.6971942568897626646, 0.07405724077823318263, 0.4724409448281262636 ) ) ;
#41511 = EDGE_CURVE ( 'NONE', #7349, #45730, #43231, .T. ) ;
#41512 = DIRECTION ( 'NONE',  ( 0.000000000000000000, 0.000000000000000000, 1.000000000000000000 ) ) ;
#41513 = DIRECTION ( 'NONE',  ( 0.000000000000000000, 0.000000000000000000, 1.000000000000000000 ) ) ;
#41514 = CARTESIAN_POINT ( 'NONE',  ( -0.9500414927467378812, -0.1787899950787401604, 1.353346456639149986 ) ) ;
#41515 = CARTESIAN_POINT ( 'NONE',  ( 1.033464566929134687, -0.06523048226347956391, 0.7849409447743628254 ) ) ;
#41516 = VERTEX_POINT ( 'NONE', #36059 ) ;
#41517 = FACE_OUTER_BOUND ( 'NONE', #16360, .T. ) ;
#41518 = ADVANCED_FACE ( 'NONE', ( #32250 ), #23325, .F. ) ;
#41519 = ORIENTED_EDGE ( 'NONE', *, *, #23278, .F. ) ;
#41521 = CARTESIAN_POINT ( 'NONE',  ( -0.1787899950787401882, -1.304625984198204636, 0.000000000000000000 ) ) ;
#41520 = CARTESIAN_POINT ( 'NONE',  ( -9.642888182262618425E-18, -1.051181102254677313, -0.1574803149606299191 ) ) ;
#41522 = CARTESIAN_POINT ( 'NONE',  ( -0.8759842519685039353, -0.1574803149606299191, 0.6200787400499527813 ) ) ;
#41523 = CARTESIAN_POINT ( 'NONE',  ( -0.9412147342319837628, -0.1574803149606297803, 1.222933070866141669 ) ) ;
#41524 = CARTESIAN_POINT ( 'NONE',  ( -0.7646288533564489232, -0.1113553986120547346, 1.048228346349165507 ) ) ;
#41526 = CARTESIAN_POINT ( 'NONE',  ( 0.5839895013123354017, 4.616380251121755931E-17, 0.000000000000000000 ) ) ;
#41525 = CARTESIAN_POINT ( 'NONE',  ( 0.4736248074375835060, 1.205832402325950792, -1.129708666049259902 ) ) ;
#41527 = CARTESIAN_POINT ( 'NONE',  ( 0.8759842519685039353, -0.1787899950787401882, 0.05659448813521291560 ) ) ;
#41528 = CARTESIAN_POINT ( 'NONE',  ( 0.7646288533564489232, -0.1113553986120547346, 1.481299212490897466 ) ) ;
#41529 = ORIENTED_EDGE ( 'NONE', *, *, #30673, .T. ) ;
#41530 = ORIENTED_EDGE ( 'NONE', *, *, #4859, .T. ) ;
#41531 = AXIS2_PLACEMENT_3D ( 'NONE', #4489, #27312, #27069 ) ;
#41532 = CARTESIAN_POINT ( 'NONE',  ( 0.6971942568897637749, 2.189545951927499583E-17, 0.9522637794737952577 ) ) ;
#41533 = CARTESIAN_POINT ( 'NONE',  ( -1.054774247047244540, -0.07405724077823318263, 1.594488188922615457 ) ) ;
#41534 = CARTESIAN_POINT ( 'NONE',  ( -0.1574803149606299191, 0.02165354341461366364, 0.000000000000000000 ) ) ;
#41535 = CARTESIAN_POINT ( 'NONE',  ( -1.054774247047244540, 0.07405724077823318263, 1.328740157426552049 ) ) ;
#41536 = PRODUCT_DEFINITION_FORMATION_WITH_SPECIFIED_SOURCE ( 'ANY', '', #44040, .NOT_KNOWN. ) ;
#41537 = AXIS2_PLACEMENT_3D ( 'NONE', #46699, #46229, #10548 ) ;
#41538 = CLOSED_SHELL ( 'NONE', ( #22503, #2639, #11221, #39474, #30238, #1356, #6442, #29395, #21036, #20773, #130, #25011, #19655, #38802, #39205, #38425, #4526, #31292, #523, #46828, #47062, #18126, #46999, #35823, #31762, #13645 ) ) ;
#41539 = LINE ( 'NONE', #42019, #10002 ) ;
#41540 = CARTESIAN_POINT ( 'NONE',  ( -0.8759842519685039353, -0.1787899950787401882, 0.3715551180564728440 ) ) ;
#41541 = FACE_OUTER_BOUND ( 'NONE', #46907, .T. ) ;
#41542 = FACE_OUTER_BOUND ( 'NONE', #36672, .T. ) ;
#41543 = CARTESIAN_POINT ( 'NONE',  ( 0.1264236179284866091, -0.9366397162607342786, -0.1264236179284866091 ) ) ;
#41544 = CARTESIAN_POINT ( 'NONE',  ( 0.1787899950787401604, -0.02263779522182702078, 0.07405724077823318263 ) ) ;
#41545 = ORIENTED_EDGE ( 'NONE', *, *, #28623, .F. ) ;
#41546 = ORIENTED_EDGE ( 'NONE', *, *, #42772, .F. ) ;
#41547 = CARTESIAN_POINT ( 'NONE',  ( 3.624546087963248077E-17, -0.09842519685039370636, 0.2854330708661417804 ) ) ;
#41548 = DIRECTION ( 'NONE',  ( -1.000000000000000000, 0.000000000000000000, 0.000000000000000000 ) ) ;
#41549 = CARTESIAN_POINT ( 'NONE',  ( -0.07405724077823318263, -0.6033464566391496531, -0.1787899950787401604 ) ) ;
#41550 = AXIS2_PLACEMENT_3D ( 'NONE', #207, #35942, #6937 ) ;
#41551 = DIRECTION ( 'NONE',  ( -1.000000000000000000, 0.000000000000000000, 0.000000000000000000 ) ) ;
#41552 = CARTESIAN_POINT ( 'NONE',  ( -0.1797182628040039087, -1.100929636354699426, 0.07444174185955065859 ) ) ;
#41553 = CARTESIAN_POINT ( 'NONE',  ( 0.1747918830520822919, 0.1299212598425196763, 0.01616506989262271946 ) ) ;
#41554 = CARTESIAN_POINT ( 'NONE',  ( 1.054774247047244096, 0.000000000000000000, 0.8538385826234016207 ) ) ;
#41555 = CARTESIAN_POINT ( 'NONE',  ( 0.9500414927467377701, -0.1787899950787401604, 1.432086614119464141 ) ) ;
#41556 = CARTESIAN_POINT ( 'NONE',  ( 0.7495606340400177148, -0.1264236179284866091, 0.1254921259304885850 ) ) ;
#41557 = AXIS2_PLACEMENT_3D ( 'NONE', #39979, #22019, #36645 ) ;
#41559 = EDGE_CURVE ( 'NONE', #2953, #38075, #38011, .T. ) ;
#41558 = DIRECTION ( 'NONE',  ( 1.822029033848725028E-16, 0.000000000000000000, 1.000000000000000000 ) ) ;
#41560 = CARTESIAN_POINT ( 'NONE',  ( 0.9873396505805591694, 0.1113553986120547346, 1.589566929133858331 ) ) ;
#41562 = CARTESIAN_POINT ( 'NONE',  ( -0.2559055118110236116, -0.1477471161312047254, -0.2921040715117803055 ) ) ;
#41561 = CARTESIAN_POINT ( 'NONE',  ( 0.7257667744041150781, -0.07649319432550391595, 1.984749488431225561 ) ) ;
#41563 = FACE_OUTER_BOUND ( 'NONE', #30819, .T. ) ;
#41564 = CARTESIAN_POINT ( 'NONE',  ( 0.06523048226347956391, -0.6747047243019220764, 0.1574803149606297803 ) ) ;
#41565 = CARTESIAN_POINT ( 'NONE',  ( -1.033464566929134687, -0.06523048226347956391, 1.611712598317668999 ) ) ;
#41566 = CARTESIAN_POINT ( 'NONE',  ( -0.07405724077823318263, 0.1250000000537635492, 0.1787899950787401604 ) ) ;
#41567 = ADVANCED_FACE ( 'NONE', ( #8677 ), #1080, .F. ) ;
#41568 = DIRECTION ( 'NONE',  ( 0.000000000000000000, 0.000000000000000000, -1.000000000000000000 ) ) ;
#41569 = CARTESIAN_POINT ( 'NONE',  ( 1.054774247047244540, 0.07405724077823318263, 1.048228346402928723 ) ) ;
#41570 = CARTESIAN_POINT ( 'NONE',  ( 0.8019270111902716547, 0.1787899950787401604, 1.889763779473794481 ) ) ;
#41571 = CARTESIAN_POINT ( 'NONE',  ( 0.7646288533564489232, 0.1113553986120547346, 0.2903543306011346359 ) ) ;
#41572 = ORIENTED_EDGE ( 'NONE', *, *, #2783, .F. ) ;
#41573 = CONICAL_SURFACE ( 'NONE', #13305, 0.2431102362204724532, 0.4367866272367255109 ) ;
#41574 = CYLINDRICAL_SURFACE ( 'NONE', #12348, 0.1003937007874010356 ) ;
#41575 = EDGE_CURVE ( 'NONE', #47237, #23773, #23311, .T. ) ;
#41576 = DIRECTION ( 'NONE',  ( 0.000000000000000000, 0.000000000000000000, 1.000000000000000000 ) ) ;
#41577 = CARTESIAN_POINT ( 'NONE',  ( 0.06523048226347956391, -1.737696850286174266, 0.1574803149606297803 ) ) ;
#41578 = CARTESIAN_POINT ( 'NONE',  ( -1.033464566929134687, 0.06523048226347956391, 0.2386811022546777294 ) ) ;
#41579 = ORIENTED_EDGE ( 'NONE', *, *, #30083, .T. ) ;
#41580 = CARTESIAN_POINT ( 'NONE',  ( 0.000000000000000000, 0.000000000000000000, -0.1574803149606298636 ) ) ;
#41581 = CARTESIAN_POINT ( 'NONE',  ( 1.054774247047244540, -0.07405724077823318263, 1.122047244040725644 ) ) ;
#41582 = ADVANCED_FACE ( 'NONE', ( #37926 ), #15660, .T. ) ;
#41583 = LINE ( 'NONE', #3997, #44813 ) ;
#41584 = CARTESIAN_POINT ( 'NONE',  ( -0.1113553986120547346, -1.794291338582677087, 0.1113553986120547346 ) ) ;
#41585 = DIRECTION ( 'NONE',  ( -0.000000000000000000, -0.000000000000000000, 1.000000000000000000 ) ) ;
#41586 = CARTESIAN_POINT ( 'NONE',  ( -1.002407869896990045, 0.1264236179284866091, 0.5782480314422993040 ) ) ;
#41587 = DIRECTION ( 'NONE',  ( 1.822029033848725028E-16, 0.000000000000000000, 1.000000000000000000 ) ) ;
#41588 = CARTESIAN_POINT ( 'NONE',  ( -1.054774247047244540, 0.07405724077823318263, 0.3001968503399373711 ) ) ;
#41589 = CARTESIAN_POINT ( 'NONE',  ( -0.1264236179284866091, -1.575295275536787276, 0.1264236179284866091 ) ) ;
#41590 = CARTESIAN_POINT ( 'NONE',  ( -1.002407869896990045, 0.1264236179284866091, 0.4650590550643464716 ) ) ;
#41591 = DIRECTION ( 'NONE',  ( -7.051687499798870116E-15, -1.406820448837680035E-16, -1.000000000000000000 ) ) ;
#41592 = LINE ( 'NONE', #23663, #47107 ) ;
#41593 = CARTESIAN_POINT ( 'NONE',  ( -0.7185039370078739607, 1.928577636452523993E-17, 0.9350393700787401619 ) ) ;
#41594 = CARTESIAN_POINT ( 'NONE',  ( -0.1264236179284866091, -0.5330964091741204891, -0.1264236179284866091 ) ) ;
#41595 = CARTESIAN_POINT ( 'NONE',  ( -0.1699750452893318831, -0.08956104039312501319, -0.005819416704781811035 ) ) ;
#41596 = CARTESIAN_POINT ( 'NONE',  ( 0.1113553986120547346, 0.04625984262721204859, -0.1113553986120547346 ) ) ;
#41597 = CARTESIAN_POINT ( 'NONE',  ( 0.8107537697050254399, -0.1574803149606297803, 0.4699803149606304742 ) ) ;
#41598 = CARTESIAN_POINT ( 'NONE',  ( -0.04259491748599998628, -0.09487271926367001063, 0.1523944991998174292 ) ) ;
#41599 = EDGE_CURVE ( 'NONE', #40880, #370, #4157, .T. ) ;
#41600 = CARTESIAN_POINT ( 'NONE',  ( 0.2559023402149968041, -0.1254131385238003160, -0.08931362558432201504 ) ) ;
#41601 = CARTESIAN_POINT ( 'NONE',  ( -0.9500414927467378812, -0.1787899950787401604, 0.4872047243556847929 ) ) ;
#41602 = CARTESIAN_POINT ( 'NONE',  ( 0.8759842519685039353, 0.1574803149606299191, 1.190944881782236342 ) ) ;
#41603 = EDGE_LOOP ( 'NONE', ( #30454, #45321, #14126, #46874 ) ) ;
#41604 = CARTESIAN_POINT ( 'NONE',  ( 0.1377952755905511861, 0.1564960629921262614, 0.9074803149606294195 ) ) ;
#41605 = CIRCLE ( 'NONE', #42410, 0.09842519685039370636 ) ;
#41606 = CARTESIAN_POINT ( 'NONE',  ( -1.054774247047244540, 0.07405724077823318263, 1.486220472387181912 ) ) ;
#41607 = ADVANCED_FACE ( 'NONE', ( #30759 ), #23071, .F. ) ;
#41608 = CARTESIAN_POINT ( 'NONE',  ( 3.284318927891251994E-17, -1.531003936954110189, 0.1787899950787401882 ) ) ;
#41609 = CARTESIAN_POINT ( 'NONE',  ( 0.1787899950787401604, -1.597440944828127485, 0.07405724077823318263 ) ) ;
#41610 = ( BOUNDED_CURVE ( )  B_SPLINE_CURVE ( 2, ( #8116, #14613, #18663, #36656, #22500, #11978, #3814, #18433, #22741 ),
 .UNSPECIFIED., .F., .T. ) 
 B_SPLINE_CURVE_WITH_KNOTS ( ( 3, 2, 2, 2, 3 ),
 ( 0.7700000000000000178, 0.7724999999999999645, 0.7750000000000000222, 0.7774999999999999689, 0.7800000000000000266 ),
 .UNSPECIFIED. ) 
 CURVE ( )  GEOMETRIC_REPRESENTATION_ITEM ( )  RATIONAL_B_SPLINE_CURVE ( ( 1.000000000000000000, 0.9238795325112869605, 1.000000000000000000, 0.9238795325112869605, 1.000000000000000000, 0.9238795325112869605, 1.000000000000000000, 0.9238795325112869605, 1.000000000000000000 ) ) 
 REPRESENTATION_ITEM ( '' )  ) ;
#41611 = CARTESIAN_POINT ( 'NONE',  ( -0.7185039370078739607, 0.000000000000000000, -2.869337061179095023E-17 ) ) ;
#41612 = CARTESIAN_POINT ( 'NONE',  ( 0.8759842519685039353, -0.1574803149606299191, 0.4724409448818898127 ) ) ;
#41613 = DIRECTION ( 'NONE',  ( -1.000000000000000000, 3.469446951953614189E-15, 1.144917494144692682E-16 ) ) ;
#41614 = CARTESIAN_POINT ( 'NONE',  ( -0.7185039370078739607, 1.928577636452523993E-17, 1.200787401467275695 ) ) ;
#41615 = CARTESIAN_POINT ( 'NONE',  ( 1.002407869896990045, -0.1264236179284866091, 0.09596456687537027741 ) ) ;
#41617 = CARTESIAN_POINT ( 'NONE',  ( -1.181102362204724310, 0.000000000000000000, -0.9842519685039370358 ) ) ;
#41616 = CARTESIAN_POINT ( 'NONE',  ( 0.1574803149606299191, -0.4803149606299212948, -1.928577636452523993E-17 ) ) ;
#41618 = CARTESIAN_POINT ( 'NONE',  ( -0.9873396505805591694, 0.1113553986120547346, 1.186023621939716666 ) ) ;
#41619 = ORIENTED_EDGE ( 'NONE', *, *, #30183, .F. ) ;
#41620 = FACE_BOUND ( 'NONE', #44252, .T. ) ;
#41621 = CARTESIAN_POINT ( 'NONE',  ( -0.8759842519685039353, 0.1787899950787401882, 1.060531496009228247 ) ) ;
#41622 = CARTESIAN_POINT ( 'NONE',  ( 0.7185039370078746268, -0.06523048226347956391, 1.173720472440945573 ) ) ;
#41623 = DIRECTION ( 'NONE',  ( 0.000000000000000000, -1.000000000000000000, 0.000000000000000000 ) ) ;
#41624 = CARTESIAN_POINT ( 'NONE',  ( -0.8107537697050254399, 0.1574803149606300301, 0.7209645668216064784 ) ) ;
#41625 = EDGE_CURVE ( 'NONE', #6499, #24890, #8202, .T. ) ;
#41627 = DIRECTION ( 'NONE',  ( 0.000000000000000000, 0.000000000000000000, 1.000000000000000000 ) ) ;
#41626 = CARTESIAN_POINT ( 'NONE',  ( 0.8759842519685039353, -0.1574803149606299191, 0.5807086613097960370 ) ) ;
#41628 = CARTESIAN_POINT ( 'NONE',  ( 0.9873396505805591694, 0.1113553986120547346, 0.5954724408373543998 ) ) ;
#41629 = CARTESIAN_POINT ( 'NONE',  ( -0.1598598147400959735, -0.08956144258305162587, 0.04681090282771781935 ) ) ;
#41631 = CIRCLE ( 'NONE', #20986, 0.09842519685039370636 ) ;
#41630 = CARTESIAN_POINT ( 'NONE',  ( -0.1264236179284866091, -0.5565944881352126172, -0.1264236179284866091 ) ) ;
#41632 = ORIENTED_EDGE ( 'NONE', *, *, #23227, .F. ) ;
#41633 = AXIS2_PLACEMENT_3D ( 'NONE', #45578, #39284, #21076 ) ;
#41634 = DIRECTION ( 'NONE',  ( 1.000000000000000000, 0.000000000000000000, -1.822029033848725275E-16 ) ) ;
#41635 = CARTESIAN_POINT ( 'NONE',  ( 0.9500414927467378812, -0.1787899950787401604, 0.6840551180564720113 ) ) ;
#41636 = ADVANCED_FACE ( 'NONE', ( #12060 ), #24258, .T. ) ;
#41637 = ORIENTED_EDGE ( 'NONE', *, *, #21305, .T. ) ;
#41638 = CARTESIAN_POINT ( 'NONE',  ( -0.7646288533564489232, 0.1113553986120547346, 1.786417322727117840 ) ) ;
#41639 = CARTESIAN_POINT ( 'NONE',  ( 0.1099139000111727937, -0.5708661417322835607, 1.120507485783946100 ) ) ;
#41640 = CARTESIAN_POINT ( 'NONE',  ( -0.1787899950787401604, -1.690944881836001334, 0.07405724077823318263 ) ) ;
#41641 = CARTESIAN_POINT ( 'NONE',  ( 0.07405724077823318263, -0.9625984251430860228, -0.1787899950787401604 ) ) ;
#41642 = CARTESIAN_POINT ( 'NONE',  ( -0.06523048226347956391, -1.319389763779527769, 0.1574803149606297803 ) ) ;
#41644 = ( BOUNDED_CURVE ( )  B_SPLINE_CURVE ( 2, ( #38005, #5166, #31077, #38475, #20256, #34904, #10915, #39393, #43467 ),
 .UNSPECIFIED., .F., .T. ) 
 B_SPLINE_CURVE_WITH_KNOTS ( ( 3, 2, 2, 2, 3 ),
 ( 0.2999999999999999889, 0.3024999999999999911, 0.3049999999999999933, 0.3074999999999999956, 0.3099999999999999978 ),
 .UNSPECIFIED. ) 
 CURVE ( )  GEOMETRIC_REPRESENTATION_ITEM ( )  RATIONAL_B_SPLINE_CURVE ( ( 1.000000000000000000, 0.9238795325112869605, 1.000000000000000000, 0.9238795325112869605, 1.000000000000000000, 0.9238795325112869605, 1.000000000000000000, 0.9238795325112869605, 1.000000000000000000 ) ) 
 REPRESENTATION_ITEM ( '' )  ) ;
#41643 = CARTESIAN_POINT ( 'NONE',  ( 0.8759842519685039353, 0.1574803149606299191, 1.151574803042078710 ) ) ;
#41645 = CARTESIAN_POINT ( 'NONE',  ( -0.7646288533564489232, 0.1113553986120547346, 1.865157480207432883 ) ) ;
#41646 = CARTESIAN_POINT ( 'NONE',  ( -0.9500414927467378812, 0.1787899950787401604, 0.4625984251430869665 ) ) ;
#41647 = VERTEX_POINT ( 'NONE', #13690 ) ;
#41648 = ORIENTED_EDGE ( 'NONE', *, *, #38813, .T. ) ;
#41649 = AXIS2_PLACEMENT_3D ( 'NONE', #2470, #10155, #42701 ) ;
#41650 = CARTESIAN_POINT ( 'NONE',  ( -1.002407869896990045, 0.1264236179284866091, 1.724901574749385880 ) ) ;
#41651 = CARTESIAN_POINT ( 'NONE',  ( 0.6971942568897648851, -0.07405724077823297447, 1.899606299158834943 ) ) ;
#41652 = ORIENTED_EDGE ( 'NONE', *, *, #10658, .F. ) ;
#41653 = LINE ( 'NONE', #35221, #34069 ) ;
#41654 = CARTESIAN_POINT ( 'NONE',  ( 1.002407869896990045, 0.1264236179284866091, 0.4650590550643464716 ) ) ;
#41655 = CARTESIAN_POINT ( 'NONE',  ( -0.9500414927467378812, -0.1787899950787401604, 1.432086614119464141 ) ) ;
#41656 = CARTESIAN_POINT ( 'NONE',  ( 0.05425864391567861156, 0.2641663005107173223, -0.3070225280281027036 ) ) ;
#41657 = CARTESIAN_POINT ( 'NONE',  ( -1.054774247047244540, -0.07405724077823318263, 0.1033464566391498751 ) ) ;
#41658 = CARTESIAN_POINT ( 'NONE',  ( 0.7185039370078739607, 1.928577636452523993E-17, 1.564960629921259949 ) ) ;
#41659 = CARTESIAN_POINT ( 'NONE',  ( -0.9500414927467378812, -0.1787899950787401604, 1.673228346402929834 ) ) ;
#41660 = CARTESIAN_POINT ( 'NONE',  ( -1.033464566929134687, -0.06523048226347956391, 1.966043306979087246 ) ) ;
#41661 = CARTESIAN_POINT ( 'NONE',  ( 0.009745153983727742816, -0.04193537623276881454, -0.2798067035903422095 ) ) ;
#41662 = CARTESIAN_POINT ( 'NONE',  ( -0.7646288533564489232, -0.1113553986120547346, 1.727362204724409489 ) ) ;
#41663 = CARTESIAN_POINT ( 'NONE',  ( 0.5660731898098425585, 0.09842519685039370636, 0.000000000000000000 ) ) ;
#41664 = CARTESIAN_POINT ( 'NONE',  ( 0.6971942568897648851, 0.07405724077823318263, 1.658464566875369472 ) ) ;
#41665 = CARTESIAN_POINT ( 'NONE',  ( 0.1188451152720541443, -0.09842519685039231858, -0.1576307852885025784 ) ) ;
#41666 = CARTESIAN_POINT ( 'NONE',  ( 0.3849708276051176936, 4.766607801171850497E-17, 0.000000000000000000 ) ) ;
#41667 = AXIS2_PLACEMENT_3D ( 'NONE', #17494, #15934, #45367 ) ;
#41668 = EDGE_CURVE ( 'NONE', #18452, #23773, #14140, .T. ) ;
#41669 = ORIENTED_EDGE ( 'NONE', *, *, #28375, .T. ) ;
#41670 = CIRCLE ( 'NONE', #40140, 0.1377952755905511861 ) ;
#41671 = ORIENTED_EDGE ( 'NONE', *, *, #28166, .F. ) ;
#41672 = CONICAL_SURFACE ( 'NONE', #21025, 0.1567662409572586624, 0.9599310885969887241 ) ;
#41673 = CARTESIAN_POINT ( 'NONE',  ( 3.284318927891251994E-17, -1.058562992072220377, 0.1787899950787401882 ) ) ;
#41674 = CARTESIAN_POINT ( 'NONE',  ( -0.1787899950787401604, -1.021653543253323138, 0.07405724077823318263 ) ) ;
#41675 = DIRECTION ( 'NONE',  ( 0.000000000000000000, 0.000000000000000000, 1.000000000000000000 ) ) ;
#41676 = SHAPE_REPRESENTATION_RELATIONSHIP ( 'NONE' , 'NONE' ,  #5950, #32480 ) ;
#41677 = CARTESIAN_POINT ( 'NONE',  ( -0.1797182628040039365, -0.2766186127326519251, 0.000000000000000000 ) ) ;
#41678 = CARTESIAN_POINT ( 'NONE',  ( -0.7185039370078739607, 1.928577636452523993E-17, 0.8070866140657008136 ) ) ;
#41679 = CARTESIAN_POINT ( 'NONE',  ( 0.06523048226347956391, 0.02411417322834644855, 0.1574803149606297803 ) ) ;
#41680 = DIRECTION ( 'NONE',  ( 0.000000000000000000, -1.000000000000000000, 0.000000000000000000 ) ) ;
#41682 = ADVANCED_FACE ( 'NONE', ( #27875 ), #42435, .T. ) ;
#41681 = CARTESIAN_POINT ( 'NONE',  ( 1.054774247047244096, 0.000000000000000000, 0.9276574802611967652 ) ) ;
#41683 = EDGE_CURVE ( 'NONE', #30077, #8512, #42432, .T. ) ;
#41684 = CARTESIAN_POINT ( 'NONE',  ( -1.033464566929133799, 0.000000000000000000, 1.574803149498771537 ) ) ;
#41685 = B_SPLINE_CURVE_WITH_KNOTS ( 'NONE', 3,
 ( #33388, #37182, #33, #40752, #15396, #7948, #22092, #22567, #4326, #7252, #3881, #47266, #36952, #278, #29805, #18959, #18500, #40052, #14923, #33157, #18270, #40989 ),
 .UNSPECIFIED., .F., .F.,
 ( 4, 2, 2, 2, 2, 2, 2, 2, 2, 2, 4 ),
 ( 0.000000000000000000, 0.1250000000000002776, 0.1875000000000003331, 0.2187500000000003053, 0.2500000000000002776, 0.5000000000000002220, 0.6250000000000002220, 0.6875000000000003331, 0.7187500000000002220, 0.7500000000000002220, 1.000000000000000000 ),
 .UNSPECIFIED. ) ;
#41686 = CARTESIAN_POINT ( 'NONE',  ( 0.8107537697050254399, -0.1574803149606297803, 1.257381889763780736 ) ) ;
#41687 = CARTESIAN_POINT ( 'NONE',  ( 0.8019270111902717657, -0.1787899950787401604, 1.943897637741510254 ) ) ;
#41688 = ORIENTED_EDGE ( 'NONE', *, *, #29904, .F. ) ;
#41689 = CIRCLE ( 'NONE', #21055, 0.7874015748031496509 ) ;
#41690 = CARTESIAN_POINT ( 'NONE',  ( 0.9873396505805591694, 0.1113553986120547346, 0.2116141732283464416 ) ) ;
#41691 = CARTESIAN_POINT ( 'NONE',  ( 0.1574803149606300023, 0.2876548164643194516, -0.2627373885913887319 ) ) ;
#41693 = CARTESIAN_POINT ( 'NONE',  ( -0.1787899950787401604, -0.4753937007336378473, 0.07405724077823318263 ) ) ;
#41692 = CARTESIAN_POINT ( 'NONE',  ( -0.06523048226347956391, -0.9699803148531034314, -0.1574803149606300301 ) ) ;
#41694 = DIRECTION ( 'NONE',  ( 0.000000000000000000, 0.000000000000000000, -1.000000000000000000 ) ) ;
#41695 = CARTESIAN_POINT ( 'NONE',  ( 0.07405724077823318263, -1.272637795221826629, -0.1787899950787401604 ) ) ;
#41696 = FACE_OUTER_BOUND ( 'NONE', #17243, .T. ) ;
#41697 = CARTESIAN_POINT ( 'NONE',  ( -0.9500414927467378812, -0.1787899950787401604, 1.707677165300566235 ) ) ;
#41698 = VERTEX_POINT ( 'NONE', #38854 ) ;
#41699 = AXIS2_PLACEMENT_3D ( 'NONE', #43090, #22230, #39500 ) ;
#41700 = CARTESIAN_POINT ( 'NONE',  ( -0.8759842519685039353, -0.1787899950787401882, 1.237696850339937038 ) ) ;
#41701 = CARTESIAN_POINT ( 'NONE',  ( 1.033464566929133799, 0.000000000000000000, 1.850393700679873854 ) ) ;
#41702 = CARTESIAN_POINT ( 'NONE',  ( 1.002407869896990045, -0.1264236179284866091, 1.360728346402929168 ) ) ;
#41703 = AXIS2_PLACEMENT_3D ( 'NONE', #10715, #6847, #21465 ) ;
#41704 = CARTESIAN_POINT ( 'NONE',  ( -0.9500414927467378812, -0.1787899950787401604, 0.5708661416785201226 ) ) ;
#41705 = CARTESIAN_POINT ( 'NONE',  ( -0.6971942568897637749, 2.189545951927499583E-17, 1.222933070812378009 ) ) ;
#41706 = CARTESIAN_POINT ( 'NONE',  ( 0.9412147342319837628, 0.1574803149606300301, 1.542814960522393308 ) ) ;
#41707 = CARTESIAN_POINT ( 'NONE',  ( 0.1644020957507539848, 0.1623118080249112138, 1.367956046207553540E-19 ) ) ;
#41708 = DIRECTION ( 'NONE',  ( 0.000000000000000000, 0.9771240687918550938, 0.2126700594527823895 ) ) ;
#41709 = CARTESIAN_POINT ( 'NONE',  ( 0.8759842519685039353, 0.1787899950787401882, 0.5880905511273386566 ) ) ;
#41710 = CARTESIAN_POINT ( 'NONE',  ( -1.002407869896990045, -0.1264236179284866091, 0.4502952755367874427 ) ) ;
#41711 = CARTESIAN_POINT ( 'NONE',  ( -0.5555748031496030581, 1.061695335278756813, -0.02376411959061705201 ) ) ;
#41712 = CARTESIAN_POINT ( 'NONE',  ( -0.1574803149606299191, 1.174718201258053041, -3.430321324600322797 ) ) ;
#41713 = VERTEX_POINT ( 'NONE', #20167 ) ;
#41714 = CARTESIAN_POINT ( 'NONE',  ( -1.033464566929133799, 0.000000000000000000, 0.3641732283464567121 ) ) ;
#41715 = CARTESIAN_POINT ( 'NONE',  ( 0.7495606340400177148, 0.1264236179284866091, 1.144192913332062966 ) ) ;
#41716 = CARTESIAN_POINT ( 'NONE',  ( -0.1098090583144935017, -0.09851385237441358245, -0.2293689557742909502 ) ) ;
#41717 = VERTEX_POINT ( 'NONE', #24021 ) ;
#41718 = CARTESIAN_POINT ( 'NONE',  ( -0.7495606340400177148, -0.1264236179284866091, 0.9178149605761574126 ) ) ;
#41719 = EDGE_CURVE ( 'NONE', #31435, #15186, #24717, .T. ) ;
#41720 = CARTESIAN_POINT ( 'NONE',  ( -0.7185039370078746268, -0.06523048226347956391, 0.3075787401574803792 ) ) ;
#41721 = CARTESIAN_POINT ( 'NONE',  ( -1.054774247047244540, 0.07405724077823318263, 0.06397637789899228433 ) ) ;
#41722 = CARTESIAN_POINT ( 'NONE',  ( 0.07405724077823318263, -1.603470424922151416, -0.1787899950787401604 ) ) ;
#41723 = ORIENTED_EDGE ( 'NONE', *, *, #686, .T. ) ;
#41724 = DIRECTION ( 'NONE',  ( 1.000000000000000000, -0.000000000000000000, -0.000000000000000000 ) ) ;
#41725 = CARTESIAN_POINT ( 'NONE',  ( -0.1787899950787401604, -0.4704724408911186706, 0.07405724077823318263 ) ) ;
#41726 = ORIENTED_EDGE ( 'NONE', *, *, #7734, .F. ) ;
#41727 = CARTESIAN_POINT ( 'NONE',  ( 0.8759842519685039353, 0.1787899950787401882, 1.331200787347811110 ) ) ;
#41728 = CIRCLE ( 'NONE', #24932, 0.09842519685039370636 ) ;
#41729 = CARTESIAN_POINT ( 'NONE',  ( 0.000000000000000000, 0.1193342091828950846, 0.06889763779527559306 ) ) ;
#41730 = CARTESIAN_POINT ( 'NONE',  ( -0.1787899950787401604, -0.2391732282926934683, 0.07405724077823318263 ) ) ;
#41731 = CARTESIAN_POINT ( 'NONE',  ( 0.9873396505805591694, 0.1113553986120547346, 1.865157480314960647 ) ) ;
#41732 = ADVANCED_FACE ( 'NONE', ( #35286 ), #46511, .T. ) ;
#41733 = AXIS2_PLACEMENT_3D ( 'NONE', #24503, #2212, #28345 ) ;
#41734 = CIRCLE ( 'NONE', #37844, 0.08090551181102362266 ) ;
#41735 = CARTESIAN_POINT ( 'NONE',  ( 0.07405724077823318263, -1.804133858213953889, 0.1787899950787401604 ) ) ;
#41736 = CARTESIAN_POINT ( 'NONE',  ( 0.1787899950787401882, -1.791830708607653699, -2.189545951927503898E-17 ) ) ;
#41737 = SHAPE_DEFINITION_REPRESENTATION ( #14999, #11151 ) ;
#41738 = CARTESIAN_POINT ( 'NONE',  ( 0.000000000000000000, 0.000000000000000000, -0.0004999999999998990712 ) ) ;
#41739 = CARTESIAN_POINT ( 'NONE',  ( -0.9500414927467377701, -0.1787899950787401604, 0.6889763778989936860 ) ) ;
#41740 = EDGE_CURVE ( 'NONE', #6896, #13064, #16603, .T. ) ;
#41742 = DIRECTION ( 'NONE',  ( 0.000000000000000000, 0.000000000000000000, -1.000000000000000000 ) ) ;
#41741 = CARTESIAN_POINT ( 'NONE',  ( 0.1574803149606299191, -0.6771653543307086798, -1.928577636452523993E-17 ) ) ;
#41743 = CARTESIAN_POINT ( 'NONE',  ( -1.100456976456230270E-17, -1.585673730842887652, -0.1797182628040039365 ) ) ;
#41744 = DIRECTION ( 'NONE',  ( 1.000000000000000000, 0.000000000000000000, -1.822029033848725275E-16 ) ) ;
#41745 = CARTESIAN_POINT ( 'NONE',  ( 0.000000000000000000, 0.000000000000000000, -0.3149606299212598381 ) ) ;
#41746 = CARTESIAN_POINT ( 'NONE',  ( 1.002407869896990045, -0.1264236179284866091, 1.518208661363559031 ) ) ;
#41747 = CARTESIAN_POINT ( 'NONE',  ( 1.002407869896990045, -0.1264236179284866091, 1.906988188922614125 ) ) ;
#41748 = CARTESIAN_POINT ( 'NONE',  ( 0.7495606340400177148, 0.1264236179284866091, 0.3124999999462365619 ) ) ;
#41750 = ORIENTED_EDGE ( 'NONE', *, *, #45207, .T. ) ;
#41749 = DIRECTION ( 'NONE',  ( 1.000000000000000000, 0.000000000000000000, 0.000000000000000000 ) ) ;
#41751 = CYLINDRICAL_SURFACE ( 'NONE', #32775, 0.1574803149606299191 ) ;
#41752 = CARTESIAN_POINT ( 'NONE',  ( -0.1296641775163210608, 0.1169123912647635627, -2.121729632260043186 ) ) ;
#41753 = CARTESIAN_POINT ( 'NONE',  ( -0.1264236179284866091, -0.0004921259304884456750, 0.1264236179284866091 ) ) ;
#41754 = CARTESIAN_POINT ( 'NONE',  ( 0.8759842519685039353, 0.1787899950787401882, 0.4650590550643464716 ) ) ;
#41755 = CARTESIAN_POINT ( 'NONE',  ( -0.7646288533564489232, -0.1113553986120547346, 0.7431102362204724532 ) ) ;
#41756 = EDGE_CURVE ( 'NONE', #5495, #32411, #13363, .T. ) ;
#41757 = CARTESIAN_POINT ( 'NONE',  ( -0.8107537697050254399, -0.1574803149606297803, 1.326279527451528661 ) ) ;
#41758 = CARTESIAN_POINT ( 'NONE',  ( -0.7185039370078714072, 0.06523048226347728795, 1.592027558947592958 ) ) ;
#41759 = CARTESIAN_POINT ( 'NONE',  ( -1.054774247047244540, -0.07405724077823318263, 1.318897637741511364 ) ) ;
#41760 = CARTESIAN_POINT ( 'NONE',  ( 0.8107537697050253289, 0.1574803149606300301, 0.7997047243019228535 ) ) ;
#41761 = ORIENTED_EDGE ( 'NONE', *, *, #18239, .T. ) ;
#41762 = CARTESIAN_POINT ( 'NONE',  ( 1.002407869896990045, 0.1264236179284866091, 0.9374999999462362288 ) ) ;
#41763 = ORIENTED_EDGE ( 'NONE', *, *, #847, .T. ) ;
#41765 = EDGE_LOOP ( 'NONE', ( #12662, #44412, #15923, #6823, #25429 ) ) ;
#41764 = CARTESIAN_POINT ( 'NONE',  ( -0.07405724077823318263, -1.297244094434425010, 0.1787899950787401604 ) ) ;
#41766 = CARTESIAN_POINT ( 'NONE',  ( -0.9412147342319837628, 0.1574803149606300301, 0.5191929132782994172 ) ) ;
#41767 = CARTESIAN_POINT ( 'NONE',  ( 0.1574803149606300023, 1.174718201258053041, -3.430321324600322797 ) ) ;
#41768 = CARTESIAN_POINT ( 'NONE',  ( -0.8759842519685039353, -0.1574803149606299191, 1.181102362204724310 ) ) ;
#41769 = LINE ( 'NONE', #27218, #26622 ) ;
#41771 = CARTESIAN_POINT ( 'NONE',  ( 0.04756641494945763188, -0.5708661417322835607, 1.120507485783946766 ) ) ;
#41770 = DIRECTION ( 'NONE',  ( -1.000000000000000000, 0.000000000000000000, 0.000000000000000000 ) ) ;
#41772 = DIRECTION ( 'NONE',  ( 0.000000000000000000, 6.938893903907222856E-15, -1.000000000000000000 ) ) ;
#41773 = CARTESIAN_POINT ( 'NONE',  ( 0.8759842519685039353, -0.1574803149606299191, 1.368110236112944911 ) ) ;
#41774 = ORIENTED_EDGE ( 'NONE', *, *, #14956, .F. ) ;
#41775 = EDGE_LOOP ( 'NONE', ( #24434, #24997, #32294, #34789 ) ) ;
#41776 = CARTESIAN_POINT ( 'NONE',  ( -0.09072478486328348912, -0.09340956239926175020, -0.2330530577653659730 ) ) ;
#41777 = ORIENTED_EDGE ( 'NONE', *, *, #46677, .F. ) ;
#41778 = CARTESIAN_POINT ( 'NONE',  ( 0.8019270111902716547, 0.1787899950787401604, 0.9448818897100165204 ) ) ;
#41779 = CARTESIAN_POINT ( 'NONE',  ( -1.054774247047244096, 0.000000000000000000, 1.596948818843874074 ) ) ;
#41780 = CARTESIAN_POINT ( 'NONE',  ( -0.1574803149606300301, -0.02017716524680367163, -0.06523048226347956391 ) ) ;
#41781 = CARTESIAN_POINT ( 'NONE',  ( -1.054774247047244540, 0.07405724077823318263, 1.486220472387181690 ) ) ;
#41782 = AXIS2_PLACEMENT_3D ( 'NONE', #18870, #22007, #29720 ) ;
#41783 = ORIENTED_EDGE ( 'NONE', *, *, #35518, .F. ) ;
#41784 = VERTEX_POINT ( 'NONE', #32157 ) ;
#41785 = LINE ( 'NONE', #12838, #3110 ) ;
#41786 = CARTESIAN_POINT ( 'NONE',  ( 0.1377952755905511861, -1.365923996832131609E-16, 0.8070866141732283561 ) ) ;
#41787 = CARTESIAN_POINT ( 'NONE',  ( 0.5555748031496077211, 2.762335417273526192E-15, -0.7480314960629921295 ) ) ;
#41788 = CARTESIAN_POINT ( 'NONE',  ( 0.1787899950787401604, -1.101501920985143990, 0.07405724077823318263 ) ) ;
#41789 = ORIENTED_EDGE ( 'NONE', *, *, #15662, .F. ) ;
#41790 = CARTESIAN_POINT ( 'NONE',  ( 0.1264236179284866091, 0.02411417328210995956, -0.1264236179284866091 ) ) ;
#41791 = ORIENTED_EDGE ( 'NONE', *, *, #27486, .T. ) ;
#41792 = EDGE_LOOP ( 'NONE', ( #41471, #33616, #4572, #20108 ) ) ;
#41793 = EDGE_CURVE ( 'NONE', #13799, #22426, #17850, .T. ) ;
#41794 = DIRECTION ( 'NONE',  ( 0.4999999999999998890, 0.000000000000000000, 0.8660254037844388186 ) ) ;
#41795 = DIRECTION ( 'NONE',  ( 1.822029033848725028E-16, 0.000000000000000000, 1.000000000000000000 ) ) ;
#41796 = CARTESIAN_POINT ( 'NONE',  ( 0.9412147342319837628, -0.1574803149606297803, 1.813484251968503935 ) ) ;
#41797 = EDGE_CURVE ( 'NONE', #16719, #2629, #27980, .T. ) ;
#41798 = CARTESIAN_POINT ( 'NONE',  ( -0.1264236179284866091, -0.5615157479777322935, -0.1264236179284866091 ) ) ;
#41799 = CARTESIAN_POINT ( 'NONE',  ( -1.054774247047244540, -0.07405724077823318263, 0.1427165353793073133 ) ) ;
#41800 = CARTESIAN_POINT ( 'NONE',  ( -0.8107537697050253289, -0.1574803149606297803, 1.099901574803150650 ) ) ;
#41801 = CARTESIAN_POINT ( 'NONE',  ( 0.1270800023317771588, -1.206736722968872133, 0.1270800023317771588 ) ) ;
#41802 = CARTESIAN_POINT ( 'NONE',  ( 0.5538057742782149795, 4.616380251121755931E-17, 0.000000000000000000 ) ) ;
#41803 = CARTESIAN_POINT ( 'NONE',  ( 0.8759842519685039353, 0.1787899950787401882, 1.139271653489543290 ) ) ;
#41804 = CARTESIAN_POINT ( 'NONE',  ( 1.002407869896990045, 0.1264236179284866091, 1.444389763725763665 ) ) ;
#41805 = CYLINDRICAL_SURFACE ( 'NONE', #19907, 0.09842519685039370636 ) ;
#41806 = CARTESIAN_POINT ( 'NONE',  ( 0.8759842519685039353, -0.1574803149606299191, 1.614173228346456712 ) ) ;
#41808 = CARTESIAN_POINT ( 'NONE',  ( -0.1711860128076768406, -0.1966586703792297941, -0.3122165016188725994 ) ) ;
#41807 = DIRECTION ( 'NONE',  ( 0.000000000000000000, -0.6121968903568536513, -0.7907053606985338101 ) ) ;
#41809 = CARTESIAN_POINT ( 'NONE',  ( 0.9873396505805591694, -0.1113553986120547346, 0.4675196849318432601 ) ) ;
#41810 = CARTESIAN_POINT ( 'NONE',  ( -0.9412147342319837628, -0.1574803149606297803, 1.606791338475149766 ) ) ;
#41811 = DIRECTION ( 'NONE',  ( 1.000000000000000000, 0.000000000000000000, 0.000000000000000000 ) ) ;
#41812 = CARTESIAN_POINT ( 'NONE',  ( 0.7495606340400177148, -0.1264236179284866091, 0.9916338582139527791 ) ) ;
#41813 = CARTESIAN_POINT ( 'NONE',  ( 0.6971942568897648851, -0.07405724077823297447, 1.820866141678520789 ) ) ;
#41814 = CARTESIAN_POINT ( 'NONE',  ( 0.8759842519685039353, -0.1574803149606299191, 0.3444881888688507976 ) ) ;
#41815 = ORIENTED_EDGE ( 'NONE', *, *, #38837, .T. ) ;
#41816 = CARTESIAN_POINT ( 'NONE',  ( 0.9873396505805591694, -0.1113553986120547346, 1.894685039370078927 ) ) ;
#41817 = CARTESIAN_POINT ( 'NONE',  ( 2.892866454678787531E-17, -1.740157480207433105, 0.1574803149606299191 ) ) ;
#41818 = CARTESIAN_POINT ( 'NONE',  ( -0.9873396505805591694, -0.1113553986120547346, 0.2706692912310554866 ) ) ;
#41819 = CYLINDRICAL_SURFACE ( 'NONE', #24446, 0.1574803149606299191 ) ;
#41820 = CARTESIAN_POINT ( 'NONE',  ( 0.9500414927467378812, 0.1787899950787401604, 1.249999999946235896 ) ) ;
#41821 = CARTESIAN_POINT ( 'NONE',  ( 0.4330708661417322913, 0.1574803149606299191, 1.186023622047243986 ) ) ;
#41822 = CARTESIAN_POINT ( 'NONE',  ( 0.07405724077823318263, 0.09055118115612580121, 0.1787899950787401604 ) ) ;
#41823 = AXIS2_PLACEMENT_3D ( 'NONE', #34112, #29831, #26209 ) ;
#41824 = CARTESIAN_POINT ( 'NONE',  ( -0.9873396505805591694, -0.1113553986120547346, 1.018700787294047228 ) ) ;
#41825 = CARTESIAN_POINT ( 'NONE',  ( -0.7495606340400177148, 0.1264236179284866091, 0.5880905511273386566 ) ) ;
#41826 = CARTESIAN_POINT ( 'NONE',  ( 0.8759842519685039353, -0.1574803149606299191, 1.368110236112944911 ) ) ;
#41827 = DIRECTION ( 'NONE',  ( 0.000000000000000000, -1.020425574104001164E-16, 1.000000000000000000 ) ) ;
#41828 = VERTEX_POINT ( 'NONE', #248 ) ;
#41830 = CARTESIAN_POINT ( 'NONE',  ( 0.1787899950787401604, -1.562992125930488196, 0.07405724077823318263 ) ) ;
#41829 = CARTESIAN_POINT ( 'NONE',  ( -0.1574803149606300301, -0.3745078739082211006, -0.06523048226347956391 ) ) ;
#41831 = CARTESIAN_POINT ( 'NONE',  ( -1.002407869896990045, -0.1264236179284866091, 1.045767716481669440 ) ) ;
#41832 = CARTESIAN_POINT ( 'NONE',  ( -0.9500414927467378812, 0.1787899950787401604, 1.761811023568284007 ) ) ;
#41833 = ORIENTED_EDGE ( 'NONE', *, *, #5865, .F. ) ;
#41834 = CARTESIAN_POINT ( 'NONE',  ( -0.8019270111902717657, -0.1787899950787401604, 0.6053149605761579677 ) ) ;
#41835 = ORIENTED_EDGE ( 'NONE', *, *, #40975, .T. ) ;
#41836 = CARTESIAN_POINT ( 'NONE',  ( 0.1574803149606299746, -0.5708661417322837828, 2.134496832518260172E-17 ) ) ;
#41837 = CARTESIAN_POINT ( 'NONE',  ( 0.1580704331077708857, 0.1206688581849416769, -0.006611858888777481270 ) ) ;
#41838 = LINE ( 'NONE', #15786, #42731 ) ;
#41839 = CARTESIAN_POINT ( 'NONE',  ( -1.094772975963752103E-17, -0.5380176690166401654, -0.1787899950787401882 ) ) ;
#41840 = CARTESIAN_POINT ( 'NONE',  ( 0.1442972407897856468, -0.08956032687278150939, -0.1319430747994370101 ) ) ;
#41841 = DIRECTION ( 'NONE',  ( 0.000000000000000000, 0.7880107536067203489, -0.6156614753256602901 ) ) ;
#41842 = FACE_OUTER_BOUND ( 'NONE', #29936, .T. ) ;
#41843 = EDGE_CURVE ( 'NONE', #4993, #28970, #7290, .T. ) ;
#41844 = CARTESIAN_POINT ( 'NONE',  ( -0.7495606340400177148, -0.1264236179284866091, 0.4010826771115905687 ) ) ;
#41845 = CYLINDRICAL_SURFACE ( 'NONE', #18019, 0.1574803149606299191 ) ;
#41846 = EDGE_CURVE ( 'NONE', #22349, #15853, #9530, .T. ) ;
#41847 = ORIENTED_EDGE ( 'NONE', *, *, #14520, .F. ) ;
#41848 = CARTESIAN_POINT ( 'NONE',  ( -1.033464566929133799, 0.000000000000000000, 1.220472440837354400 ) ) ;
#41849 = EDGE_CURVE ( 'NONE', #8597, #5132, #11895, .T. ) ;
#41850 = ADVANCED_FACE ( 'NONE', ( #41842 ), #27049, .T. ) ;
#41851 = CARTESIAN_POINT ( 'NONE',  ( 0.1264236179284866091, -1.516240157426551161, -0.1264236179284866091 ) ) ;
#41852 = CARTESIAN_POINT ( 'NONE',  ( -0.2559053145832481668, 0.09876138958662310230, -0.3048888299123765910 ) ) ;
#41853 = CIRCLE ( 'NONE', #18922, 0.1377952755905509363 ) ;
#41854 = CARTESIAN_POINT ( 'NONE',  ( 0.1643927466631365242, -0.08114304634203027555, 0.1405438789450154657 ) ) ;
#41855 = CARTESIAN_POINT ( 'NONE',  ( 0.9412147342319837628, 0.1574803149606300301, 0.4502952755905510474 ) ) ;
#41856 = CARTESIAN_POINT ( 'NONE',  ( 0.1797182628040039087, -0.6875438095830463947, -0.07444174185955065859 ) ) ;
#41857 = DIRECTION ( 'NONE',  ( 0.000000000000000000, -1.000000000000000000, 1.073081856240829922E-16 ) ) ;
#41858 = CARTESIAN_POINT ( 'NONE',  ( -1.033464566929134687, -0.06523048226347956391, 1.296751968396409049 ) ) ;
#41859 = CARTESIAN_POINT ( 'NONE',  ( 1.054774247047244540, -0.07405724077823318263, 0.6151574802611974313 ) ) ;
#41860 = CARTESIAN_POINT ( 'NONE',  ( 0.7495606340400177148, 0.1264236179284866091, 0.07627952750529173875 ) ) ;
#41862 = CARTESIAN_POINT ( 'NONE',  ( 0.9873396505805591694, -0.1113553986120547346, 0.3592519685039369803 ) ) ;
#41861 = CARTESIAN_POINT ( 'NONE',  ( 0.1113553986120547346, -0.4852362204724409156, 0.1113553986120547346 ) ) ;
#41863 = DIRECTION ( 'NONE',  ( 0.000000000000000000, 1.000000000000000000, 0.000000000000000000 ) ) ;
#41864 = ORIENTED_EDGE ( 'NONE', *, *, #21660, .F. ) ;
#41865 = DIRECTION ( 'NONE',  ( 1.000000000000000000, -0.000000000000000000, -0.000000000000000000 ) ) ;
#41866 = CARTESIAN_POINT ( 'NONE',  ( -0.7495606340400177148, 0.1264236179284866091, 1.144192913332062966 ) ) ;
#41867 = CARTESIAN_POINT ( 'NONE',  ( 0.7646288533564489232, 0.1113553986120547346, 1.048228346456692828 ) ) ;
#41868 = CARTESIAN_POINT ( 'NONE',  ( -0.9972233763874301937, -0.1313180930730347140, 1.990531206743730630 ) ) ;
#41869 = DIRECTION ( 'NONE',  ( 1.000000000000000000, 0.000000000000000000, 0.000000000000000000 ) ) ;
#41871 = CARTESIAN_POINT ( 'NONE',  ( -0.7185039370078739607, 0.000000000000000000, -2.869337061179095023E-17 ) ) ;
#41870 = DIRECTION ( 'NONE',  ( -1.000000000000000000, 0.000000000000000000, 0.000000000000000000 ) ) ;
#41872 = PLANE ( 'NONE',  #26989 ) ;
#41873 = CARTESIAN_POINT ( 'NONE',  ( -0.1787899950787401604, -0.4704724408911186706, 0.07405724077823318263 ) ) ;
#41874 = EDGE_LOOP ( 'NONE', ( #37044, #26977, #10766 ) ) ;
#41875 = CARTESIAN_POINT ( 'NONE',  ( 0.7185039370078739607, 1.928577636452523993E-17, 0.2657480314960630197 ) ) ;
#41876 = CARTESIAN_POINT ( 'NONE',  ( 1.002407869896990045, -0.1264236179284866091, 0.8046259841982047467 ) ) ;
#41877 = CYLINDRICAL_SURFACE ( 'NONE', #39450, 0.1574803149606299191 ) ;
#41878 = CARTESIAN_POINT ( 'NONE',  ( 0.8759842519685039353, -0.1574803149606299191, 0.9055118110236221041 ) ) ;
#41879 = CARTESIAN_POINT ( 'NONE',  ( 3.284318927891251994E-17, -1.722933070812378009, 0.1787899950787401882 ) ) ;
#41880 = CARTESIAN_POINT ( 'NONE',  ( 0.1264236179284866091, -0.8469488188438739629, -0.1264236179284866091 ) ) ;
#41881 = CARTESIAN_POINT ( 'NONE',  ( -0.06523048226347956391, -1.334153543307087242, -0.1574803149606300301 ) ) ;
#41882 = CARTESIAN_POINT ( 'NONE',  ( -0.2559055118110236116, 0.1477471161312031434, -0.3149606299212598381 ) ) ;
#41883 = EDGE_LOOP ( 'NONE', ( #42530, #40218, #47182, #39248, #3000 ) ) ;
#41884 = ORIENTED_EDGE ( 'NONE', *, *, #22016, .F. ) ;
#41885 = CARTESIAN_POINT ( 'NONE',  ( -0.6971942568897648851, -0.07405724077823297447, 1.938976377898990799 ) ) ;
#41886 = CARTESIAN_POINT ( 'NONE',  ( 1.054774247047244540, -0.07405724077823318263, 1.914370078686394860 ) ) ;
#41887 = ORIENTED_EDGE ( 'NONE', *, *, #43700, .F. ) ;
#41888 = CARTESIAN_POINT ( 'NONE',  ( 0.06523048226347956391, 0.009350393808314453811, -0.1574803149606300301 ) ) ;
#41889 = CARTESIAN_POINT ( 'NONE',  ( 1.054774247047244540, -0.07405724077823318263, 0.4576771653005669016 ) ) ;
#41890 = CARTESIAN_POINT ( 'NONE',  ( -0.9500414927467378812, -0.1787899950787401604, 1.353346456639149986 ) ) ;
#41891 = CYLINDRICAL_SURFACE ( 'NONE', #602, 0.1574803149606299191 ) ;
#41892 = CARTESIAN_POINT ( 'NONE',  ( -0.8019270111902717657, -0.1787899950787401604, 0.9940944881352130613 ) ) ;
#41893 = AXIS2_PLACEMENT_3D ( 'NONE', #10585, #29538, #22280 ) ;
#41894 = CARTESIAN_POINT ( 'NONE',  ( -0.9500414927467378812, 0.1787899950787401604, 0.1525590550643468046 ) ) ;
#41895 = CARTESIAN_POINT ( 'NONE',  ( 0.9873396505805591694, -0.1113553986120547346, 1.579724409448818978 ) ) ;
#41896 = CARTESIAN_POINT ( 'NONE',  ( -0.9500414927467378812, 0.1787899950787401604, 1.806102362150961316 ) ) ;
#41897 = CARTESIAN_POINT ( 'NONE',  ( -0.8759842519685039353, -0.1787899950787401882, 0.05659448813521291560 ) ) ;
#41898 = CARTESIAN_POINT ( 'NONE',  ( -0.1894960330211026833, 0.07859832706092077792, 0.1760274851910419436 ) ) ;
#41899 = CARTESIAN_POINT ( 'NONE',  ( -0.9873396505805591694, -0.1113553986120547346, 1.737204724409448842 ) ) ;
#41900 = DIRECTION ( 'NONE',  ( -1.000000000000000000, -6.679788269418529283E-17, 0.000000000000000000 ) ) ;
#41901 = CARTESIAN_POINT ( 'NONE',  ( 0.8759842519685039353, 0.1787899950787401882, 1.729822834591905556 ) ) ;
#41902 = CARTESIAN_POINT ( 'NONE',  ( 0.09176752663691399581, -0.09842519685039370636, -0.1728335834645769731 ) ) ;
#41903 = ( BOUNDED_CURVE ( )  B_SPLINE_CURVE ( 2, ( #26902, #12048, #27151, #41706, #26670, #23537, #8906, #25789, #41220 ),
 .UNSPECIFIED., .F., .F. ) 
 B_SPLINE_CURVE_WITH_KNOTS ( ( 3, 2, 2, 2, 3 ),
 ( 0.7600000000000000089, 0.7624999999999999556, 0.7650000000000000133, 0.7674999999999999600, 0.7700000000000000178 ),
 .UNSPECIFIED. ) 
 CURVE ( )  GEOMETRIC_REPRESENTATION_ITEM ( )  RATIONAL_B_SPLINE_CURVE ( ( 1.000000000000000000, 0.9238795325112869605, 1.000000000000000000, 0.9238795325112869605, 1.000000000000000000, 0.9238795325112869605, 1.000000000000000000, 0.9238795325112829637, 1.000000000000000000 ) ) 
 REPRESENTATION_ITEM ( '' )  ) ;
#41904 = EDGE_CURVE ( 'NONE', #3164, #2574, #713, .T. ) ;
#41905 = VERTEX_POINT ( 'NONE', #38044 ) ;
#41906 = EDGE_LOOP ( 'NONE', ( #6525, #36327, #1839, #3830 ) ) ;
#41907 = EDGE_CURVE ( 'NONE', #30831, #9904, #34098, .T. ) ;
#41908 = CARTESIAN_POINT ( 'NONE',  ( 0.1787899950787401604, -1.011811023568284451, 0.07405724077823318263 ) ) ;
#41909 = CARTESIAN_POINT ( 'NONE',  ( 0.1787899950787401882, -1.161909448765133801, -2.189545951927503898E-17 ) ) ;
#41910 = CIRCLE ( 'NONE', #14419, 0.1003937007874010356 ) ;
#41911 = CARTESIAN_POINT ( 'NONE',  ( -1.033464566929134687, -0.06523048226347956391, 0.5979330708661413363 ) ) ;
#41912 = CARTESIAN_POINT ( 'NONE',  ( 0.1797182628040039365, -0.4931540458035180707, -2.200913952912460540E-17 ) ) ;
#41913 = CARTESIAN_POINT ( 'NONE',  ( -0.1574803149606297803, -1.826279527451528661, 0.06523048226347956391 ) ) ;
#41914 = CARTESIAN_POINT ( 'NONE',  ( -0.9412147342319837628, 0.1574803149606300301, 0.8735236219397174429 ) ) ;
#41915 = CARTESIAN_POINT ( 'NONE',  ( 0.06523048226347956391, 0.03887795275590551908, -0.1574803149606300301 ) ) ;
#41916 = CARTESIAN_POINT ( 'NONE',  ( 0.7495606340400177148, 0.1264236179284866091, 0.8636811023084409733 ) ) ;
#41917 = AXIS2_PLACEMENT_3D ( 'NONE', #2141, #45503, #1909 ) ;
#41918 = ( BOUNDED_CURVE ( )  B_SPLINE_CURVE ( 2, ( #26147, #36460, #40717, #8145, #3617, #4533, #19170, #33828, #18234 ),
 .UNSPECIFIED., .F., .T. ) 
 B_SPLINE_CURVE_WITH_KNOTS ( ( 3, 2, 2, 2, 3 ),
 ( 0.4699999999999999734, 0.4724999999999999756, 0.4749999999999999778, 0.4774999999999999800, 0.4799999999999999822 ),
 .UNSPECIFIED. ) 
 CURVE ( )  GEOMETRIC_REPRESENTATION_ITEM ( )  RATIONAL_B_SPLINE_CURVE ( ( 1.000000000000000000, 0.9238795325112879597, 1.000000000000000000, 0.9238795325112869605, 1.000000000000000000, 0.9238795325112869605, 1.000000000000000000, 0.9238795325112869605, 1.000000000000000000 ) ) 
 REPRESENTATION_ITEM ( '' )  ) ;
#41920 = CARTESIAN_POINT ( 'NONE',  ( 0.001106411046829902005, 0.1060985490482350690, 0.09184399599020635907 ) ) ;
#41919 = CARTESIAN_POINT ( 'NONE',  ( 0.07097307671277083840, 0.2545179073170722450, -0.04495255068439106549 ) ) ;
#41921 = CARTESIAN_POINT ( 'NONE',  ( 0.7646288533564489232, -0.1113553986120547346, 1.087598425089322918 ) ) ;
#41922 = CARTESIAN_POINT ( 'NONE',  ( 0.6971942568897648851, 0.07405724077823318263, 1.934055118056471567 ) ) ;
#41923 = CARTESIAN_POINT ( 'NONE',  ( 0.8107537697050234415, -0.1574803149606297803, 0.1943897637795276023 ) ) ;
#41924 = CYLINDRICAL_SURFACE ( 'NONE', #10701, 0.1574803149606299191 ) ;
#41925 = CARTESIAN_POINT ( 'NONE',  ( 0.1264236179284866091, -0.3745078739619845942, -0.1264236179284866091 ) ) ;
#41926 = DIRECTION ( 'NONE',  ( 1.822029033848725028E-16, 0.000000000000000000, 1.000000000000000000 ) ) ;
#41927 = EDGE_CURVE ( 'NONE', #34447, #815, #5686, .T. ) ;
#41928 = CARTESIAN_POINT ( 'NONE',  ( 0.1787899950787401604, -1.356299212544662014, -0.07405724077823318263 ) ) ;
#41929 = CARTESIAN_POINT ( 'NONE',  ( 1.002407869896990045, 0.1264236179284866091, 0.3469488188438744070 ) ) ;
#41930 = CARTESIAN_POINT ( 'NONE',  ( -0.7495606340400177148, -0.1264236179284866091, 1.857775590497417362 ) ) ;
#41931 = EDGE_LOOP ( 'NONE', ( #19289, #10447, #20161, #298 ) ) ;
#41932 = CARTESIAN_POINT ( 'NONE',  ( -1.002407869896990045, 0.1264236179284866091, 1.252460629867496067 ) ) ;
#41933 = DIRECTION ( 'NONE',  ( 2.943801717310650128E-16, -1.000000000000000000, -2.355041373848520102E-15 ) ) ;
#41934 = CARTESIAN_POINT ( 'NONE',  ( 0.7495606340400177148, 0.1264236179284866091, 1.419783464513165505 ) ) ;
#41935 = LINE ( 'NONE', #16799, #45843 ) ;
#41936 = CARTESIAN_POINT ( 'NONE',  ( 0.6971942568897626646, 0.07405724077823318263, 0.08366141726907129483 ) ) ;
#41937 = CARTESIAN_POINT ( 'NONE',  ( -0.6971942568897648851, 0.07405724077823318263, 1.259842519631276359 ) ) ;
#41938 = CARTESIAN_POINT ( 'NONE',  ( -0.7185039370078739607, 1.928577636452523993E-17, 0.5807086614173228023 ) ) ;
#41939 = CARTESIAN_POINT ( 'NONE',  ( 0.8107537697050254399, 0.1574803149606300301, 1.203248031496062520 ) ) ;
#41940 = CARTESIAN_POINT ( 'NONE',  ( 0.6971942568897648851, 0.07405724077823318263, 0.5954724408911187261 ) ) ;
#41941 = CARTESIAN_POINT ( 'NONE',  ( -0.7495606340400177148, -0.1264236179284866091, 0.5585629920722204877 ) ) ;
#41942 = CARTESIAN_POINT ( 'NONE',  ( -0.05554372828378579402, -0.07731288306167675983, 0.2533648624690310047 ) ) ;
#41943 = DIRECTION ( 'NONE',  ( 0.000000000000000000, 0.000000000000000000, 1.000000000000000000 ) ) ;
#41944 = VERTEX_POINT ( 'NONE', #1847 ) ;
#41945 = EDGE_LOOP ( 'NONE', ( #46252, #44892, #34641, #14397, #12780 ) ) ;
#41946 = FACE_OUTER_BOUND ( 'NONE', #3055, .T. ) ;
#41947 = CARTESIAN_POINT ( 'NONE',  ( -1.033464566929133799, 0.000000000000000000, 0.3248031496062992463 ) ) ;
#41948 = CARTESIAN_POINT ( 'NONE',  ( 1.002407869896990045, -0.1264236179284866091, 1.203248031442299304 ) ) ;
#41949 = CARTESIAN_POINT ( 'NONE',  ( -0.2118463275878102459, -0.09851385012822971854, 0.1047257731708598344 ) ) ;
#41950 = CARTESIAN_POINT ( 'NONE',  ( 1.033464566929133799, 0.000000000000000000, 1.220472440837354400 ) ) ;
#41951 = ORIENTED_EDGE ( 'NONE', *, *, #18881, .F. ) ;
#41952 = DIRECTION ( 'NONE',  ( 0.000000000000000000, 0.000000000000000000, 1.000000000000000000 ) ) ;
#41953 = CARTESIAN_POINT ( 'NONE',  ( -0.8759842519685039353, 0.1787899950787401882, 0.9030511810485984947 ) ) ;
#41954 = EDGE_CURVE ( 'NONE', #42075, #16859, #20535, .T. ) ;
#41955 = CARTESIAN_POINT ( 'NONE',  ( -0.6971942568897626646, -0.07405724077823297447, 0.2017716534895435399 ) ) ;
#41956 = ORIENTED_EDGE ( 'NONE', *, *, #13436, .T. ) ;
#41957 = LINE ( 'NONE', #12777, #12793 ) ;
#41958 = CARTESIAN_POINT ( 'NONE',  ( -0.1264236179284866091, -0.5172244093950552069, -0.1264236179284866091 ) ) ;
#41959 = CARTESIAN_POINT ( 'NONE',  ( -0.2618967166504349020, -0.1659366058165111513, 0.8981965965474308922 ) ) ;
#41960 = CARTESIAN_POINT ( 'NONE',  ( 0.9500414927467378812, 0.1787899950787401604, 1.328740157426552049 ) ) ;
#41961 = EDGE_CURVE ( 'NONE', #39584, #11722, #4195, .T. ) ;
#41962 = CARTESIAN_POINT ( 'NONE',  ( 7.107660667885992191E-05, 0.1226968624037449579, 0.06307306040125523761 ) ) ;
#41963 = DIRECTION ( 'NONE',  ( 0.000000000000000000, 0.000000000000000000, -1.000000000000000000 ) ) ;
#41964 = CARTESIAN_POINT ( 'NONE',  ( 0.1787899950787401882, -0.7288385826234015097, -2.189545951927503898E-17 ) ) ;
#41965 = CARTESIAN_POINT ( 'NONE',  ( 0.8107537697050254399, 0.1574803149606300301, 1.872539370078740495 ) ) ;
#41966 = CARTESIAN_POINT ( 'NONE',  ( 0.8019270111902717657, 0.1787899950787401604, 1.569881889710015299 ) ) ;
#41967 = CARTESIAN_POINT ( 'NONE',  ( -0.07405724077823318263, -0.008982235945774144636, 0.1787899950787401604 ) ) ;
#41968 = CARTESIAN_POINT ( 'NONE',  ( -1.094772975963752103E-17, 0.1422244095025824717, -0.1787899950787401882 ) ) ;
#41969 = CARTESIAN_POINT ( 'NONE',  ( -1.033464566929133799, 0.000000000000000000, 1.732283464459401623 ) ) ;
#41970 = CARTESIAN_POINT ( 'NONE',  ( -0.9500414927467377701, 0.1787899950787401604, 0.8218503936470251681 ) ) ;
#41971 = AXIS2_PLACEMENT_3D ( 'NONE', #41752, #23348, #8956 ) ;
#41973 = FACE_OUTER_BOUND ( 'NONE', #47186, .T. ) ;
#41972 = CARTESIAN_POINT ( 'NONE',  ( 0.06523048226347956391, -0.9207677165354321014, 0.1574803149606297803 ) ) ;
#41975 = CARTESIAN_POINT ( 'NONE',  ( -0.7799827560997787401, -0.1420106181070925344, 1.986315487003310620 ) ) ;
#41974 = CARTESIAN_POINT ( 'NONE',  ( 0.07444174185955065859, -1.642268219031864707, 0.1797182628040039087 ) ) ;
#41976 = CARTESIAN_POINT ( 'NONE',  ( -0.7185039370078739607, 1.928577636452523993E-17, 1.250000000000000000 ) ) ;
#41977 = CARTESIAN_POINT ( 'NONE',  ( 0.1787899950787401604, -0.3375984251430867999, 0.07405724077823318263 ) ) ;
#41978 = DIRECTION ( 'NONE',  ( 5.724375810226264544E-16, 0.6156614753256587358, 0.7880107536067215701 ) ) ;
#41979 = CARTESIAN_POINT ( 'NONE',  ( 0.7495606340400177148, -0.1264236179284866091, 1.468996062938362046 ) ) ;
#41980 = CARTESIAN_POINT ( 'NONE',  ( 0.9500414927467377701, 0.1787899950787401604, 1.840551181048599938 ) ) ;
#41981 = CARTESIAN_POINT ( 'NONE',  ( 0.8019270111902716547, -0.1787899950787401604, 0.3248031495525355861 ) ) ;
#41982 = EDGE_LOOP ( 'NONE', ( #522, #35189, #15093, #23183, #13554, #25045 ) ) ;
#41983 = DIRECTION ( 'NONE',  ( 0.000000000000000000, -1.000000000000000000, -0.000000000000000000 ) ) ;
#41984 = CARTESIAN_POINT ( 'NONE',  ( -0.1377952755905511861, 0.1574803149606320007, -0.7066929133858274037 ) ) ;
#41985 = DIRECTION ( 'NONE',  ( 0.000000000000000000, 0.000000000000000000, -1.000000000000000000 ) ) ;
#41987 = CARTESIAN_POINT ( 'NONE',  ( 0.1787899950787401882, 0.09301181107738563936, -2.189545951927503898E-17 ) ) ;
#41986 = CARTESIAN_POINT ( 'NONE',  ( -0.1574803149606300301, -0.8469488187901119680, -0.06523048226347956391 ) ) ;
#41988 = CARTESIAN_POINT ( 'NONE',  ( 0.9873396505805591694, -0.1113553986120547346, 0.5068897636720007815 ) ) ;
#41989 = VECTOR ( 'NONE', #29613, 39.37007874015748854 ) ;
#41990 = CARTESIAN_POINT ( 'NONE',  ( 0.7495606340400177148, -0.1264236179284866091, 0.4010826771115905687 ) ) ;
#41991 = CARTESIAN_POINT ( 'NONE',  ( 0.7185039370078739607, 1.928577636452523993E-17, 0.2263779527559055260 ) ) ;
#41992 = CARTESIAN_POINT ( 'NONE',  ( -0.7495606340400177148, -0.1264236179284866091, 1.345964566875370139 ) ) ;
#41993 = CARTESIAN_POINT ( 'NONE',  ( 0.9873396505805591694, -0.1113553986120547346, 0.7824803148531023211 ) ) ;
#41994 = ORIENTED_EDGE ( 'NONE', *, *, #41954, .T. ) ;
#41995 = AXIS2_PLACEMENT_3D ( 'NONE', #18397, #30173, #19090 ) ;
#41996 = CARTESIAN_POINT ( 'NONE',  ( 1.054774247047244540, -0.07405724077823318263, 1.008858267662772423 ) ) ;
#41997 = ORIENTED_EDGE ( 'NONE', *, *, #45701, .F. ) ;
#41999 = ORIENTED_EDGE ( 'NONE', *, *, #11231, .T. ) ;
#41998 = CARTESIAN_POINT ( 'NONE',  ( 0.07405724077823318263, -1.395669291284819868, -0.1787899950787401604 ) ) ;
#42000 = CARTESIAN_POINT ( 'NONE',  ( -1.033464566929134687, -0.06523048226347956391, 0.5880905510735753294 ) ) ;
#42001 = CARTESIAN_POINT ( 'NONE',  ( 0.9873396505805591694, 0.1113553986120547346, 0.09350393700787401619 ) ) ;
#42002 = CARTESIAN_POINT ( 'NONE',  ( -0.7185039370078746268, -0.06523048226347956391, 1.213090551181103427 ) ) ;
#42003 = CARTESIAN_POINT ( 'NONE',  ( 0.7185039370078746268, 0.06523048226347956391, 0.5782480314960627421 ) ) ;
#42005 = CARTESIAN_POINT ( 'NONE',  ( 0.000000000000000000, 0.000000000000000000, -0.3139606299212599483 ) ) ;
#42004 = DIRECTION ( 'NONE',  ( 0.000000000000000000, 0.000000000000000000, -1.000000000000000000 ) ) ;
#42006 = CARTESIAN_POINT ( 'NONE',  ( 0.8019270111902716547, 0.1787899950787401604, 0.1181102361667090567 ) ) ;
#42007 = CARTESIAN_POINT ( 'NONE',  ( -0.8019270111902716547, -0.1787899950787401604, 0.1279527558517483676 ) ) ;
#42008 = CARTESIAN_POINT ( 'NONE',  ( 0.9412147342319837628, -0.1574803149606297803, 1.370570866034205970 ) ) ;
#42009 = ORIENTED_EDGE ( 'NONE', *, *, #40711, .T. ) ;
#42010 = ORIENTED_EDGE ( 'NONE', *, *, #11332, .T. ) ;
#42011 = DIRECTION ( 'NONE',  ( 0.000000000000000000, 0.000000000000000000, -1.000000000000000000 ) ) ;
#42012 = PLANE ( 'NONE',  #22178 ) ;
#42013 = CARTESIAN_POINT ( 'NONE',  ( 0.8759842519685039353, 0.1787899950787401882, 0.7062007873478109987 ) ) ;
#42014 = ADVANCED_FACE ( 'NONE', ( #16714 ), #31344, .T. ) ;
#42015 = CARTESIAN_POINT ( 'NONE',  ( -0.9500414927467377701, -0.1787899950787401604, 1.747047244040724312 ) ) ;
#42016 = CARTESIAN_POINT ( 'NONE',  ( -0.06523048226347956391, -0.1825787400499532531, -0.1574803149606300301 ) ) ;
#42017 = ORIENTED_EDGE ( 'NONE', *, *, #24214, .T. ) ;
#42018 = EDGE_CURVE ( 'NONE', #36896, #42619, #12898, .T. ) ;
#42019 = CARTESIAN_POINT ( 'NONE',  ( 0.3980944881889776910, 0.3833307086614178294, 0.7480314960629921295 ) ) ;
#42020 = AXIS2_PLACEMENT_3D ( 'NONE', #28074, #5772, #16564 ) ;
#42021 = DIRECTION ( 'NONE',  ( 1.000000000000000000, -3.469446951953614583E-15, -1.144917494144684547E-16 ) ) ;
#42022 = DIRECTION ( 'NONE',  ( 0.000000000000000000, 0.000000000000000000, 1.000000000000000000 ) ) ;
#42023 = CARTESIAN_POINT ( 'NONE',  ( -0.07405724077823318263, -1.150714519410340753, 0.1787899950787401604 ) ) ;
#42024 = ORIENTED_EDGE ( 'NONE', *, *, #12957, .F. ) ;
#42025 = CARTESIAN_POINT ( 'NONE',  ( 0.1264236179284866091, -0.1038385826234017734, 0.1264236179284866091 ) ) ;
#42026 = ORIENTED_EDGE ( 'NONE', *, *, #17805, .T. ) ;
#42027 = ORIENTED_EDGE ( 'NONE', *, *, #33699, .T. ) ;
#42028 = ADVANCED_FACE ( 'NONE', ( #31116 ), #42335, .T. ) ;
#42029 = DIRECTION ( 'NONE',  ( 0.000000000000000000, 0.9771240687918556489, 0.2126700594527794475 ) ) ;
#42030 = CIRCLE ( 'NONE', #10665, 0.09842519685039370636 ) ;
#42031 = DIRECTION ( 'NONE',  ( 1.000000000000000000, -3.469446951953613794E-15, -0.000000000000000000 ) ) ;
#42032 = EDGE_CURVE ( 'NONE', #6761, #24301, #8564, .T. ) ;
#42033 = CARTESIAN_POINT ( 'NONE',  ( 0.7185039370078746268, -0.06523048226347956391, 1.803641732283465693 ) ) ;
#42034 = AXIS2_PLACEMENT_3D ( 'NONE', #9027, #23424, #38739 ) ;
#42035 = CARTESIAN_POINT ( 'NONE',  ( 0.1787899950787401882, -0.6550196849856062542, -2.189545951927503898E-17 ) ) ;
#42036 = ORIENTED_EDGE ( 'NONE', *, *, #29054, .F. ) ;
#42037 = ( BOUNDED_CURVE ( )  B_SPLINE_CURVE ( 2, ( #20539, #10727, #7352, #14314, #600, #15257, #33250, #29209, #40613 ),
 .UNSPECIFIED., .F., .T. ) 
 B_SPLINE_CURVE_WITH_KNOTS ( ( 3, 2, 2, 2, 3 ),
 ( 0.2700000000000000178, 0.2725000000000000200, 0.2750000000000000222, 0.2775000000000000244, 0.2800000000000000266 ),
 .UNSPECIFIED. ) 
 CURVE ( )  GEOMETRIC_REPRESENTATION_ITEM ( )  RATIONAL_B_SPLINE_CURVE ( ( 1.000000000000000000, 0.9238795325112869605, 1.000000000000000000, 0.9238795325112869605, 1.000000000000000000, 0.9238795325112869605, 1.000000000000000000, 0.9238795325112869605, 1.000000000000000000 ) ) 
 REPRESENTATION_ITEM ( '' )  ) ;
#42038 = CARTESIAN_POINT ( 'NONE',  ( -1.054774247047244540, 0.07405724077823318263, 0.3444881889226146243 ) ) ;
#42039 = CARTESIAN_POINT ( 'NONE',  ( -0.9873396505805591694, -0.1113553986120547346, 1.028543307086614123 ) ) ;
#42040 = CARTESIAN_POINT ( 'NONE',  ( 0.1797182628040039365, -1.162445384386194824, -2.200913952912460540E-17 ) ) ;
#42041 = CARTESIAN_POINT ( 'NONE',  ( 0.7646288533564489232, 0.1113553986120547346, 0.4183070866141732624 ) ) ;
#42042 = CARTESIAN_POINT ( 'NONE',  ( 1.054774247047244540, 0.07405724077823318263, 0.2214566928596221063 ) ) ;
#42043 = CARTESIAN_POINT ( 'NONE',  ( 0.9412147342319837628, -0.1574803149606297803, 0.2386811023622048278 ) ) ;
#42044 = CARTESIAN_POINT ( 'NONE',  ( 0.7185039370078746268, 0.06523048226347956391, 1.523129921259841923 ) ) ;
#42046 = DIRECTION ( 'NONE',  ( -1.000000000000000000, 0.000000000000000000, 0.000000000000000000 ) ) ;
#42045 = CARTESIAN_POINT ( 'NONE',  ( 0.8107537697050254399, -0.1574803149606297803, 1.414862204724410377 ) ) ;
#42047 = CARTESIAN_POINT ( 'NONE',  ( -0.01380083870287700763, -0.09697728935039548470, 0.1574803149606300023 ) ) ;
#42048 = CARTESIAN_POINT ( 'NONE',  ( 0.1574803149606299191, -0.7460629920184567165, -1.928577636452523993E-17 ) ) ;
#42049 = CARTESIAN_POINT ( 'NONE',  ( 0.1787899950787401882, 0.05856299217974772486, -2.189545951927503898E-17 ) ) ;
#42050 = CARTESIAN_POINT ( 'NONE',  ( 0.9873396505805591694, -0.1113553986120547346, 1.658464566929134021 ) ) ;
#42051 = CARTESIAN_POINT ( 'NONE',  ( 0.6971942568897648851, -0.07405724077823297447, 0.9104330708123777871 ) ) ;
#42052 = VECTOR ( 'NONE', #1348, 39.37007874015748143 ) ;
#42053 = CARTESIAN_POINT ( 'NONE',  ( 0.9500414927467377701, 0.1787899950787401604, 1.963582677111591401 ) ) ;
#42054 = CARTESIAN_POINT ( 'NONE',  ( 0.7646288533564489232, 0.1113553986120547346, 0.3690944880814492901 ) ) ;
#42055 = VERTEX_POINT ( 'NONE', #34236 ) ;
#42056 = CARTESIAN_POINT ( 'NONE',  ( 1.000925231368313018, 0.1081788907238402098, 0.03936919960863846657 ) ) ;
#42057 = CARTESIAN_POINT ( 'NONE',  ( -1.033464566929133799, 0.000000000000000000, 1.062992125876724314 ) ) ;
#42058 = CARTESIAN_POINT ( 'NONE',  ( 0.06523048226347956391, -1.644192913278300860, -0.1574803149606300301 ) ) ;
#42059 = CARTESIAN_POINT ( 'NONE',  ( -0.8107537697050234415, -0.1574803149606297803, 0.2632874014672759722 ) ) ;
#42060 = CARTESIAN_POINT ( 'NONE',  ( 1.054774247047244540, -0.07405724077823318263, 1.240157480261197431 ) ) ;
#42061 = EDGE_CURVE ( 'NONE', #36671, #27780, #15736, .T. ) ;
#42062 = CARTESIAN_POINT ( 'NONE',  ( 0.8759842519685039353, 0.1574803149606299191, 1.230314960522393752 ) ) ;
#42064 = AXIS2_PLACEMENT_3D ( 'NONE', #34811, #42652, #30749 ) ;
#42063 = CARTESIAN_POINT ( 'NONE',  ( -0.07405724077823318263, 0.08562992131360593062, 0.1787899950787401604 ) ) ;
#42065 = DIRECTION ( 'NONE',  ( -1.000000000000000000, 0.000000000000000000, 0.000000000000000000 ) ) ;
#42066 = CARTESIAN_POINT ( 'NONE',  ( -0.6971942568897626646, 0.07405724077823318263, 0.6299212597887560161 ) ) ;
#42067 = CARTESIAN_POINT ( 'NONE',  ( -0.7185039370078746268, -0.06523048226347956391, 0.2682086614173227468 ) ) ;
#42068 = FACE_OUTER_BOUND ( 'NONE', #44330, .T. ) ;
#42069 = VERTEX_POINT ( 'NONE', #32533 ) ;
#42070 = EDGE_CURVE ( 'NONE', #19175, #43630, #28224, .T. ) ;
#42072 = CARTESIAN_POINT ( 'NONE',  ( -0.07405724077823318263, -1.690944881836001334, 0.1787899950787401604 ) ) ;
#42071 = CARTESIAN_POINT ( 'NONE',  ( 0.1113553986120547346, -0.3868110235145200693, -0.1113553986120547346 ) ) ;
#42073 = CARTESIAN_POINT ( 'NONE',  ( -0.8019270111902717657, 0.1787899950787401604, 1.023622047190330342 ) ) ;
#42074 = CARTESIAN_POINT ( 'NONE',  ( -1.054774247047244540, -0.07405724077823318263, 1.988188976324187562 ) ) ;
#42075 = VERTEX_POINT ( 'NONE', #46635 ) ;
#42076 = CARTESIAN_POINT ( 'NONE',  ( -0.8759842519685039353, 0.1787899950787401882, 0.9768700786863937502 ) ) ;
#42077 = CARTESIAN_POINT ( 'NONE',  ( -0.8759842519685039353, 0.1787899950787401882, 0.7455708660879684091 ) ) ;
#42078 = DIRECTION ( 'NONE',  ( -1.000000000000000000, 0.000000000000000000, 0.000000000000000000 ) ) ;
#42079 = LINE ( 'NONE', #4961, #23659 ) ;
#42080 = CARTESIAN_POINT ( 'NONE',  ( 0.1787899950787401882, -0.7447105824024665699, -2.189545951927503898E-17 ) ) ;
#42081 = ORIENTED_EDGE ( 'NONE', *, *, #37554, .F. ) ;
#42082 = CARTESIAN_POINT ( 'NONE',  ( -0.1484669515004454765, -0.08956113575196811283, -0.09387933231569273174 ) ) ;
#42083 = CARTESIAN_POINT ( 'NONE',  ( 0.7185039370078746268, -0.06523048226347956391, 1.921751968503937480 ) ) ;
#42084 = ORIENTED_EDGE ( 'NONE', *, *, #7679, .T. ) ;
#42085 = CARTESIAN_POINT ( 'NONE',  ( 0.1574803149606299746, -0.2714884749021747590, -1.284167712019358198 ) ) ;
#42086 = CARTESIAN_POINT ( 'NONE',  ( -0.6971942568897626646, 0.07405724077823318263, 0.4724409448281262636 ) ) ;
#42087 = DIRECTION ( 'NONE',  ( -1.000000000000000000, 0.000000000000000000, 0.000000000000000000 ) ) ;
#42089 = ORIENTED_EDGE ( 'NONE', *, *, #36108, .T. ) ;
#42088 = AXIS2_PLACEMENT_3D ( 'NONE', #36339, #21705, #46852 ) ;
#42090 = CARTESIAN_POINT ( 'NONE',  ( -0.7495606340400177148, 0.1264236179284866091, 1.695374015694267822 ) ) ;
#42091 = VECTOR ( 'NONE', #26602, 39.37007874015748143 ) ;
#42092 = CARTESIAN_POINT ( 'NONE',  ( 0.1264236179284866091, -1.437499999946236340, -0.1264236179284866091 ) ) ;
#42093 = AXIS2_PLACEMENT_3D ( 'NONE', #30184, #8318, #11704 ) ;
#42094 = DIRECTION ( 'NONE',  ( 0.000000000000000000, 0.000000000000000000, -1.000000000000000000 ) ) ;
#42095 = CARTESIAN_POINT ( 'NONE',  ( -0.1476377952755905387, -0.9875035750853327077, -1.463737590216208861 ) ) ;
#42096 = CARTESIAN_POINT ( 'NONE',  ( 3.301370929368692659E-17, -0.7392170379295019966, 0.1797182628040039365 ) ) ;
#42097 = CARTESIAN_POINT ( 'NONE',  ( -0.8759842519685039353, 0.1574803149606299191, 1.230314960522393752 ) ) ;
#42099 = CARTESIAN_POINT ( 'NONE',  ( 0.8070866141732283561, 0.000000000000000000, 0.7574803149606299524 ) ) ;
#42098 = CARTESIAN_POINT ( 'NONE',  ( -0.1574803149606299191, -0.5000000000000000000, 0.000000000000000000 ) ) ;
#42100 = CARTESIAN_POINT ( 'NONE',  ( -0.7185039370078746268, 0.06523048226347956391, 1.198326771546015967 ) ) ;
#42101 = ORIENTED_EDGE ( 'NONE', *, *, #4250, .F. ) ;
#42102 = DIRECTION ( 'NONE',  ( 0.000000000000000000, 0.000000000000000000, -1.000000000000000000 ) ) ;
#42103 = CARTESIAN_POINT ( 'NONE',  ( -0.6971942568897648851, -0.07405724077823297447, 1.112204724355684959 ) ) ;
#42104 = CARTESIAN_POINT ( 'NONE',  ( 0.8107537697050253289, -0.1574803149606297803, 1.060531496062992352 ) ) ;
#42106 = CARTESIAN_POINT ( 'NONE',  ( -0.7185039370078739607, 0.000000000000000000, -2.869337061179095023E-17 ) ) ;
#42105 = CARTESIAN_POINT ( 'NONE',  ( 0.000000000000000000, 0.000000000000000000, 0.000000000000000000 ) ) ;
#42107 = CARTESIAN_POINT ( 'NONE',  ( 0.1377952755905513804, 0.000000000000000000, -0.3001770169643759867 ) ) ;
#42109 = CARTESIAN_POINT ( 'NONE',  ( -0.9873396505805591694, -0.1113553986120547346, 1.963582677057826853 ) ) ;
#42108 = FACE_OUTER_BOUND ( 'NONE', #39311, .T. ) ;
#42110 = CARTESIAN_POINT ( 'NONE',  ( 0.8759842519685039353, 0.1574803149606299191, 0.6003937006798740761 ) ) ;
#42111 = CARTESIAN_POINT ( 'NONE',  ( 3.284318927891251994E-17, -0.5812007873478111097, 0.1787899950787401882 ) ) ;
#42112 = CARTESIAN_POINT ( 'NONE',  ( -0.3053042314538801927, 0.05494681823601579862, 0.7175656113863903007 ) ) ;
#42113 = CARTESIAN_POINT ( 'NONE',  ( 1.054774247047244540, 0.07405724077823318263, 0.7726377952218265177 ) ) ;
#42114 = EDGE_CURVE ( 'NONE', #16713, #29837, #22574, .T. ) ;
#42115 = CARTESIAN_POINT ( 'NONE',  ( 0.7185039370078739607, 1.928577636452523993E-17, 1.446850393700787274 ) ) ;
#42116 = CARTESIAN_POINT ( 'NONE',  ( -0.7185039370078746268, 0.06523048226347956391, 0.4502952754830242821 ) ) ;
#42117 = CARTESIAN_POINT ( 'NONE',  ( 3.284318927891251994E-17, -1.762303149552535642, 0.1787899950787401882 ) ) ;
#42118 = CARTESIAN_POINT ( 'NONE',  ( 0.1787899950787401604, -1.090551181048598606, 0.07405724077823318263 ) ) ;
#42119 = CARTESIAN_POINT ( 'NONE',  ( -0.1113553986120547346, -1.371062992125984259, -0.1113553986120547346 ) ) ;
#42120 = EDGE_CURVE ( 'NONE', #19153, #6659, #25079, .T. ) ;
#42121 = CARTESIAN_POINT ( 'NONE',  ( 0.8107537697050254399, -0.1574803149606297803, 1.168799212490898576 ) ) ;
#42122 = AXIS2_PLACEMENT_3D ( 'NONE', #45594, #6293, #45835 ) ;
#42123 = ORIENTED_EDGE ( 'NONE', *, *, #31033, .T. ) ;
#42124 = ORIENTED_EDGE ( 'NONE', *, *, #24724, .F. ) ;
#42125 = CARTESIAN_POINT ( 'NONE',  ( -0.8019270111902717657, -0.1787899950787401604, 1.983267716481667886 ) ) ;
#42126 = EDGE_CURVE ( 'NONE', #34753, #460, #5260, .T. ) ;
#42127 = CARTESIAN_POINT ( 'NONE',  ( 0.7495606340400177148, -0.1264236179284866091, 1.823326771599779406 ) ) ;
#42128 = ORIENTED_EDGE ( 'NONE', *, *, #22625, .F. ) ;
#42129 = CARTESIAN_POINT ( 'NONE',  ( 0.8107537697050254399, -0.1574803149606297803, 1.769192913385826404 ) ) ;
#42130 = CARTESIAN_POINT ( 'NONE',  ( 0.9500414927467378812, 0.1787899950787401604, 0.3887795275052913224 ) ) ;
#42131 = AXIS2_PLACEMENT_3D ( 'NONE', #42308, #31792, #34673 ) ;
#42132 = CARTESIAN_POINT ( 'NONE',  ( -0.6971942568897637749, 2.189545951927499583E-17, 1.301673228292692830 ) ) ;
#42133 = EDGE_CURVE ( 'NONE', #8550, #32499, #32860, .T. ) ;
#42134 = DIRECTION ( 'NONE',  ( 0.000000000000000000, 0.000000000000000000, 1.000000000000000000 ) ) ;
#42135 = AXIS2_PLACEMENT_3D ( 'NONE', #1518, #27452, #24299 ) ;
#42136 = CARTESIAN_POINT ( 'NONE',  ( -1.054774247047244540, 0.07405724077823318263, 0.3051181101824569919 ) ) ;
#42137 = CARTESIAN_POINT ( 'NONE',  ( -0.7185039370078739607, 1.928577636452523993E-17, 0.5807086614173228023 ) ) ;
#42138 = CARTESIAN_POINT ( 'NONE',  ( -0.6971942568897648851, -0.07405724077823297447, 1.663385826717890925 ) ) ;
#42139 = CARTESIAN_POINT ( 'NONE',  ( -0.1711856790334027878, 0.08819060268785008927, 0.1865989729947978293 ) ) ;
#42140 = CARTESIAN_POINT ( 'NONE',  ( -0.9873396505805591694, 0.1113553986120547346, 1.786417322834645605 ) ) ;
#42141 = CARTESIAN_POINT ( 'NONE',  ( -0.7646288533564489232, -0.1113553986120547346, 0.9399606299212598381 ) ) ;
#42142 = CARTESIAN_POINT ( 'NONE',  ( -1.094772975963752103E-17, -0.3017971965756956476, -0.1787899950787401882 ) ) ;
#42143 = CONICAL_SURFACE ( 'NONE', #45213, 0.1003937007874010356, 0.7853981633978559529 ) ;
#42144 = CARTESIAN_POINT ( 'NONE',  ( 1.002407869896990045, -0.1264236179284866091, 1.715059055064346527 ) ) ;
#42145 = CARTESIAN_POINT ( 'NONE',  ( -0.03864956553883512613, -0.09842519685039370636, 0.2227303740875846427 ) ) ;
#42146 = CARTESIAN_POINT ( 'NONE',  ( -1.033464566929134687, -0.06523048226347956391, 0.7455708660342049710 ) ) ;
#42147 = B_SPLINE_CURVE_WITH_KNOTS ( 'NONE', 3,
 ( #1179, #30462, #41416, #34286, #12482, #27107, #41656, #5257, #9813, #20814, #35452, #31165, #9344, #35224, #19877, #5735, #28043, #10041, #6190 ),
 .UNSPECIFIED., .F., .F.,
 ( 4, 2, 2, 1, 2, 2, 2, 2, 2, 4 ),
 ( 0.000000000000000000, 0.2500000000000006661, 0.3750000000000009992, 0.4375000000000009437, 0.4687500000000006661, 0.5000000000000004441, 0.6250000000000000000, 0.6875000000000000000, 0.7500000000000001110, 1.000000000000000000 ),
 .UNSPECIFIED. ) ;
#42148 = ORIENTED_EDGE ( 'NONE', *, *, #44773, .T. ) ;
#42149 = CARTESIAN_POINT ( 'NONE',  ( -0.8019270111902716547, 0.1787899950787401604, 1.259842519631276359 ) ) ;
#42150 = ORIENTED_EDGE ( 'NONE', *, *, #24787, .T. ) ;
#42151 = CARTESIAN_POINT ( 'NONE',  ( 0.1787899950787401604, -1.051181102308440529, 0.07405724077823318263 ) ) ;
#42152 = CARTESIAN_POINT ( 'NONE',  ( 0.1787899950787401604, -1.203740157426551383, 0.07405724077823318263 ) ) ;
#42153 = VECTOR ( 'NONE', #31367, 39.37007874015748143 ) ;
#42154 = CARTESIAN_POINT ( 'NONE',  ( -0.9412147342319837628, 0.1574803149606300301, 1.277066929133857442 ) ) ;
#42155 = ( NAMED_UNIT ( * ) PLANE_ANGLE_UNIT ( ) SI_UNIT ( $, .RADIAN. ) ) ;
#42156 = CARTESIAN_POINT ( 'NONE',  ( 0.1270800023317771588, -0.4488627072208409285, -0.1270800023317771588 ) ) ;
#42157 = CARTESIAN_POINT ( 'NONE',  ( -0.1574803149606299191, -1.789370078632629868, 0.000000000000000000 ) ) ;
#42158 = CARTESIAN_POINT ( 'NONE',  ( -0.7646288533564489232, 0.1113553986120547346, 0.7627952754830236159 ) ) ;
#42159 = CARTESIAN_POINT ( 'NONE',  ( 2.892866454678787531E-17, 0.06102362204724409711, 0.1574803149606299191 ) ) ;
#42160 = VECTOR ( 'NONE', #26755, 39.37007874015748143 ) ;
#42161 = CIRCLE ( 'NONE', #835, 0.1673228346456692994 ) ;
#42162 = LINE ( 'NONE', #9606, #6192 ) ;
#42163 = CARTESIAN_POINT ( 'NONE',  ( 0.7495606340400177148, 0.1264236179284866091, 0.9817913385289134265 ) ) ;
#42164 = AXIS2_PLACEMENT_3D ( 'NONE', #22026, #18426, #10313 ) ;
#42166 = DIRECTION ( 'NONE',  ( 1.000000000000000000, 0.000000000000000000, 0.000000000000000000 ) ) ;
#42165 = CARTESIAN_POINT ( 'NONE',  ( 0.7185039370078746268, 0.06523048226347956391, 0.6176181102362199304 ) ) ;
#42167 = CARTESIAN_POINT ( 'NONE',  ( 0.8759842519685039353, 0.1574803149606299191, 0.04921259831766984505 ) ) ;
#42168 = CARTESIAN_POINT ( 'NONE',  ( 0.7185039370078746268, -0.06523048226347956391, 0.2288385826771656140 ) ) ;
#42169 = FACE_BOUND ( 'NONE', #6882, .T. ) ;
#42170 = CARTESIAN_POINT ( 'NONE',  ( 3.284318927891251994E-17, -0.5073818897100158543, 0.1787899950787401882 ) ) ;
#42171 = DIRECTION ( 'NONE',  ( 0.000000000000000000, -0.8660254037844384856, -0.5000000000000003331 ) ) ;
#42172 = CARTESIAN_POINT ( 'NONE',  ( -0.1264236179284866091, -1.452263779473795369, 0.1264236179284866091 ) ) ;
#42173 = ADVANCED_FACE ( 'NONE', ( #28217 ), #6490, .T. ) ;
#42174 = CARTESIAN_POINT ( 'NONE',  ( -0.7495606340400177148, 0.1264236179284866091, 1.887303149552535420 ) ) ;
#42175 = ORIENTED_EDGE ( 'NONE', *, *, #28714, .F. ) ;
#42176 = CARTESIAN_POINT ( 'NONE',  ( -0.8019270111902717657, -0.1787899950787401604, 1.392716535379308285 ) ) ;
#42177 = DIRECTION ( 'NONE',  ( 0.000000000000000000, 0.2432573283306931344, -0.9699617890481117000 ) ) ;
#42178 = ADVANCED_FACE ( 'NONE', ( #24846 ), #39444, .F. ) ;
#42179 = CARTESIAN_POINT ( 'NONE',  ( 1.002407869896990045, -0.1264236179284866091, 1.478838582623401399 ) ) ;
#42180 = CARTESIAN_POINT ( 'NONE',  ( -1.033464566929133799, 0.000000000000000000, 0.9153543307086614567 ) ) ;
#42181 = CARTESIAN_POINT ( 'NONE',  ( -0.1574803149606300301, -1.240649606191686072, -0.06523048226347956391 ) ) ;
#42182 = CARTESIAN_POINT ( 'NONE',  ( -1.002407869896990045, -0.1264236179284866091, 0.6914370078202519698 ) ) ;
#42183 = CARTESIAN_POINT ( 'NONE',  ( -0.8759842519685039353, -0.1787899950787401882, 1.232775590497417362 ) ) ;
#42184 = EDGE_CURVE ( 'NONE', #18202, #6796, #35864, .T. ) ;
#42185 = CARTESIAN_POINT ( 'NONE',  ( 0.1767609453248275564, -0.09842768728010117818, -0.02846602293845313172 ) ) ;
#42186 = CARTESIAN_POINT ( 'NONE',  ( 1.737901732061166719E-16, 0.1564960629921311464, 0.2933070866141737065 ) ) ;
#42187 = CARTESIAN_POINT ( 'NONE',  ( 1.054774247047244540, 0.07405724077823318263, 0.6200787401037166635 ) ) ;
#42188 = CARTESIAN_POINT ( 'NONE',  ( -0.6971942568897648851, 0.07405724077823318263, 0.5511811023084406402 ) ) ;
#42189 = CARTESIAN_POINT ( 'NONE',  ( -0.1574803149606299191, 1.928577636452524610E-17, -0.07924015748031493223 ) ) ;
#42190 = ( BOUNDED_CURVE ( )  B_SPLINE_CURVE ( 2, ( #32626, #2863, #29296, #7425, #21324, #33097, #3360, #218, #35955 ),
 .UNSPECIFIED., .F., .F. ) 
 B_SPLINE_CURVE_WITH_KNOTS ( ( 3, 2, 2, 2, 3 ),
 ( 0.2600000000000000089, 0.2625000000000000111, 0.2650000000000000133, 0.2675000000000000155, 0.2700000000000000178 ),
 .UNSPECIFIED. ) 
 CURVE ( )  GEOMETRIC_REPRESENTATION_ITEM ( )  RATIONAL_B_SPLINE_CURVE ( ( 1.000000000000000000, 0.9238795325112869605, 1.000000000000000000, 0.9238795325112869605, 1.000000000000000000, 0.9238795325112869605, 1.000000000000000000, 0.9238795325112869605, 1.000000000000000000 ) ) 
 REPRESENTATION_ITEM ( '' )  ) ;
#42191 = VECTOR ( 'NONE', #2101, 39.37007874015748143 ) ;
#42192 = FACE_OUTER_BOUND ( 'NONE', #22545, .T. ) ;
#42193 = VERTEX_POINT ( 'NONE', #32295 ) ;
#42194 = DIRECTION ( 'NONE',  ( -0.000000000000000000, -0.000000000000000000, -1.000000000000000000 ) ) ;
#42195 = CARTESIAN_POINT ( 'NONE',  ( -0.8759842519685039353, 0.1574803149606299191, 0.2559055118110236116 ) ) ;
#42196 = CARTESIAN_POINT ( 'NONE',  ( 0.9500414927467377701, -0.1787899950787401604, 1.318897637741511364 ) ) ;
#42197 = CARTESIAN_POINT ( 'NONE',  ( -0.2233098565426767657, -0.09851385024739447993, 0.08145678030718524198 ) ) ;
#42198 = CARTESIAN_POINT ( 'NONE',  ( -0.7185039370078766252, -0.06523048226348168721, 1.833169291231055542 ) ) ;
#42199 = AXIS2_PLACEMENT_3D ( 'NONE', #14963, #22129, #21419 ) ;
#42200 = ORIENTED_EDGE ( 'NONE', *, *, #38527, .T. ) ;
#42201 = AXIS2_PLACEMENT_3D ( 'NONE', #14273, #21691, #18089 ) ;
#42202 = VECTOR ( 'NONE', #31545, 39.37007874015748143 ) ;
#42203 = CARTESIAN_POINT ( 'NONE',  ( -1.054774247047244540, -0.07405724077823318263, 1.008858267662772423 ) ) ;
#42204 = CARTESIAN_POINT ( 'NONE',  ( 0.1264236179284866091, -1.605931054843411587, -0.1264236179284866091 ) ) ;
#42205 = ORIENTED_EDGE ( 'NONE', *, *, #8886, .F. ) ;
#42206 = CARTESIAN_POINT ( 'NONE',  ( 0.9873396505805591694, 0.1113553986120547346, 0.9990157480314961758 ) ) ;
#42207 = CARTESIAN_POINT ( 'NONE',  ( 0.1787899950787401882, -0.6107283464029291675, -2.189545951927503898E-17 ) ) ;
#42208 = CARTESIAN_POINT ( 'NONE',  ( -0.8107537697050234415, -0.1574803149606297803, 0.07627952755905519078 ) ) ;
#42209 = CARTESIAN_POINT ( 'NONE',  ( 0.7495606340400177148, -0.1264236179284866091, 1.464074803095842370 ) ) ;
#42210 = CARTESIAN_POINT ( 'NONE',  ( -0.1062722551319878611, 0.2341365745599054971, -0.3142669362052408211 ) ) ;
#42211 = FACE_OUTER_BOUND ( 'NONE', #22873, .T. ) ;
#42212 = ( BOUNDED_CURVE ( )  B_SPLINE_CURVE ( 2, ( #11456, #40882, #4003, #25838, #29480, #11938, #3553, #18166, #7603 ),
 .UNSPECIFIED., .F., .F. ) 
 B_SPLINE_CURVE_WITH_KNOTS ( ( 3, 2, 2, 2, 3 ),
 ( 0.8800000000000000044, 0.8824999999999999512, 0.8850000000000000089, 0.8874999999999999556, 0.8900000000000000133 ),
 .UNSPECIFIED. ) 
 CURVE ( )  GEOMETRIC_REPRESENTATION_ITEM ( )  RATIONAL_B_SPLINE_CURVE ( ( 1.000000000000000000, 0.9238795325112869605, 1.000000000000000000, 0.9238795325112869605, 1.000000000000000000, 0.9238795325112869605, 1.000000000000000000, 0.9238795325112869605, 1.000000000000000000 ) ) 
 REPRESENTATION_ITEM ( '' )  ) ;
#42213 = CARTESIAN_POINT ( 'NONE',  ( 0.1264236179284866091, -0.2957677164816697180, -0.1264236179284866091 ) ) ;
#42214 = CARTESIAN_POINT ( 'NONE',  ( -0.07405724077823318263, -0.7411417322297018107, 0.1787899950787401604 ) ) ;
#42215 = DIRECTION ( 'NONE',  ( -0.000000000000000000, -0.000000000000000000, -1.000000000000000000 ) ) ;
#42216 = FACE_OUTER_BOUND ( 'NONE', #9967, .T. ) ;
#42217 = CARTESIAN_POINT ( 'NONE',  ( 0.7495606340400177148, -0.1264236179284866091, 1.621555118056472455 ) ) ;
#42218 = CARTESIAN_POINT ( 'NONE',  ( 0.1787899950787401882, 0.04269099240068251894, -2.189545951927503898E-17 ) ) ;
#42219 = CARTESIAN_POINT ( 'NONE',  ( 3.284318927891251994E-17, 0.1225393701325037388, 0.1787899950787401882 ) ) ;
#42220 = APPLICATION_PROTOCOL_DEFINITION ( 'draft international standard', 'automotive_design', 1998, #11336 ) ;
#42221 = CARTESIAN_POINT ( 'NONE',  ( 0.1574803149606299191, 0.08719492171395729074, -0.5641677032617165022 ) ) ;
#42222 = VECTOR ( 'NONE', #46479, 39.37007874015748143 ) ;
#42223 = CARTESIAN_POINT ( 'NONE',  ( 1.002407869896990045, 0.1264236179284866091, 0.4601377952218267953 ) ) ;
#42224 = CIRCLE ( 'NONE', #20044, 0.1968503937007874405 ) ;
#42225 = CARTESIAN_POINT ( 'NONE',  ( -0.9500414927467377701, 0.1787899950787401604, 0.7431102361667091261 ) ) ;
#42227 = CARTESIAN_POINT ( 'NONE',  ( 0.3108999017613323090, 0.9251089822459547252, -1.060267534067256046 ) ) ;
#42226 = CARTESIAN_POINT ( 'NONE',  ( -0.1574803149606300301, -0.9749015748031498729, -0.06523048226347956391 ) ) ;
#42228 = CARTESIAN_POINT ( 'NONE',  ( 0.1797182628040039087, -1.632425699346824466, -0.07444174185955065859 ) ) ;
#42229 = CARTESIAN_POINT ( 'NONE',  ( 0.1787899950787401604, -0.3326771653005671237, -0.07405724077823318263 ) ) ;
#42230 = CARTESIAN_POINT ( 'NONE',  ( -0.8759842519685039353, 0.1574803149606299191, 1.033464566821606478 ) ) ;
#42231 = CARTESIAN_POINT ( 'NONE',  ( 1.054774247047244540, -0.07405724077823318263, 1.441929133804504604 ) ) ;
#42232 = CARTESIAN_POINT ( 'NONE',  ( 0.1806410355270341994, 0.08353766247254058863, -0.1811399203779157918 ) ) ;
#42233 = CARTESIAN_POINT ( 'NONE',  ( 0.7495606340400177148, 0.1264236179284866091, 0.4306102361667086820 ) ) ;
#42234 = EDGE_LOOP ( 'NONE', ( #38197, #21870, #20746, #9648 ) ) ;
#42235 = AXIS2_PLACEMENT_3D ( 'NONE', #25750, #7743, #36982 ) ;
#42236 = AXIS2_PLACEMENT_3D ( 'NONE', #7712, #40055, #15399 ) ;
#42237 = CARTESIAN_POINT ( 'NONE',  ( -0.9873396505805591694, -0.1113553986120547346, 0.1525590550105832555 ) ) ;
#42238 = DIRECTION ( 'NONE',  ( -0.000000000000000000, -0.7880107536067214591, 0.6156614753256588468 ) ) ;
#42239 = CARTESIAN_POINT ( 'NONE',  ( 0.1279527559055118058, -0.2216206741968047289, -0.3149606299212598381 ) ) ;
#42240 = CARTESIAN_POINT ( 'NONE',  ( -1.094772975963752103E-17, -0.01525590545804752021, -0.1787899950787401882 ) ) ;
#42241 = CARTESIAN_POINT ( 'NONE',  ( 3.284318927891251994E-17, -0.03001968498560657339, 0.1787899950787401882 ) ) ;
#42242 = CARTESIAN_POINT ( 'NONE',  ( 0.8759842519685039353, -0.1787899950787401882, 0.4060039369541102450 ) ) ;
#42243 = CARTESIAN_POINT ( 'NONE',  ( -1.094772975963752103E-17, -0.9945866141194644738, -0.1787899950787401882 ) ) ;
#42244 = EDGE_CURVE ( 'NONE', #40844, #42055, #46168, .T. ) ;
#42245 = FACE_OUTER_BOUND ( 'NONE', #3293, .T. ) ;
#42246 = CARTESIAN_POINT ( 'NONE',  ( -1.054774247047244540, 0.07405724077823318263, 1.402559055064346971 ) ) ;
#42247 = CARTESIAN_POINT ( 'NONE',  ( 0.8107537697050253289, -0.1574803149606297803, 0.8538385825696385156 ) ) ;
#42248 = ORIENTED_EDGE ( 'NONE', *, *, #5419, .T. ) ;
#42249 = CARTESIAN_POINT ( 'NONE',  ( -1.033464566929133799, 0.000000000000000000, 0.1181102361129454797 ) ) ;
#42250 = CARTESIAN_POINT ( 'NONE',  ( 0.9500414927467378812, 0.1787899950787401604, 0.9399606298674970661 ) ) ;
#42251 = ORIENTED_EDGE ( 'NONE', *, *, #4975, .T. ) ;
#42254 = ORIENTED_EDGE ( 'NONE', *, *, #23599, .T. ) ;
#42253 = CARTESIAN_POINT ( 'NONE',  ( 0.1787899950787401882, -1.403051181048598384, -2.189545951927503898E-17 ) ) ;
#42252 = CARTESIAN_POINT ( 'NONE',  ( 2.892866454678787531E-17, -1.070866141624756018, 0.1574803149606299191 ) ) ;
#42255 = CARTESIAN_POINT ( 'NONE',  ( -0.8759842519685039353, 0.1574803149606299191, 0.6397637794200314865 ) ) ;
#42256 = CARTESIAN_POINT ( 'NONE',  ( 0.2759478392031617933, 0.3740157480314960647, 1.713085361781125915 ) ) ;
#42257 = CARTESIAN_POINT ( 'NONE',  ( -1.033464566929134687, 0.06523048226347956391, 1.429625984251968074 ) ) ;
#42258 = EDGE_CURVE ( 'NONE', #5428, #46578, #27992, .T. ) ;
#42259 = CARTESIAN_POINT ( 'NONE',  ( -1.033464566929134687, 0.06523048226347956391, 0.5142716534357801850 ) ) ;
#42261 = LINE ( 'NONE', #17101, #28555 ) ;
#42260 = CARTESIAN_POINT ( 'NONE',  ( -1.033464566929134687, 0.06523048226347956391, 0.7209645669291341319 ) ) ;
#42262 = CARTESIAN_POINT ( 'NONE',  ( 0.8759842519685039353, -0.1787899950787401882, 0.2140748030958428971 ) ) ;
#42263 = CARTESIAN_POINT ( 'NONE',  ( 0.9873396505805591694, -0.1113553986120547346, 1.373031495955464587 ) ) ;
#42264 = ORIENTED_EDGE ( 'NONE', *, *, #10963, .T. ) ;
#42265 = EDGE_LOOP ( 'NONE', ( #46500, #42512, #32056, #26218 ) ) ;
#42266 = DIRECTION ( 'NONE',  ( 0.000000000000000000, 0.000000000000000000, 1.000000000000000000 ) ) ;
#42267 = CARTESIAN_POINT ( 'NONE',  ( -0.02739131347899105909, -0.09752745740044843625, 0.1550798682808147422 ) ) ;
#42268 = CARTESIAN_POINT ( 'NONE',  ( -0.7495606340400177148, 0.1264236179284866091, 1.729822834591905556 ) ) ;
#42269 = VERTEX_POINT ( 'NONE', #20763 ) ;
#42270 = VECTOR ( 'NONE', #33608, 39.37007874015748143 ) ;
#42271 = VECTOR ( 'NONE', #44656, 39.37007874015748143 ) ;
#42272 = DIRECTION ( 'NONE',  ( -0.000000000000000000, 1.000000000000000000, -0.000000000000000000 ) ) ;
#42273 = CARTESIAN_POINT ( 'NONE',  ( 0.7185039370078739607, 1.928577636452523993E-17, 1.594488188868850242 ) ) ;
#42274 = CARTESIAN_POINT ( 'NONE',  ( 0.07405724077823318263, -1.067053102087507366, 0.1787899950787401604 ) ) ;
#42275 = ORIENTED_EDGE ( 'NONE', *, *, #43745, .F. ) ;
#42276 = CARTESIAN_POINT ( 'NONE',  ( 0.1264236179284866091, -0.1825787401037169411, 0.1264236179284866091 ) ) ;
#42277 = ORIENTED_EDGE ( 'NONE', *, *, #35776, .F. ) ;
#42278 = ORIENTED_EDGE ( 'NONE', *, *, #29231, .F. ) ;
#42279 = CONICAL_SURFACE ( 'NONE', #21626, 0.1377952755905509363, 0.9599310885968936891 ) ;
#42280 = CARTESIAN_POINT ( 'NONE',  ( 0.7646288533564489232, 0.1113553986120547346, 1.747047243986960652 ) ) ;
#42281 = EDGE_CURVE ( 'NONE', #14529, #41944, #31314, .T. ) ;
#42282 = CARTESIAN_POINT ( 'NONE',  ( -1.033464566929133799, 0.000000000000000000, 1.466535433070866201 ) ) ;
#42283 = PRODUCT_DEFINITION_SHAPE ( 'NONE', 'NONE',  #24794 ) ;
#42284 = CARTESIAN_POINT ( 'NONE',  ( 0.8107537697050253289, 0.1574803149606300301, 1.872539370078740495 ) ) ;
#42285 = CARTESIAN_POINT ( 'NONE',  ( -1.094772975963752103E-17, -0.5664370078202519698, -0.1787899950787401882 ) ) ;
#42286 = CARTESIAN_POINT ( 'NONE',  ( -0.9500414927467377701, -0.1787899950787401604, 0.3346456692375752162 ) ) ;
#42287 = CARTESIAN_POINT ( 'NONE',  ( -0.7185039370078739607, 1.928577636452523993E-17, 1.092519685039370136 ) ) ;
#42288 = CARTESIAN_POINT ( 'NONE',  ( -0.1270800023317771588, -1.177209163913754075, 0.1270800023317771588 ) ) ;
#42289 = CARTESIAN_POINT ( 'NONE',  ( -0.1219373188186450574, 0.2250936884182012654, -0.02739586109244948955 ) ) ;
#42290 = CARTESIAN_POINT ( 'NONE',  ( 1.054774247047244540, -0.07405724077823318263, 1.087598425143086578 ) ) ;
#42291 = CARTESIAN_POINT ( 'NONE',  ( 1.054774247047244540, -0.07405724077823318263, 1.397637795221827517 ) ) ;
#42292 = CARTESIAN_POINT ( 'NONE',  ( 0.9500414927467377701, -0.1787899950787401604, 0.2116141731745827814 ) ) ;
#42293 = CARTESIAN_POINT ( 'NONE',  ( 0.9873396505805591694, -0.1113553986120547346, 0.2411417322834645827 ) ) ;
#42294 = EDGE_CURVE ( 'NONE', #38421, #17885, #19943, .T. ) ;
#42295 = CARTESIAN_POINT ( 'NONE',  ( 0.8759842519685039353, 0.1574803149606299191, 1.633858267716535639 ) ) ;
#42296 = EDGE_CURVE ( 'NONE', #47458, #22666, #30124, .T. ) ;
#42298 = CARTESIAN_POINT ( 'NONE',  ( 0.7185039370078739607, 1.928577636452523993E-17, 1.722440944881889813 ) ) ;
#42297 = CARTESIAN_POINT ( 'NONE',  ( 0.7560775457342543415, 0.1089356967155813427, 1.980950116515386217 ) ) ;
#42299 = CARTESIAN_POINT ( 'NONE',  ( 0.5660731898098425585, 0.09842519685039370636, 0.000000000000000000 ) ) ;
#42300 = CARTESIAN_POINT ( 'NONE',  ( -0.1787899950787401604, 0.1151574803687242243, -0.07405724077823318263 ) ) ;
#42301 = AXIS2_PLACEMENT_3D ( 'NONE', #13743, #39603, #35334 ) ;
#42302 = CARTESIAN_POINT ( 'NONE',  ( -1.181102362204724310, -0.3937007874015748254, -0.9842519685039370358 ) ) ;
#42303 = EDGE_CURVE ( 'NONE', #13605, #4124, #19830, .T. ) ;
#42304 = CARTESIAN_POINT ( 'NONE',  ( 0.8019270111902716547, 0.1787899950787401604, 0.9399606298674970661 ) ) ;
#42305 = CARTESIAN_POINT ( 'NONE',  ( -1.002407869896990045, -0.1264236179284866091, 1.158956692859621995 ) ) ;
#42306 = CARTESIAN_POINT ( 'NONE',  ( 0.9873396505805591694, 0.1113553986120547346, 0.3986220471365669038 ) ) ;
#42307 = ORIENTED_EDGE ( 'NONE', *, *, #29035, .F. ) ;
#42308 = CARTESIAN_POINT ( 'NONE',  ( -0.2362204724409464052, 0.1574803149606323616, 0.9891732283464568232 ) ) ;
#42309 = CARTESIAN_POINT ( 'NONE',  ( 1.032071497351902956, 0.03428311989231668661, 0.03936989784698766148 ) ) ;
#42310 = CARTESIAN_POINT ( 'NONE',  ( -0.6971942568897637749, 2.189545951927499583E-17, 0.8341535432533228045 ) ) ;
#42311 = CARTESIAN_POINT ( 'NONE',  ( -0.1113553986120547346, -1.705708661309795149, 0.1113553986120547346 ) ) ;
#42312 = CARTESIAN_POINT ( 'NONE',  ( -0.9873396505805591694, 0.1113553986120547346, 0.3198818896562523606 ) ) ;
#42313 = CARTESIAN_POINT ( 'NONE',  ( 0.8019270111902717657, 0.1787899950787401604, 1.294291338528912982 ) ) ;
#42314 = ADVANCED_FACE ( 'NONE', ( #44739 ), #29512, .T. ) ;
#42316 = CARTESIAN_POINT ( 'NONE',  ( 0.8759842519685039353, 0.000000000000000000, 4.498031496062992574 ) ) ;
#42315 = CARTESIAN_POINT ( 'NONE',  ( 0.03837864586585212900, -0.06712557525767723354, 0.2632749781601034789 ) ) ;
#42317 = CARTESIAN_POINT ( 'NONE',  ( 0.06523048226347956391, -1.786909448818898571, 0.1574803149606297803 ) ) ;
#42318 = CARTESIAN_POINT ( 'NONE',  ( -0.6195511811023656223, 0.6102362204724407491, 1.186023622047243986 ) ) ;
#42319 = CARTESIAN_POINT ( 'NONE',  ( -0.9500414927467378812, 0.1787899950787401604, 0.6200787401037165525 ) ) ;
#42320 = FACE_OUTER_BOUND ( 'NONE', #4501, .T. ) ;
#42321 = CARTESIAN_POINT ( 'NONE',  ( -0.08643384275325982635, 0.09202339627320535453, 0.2355304684854533370 ) ) ;
#42322 = ORIENTED_EDGE ( 'NONE', *, *, #46459, .T. ) ;
#42323 = CARTESIAN_POINT ( 'NONE',  ( 0.1787899950787401604, -1.681102362150960650, 0.07405724077823318263 ) ) ;
#42324 = CARTESIAN_POINT ( 'NONE',  ( -0.8019270111902717657, -0.1787899950787401604, 0.9596456692375764375 ) ) ;
#42325 = CARTESIAN_POINT ( 'NONE',  ( -0.8107537697050253289, 0.1574803149606300301, 0.06151574803149607168 ) ) ;
#42326 = CARTESIAN_POINT ( 'NONE',  ( -1.002407869896990045, 0.1264236179284866091, 0.9719488188438739629 ) ) ;
#42327 = CARTESIAN_POINT ( 'NONE',  ( -1.002407869896990045, 0.1264236179284866091, 0.6619094487651338010 ) ) ;
#42328 = CARTESIAN_POINT ( 'NONE',  ( 0.1583756834309467398, 0.1213737535021009450, -0.01438113282651966134 ) ) ;
#42329 = CARTESIAN_POINT ( 'NONE',  ( -0.7185039370078739607, 1.928577636452523993E-17, 0.09842519674286673292 ) ) ;
#42330 = CARTESIAN_POINT ( 'NONE',  ( 0.07405724077823318263, -0.6733523146859311526, 0.1787899950787401604 ) ) ;
#42331 = ORIENTED_EDGE ( 'NONE', *, *, #42871, .F. ) ;
#42332 = CARTESIAN_POINT ( 'NONE',  ( -0.1377866315803517872, -0.08956094045033681506, -0.1113219018184753994 ) ) ;
#42333 = CARTESIAN_POINT ( 'NONE',  ( -0.2066929133858267931, 0.7443365962042343131, -3.523993443072799270 ) ) ;
#42334 = ORIENTED_EDGE ( 'NONE', *, *, #10243, .F. ) ;
#42335 = CYLINDRICAL_SURFACE ( 'NONE', #38659, 0.09842519685039370636 ) ;
#42336 = CARTESIAN_POINT ( 'NONE',  ( 0.7185039370078739607, 1.928577636452523993E-17, 1.761811023622047223 ) ) ;
#42337 = CARTESIAN_POINT ( 'NONE',  ( -0.8759842519685039353, 0.1787899950787401882, 0.5831692912848189803 ) ) ;
#42338 = CARTESIAN_POINT ( 'NONE',  ( 0.4811709046783464450, 4.466152701071653354E-17, 0.000000000000000000 ) ) ;
#42339 = ORIENTED_EDGE ( 'NONE', *, *, #4497, .F. ) ;
#42340 = CARTESIAN_POINT ( 'NONE',  ( -0.8019270111902716547, -0.1787899950787401604, 1.628937007820252303 ) ) ;
#42341 = AXIS2_PLACEMENT_3D ( 'NONE', #32366, #17715, #32113 ) ;
#42342 = DIRECTION ( 'NONE',  ( 1.000000000000000000, 0.000000000000000000, 0.000000000000000000 ) ) ;
#42343 = CARTESIAN_POINT ( 'NONE',  ( -1.033464566929133799, 0.000000000000000000, 0.1968503935932602311 ) ) ;
#42344 = CARTESIAN_POINT ( 'NONE',  ( 0.9412147342319837628, 0.1574803149606300301, 0.6471456692913394315 ) ) ;
#42345 = CARTESIAN_POINT ( 'NONE',  ( 0.8107537697050253289, -0.1574803149606297803, 0.5487204724409447953 ) ) ;
#42346 = CARTESIAN_POINT ( 'NONE',  ( 0.1270800023317771588, -0.7638233371421003781, -0.1270800023317771588 ) ) ;
#42347 = CARTESIAN_POINT ( 'NONE',  ( 0.2471922904502826812, 0.08811029028641703675, 0.05516800237527588052 ) ) ;
#42348 = CARTESIAN_POINT ( 'NONE',  ( -0.8107537697050253289, 0.1574803149606300301, 1.232775590443654812 ) ) ;
#42349 = ADVANCED_FACE ( 'NONE', ( #8097 ), #41672, .F. ) ;
#42350 = DIRECTION ( 'NONE',  ( 0.000000000000000000, 0.000000000000000000, 1.000000000000000000 ) ) ;
#42352 = CARTESIAN_POINT ( 'NONE',  ( -0.1439004954719960427, -0.09842519685039366473, 0.08538203236020840137 ) ) ;
#42351 = CARTESIAN_POINT ( 'NONE',  ( 2.892866454678787531E-17, -0.3720472440944881942, 0.1574803149606299191 ) ) ;
#42353 = CARTESIAN_POINT ( 'NONE',  ( -1.033464566929133799, 0.000000000000000000, 1.742125984251968518 ) ) ;
#42354 = ORIENTED_EDGE ( 'NONE', *, *, #25392, .F. ) ;
#42355 = DIRECTION ( 'NONE',  ( 0.000000000000000000, 1.000000000000000000, 0.000000000000000000 ) ) ;
#42356 = CARTESIAN_POINT ( 'NONE',  ( 1.033464566929134687, -0.06523048226347956391, 1.109744094488189115 ) ) ;
#42358 = PLANE ( 'NONE',  #24712 ) ;
#42357 = CARTESIAN_POINT ( 'NONE',  ( 0.1822895153388602307, 0.000000000000000000, -0.2114570894355444486 ) ) ;
#42359 = LINE ( 'NONE', #23466, #45754 ) ;
#42360 = CARTESIAN_POINT ( 'NONE',  ( -0.1574803149606299191, -0.6082677164279055582, 0.000000000000000000 ) ) ;
#42361 = ADVANCED_FACE ( 'NONE', ( #4475 ), #37881, .T. ) ;
#42363 = DIRECTION ( 'NONE',  ( 0.000000000000000000, 0.000000000000000000, 1.000000000000000000 ) ) ;
#42362 = FACE_OUTER_BOUND ( 'NONE', #4476, .T. ) ;
#42364 = CARTESIAN_POINT ( 'NONE',  ( 1.033464566929133799, 0.000000000000000000, 1.663385826771653697 ) ) ;
#42365 = CARTESIAN_POINT ( 'NONE',  ( -0.1264236179284866091, -0.5861220471903307860, 0.1264236179284866091 ) ) ;
#42366 = CARTESIAN_POINT ( 'NONE',  ( 0.1574803149606299746, -0.09842519685039370636, 1.713085361781126803 ) ) ;
#42367 = CARTESIAN_POINT ( 'NONE',  ( 0.8019270111902717657, -0.1787899950787401604, 0.8366141731745828647 ) ) ;
#42368 = EDGE_LOOP ( 'NONE', ( #13571, #41847, #33759, #4416 ) ) ;
#42369 = CARTESIAN_POINT ( 'NONE',  ( 0.8107537697050254399, -0.1574803149606297803, 1.296751968503936592 ) ) ;
#42370 = CARTESIAN_POINT ( 'NONE',  ( -0.7185039370078746268, 0.06523048226347956391, 0.5388779527559055538 ) ) ;
#42371 = CARTESIAN_POINT ( 'NONE',  ( 0.1797182628040039087, 0.09493650537758448194, 0.07444174185955046430 ) ) ;
#42372 = CARTESIAN_POINT ( 'NONE',  ( 0.1787899950787401882, -1.127460629867496067, -2.189545951927503898E-17 ) ) ;
#42373 = CARTESIAN_POINT ( 'NONE',  ( -0.1113553986120547346, -1.292322834645669438, -0.1113553986120547346 ) ) ;
#42374 = CARTESIAN_POINT ( 'NONE',  ( 0.7185039370078739607, 1.928577636452523993E-17, 1.161417322727118284 ) ) ;
#42375 = ORIENTED_EDGE ( 'NONE', *, *, #20352, .F. ) ;
#42376 = CARTESIAN_POINT ( 'NONE',  ( -0.8019270111902717657, 0.1787899950787401604, 1.929133858213952335 ) ) ;
#42377 = CARTESIAN_POINT ( 'NONE',  ( 0.8759842519685039353, -0.1787899950787401882, 1.788877952702141672 ) ) ;
#42378 = ORIENTED_EDGE ( 'NONE', *, *, #42184, .F. ) ;
#42379 = CARTESIAN_POINT ( 'NONE',  ( -0.06523048226347956391, -1.348917322727117174, 0.1574803149606297803 ) ) ;
#42380 = CARTESIAN_POINT ( 'NONE',  ( 0.9412147342319837628, -0.1574803149606297803, 1.774114173228345859 ) ) ;
#42381 = CARTESIAN_POINT ( 'NONE',  ( -1.054774247047244096, 0.000000000000000000, 1.478838582623401399 ) ) ;
#42382 = DIRECTION ( 'NONE',  ( 0.000000000000000000, 0.000000000000000000, 1.000000000000000000 ) ) ;
#42383 = CARTESIAN_POINT ( 'NONE',  ( -0.8019270111902717657, 0.1787899950787401604, 0.3149606298674962890 ) ) ;
#42384 = DIRECTION ( 'NONE',  ( 1.000000000000000000, -3.368395098984144529E-15, 0.000000000000000000 ) ) ;
#42385 = CARTESIAN_POINT ( 'NONE',  ( -1.002407869896990045, 0.1264236179284866091, 1.685531496009228469 ) ) ;
#42386 = CARTESIAN_POINT ( 'NONE',  ( -0.8107537697050253289, 0.1574803149606300301, 1.675688976377952777 ) ) ;
#42387 = AXIS2_PLACEMENT_3D ( 'NONE', #33541, #43575, #25398 ) ;
#42388 = CARTESIAN_POINT ( 'NONE',  ( 0.2559042684362457520, 0.05603847011398876976, -0.04023020774663194771 ) ) ;
#42389 = CARTESIAN_POINT ( 'NONE',  ( -0.07405724077823318263, -0.2205964091741206001, -0.1787899950787401604 ) ) ;
#42390 = CARTESIAN_POINT ( 'NONE',  ( 0.6971942568897648851, 0.07405724077823318263, 1.697834645615527771 ) ) ;
#42391 = CARTESIAN_POINT ( 'NONE',  ( 0.1098058327898338432, -0.09842519685039370636, 0.1888946959883346655 ) ) ;
#42392 = CARTESIAN_POINT ( 'NONE',  ( 0.5415383587465882886, 1.205361022782824954E-17, -0.09842519685039370636 ) ) ;
#42393 = CARTESIAN_POINT ( 'NONE',  ( -0.8107537697050254399, 0.1574803149606300301, 0.05167322823892971789 ) ) ;
#42394 = VERTEX_POINT ( 'NONE', #41132 ) ;
#42395 = VERTEX_POINT ( 'NONE', #41604 ) ;
#42396 = CARTESIAN_POINT ( 'NONE',  ( -1.054774247047244096, 0.000000000000000000, 1.208169291284818980 ) ) ;
#42397 = VERTEX_POINT ( 'NONE', #1607 ) ;
#42398 = EDGE_CURVE ( 'NONE', #46714, #8724, #17213, .T. ) ;
#42399 = CARTESIAN_POINT ( 'NONE',  ( -0.1787899950787401604, -1.297244094434425010, 0.07405724077823318263 ) ) ;
#42400 = DIRECTION ( 'NONE',  ( -1.000000000000000000, -0.000000000000000000, 0.000000000000000000 ) ) ;
#42401 = CARTESIAN_POINT ( 'NONE',  ( -0.1797182628040039087, -0.4316382977720212843, 0.07444174185955065859 ) ) ;
#42402 = CARTESIAN_POINT ( 'NONE',  ( 0.1113553986120547346, -1.774606299105070839, 0.1113553986120547346 ) ) ;
#42403 = CARTESIAN_POINT ( 'NONE',  ( -1.033464566929134687, 0.06523048226347956391, 0.8686023620971983217 ) ) ;
#42404 = CARTESIAN_POINT ( 'NONE',  ( -0.8759842519685039353, 0.1574803149606299191, 0.6889763779527560139 ) ) ;
#42405 = EDGE_CURVE ( 'NONE', #954, #15682, #8807, .T. ) ;
#42406 = CARTESIAN_POINT ( 'NONE',  ( 0.06523048226347956391, -0.05462598425196847629, 0.1574803149606297803 ) ) ;
#42407 = CARTESIAN_POINT ( 'NONE',  ( 1.002407869896990045, -0.1264236179284866091, 1.001476377898992132 ) ) ;
#42409 = CARTESIAN_POINT ( 'NONE',  ( 0.1618465483937499283, -0.06719994080176183715, 0.1405161193130591291 ) ) ;
#42408 = CARTESIAN_POINT ( 'NONE',  ( 0.1985616933439197651, 0.1808545851595462772, -0.05455490385609955417 ) ) ;
#42410 = AXIS2_PLACEMENT_3D ( 'NONE', #35927, #2613, #14132 ) ;
#42411 = CARTESIAN_POINT ( 'NONE',  ( 0.7646288533564489232, 0.1113553986120547346, 0.05413385816018952829 ) ) ;
#42412 = CARTESIAN_POINT ( 'NONE',  ( -0.1787899950787401882, -0.5565944881352126172, 0.000000000000000000 ) ) ;
#42413 = CARTESIAN_POINT ( 'NONE',  ( 3.284318927891251994E-17, -1.368602362150960650, 0.1787899950787401882 ) ) ;
#42414 = CARTESIAN_POINT ( 'NONE',  ( -1.054774247047244540, 0.07405724077823318263, 1.953740157426552715 ) ) ;
#42415 = EDGE_LOOP ( 'NONE', ( #11991, #7554, #27469, #45670, #25904, #41408 ) ) ;
#42416 = VERTEX_POINT ( 'NONE', #45451 ) ;
#42417 = CARTESIAN_POINT ( 'NONE',  ( -0.6971942568897637749, 2.189545951927499583E-17, 1.385334645615527549 ) ) ;
#42418 = CARTESIAN_POINT ( 'NONE',  ( 1.002407869896990045, 0.1264236179284866091, 1.409940944828126153 ) ) ;
#42419 = DIRECTION ( 'NONE',  ( 1.822029033848725028E-16, 0.000000000000000000, 1.000000000000000000 ) ) ;
#42420 = CYLINDRICAL_SURFACE ( 'NONE', #4410, 0.1574803149606299191 ) ;
#42421 = CARTESIAN_POINT ( 'NONE',  ( 0.8759842519685039353, -0.1787899950787401882, 0.6865157479777322935 ) ) ;
#42422 = CARTESIAN_POINT ( 'NONE',  ( -1.054774247047244096, 0.000000000000000000, 0.4945866141194645849 ) ) ;
#42423 = CARTESIAN_POINT ( 'NONE',  ( 0.7185039370078739607, 1.928577636452523993E-17, 0.6200787401574803237 ) ) ;
#42424 = CARTESIAN_POINT ( 'NONE',  ( 1.033464566929133799, 0.000000000000000000, 1.653543306979086580 ) ) ;
#42425 = EDGE_LOOP ( 'NONE', ( #30371, #24637, #17120, #21764, #29520 ) ) ;
#42426 = ORIENTED_EDGE ( 'NONE', *, *, #17045, .T. ) ;
#42427 = CARTESIAN_POINT ( 'NONE',  ( 0.000000000000000000, 0.000000000000000000, -0.1828167807439035619 ) ) ;
#42428 = CARTESIAN_POINT ( 'NONE',  ( -0.7185039370078746268, -0.06523048226347956391, 0.3469488188976379561 ) ) ;
#42429 = CARTESIAN_POINT ( 'NONE',  ( 0.8759842519685039353, 0.1787899950787401882, 1.336122047190330786 ) ) ;
#42430 = CARTESIAN_POINT ( 'NONE',  ( 0.2074133033502960355, -0.09851384765663445675, 0.004766324057523401575 ) ) ;
#42431 = DIRECTION ( 'NONE',  ( 0.000000000000000000, -1.000000000000000000, 0.000000000000000000 ) ) ;
#42432 = CIRCLE ( 'NONE', #38622, 0.02900000000000001882 ) ;
#42433 = AXIS2_PLACEMENT_3D ( 'NONE', #11845, #26234, #15920 ) ;
#42434 = VERTEX_POINT ( 'NONE', #41848 ) ;
#42435 = CYLINDRICAL_SURFACE ( 'NONE', #36360, 0.1574803149606299191 ) ;
#42436 = CARTESIAN_POINT ( 'NONE',  ( -1.054774247047244540, 0.07405724077823318263, 0.9350393700249758355 ) ) ;
#42437 = CARTESIAN_POINT ( 'NONE',  ( -1.094772975963752103E-17, -1.640379873741049321, -0.1787899950787401882 ) ) ;
#42438 = EDGE_LOOP ( 'NONE', ( #22392, #10687, #12919, #17333 ) ) ;
#42439 = CARTESIAN_POINT ( 'NONE',  ( -0.1787899950787401882, -0.5123031495525355306, 0.000000000000000000 ) ) ;
#42440 = DIRECTION ( 'NONE',  ( -1.000000000000000000, -2.980860836206319941E-17, 2.307906111702434570E-17 ) ) ;
#42441 = VERTEX_POINT ( 'NONE', #15553 ) ;
#42442 = EDGE_CURVE ( 'NONE', #2951, #15186, #46275, .T. ) ;
#42443 = CARTESIAN_POINT ( 'NONE',  ( -0.07405724077823318263, -0.2736220471903310081, 0.1787899950787401604 ) ) ;
#42444 = EDGE_CURVE ( 'NONE', #24988, #8606, #43991, .T. ) ;
#42445 = CARTESIAN_POINT ( 'NONE',  ( 0.07405724077823318263, -0.7755905511273385455, 0.1787899950787401604 ) ) ;
#42446 = CARTESIAN_POINT ( 'NONE',  ( 1.033464566929133799, 0.000000000000000000, 0.5118110235145204578 ) ) ;
#42447 = DIRECTION ( 'NONE',  ( -1.000000000000000000, 0.000000000000000000, 0.000000000000000000 ) ) ;
#42448 = CARTESIAN_POINT ( 'NONE',  ( 0.8019270111902717657, -0.1787899950787401604, 1.702755905458047003 ) ) ;
#42449 = EDGE_CURVE ( 'NONE', #43974, #15794, #37570, .T. ) ;
#42450 = CARTESIAN_POINT ( 'NONE',  ( -0.07405724077823318263, 0.05499414200698173744, -0.1787899950787401604 ) ) ;
#42451 = CARTESIAN_POINT ( 'NONE',  ( -0.1264236179284866091, 0.07824803154982658271, 0.1264236179284866091 ) ) ;
#42452 = PRODUCT_CONTEXT ( 'NONE', #3691, 'mechanical' ) ;
#42453 = CARTESIAN_POINT ( 'NONE',  ( -0.02321135729119747776, -0.09842519685039372024, 0.1582298369811388494 ) ) ;
#42454 = AXIS2_PLACEMENT_3D ( 'NONE', #6942, #29289, #28794 ) ;
#42455 = ADVANCED_FACE ( 'NONE', ( #30650 ), #35589, .T. ) ;
#42456 = CARTESIAN_POINT ( 'NONE',  ( 0.6971942568897626646, -0.07405724077823297447, 0.5167322834108034613 ) ) ;
#42457 = CARTESIAN_POINT ( 'NONE',  ( -0.6971942568897648851, -0.07405724077823297447, 0.8366141731745828647 ) ) ;
#42459 = DIRECTION ( 'NONE',  ( 0.000000000000000000, 0.000000000000000000, -1.000000000000000000 ) ) ;
#42458 = CARTESIAN_POINT ( 'NONE',  ( -0.06523048226347956391, -0.8617125984251972071, -0.1574803149606300301 ) ) ;
#42461 = CARTESIAN_POINT ( 'NONE',  ( -0.7747212423720944985, -0.1378797577226987259, 1.986191570711806964 ) ) ;
#42460 = CARTESIAN_POINT ( 'NONE',  ( 0.1270800023317771588, -1.639807589110604313, 0.1270800023317771588 ) ) ;
#42462 = VECTOR ( 'NONE', #2371, 39.37007874015748854 ) ;
#42463 = CARTESIAN_POINT ( 'NONE',  ( -0.1787899950787401604, -0.3966535432533230265, -0.07405724077823318263 ) ) ;
#42464 = CARTESIAN_POINT ( 'NONE',  ( 0.9500414927467378812, 0.1787899950787401604, 1.451771653489543290 ) ) ;
#42466 = DIRECTION ( 'NONE',  ( -0.4230299666438205319, 0.000000000000000000, -0.9061156920180379881 ) ) ;
#42465 = CARTESIAN_POINT ( 'NONE',  ( 0.8019270111902716547, -0.1787899950787401604, 1.978346456639149098 ) ) ;
#42467 = CARTESIAN_POINT ( 'NONE',  ( 0.8019270111902716547, 0.1787899950787401604, 0.4281496062454490659 ) ) ;
#42468 = AXIS2_PLACEMENT_3D ( 'NONE', #26803, #20297, #16485 ) ;
#42469 = AXIS2_PLACEMENT_3D ( 'NONE', #10248, #24618, #14072 ) ;
#42470 = CARTESIAN_POINT ( 'NONE',  ( 0.8759842519685039353, 0.000000000000000000, 4.498031496062992574 ) ) ;
#42471 = DIRECTION ( 'NONE',  ( 0.000000000000000000, -1.000000000000000000, 0.000000000000000000 ) ) ;
#42472 = CARTESIAN_POINT ( 'NONE',  ( 0.1787899950787401882, -0.06446850388324429360, -2.189545951927503898E-17 ) ) ;
#42473 = CARTESIAN_POINT ( 'NONE',  ( 0.8019270111902717657, 0.1787899950787401604, 0.4675196849856070869 ) ) ;
#42474 = CARTESIAN_POINT ( 'NONE',  ( -0.1264236179284866091, -0.8715551180564724554, -0.1264236179284866091 ) ) ;
#42475 = CARTESIAN_POINT ( 'NONE',  ( 1.033464566929134687, -0.06523048226347956391, 0.08612204724409450174 ) ) ;
#42476 = ( BOUNDED_CURVE ( )  B_SPLINE_CURVE ( 2, ( #11914, #40167, #7367, #39938, #33268, #43776, #25595, #21979, #36602 ),
 .UNSPECIFIED., .F., .F. ) 
 B_SPLINE_CURVE_WITH_KNOTS ( ( 3, 2, 2, 2, 3 ),
 ( 0.7299999999999999822, 0.7325000000000000400, 0.7349999999999999867, 0.7375000000000000444, 0.7399999999999999911 ),
 .UNSPECIFIED. ) 
 CURVE ( )  GEOMETRIC_REPRESENTATION_ITEM ( )  RATIONAL_B_SPLINE_CURVE ( ( 1.000000000000000000, 0.9238795325112939549, 1.000000000000000000, 0.9238795325112869605, 1.000000000000000000, 0.9238795325112869605, 1.000000000000000000, 0.9238795325112869605, 1.000000000000000000 ) ) 
 REPRESENTATION_ITEM ( '' )  ) ;
#42477 = CARTESIAN_POINT ( 'NONE',  ( -0.7185039370078739607, 1.928577636452523993E-17, 0.7381889763779527769 ) ) ;
#42478 = CARTESIAN_POINT ( 'NONE',  ( -1.054774247047244540, -0.07405724077823318263, 1.437007873961985371 ) ) ;
#42479 = VERTEX_POINT ( 'NONE', #3975 ) ;
#42480 = CARTESIAN_POINT ( 'NONE',  ( -0.9500414927467378812, 0.1787899950787401604, 1.097440944828127041 ) ) ;
#42481 = CARTESIAN_POINT ( 'NONE',  ( 0.6971942568897637749, 2.189545951927499583E-17, 0.9522637794737952577 ) ) ;
#42482 = EDGE_LOOP ( 'NONE', ( #35750, #38047, #20470, #2073 ) ) ;
#42483 = CARTESIAN_POINT ( 'NONE',  ( -1.033464566929134687, 0.06523048226347956391, 0.5142716534357801850 ) ) ;
#42484 = CARTESIAN_POINT ( 'NONE',  ( 0.6971942568897648851, 0.07405724077823318263, 1.692913385773008539 ) ) ;
#42485 = DIRECTION ( 'NONE',  ( 0.000000000000000000, 0.000000000000000000, 1.000000000000000000 ) ) ;
#42486 = CARTESIAN_POINT ( 'NONE',  ( 0.6971942568897637749, 2.189545951927499583E-17, 0.1648622046706460786 ) ) ;
#42487 = CARTESIAN_POINT ( 'NONE',  ( -0.8019270111902716547, -0.1787899950787401604, 0.08858267711159095725 ) ) ;
#42488 = CARTESIAN_POINT ( 'NONE',  ( 1.033464566929134687, 0.06523048226347956391, 1.459153543199560144 ) ) ;
#42489 = VERTEX_POINT ( 'NONE', #26520 ) ;
#42490 = ORIENTED_EDGE ( 'NONE', *, *, #32872, .T. ) ;
#42491 = CARTESIAN_POINT ( 'NONE',  ( 0.8759842519685039353, 0.1574803149606299191, 1.781496062884598164 ) ) ;
#42492 = CARTESIAN_POINT ( 'NONE',  ( -1.002407869896990045, 0.1264236179284866091, 1.680610236166708793 ) ) ;
#42493 = ORIENTED_EDGE ( 'NONE', *, *, #45099, .F. ) ;
#42494 = ORIENTED_EDGE ( 'NONE', *, *, #28826, .F. ) ;
#42495 = ( BOUNDED_CURVE ( )  B_SPLINE_CURVE ( 2, ( #46209, #28040, #42600, #9811, #38149, #27163, #1241, #3734, #1717 ),
 .UNSPECIFIED., .F., .T. ) 
 B_SPLINE_CURVE_WITH_KNOTS ( ( 3, 2, 2, 2, 3 ),
 ( 0.2200000000000000011, 0.2225000000000000033, 0.2250000000000000056, 0.2275000000000000078, 0.2300000000000000100 ),
 .UNSPECIFIED. ) 
 CURVE ( )  GEOMETRIC_REPRESENTATION_ITEM ( )  RATIONAL_B_SPLINE_CURVE ( ( 1.000000000000000000, 0.9238795325112869605, 1.000000000000000000, 0.9238795325112869605, 1.000000000000000000, 0.9238795325112869605, 1.000000000000000000, 0.9238795325112869605, 1.000000000000000000 ) ) 
 REPRESENTATION_ITEM ( '' )  ) ;
#42496 = DIRECTION ( 'NONE',  ( 0.000000000000000000, 1.000000000000000000, 0.000000000000000000 ) ) ;
#42497 = AXIS2_PLACEMENT_3D ( 'NONE', #21960, #33478, #371 ) ;
#42498 = ( BOUNDED_CURVE ( )  B_SPLINE_CURVE ( 2, ( #3295, #21267, #43063, #46904, #6885, #35892, #10756, #13607, #10510 ),
 .UNSPECIFIED., .F., .T. ) 
 B_SPLINE_CURVE_WITH_KNOTS ( ( 3, 2, 2, 2, 3 ),
 ( 0.3499999999999999778, 0.3524999999999999800, 0.3549999999999999822, 0.3574999999999999845, 0.3599999999999999867 ),
 .UNSPECIFIED. ) 
 CURVE ( )  GEOMETRIC_REPRESENTATION_ITEM ( )  RATIONAL_B_SPLINE_CURVE ( ( 1.000000000000000000, 0.9238795325112879597, 1.000000000000000000, 0.9238795325112869605, 1.000000000000000000, 0.9238795325112869605, 1.000000000000000000, 0.9238795325112869605, 1.000000000000000000 ) ) 
 REPRESENTATION_ITEM ( '' )  ) ;
#42499 = CARTESIAN_POINT ( 'NONE',  ( 0.5555748031496118289, 1.194414586609139128, -0.06082000038405787484 ) ) ;
#42500 = CARTESIAN_POINT ( 'NONE',  ( -0.07405724077823318263, -1.190084598150498607, 0.1787899950787401604 ) ) ;
#42501 = ORIENTED_EDGE ( 'NONE', *, *, #40924, .T. ) ;
#42502 = CARTESIAN_POINT ( 'NONE',  ( 0.1787899950787401882, -0.09891732278088229136, -2.189545951927503898E-17 ) ) ;
#42503 = EDGE_LOOP ( 'NONE', ( #13619, #18233, #26319, #5954 ) ) ;
#42504 = CIRCLE ( 'NONE', #25687, 0.009842519685039330044 ) ;
#42505 = VECTOR ( 'NONE', #5264, 39.37007874015748143 ) ;
#42506 = ORIENTED_EDGE ( 'NONE', *, *, #15612, .T. ) ;
#42507 = CARTESIAN_POINT ( 'NONE',  ( -0.2559040288302377730, -0.08492902731590018517, -0.3070526160130827575 ) ) ;
#42508 = CARTESIAN_POINT ( 'NONE',  ( -0.8107537697050254399, 0.1574803149606300301, 0.9178149605223947516 ) ) ;
#42509 = EDGE_CURVE ( 'NONE', #5319, #36821, #10170, .T. ) ;
#42510 = CARTESIAN_POINT ( 'NONE',  ( 0.9412147342319837628, 0.1574803149606300301, 1.828248031496063630 ) ) ;
#42511 = CARTESIAN_POINT ( 'NONE',  ( -0.07405724077823318263, -0.7214566928596228834, -0.1787899950787401604 ) ) ;
#42512 = ORIENTED_EDGE ( 'NONE', *, *, #11600, .T. ) ;
#42513 = EDGE_CURVE ( 'NONE', #25167, #4886, #37218, .T. ) ;
#42514 = CARTESIAN_POINT ( 'NONE',  ( -0.8019270111902716547, 0.1787899950787401604, 0.3937007873478114983 ) ) ;
#42515 = CARTESIAN_POINT ( 'NONE',  ( -0.7185039370078746268, 0.06523048226347956391, 0.9719488188976380671 ) ) ;
#42516 = CARTESIAN_POINT ( 'NONE',  ( -0.1797182628040039087, -1.223961132417690889, -0.07444174185955065859 ) ) ;
#42517 = CARTESIAN_POINT ( 'NONE',  ( -0.8107537697050254399, 0.1574803149606300301, 0.2189960629921262614 ) ) ;
#42518 = CARTESIAN_POINT ( 'NONE',  ( 0.9500414927467378812, 0.1787899950787401604, 1.136811023568283119 ) ) ;
#42519 = CARTESIAN_POINT ( 'NONE',  ( 0.8759842519685039353, -0.1787899950787401882, 1.468996062938362046 ) ) ;
#42520 = CARTESIAN_POINT ( 'NONE',  ( 0.8019270111902716547, -0.1787899950787401604, 0.1673228345919057503 ) ) ;
#42521 = CIRCLE ( 'NONE', #20350, 0.009842519685039428923 ) ;
#42522 = DIRECTION ( 'NONE',  ( 1.822029033848725028E-16, 0.000000000000000000, 1.000000000000000000 ) ) ;
#42524 = CARTESIAN_POINT ( 'NONE',  ( -1.033464566929133799, 0.000000000000000000, 1.151574803149606474 ) ) ;
#42523 = CARTESIAN_POINT ( 'NONE',  ( 0.7959181182529732057, 0.1389122916488840231, 1.979994088609052127 ) ) ;
#42525 = CARTESIAN_POINT ( 'NONE',  ( 1.033464566929134687, -0.06523048226347956391, 0.7849409447743629364 ) ) ;
#42526 = CARTESIAN_POINT ( 'NONE',  ( -0.8759842519685039353, 0.000000000000000000, 0.000000000000000000 ) ) ;
#42527 = CARTESIAN_POINT ( 'NONE',  ( 0.6971942568897637749, 2.189545951927499583E-17, 1.144192913332062966 ) ) ;
#42528 = CARTESIAN_POINT ( 'NONE',  ( 0.9500414927467377701, -0.1787899950787401604, 1.988188976324191781 ) ) ;
#42529 = CARTESIAN_POINT ( 'NONE',  ( 0.9412147342319837628, 0.1574803149606300301, 0.4010826770578274081 ) ) ;
#42530 = ORIENTED_EDGE ( 'NONE', *, *, #1541, .F. ) ;
#42531 = CARTESIAN_POINT ( 'NONE',  ( 0.1377952755905511861, 0.000000000000000000, -0.05390369169704170571 ) ) ;
#42532 = CARTESIAN_POINT ( 'NONE',  ( -0.7185039370078746268, 0.06523048226347956391, 0.1747047243019218821 ) ) ;
#42533 = ORIENTED_EDGE ( 'NONE', *, *, #36897, .T. ) ;
#42534 = CARTESIAN_POINT ( 'NONE',  ( 0.7495606340400177148, -0.1264236179284866091, 1.227854330654897685 ) ) ;
#42536 = DIRECTION ( 'NONE',  ( -0.000000000000000000, -0.000000000000000000, -1.000000000000000000 ) ) ;
#42535 = FACE_BOUND ( 'NONE', #20621, .T. ) ;
#42537 = CARTESIAN_POINT ( 'NONE',  ( 0.1787899950787401604, 0.05610236225848785896, 0.07405724077823318263 ) ) ;
#42538 = EDGE_CURVE ( 'NONE', #20302, #44293, #29845, .T. ) ;
#42539 = CARTESIAN_POINT ( 'NONE',  ( -0.9873396505805591694, 0.1113553986120547346, 1.865157480314960647 ) ) ;
#42540 = ORIENTED_EDGE ( 'NONE', *, *, #42120, .T. ) ;
#42541 = FACE_OUTER_BOUND ( 'NONE', #13409, .T. ) ;
#42542 = DIRECTION ( 'NONE',  ( 0.000000000000000000, 0.000000000000000000, 1.000000000000000000 ) ) ;
#42543 = ORIENTED_EDGE ( 'NONE', *, *, #21771, .F. ) ;
#42544 = EDGE_LOOP ( 'NONE', ( #33089, #38435, #40542, #10957 ) ) ;
#42545 = CARTESIAN_POINT ( 'NONE',  ( -0.7495606340400177148, 0.1264236179284866091, 1.375492125930488196 ) ) ;
#42547 = CARTESIAN_POINT ( 'NONE',  ( -0.07405724077823318263, -1.626968503883244876, -0.1787899950787401604 ) ) ;
#42546 = CARTESIAN_POINT ( 'NONE',  ( 2.892866454678787531E-17, -0.4015748030420787651, 0.1574803149606299191 ) ) ;
#42548 = CARTESIAN_POINT ( 'NONE',  ( -0.9500414927467378812, -0.1787899950787401604, 0.9251968503399374821 ) ) ;
#42549 = CARTESIAN_POINT ( 'NONE',  ( -0.8019270111902717657, -0.1787899950787401604, 1.978346456639149320 ) ) ;
#42550 = ORIENTED_EDGE ( 'NONE', *, *, #10572, .F. ) ;
#42551 = CARTESIAN_POINT ( 'NONE',  ( -0.8019270111902716547, 0.1787899950787401604, 0.9793307086076531442 ) ) ;
#42552 = CARTESIAN_POINT ( 'NONE',  ( -0.8759842519685039353, -0.1787899950787401882, 0.7258858267178898149 ) ) ;
#42553 = CARTESIAN_POINT ( 'NONE',  ( 0.001144830380275972063, 0.02367899979687082546, -0.1377991226254607904 ) ) ;
#42554 = CARTESIAN_POINT ( 'NONE',  ( 0.1787899950787401604, -0.7028798737410506536, -0.07405724077823318263 ) ) ;
#42555 = VERTEX_POINT ( 'NONE', #1255 ) ;
#42556 = CARTESIAN_POINT ( 'NONE',  ( 0.09025693572801693487, -0.08956069895912480150, -0.1695530491970364262 ) ) ;
#42557 = ORIENTED_EDGE ( 'NONE', *, *, #28268, .F. ) ;
#42558 = CARTESIAN_POINT ( 'NONE',  ( -0.8759842519685039353, -0.1787899950787401882, 0.6815944881352126172 ) ) ;
#42559 = CARTESIAN_POINT ( 'NONE',  ( 0.06523048226347956391, 0.06348425196850393526, 0.1574803149606297803 ) ) ;
#42560 = EDGE_CURVE ( 'NONE', #18221, #34218, #45497, .T. ) ;
#42561 = EDGE_LOOP ( 'NONE', ( #46099, #29436, #26377, #36089 ) ) ;
#42562 = CARTESIAN_POINT ( 'NONE',  ( -0.9500414927467377701, -0.1787899950787401604, 1.712598425143087466 ) ) ;
#42563 = ADVANCED_FACE ( 'NONE', ( #8691 ), #36989, .F. ) ;
#42564 = CARTESIAN_POINT ( 'NONE',  ( 0.1377952755905510751, 0.000000000000000000, -0.3149606299212598381 ) ) ;
#42565 = CARTESIAN_POINT ( 'NONE',  ( 0.1574803149606299746, 0.3740157480314960647, 1.713085361781126803 ) ) ;
#42566 = VERTEX_POINT ( 'NONE', #15675 ) ;
#42567 = CARTESIAN_POINT ( 'NONE',  ( 0.8759842519685039353, 0.1574803149606299191, 0.5314960629921260393 ) ) ;
#42568 = CARTESIAN_POINT ( 'NONE',  ( -0.1797182628040039365, -0.6703194001342264174, 0.000000000000000000 ) ) ;
#42569 = CARTESIAN_POINT ( 'NONE',  ( -0.3551574803149606385, 9.222549191038288286E-34, 0.000000000000000000 ) ) ;
#42570 = CARTESIAN_POINT ( 'NONE',  ( -0.7185039370078739607, 1.928577636452523993E-17, 1.240157480207432883 ) ) ;
#42572 = CARTESIAN_POINT ( 'NONE',  ( -0.8107537697050254399, 0.1574803149606300301, 0.6815944880814486240 ) ) ;
#42571 = CARTESIAN_POINT ( 'NONE',  ( 0.1113553986120547346, -0.3572834645669291098, -0.1113553986120547346 ) ) ;
#42573 = CARTESIAN_POINT ( 'NONE',  ( 1.033464566929133799, 0.000000000000000000, 1.377952755797984263 ) ) ;
#42574 = VERTEX_POINT ( 'NONE', #19239 ) ;
#42575 = CARTESIAN_POINT ( 'NONE',  ( -0.1476377952755905387, -0.2142072668875215635, -1.269802121763611291 ) ) ;
#42576 = CARTESIAN_POINT ( 'NONE',  ( 0.9873396505805591694, 0.1113553986120547346, 1.274606299212598604 ) ) ;
#42577 = DIRECTION ( 'NONE',  ( 0.000000000000000000, 0.000000000000000000, 1.000000000000000000 ) ) ;
#42578 = CARTESIAN_POINT ( 'NONE',  ( 0.7185039370078739607, 1.928577636452523993E-17, 1.840551181102362266 ) ) ;
#42579 = CARTESIAN_POINT ( 'NONE',  ( 0.1113553986120547346, -0.5836614172153071767, -0.1113553986120547346 ) ) ;
#42580 = CARTESIAN_POINT ( 'NONE',  ( 0.3161444924769519216, 1.495705267341507883, -0.3569552279982051712 ) ) ;
#42581 = CARTESIAN_POINT ( 'NONE',  ( 0.07405724077823318263, -0.5246062991588343882, -0.1787899950787401604 ) ) ;
#42582 = DIRECTION ( 'NONE',  ( -1.000000000000000000, 0.000000000000000000, 0.000000000000000000 ) ) ;
#42583 = VERTEX_POINT ( 'NONE', #30310 ) ;
#42584 = CARTESIAN_POINT ( 'NONE',  ( -0.3161444924769509779, 1.798092712879851174, -3.826876940038414610 ) ) ;
#42585 = CARTESIAN_POINT ( 'NONE',  ( 1.054774247047244096, 0.000000000000000000, 0.7701771653005669016 ) ) ;
#42586 = ORIENTED_EDGE ( 'NONE', *, *, #38758, .F. ) ;
#42587 = CARTESIAN_POINT ( 'NONE',  ( -8.354793841626791791E-17, 0.03219022224904082713, -0.2854330708661417804 ) ) ;
#42588 = FACE_OUTER_BOUND ( 'NONE', #13050, .T. ) ;
#42589 = CARTESIAN_POINT ( 'NONE',  ( -0.1797182628040039087, 0.04080264710986784837, 0.07444174185955065859 ) ) ;
#42590 = CARTESIAN_POINT ( 'NONE',  ( -0.1787899950787401604, -1.031496062938363822, -0.07405724077823318263 ) ) ;
#42591 = CARTESIAN_POINT ( 'NONE',  ( -0.1574803149606300301, -1.329232283464566011, -0.06523048226347956391 ) ) ;
#42592 = CARTESIAN_POINT ( 'NONE',  ( 0.7185039370078746268, -0.06523048226347956391, 1.242618110128693276 ) ) ;
#42593 = ADVANCED_FACE ( 'NONE', ( #5091 ), #13480, .T. ) ;
#42594 = DIRECTION ( 'NONE',  ( 0.000000000000000000, 0.000000000000000000, 1.000000000000000000 ) ) ;
#42595 = CARTESIAN_POINT ( 'NONE',  ( -0.7495606340400177148, 0.1264236179284866091, 1.852854330654897685 ) ) ;
#42596 = ORIENTED_EDGE ( 'NONE', *, *, #34387, .T. ) ;
#42597 = CARTESIAN_POINT ( 'NONE',  ( -0.7185039370078739607, 1.928577636452523993E-17, 0.8070866140657008136 ) ) ;
#42598 = ORIENTED_EDGE ( 'NONE', *, *, #20710, .F. ) ;
#42599 = CARTESIAN_POINT ( 'NONE',  ( 0.1574803149606300301, -1.452263779420031709, -0.06523048226347956391 ) ) ;
#42600 = CARTESIAN_POINT ( 'NONE',  ( -0.9873396505805591694, 0.1113553986120547346, 0.4773622046168818911 ) ) ;
#42601 = CARTESIAN_POINT ( 'NONE',  ( -0.8019270111902717657, 0.1787899950787401604, 1.491141732229701367 ) ) ;
#42602 = CARTESIAN_POINT ( 'NONE',  ( 0.7185039370078739607, 1.928577636452523993E-17, 1.446850393700787274 ) ) ;
#42603 = CARTESIAN_POINT ( 'NONE',  ( -0.8019270111902717657, 0.1787899950787401604, 0.9793307086076531442 ) ) ;
#42604 = CARTESIAN_POINT ( 'NONE',  ( -0.6971942568897626646, 0.07405724077823318263, 0.2805118109698587214 ) ) ;
#42605 = ( BOUNDED_CURVE ( )  B_SPLINE_CURVE ( 2, ( #41969, #16383, #34836, #30539, #45102, #26937, #20187, #1023, #41255 ),
 .UNSPECIFIED., .F., .F. ) 
 B_SPLINE_CURVE_WITH_KNOTS ( ( 3, 2, 2, 2, 3 ),
 ( 0.8599999999999999867, 0.8625000000000000444, 0.8649999999999999911, 0.8675000000000000488, 0.8699999999999999956 ),
 .UNSPECIFIED. ) 
 CURVE ( )  GEOMETRIC_REPRESENTATION_ITEM ( )  RATIONAL_B_SPLINE_CURVE ( ( 1.000000000000000000, 0.9238795325112869605, 1.000000000000000000, 0.9238795325112869605, 1.000000000000000000, 0.9238795325112869605, 1.000000000000000000, 0.9238795325112829637, 1.000000000000000000 ) ) 
 REPRESENTATION_ITEM ( '' )  ) ;
#42606 = CARTESIAN_POINT ( 'NONE',  ( 0.2642359194686346169, -0.09842519685039370636, 1.205361022782828805E-17 ) ) ;
#42607 = CARTESIAN_POINT ( 'NONE',  ( -0.8019270111902717657, -0.1787899950787401604, 1.943897637741510254 ) ) ;
#42608 = LINE ( 'NONE', #31870, #14969 ) ;
#42609 = CARTESIAN_POINT ( 'NONE',  ( 0.2559055127798368634, 0.08170875243442862756, -0.05466978143083393860 ) ) ;
#42610 = CARTESIAN_POINT ( 'NONE',  ( 0.1787899950787401882, -0.2328995587804200962, -2.189545951927503898E-17 ) ) ;
#42611 = ADVANCED_FACE ( 'NONE', ( #6264 ), #8936, .T. ) ;
#42612 = CARTESIAN_POINT ( 'NONE',  ( 0.1762049892238537474, -0.09842519685039370636, -0.09843609369557973499 ) ) ;
#42613 = CYLINDRICAL_SURFACE ( 'NONE', #24912, 0.1574803149606299191 ) ;
#42614 = DIRECTION ( 'NONE',  ( 0.000000000000000000, 0.7880107536067203489, -0.6156614753256602901 ) ) ;
#42615 = AXIS2_PLACEMENT_3D ( 'NONE', #23073, #11501, #22036 ) ;
#42616 = EDGE_CURVE ( 'NONE', #8512, #36844, #34831, .T. ) ;
#42617 = ORIENTED_EDGE ( 'NONE', *, *, #2373, .T. ) ;
#42618 = CARTESIAN_POINT ( 'NONE',  ( -0.7495606340400177148, -0.1264236179284866091, 1.193405511757259951 ) ) ;
#42619 = VERTEX_POINT ( 'NONE', #23560 ) ;
#42620 = CARTESIAN_POINT ( 'NONE',  ( 0.1264236179284866091, -1.083169291284818980, -0.1264236179284866091 ) ) ;
#42621 = CARTESIAN_POINT ( 'NONE',  ( 0.1264236179284866091, -1.196358267662771757, -0.1264236179284866091 ) ) ;
#42622 = ADVANCED_FACE ( 'NONE', ( #39091 ), #1975, .T. ) ;
#42623 = CARTESIAN_POINT ( 'NONE',  ( -0.9412147342319837628, 0.1574803149606300301, 1.542814960522393308 ) ) ;
#42624 = ( LENGTH_UNIT ( ) NAMED_UNIT ( * ) SI_UNIT ( $, .METRE. ) ) ;
#42625 = CARTESIAN_POINT ( 'NONE',  ( 3.301370929368692659E-17, -0.5029965654885574233, 0.1797182628040039365 ) ) ;
#42626 = LINE ( 'NONE', #3342, #43853 ) ;
#42627 = CARTESIAN_POINT ( 'NONE',  ( -0.8759842519685039353, 0.1574803149606299191, 0.8366141731208189825 ) ) ;
#42628 = CARTESIAN_POINT ( 'NONE',  ( -0.7646288533564489232, -0.1113553986120547346, 0.7824803149606299746 ) ) ;
#42629 = CARTESIAN_POINT ( 'NONE',  ( -0.1113553986120547346, 0.05610236220472441387, 0.1113553986120547346 ) ) ;
#42630 = ORIENTED_EDGE ( 'NONE', *, *, #33421, .T. ) ;
#42631 = CARTESIAN_POINT ( 'NONE',  ( 0.9500414927467378812, 0.1787899950787401604, 0.8562992125446617919 ) ) ;
#42632 = CARTESIAN_POINT ( 'NONE',  ( 0.04756641494945747922, 0.3740157480314960647, 1.120507485783946766 ) ) ;
#42633 = CARTESIAN_POINT ( 'NONE',  ( 0.7185039370078746268, 0.06523048226347956391, 0.1747047243019218821 ) ) ;
#42634 = CARTESIAN_POINT ( 'NONE',  ( -1.033464566929133799, 0.000000000000000000, 0.7874015746956221085 ) ) ;
#42635 = CARTESIAN_POINT ( 'NONE',  ( -0.7185039370078739607, 1.928577636452523993E-17, 1.437007873908220601 ) ) ;
#42636 = CARTESIAN_POINT ( 'NONE',  ( -0.07405724077823318263, -0.6673228345919050009, 0.1787899950787401604 ) ) ;
#42638 = VECTOR ( 'NONE', #11858, 39.37007874015748143 ) ;
#42637 = CARTESIAN_POINT ( 'NONE',  ( -0.1787899950787401604, -1.336614173174582865, 0.07405724077823318263 ) ) ;
#42639 = CARTESIAN_POINT ( 'NONE',  ( 0.8019270111902717657, -0.1787899950787401604, 0.3690944881352128393 ) ) ;
#42640 = CARTESIAN_POINT ( 'NONE',  ( -0.8019270111902717657, -0.1787899950787401604, 1.978346456639149320 ) ) ;
#42641 = ORIENTED_EDGE ( 'NONE', *, *, #28580, .F. ) ;
#42642 = VERTEX_POINT ( 'NONE', #35056 ) ;
#42643 = CARTESIAN_POINT ( 'NONE',  ( -0.8019270111902717657, -0.1787899950787401604, 1.510826771599780294 ) ) ;
#42644 = CARTESIAN_POINT ( 'NONE',  ( 0.8019270111902717657, -0.1787899950787401604, 1.589566929080094448 ) ) ;
#42645 = PLANE ( 'NONE',  #10671 ) ;
#42646 = CARTESIAN_POINT ( 'NONE',  ( -0.9500414927467378812, -0.1787899950787401604, 0.6496062991588353874 ) ) ;
#42647 = ADVANCED_FACE ( 'NONE', ( #2206 ), #13257, .F. ) ;
#42648 = CARTESIAN_POINT ( 'NONE',  ( 0.1306058198804243842, -0.09842711666118027225, -0.1221223300366590520 ) ) ;
#42649 = CARTESIAN_POINT ( 'NONE',  ( 0.7495606340400177148, 0.1264236179284866091, 0.5536417322297008115 ) ) ;
#42650 = CARTESIAN_POINT ( 'NONE',  ( -1.002407869896990045, 0.1264236179284866091, 0.5782480314422993040 ) ) ;
#42651 = CARTESIAN_POINT ( 'NONE',  ( 0.1916485431825860897, -0.07731288306172690028, 0.1747847109491888207 ) ) ;
#42652 = DIRECTION ( 'NONE',  ( 1.000000000000000000, 6.679788269418529283E-17, 0.000000000000000000 ) ) ;
#42653 = ORIENTED_EDGE ( 'NONE', *, *, #31516, .T. ) ;
#42654 = CARTESIAN_POINT ( 'NONE',  ( -0.8019270111902717657, 0.1787899950787401604, 1.377952755851748146 ) ) ;
#42655 = CARTESIAN_POINT ( 'NONE',  ( -0.8759842519685039353, 0.000000000000000000, 0.000000000000000000 ) ) ;
#42656 = CARTESIAN_POINT ( 'NONE',  ( -0.7646288533564489232, 0.1113553986120547346, 0.3789370078740157410 ) ) ;
#42657 = EDGE_CURVE ( 'NONE', #24301, #19795, #22752, .T. ) ;
#42658 = CARTESIAN_POINT ( 'NONE',  ( 0.1954853181098232251, -0.09851384548657264595, 0.08125050196056771146 ) ) ;
#42659 = EDGE_LOOP ( 'NONE', ( #4219, #42770, #24025, #36448 ) ) ;
#42660 = AXIS2_PLACEMENT_3D ( 'NONE', #4871, #37002, #40803 ) ;
#42661 = CARTESIAN_POINT ( 'NONE',  ( -0.1787899950787401604, -1.549336566654435865, 0.07405724077823318263 ) ) ;
#42662 = ORIENTED_EDGE ( 'NONE', *, *, #17696, .T. ) ;
#42663 = CARTESIAN_POINT ( 'NONE',  ( 0.07405724077823318263, -0.5393700786863945273, 0.1787899950787401604 ) ) ;
#42664 = CARTESIAN_POINT ( 'NONE',  ( 0.9412147342319837628, 0.1574803149606300301, 0.8046259842519695171 ) ) ;
#42665 = ( NAMED_UNIT ( * ) PLANE_ANGLE_UNIT ( ) SI_UNIT ( $, .RADIAN. ) ) ;
#42666 = ORIENTED_EDGE ( 'NONE', *, *, #34815, .T. ) ;
#42667 = CARTESIAN_POINT ( 'NONE',  ( 1.002407869896990045, -0.1264236179284866091, 1.395177165300567124 ) ) ;
#42668 = DIRECTION ( 'NONE',  ( -1.000000000000000000, 0.000000000000000000, 0.000000000000000000 ) ) ;
#42669 = AXIS2_PLACEMENT_3D ( 'NONE', #30001, #44786, #37616 ) ;
#42670 = CARTESIAN_POINT ( 'NONE',  ( -0.1264236179284866091, -0.3154527558517483676, 0.1264236179284866091 ) ) ;
#42671 = CARTESIAN_POINT ( 'NONE',  ( 3.284318927891251994E-17, -0.7386811023084409733, 0.1787899950787401882 ) ) ;
#42672 = CARTESIAN_POINT ( 'NONE',  ( 0.7185039370078739607, 1.928577636452523993E-17, 0.1771653542231816925 ) ) ;
#42673 = DIRECTION ( 'NONE',  ( -1.000000000000000000, 0.000000000000000000, 0.000000000000000000 ) ) ;
#42674 = CARTESIAN_POINT ( 'NONE',  ( 0.8759842519685039353, -0.1787899950787401882, 1.665846456639149764 ) ) ;
#42675 = CARTESIAN_POINT ( 'NONE',  ( 0.1787899950787401604, 0.005781543581784898134, -0.07405724077823318263 ) ) ;
#42676 = CARTESIAN_POINT ( 'NONE',  ( 0.1787899950787401604, 0.01673228351833045899, -0.07405724077823318263 ) ) ;
#42677 = ITEM_DEFINED_TRANSFORMATION ( 'NONE', 'NONE', #228,  #20860 ) ;
#42678 = CYLINDRICAL_SURFACE ( 'NONE', #41733, 0.1574803149606299191 ) ;
#42679 = CARTESIAN_POINT ( 'NONE',  ( -0.6971942568897648851, 0.07405724077823318263, 0.7923228345919055560 ) ) ;
#42681 = CARTESIAN_POINT ( 'NONE',  ( 1.614954907737318939E-16, 0.1564960629921311464, 0.4940944881889759444 ) ) ;
#42680 = CARTESIAN_POINT ( 'NONE',  ( 0.1574803149606300301, -0.8764763779527571241, 0.06523048226347956391 ) ) ;
#42682 = CARTESIAN_POINT ( 'NONE',  ( 0.1797182628040039087, -1.716087116669659629, 0.07444174185955046430 ) ) ;
#42683 = CARTESIAN_POINT ( 'NONE',  ( 0.6971942568897637749, 2.189545951927499583E-17, 1.464074803095842370 ) ) ;
#42685 = DIRECTION ( 'NONE',  ( -0.000000000000000000, -0.2126700594527834443, 0.9771240687918547607 ) ) ;
#42684 = CARTESIAN_POINT ( 'NONE',  ( 0.1898978525284559515, 0.07836113345104910033, -0.1757954945903058008 ) ) ;
#42686 = CARTESIAN_POINT ( 'NONE',  ( 1.002407869896990045, 0.1264236179284866091, 0.3813976377415121966 ) ) ;
#42687 = DIRECTION ( 'NONE',  ( 0.000000000000000000, 0.000000000000000000, 1.000000000000000000 ) ) ;
#42688 = DIRECTION ( 'NONE',  ( 5.392424630175478286E-15, -0.2432573283306889156, 0.9699617890481125881 ) ) ;
#42690 = CARTESIAN_POINT ( 'NONE',  ( -0.1787899950787401882, -0.1628937007336379861, 0.000000000000000000 ) ) ;
#42689 = CARTESIAN_POINT ( 'NONE',  ( 2.892866454678787531E-17, -0.9133858266641260437, 0.1574803149606299191 ) ) ;
#42691 = CARTESIAN_POINT ( 'NONE',  ( 1.054774247047244096, 0.000000000000000000, 0.5733267715997795166 ) ) ;
#42692 = CARTESIAN_POINT ( 'NONE',  ( 0.1787899950787401604, -0.9625984251430860228, -0.07405724077823318263 ) ) ;
#42693 = CARTESIAN_POINT ( 'NONE',  ( 0.7870214370185560915, -0.1374925161510997529, 0.03936976900452263811 ) ) ;
#42694 = DIRECTION ( 'NONE',  ( -0.5735764363510518216, 0.8191520442889876907, 1.003171929053519693E-16 ) ) ;
#42695 = CIRCLE ( 'NONE', #38895, 0.1574803149606299191 ) ;
#42696 = CARTESIAN_POINT ( 'NONE',  ( -0.9500414927467378812, -0.1787899950787401604, 1.471456692859622217 ) ) ;
#42697 = ORIENTED_EDGE ( 'NONE', *, *, #35660, .T. ) ;
#42698 = CARTESIAN_POINT ( 'NONE',  ( 0.7185039370078746268, -0.06523048226347956391, 0.4256889763779528879 ) ) ;
#42699 = CARTESIAN_POINT ( 'NONE',  ( 0.9500414927467378812, -0.1787899950787401604, 1.043307086560409269 ) ) ;
#42700 = CARTESIAN_POINT ( 'NONE',  ( -0.8759842519685039353, -0.1574803149606299191, 0.6594488187901103027 ) ) ;
#42701 = DIRECTION ( 'NONE',  ( 0.000000000000000000, -1.000000000000000000, 0.000000000000000000 ) ) ;
#42702 = CARTESIAN_POINT ( 'NONE',  ( 1.054774247047244540, -0.07405724077823318263, 1.830708661363559253 ) ) ;
#42703 = CARTESIAN_POINT ( 'NONE',  ( -0.8107537697050253289, -0.1574803149606297803, 1.454232283464566677 ) ) ;
#42704 = CARTESIAN_POINT ( 'NONE',  ( -0.8759842519685039353, -0.1787899950787401882, 0.9178149605761574126 ) ) ;
#42705 = EDGE_CURVE ( 'NONE', #6499, #21404, #20890, .T. ) ;
#42706 = CARTESIAN_POINT ( 'NONE',  ( 0.9873396505805591694, -0.1113553986120547346, 1.806102362097196767 ) ) ;
#42707 = CARTESIAN_POINT ( 'NONE',  ( -0.7716059914281355736, -0.1284597044140924071, 0.03937007874015843040 ) ) ;
#42708 = CARTESIAN_POINT ( 'NONE',  ( 0.6971942568897626646, -0.07405724077823297447, 0.08858267711159095725 ) ) ;
#42709 = CARTESIAN_POINT ( 'NONE',  ( -0.6971942568897626646, -0.07405724077823297447, 0.1230314960092287191 ) ) ;
#42710 = UNCERTAINTY_MEASURE_WITH_UNIT (LENGTH_MEASURE( 1.000000000000000082E-05 ), #26645, 'distance_accuracy_value', 'NONE') ;
#42711 = CARTESIAN_POINT ( 'NONE',  ( 1.033464566929134687, 0.06523048226347956391, 1.537893700679874298 ) ) ;
#42712 = ORIENTED_EDGE ( 'NONE', *, *, #4811, .T. ) ;
#42713 = AXIS2_PLACEMENT_3D ( 'NONE', #22291, #40955, #22062 ) ;
#42714 = EDGE_CURVE ( 'NONE', #3332, #32743, #18415, .T. ) ;
#42715 = CARTESIAN_POINT ( 'NONE',  ( -0.1264236179284866091, 0.1176181102899840625, 0.1264236179284866091 ) ) ;
#42716 = ADVANCED_FACE ( 'NONE', ( #24270 ), #400, .F. ) ;
#42717 = CARTESIAN_POINT ( 'NONE',  ( -0.8019270111902716547, 0.1787899950787401604, 1.648622047190331230 ) ) ;
#42718 = ADVANCED_FACE ( 'NONE', ( #5573 ), #45566, .T. ) ;
#42719 = CARTESIAN_POINT ( 'NONE',  ( 0.3906197235759846786, 4.466152701071653354E-17, 0.000000000000000000 ) ) ;
#42720 = CYLINDRICAL_SURFACE ( 'NONE', #12204, 0.1574803149606299191 ) ;
#42721 = CARTESIAN_POINT ( 'NONE',  ( -0.07405724077823318263, -1.086738141457586515, -0.1787899950787401604 ) ) ;
#42722 = ORIENTED_EDGE ( 'NONE', *, *, #24896, .T. ) ;
#42723 = CARTESIAN_POINT ( 'NONE',  ( 0.1787899950787401882, -0.05954724404072461036, -2.189545951927503898E-17 ) ) ;
#42724 = CARTESIAN_POINT ( 'NONE',  ( 0.7495606340400177148, -0.1264236179284866091, 1.070374015694267600 ) ) ;
#42725 = B_SPLINE_CURVE_WITH_KNOTS ( 'NONE', 3,
 ( #17003, #21528, #38809, #31872, #13192, #45983, #39720, #27828, #31642, #2829, #13418, #24665, #42388, #21289, #39497, #28050, #17701, #28273, #14119, #42609, #46451, #10292, #6437, #28516 ),
 .UNSPECIFIED., .F., .F.,
 ( 4, 2, 2, 1, 1, 2, 2, 2, 1, 1, 1, 1, 2, 2, 4 ),
 ( 0.000000000000000000, 0.1249999999999968081, 0.1874999999999952260, 0.2187499999999943934, 0.2343749999999939493, 0.2421874999999936995, 0.2499999999999934497, 0.3749999999999907296, 0.4374999999999895084, 0.4687499999999888423, 0.4843749999999885647, 0.4921874999999884537, 0.4960937499999885092, 0.4999999999999885647, 1.000000000000000000 ),
 .UNSPECIFIED. ) ;
#42726 = CARTESIAN_POINT ( 'NONE',  ( -0.1476377952755905387, 0.5323553679591567223, -0.7566348232351032266 ) ) ;
#42727 = LINE ( 'NONE', #20246, #834 ) ;
#42728 = AXIS2_PLACEMENT_3D ( 'NONE', #22918, #44934, #19320 ) ;
#42729 = CARTESIAN_POINT ( 'NONE',  ( 0.8759842519685039353, 0.1574803149606299191, 1.791338582677165281 ) ) ;
#42730 = CARTESIAN_POINT ( 'NONE',  ( 0.1797182628040039365, -0.1781934158822582603, -2.200913952912460540E-17 ) ) ;
#42731 = VECTOR ( 'NONE', #33999, 39.37007874015748854 ) ;
#42732 = CARTESIAN_POINT ( 'NONE',  ( -0.6971942568897626646, -0.07405724077823297447, 0.2854330708123783977 ) ) ;
#42733 = CARTESIAN_POINT ( 'NONE',  ( 0.1797182628040039087, -1.278094990685408439, -0.07444174185955065859 ) ) ;
#42734 = CARTESIAN_POINT ( 'NONE',  ( -0.05824109077986367594, 0.2618687228227554176, -0.05388431474956185269 ) ) ;
#42735 = CARTESIAN_POINT ( 'NONE',  ( 0.9500414927467378812, -0.1787899950787401604, 1.082677165300567346 ) ) ;
#42736 = CARTESIAN_POINT ( 'NONE',  ( 0.8019270111902716547, -0.1787899950787401604, 1.584645669237574994 ) ) ;
#42737 = CARTESIAN_POINT ( 'NONE',  ( 0.8759842519685039353, -0.1787899950787401882, 0.2091535432533232486 ) ) ;
#42738 = CARTESIAN_POINT ( 'NONE',  ( 0.8759842519685039353, -0.1574803149606299191, 1.692913385826771533 ) ) ;
#42740 = CARTESIAN_POINT ( 'NONE',  ( -1.033464566929134687, -0.06523048226347956391, 1.109744094488189115 ) ) ;
#42739 = DIRECTION ( 'NONE',  ( 0.000000000000000000, 0.000000000000000000, -1.000000000000000000 ) ) ;
#42741 = CARTESIAN_POINT ( 'NONE',  ( 0.8759842519685039353, 0.1574803149606299191, 0.6791338581601890079 ) ) ;
#42742 = CARTESIAN_POINT ( 'NONE',  ( 0.1574803149606300301, -0.7829724408373558431, -0.06523048226347956391 ) ) ;
#42743 = CARTESIAN_POINT ( 'NONE',  ( -0.8759842519685039353, -0.1574803149606299191, 1.683070866034204638 ) ) ;
#42744 = CARTESIAN_POINT ( 'NONE',  ( 1.054774247047244540, 0.07405724077823318263, 0.2214566928596220785 ) ) ;
#42745 = CARTESIAN_POINT ( 'NONE',  ( -0.7185039370078739607, 1.928577636452523993E-17, 1.564960629921259949 ) ) ;
#42746 = CARTESIAN_POINT ( 'NONE',  ( 1.002407869896990045, 0.1264236179284866091, 1.090059055064346527 ) ) ;
#42747 = CARTESIAN_POINT ( 'NONE',  ( 0.7495606340400177148, 0.1264236179284866091, 1.931594488135212728 ) ) ;
#42748 = CARTESIAN_POINT ( 'NONE',  ( 0.9873396505805591694, 0.1113553986120547346, 0.5561023620971968784 ) ) ;
#42749 = ORIENTED_EDGE ( 'NONE', *, *, #38210, .T. ) ;
#42750 = LINE ( 'NONE', #46841, #46753 ) ;
#42751 = CARTESIAN_POINT ( 'NONE',  ( -0.9873396505805591694, -0.1113553986120547346, 0.3494094487113705294 ) ) ;
#42752 = ORIENTED_EDGE ( 'NONE', *, *, #37764, .F. ) ;
#42753 = CARTESIAN_POINT ( 'NONE',  ( 0.7495606340400177148, -0.1264236179284866091, 1.306594488135212728 ) ) ;
#42754 = CARTESIAN_POINT ( 'NONE',  ( -0.8759842519685039353, -0.1574803149606299191, 1.771653543307086576 ) ) ;
#42755 = CARTESIAN_POINT ( 'NONE',  ( -0.1787899950787401604, 0.04133858273092887170, 0.07405724077823318263 ) ) ;
#42756 = CARTESIAN_POINT ( 'NONE',  ( 0.1574803149606300023, 0.000000000000000000, -0.2952755905511806334 ) ) ;
#42757 = ( BOUNDED_CURVE ( )  B_SPLINE_CURVE ( 2, ( #6030, #13703, #42910, #20653, #6265, #13945, #6985, #2437, #17772 ),
 .UNSPECIFIED., .F., .T. ) 
 B_SPLINE_CURVE_WITH_KNOTS ( ( 3, 2, 2, 2, 3 ),
 ( 0.4699999999999999734, 0.4724999999999999756, 0.4749999999999999778, 0.4774999999999999800, 0.4799999999999999822 ),
 .UNSPECIFIED. ) 
 CURVE ( )  GEOMETRIC_REPRESENTATION_ITEM ( )  RATIONAL_B_SPLINE_CURVE ( ( 1.000000000000000000, 0.9238795325112879597, 1.000000000000000000, 0.9238795325112869605, 1.000000000000000000, 0.9238795325112869605, 1.000000000000000000, 0.9238795325112869605, 1.000000000000000000 ) ) 
 REPRESENTATION_ITEM ( '' )  ) ;
#42758 = ADVANCED_FACE ( 'NONE', ( #45809 ), #14968, .F. ) ;
#42759 = AXIS2_PLACEMENT_3D ( 'NONE', #16399, #26716, #8471 ) ;
#42760 = VERTEX_POINT ( 'NONE', #27885 ) ;
#42761 = CARTESIAN_POINT ( 'NONE',  ( 0.1627568843983490665, 0.09133345722617872142, 0.1914653398462901890 ) ) ;
#42762 = CARTESIAN_POINT ( 'NONE',  ( 0.3690944881889784424, 0.1864803149606333310, -0.7480314960629921295 ) ) ;
#42763 = ( BOUNDED_CURVE ( )  B_SPLINE_CURVE ( 2, ( #38018, #19798, #30620, #45897, #8779, #13112, #41816, #45184, #41106 ),
 .UNSPECIFIED., .F., .F. ) 
 B_SPLINE_CURVE_WITH_KNOTS ( ( 3, 2, 2, 2, 3 ),
 ( 0.9499999999999999556, 0.9525000000000000133, 0.9549999999999999600, 0.9575000000000000178, 0.9599999999999999645 ),
 .UNSPECIFIED. ) 
 CURVE ( )  GEOMETRIC_REPRESENTATION_ITEM ( )  RATIONAL_B_SPLINE_CURVE ( ( 1.000000000000000000, 0.9238795325112899581, 1.000000000000000000, 0.9238795325112869605, 1.000000000000000000, 0.9238795325112869605, 1.000000000000000000, 0.9238795325112869605, 1.000000000000000000 ) ) 
 REPRESENTATION_ITEM ( '' )  ) ;
#42764 = VERTEX_POINT ( 'NONE', #42446 ) ;
#42765 = CARTESIAN_POINT ( 'NONE',  ( -0.6971942568897648851, 0.07405724077823318263, 1.417322834591906444 ) ) ;
#42767 = CARTESIAN_POINT ( 'NONE',  ( 3.284318927891251994E-17, -1.767224409395055318, 0.1787899950787401882 ) ) ;
#42766 = CARTESIAN_POINT ( 'NONE',  ( -0.1574803149606300301, -0.4138779526483781224, -0.06523048226347956391 ) ) ;
#42768 = CARTESIAN_POINT ( 'NONE',  ( -0.8759842519685039353, -0.1787899950787401882, 1.001476377898992132 ) ) ;
#42769 = CARTESIAN_POINT ( 'NONE',  ( -1.054774247047244540, 0.07405724077823318263, 1.953740157426552715 ) ) ;
#42770 = ORIENTED_EDGE ( 'NONE', *, *, #24035, .F. ) ;
#42771 = CARTESIAN_POINT ( 'NONE',  ( -1.054774247047244540, 0.07405724077823318263, 1.126968503883244654 ) ) ;
#42772 = EDGE_CURVE ( 'NONE', #30178, #6678, #26091, .T. ) ;
#42773 = CARTESIAN_POINT ( 'NONE',  ( -0.8019270111902717657, -0.1787899950787401604, 0.7234251967966300878 ) ) ;
#42774 = CARTESIAN_POINT ( 'NONE',  ( 0.005709509457931655034, 0.05322596569711288833, -0.1377927287266135781 ) ) ;
#42775 = CARTESIAN_POINT ( 'NONE',  ( 0.1787899950787401604, -0.7078011335835699969, 0.07405724077823318263 ) ) ;
#42776 = ORIENTED_EDGE ( 'NONE', *, *, #27597, .F. ) ;
#42777 = CARTESIAN_POINT ( 'NONE',  ( -0.8070866141732283561, -0.0009842519685049383633, -0.8559055118110230342 ) ) ;
#42778 = AXIS2_PLACEMENT_3D ( 'NONE', #38731, #1580, #27270 ) ;
#42779 = CARTESIAN_POINT ( 'NONE',  ( -0.07117121207836790697, -0.08956324299011318713, 0.1404802767937309016 ) ) ;
#42780 = ORIENTED_EDGE ( 'NONE', *, *, #5999, .F. ) ;
#42781 = CARTESIAN_POINT ( 'NONE',  ( 0.7185039370078746268, 0.06523048226347956391, 0.7750984251968497940 ) ) ;
#42782 = CARTESIAN_POINT ( 'NONE',  ( -0.9500414927467378812, 0.1787899950787401604, 0.6200787401037165525 ) ) ;
#42783 = CARTESIAN_POINT ( 'NONE',  ( 0.000000000000000000, 0.5360961046428496246, -0.7563373642699310340 ) ) ;
#42784 = ORIENTED_EDGE ( 'NONE', *, *, #24727, .T. ) ;
#42785 = CARTESIAN_POINT ( 'NONE',  ( -0.7495606340400177148, 0.1264236179284866091, 1.616633858213952779 ) ) ;
#42786 = PLANE ( 'NONE',  #427 ) ;
#42787 = AXIS2_PLACEMENT_3D ( 'NONE', #11506, #45252, #12472 ) ;
#42788 = CARTESIAN_POINT ( 'NONE',  ( -0.7646288533564489232, 0.1113553986120547346, 0.1328740156405045225 ) ) ;
#42789 = CARTESIAN_POINT ( 'NONE',  ( 0.8107537697050254399, 0.1574803149606300301, 0.6520669291338587747 ) ) ;
#42790 = CARTESIAN_POINT ( 'NONE',  ( 0.7646288533564489232, 0.1113553986120547346, 0.5364173228346457156 ) ) ;
#42791 = DIRECTION ( 'NONE',  ( 1.000000000000000000, 0.000000000000000000, 0.000000000000000000 ) ) ;
#42792 = CARTESIAN_POINT ( 'NONE',  ( -0.9412147342319837628, -0.1574803149606297803, 1.331200787294047672 ) ) ;
#42793 = CARTESIAN_POINT ( 'NONE',  ( 0.8759842519685039353, 0.1787899950787401882, 0.6668307086076534773 ) ) ;
#42794 = CARTESIAN_POINT ( 'NONE',  ( -0.1574803149606300301, -0.6599409448818898127, -0.06523048226347956391 ) ) ;
#42795 = CARTESIAN_POINT ( 'NONE',  ( -0.1639265925754282704, 0.1264995129648254779, 0.007850818260147569144 ) ) ;
#42796 = ORIENTED_EDGE ( 'NONE', *, *, #1017, .T. ) ;
#42797 = CARTESIAN_POINT ( 'NONE',  ( -0.2559055118110235560, 0.04218462477718680492, -0.03480397727850406686 ) ) ;
#42798 = CARTESIAN_POINT ( 'NONE',  ( 1.033464566929133799, 0.000000000000000000, 1.190944881889763884 ) ) ;
#42800 = CARTESIAN_POINT ( 'NONE',  ( -1.033464566929134687, -0.06523048226347956391, 1.345964566929133133 ) ) ;
#42799 = DIRECTION ( 'NONE',  ( -1.000000000000000000, 0.000000000000000000, 0.000000000000000000 ) ) ;
#42801 = CIRCLE ( 'NONE', #6843, 0.09842519685039370636 ) ;
#42802 = CARTESIAN_POINT ( 'NONE',  ( 0.7185039370078739607, 1.928577636452523993E-17, 0.4625984251968504046 ) ) ;
#42804 = CARTESIAN_POINT ( 'NONE',  ( -1.054774247047244540, -0.07405724077823318263, 1.988188976324187562 ) ) ;
#42803 = CARTESIAN_POINT ( 'NONE',  ( 0.6971942568897648851, 0.07405724077823318263, 0.7086614172690703928 ) ) ;
#42805 = CARTESIAN_POINT ( 'NONE',  ( -0.8107537697050254399, 0.1574803149606300301, 0.6914370078740148529 ) ) ;
#42806 = CARTESIAN_POINT ( 'NONE',  ( -0.1636338509590271328, -0.08956016023378124413, -0.05621478700804145856 ) ) ;
#42807 = CARTESIAN_POINT ( 'NONE',  ( -0.1787899950787401604, -0.6328740156942683770, -0.07405724077823318263 ) ) ;
#42808 = CARTESIAN_POINT ( 'NONE',  ( 0.000000000000000000, 0.6241017553149685870, 0.3240160679609070948 ) ) ;
#42809 = ORIENTED_EDGE ( 'NONE', *, *, #18969, .F. ) ;
#42810 = VECTOR ( 'NONE', #44904, 39.37007874015748854 ) ;
#42811 = CARTESIAN_POINT ( 'NONE',  ( 0.1577476715125368523, 0.03207557811201351694, -0.1404216743935784162 ) ) ;
#42812 = CARTESIAN_POINT ( 'NONE',  ( 0.7495606340400177148, -0.1264236179284866091, 0.8341535432533228045 ) ) ;
#42813 = CARTESIAN_POINT ( 'NONE',  ( 1.033464566929133799, 0.000000000000000000, 1.309055118110236338 ) ) ;
#42814 = CARTESIAN_POINT ( 'NONE',  ( 0.8759842519685039353, 0.000000000000000000, 4.498031496062992574 ) ) ;
#42815 = CARTESIAN_POINT ( 'NONE',  ( 0.1797182628040039087, 0.06048768647994660214, -0.07444174185955065859 ) ) ;
#42816 = CARTESIAN_POINT ( 'NONE',  ( -1.094772975963752103E-17, -1.117618110182456714, -0.1787899950787401882 ) ) ;
#42817 = CARTESIAN_POINT ( 'NONE',  ( -0.06523048226347956391, -1.555610236220473785, 0.1574803149606297803 ) ) ;
#42818 = DIRECTION ( 'NONE',  ( 1.000000000000000000, 0.000000000000000000, 0.000000000000000000 ) ) ;
#42819 = EDGE_CURVE ( 'NONE', #26576, #33815, #13454, .T. ) ;
#42820 = ORIENTED_EDGE ( 'NONE', *, *, #38948, .T. ) ;
#42821 = CARTESIAN_POINT ( 'NONE',  ( -0.7495606340400177148, -0.1264236179284866091, 1.902066929080094448 ) ) ;
#42822 = CARTESIAN_POINT ( 'NONE',  ( 0.8019270111902717657, 0.1787899950787401604, 1.968503936954110189 ) ) ;
#42823 = EDGE_LOOP ( 'NONE', ( #16233, #26997, #30834, #15167 ) ) ;
#42824 = CARTESIAN_POINT ( 'NONE',  ( -0.06523048226347956391, -1.442421259734993244, -0.1574803149606300301 ) ) ;
#42825 = CARTESIAN_POINT ( 'NONE',  ( -0.7495606340400177148, -0.1264236179284866091, 1.902066929080094448 ) ) ;
#42826 = CARTESIAN_POINT ( 'NONE',  ( -1.002407869896990045, 0.1264236179284866091, 1.483759842465921075 ) ) ;
#42827 = CARTESIAN_POINT ( 'NONE',  ( 0.000000000000000000, 0.000000000000000000, 0.000000000000000000 ) ) ;
#42828 = ADVANCED_FACE ( 'NONE', ( #36472 ), #28836, .T. ) ;
#42829 = CARTESIAN_POINT ( 'NONE',  ( -0.9500414927467378812, -0.1787899950787401604, 0.9596456692375764375 ) ) ;
#42830 = CARTESIAN_POINT ( 'NONE',  ( -1.054774247047244540, 0.07405724077823318263, 0.1870078739619845387 ) ) ;
#42831 = VECTOR ( 'NONE', #10457, 39.37007874015748143 ) ;
#42832 = CARTESIAN_POINT ( 'NONE',  ( -0.2471922904502827090, 0.09275221067063772751, 0.04038095640780218348 ) ) ;
#42833 = CARTESIAN_POINT ( 'NONE',  ( -0.6971942568897637749, 2.189545951927499583E-17, 1.857775590497417362 ) ) ;
#42834 = CARTESIAN_POINT ( 'NONE',  ( -0.9500414927467378812, -0.1787899950787401604, 0.1377952755367876370 ) ) ;
#42835 = CARTESIAN_POINT ( 'NONE',  ( 0.07968303789223217526, -0.08956740676322874628, -0.2394271090157727711 ) ) ;
#42836 = CARTESIAN_POINT ( 'NONE',  ( -0.8759842519685039353, 0.1574803149606299191, 1.948818897637795367 ) ) ;
#42837 = CARTESIAN_POINT ( 'NONE',  ( 0.1574803149606299191, 0.000000000000000000, 0.000000000000000000 ) ) ;
#42838 = CARTESIAN_POINT ( 'NONE',  ( 0.1787899950787401604, -0.3141003461819947828, 0.07405724077823318263 ) ) ;
#42839 = CARTESIAN_POINT ( 'NONE',  ( -0.9873396505805591694, -0.1113553986120547346, 1.500984251968503935 ) ) ;
#42840 = CARTESIAN_POINT ( 'NONE',  ( 0.3690944881889784424, 0.1864803149606327759, 0.7480314960629921295 ) ) ;
#42841 = VECTOR ( 'NONE', #45740, 39.37007874015748854 ) ;
#42842 = CARTESIAN_POINT ( 'NONE',  ( -0.8019270111902717657, -0.1787899950787401604, 0.1673228345919057225 ) ) ;
#42843 = ORIENTED_EDGE ( 'NONE', *, *, #1082, .F. ) ;
#42844 = CARTESIAN_POINT ( 'NONE',  ( -0.8759842519685039353, -0.1787899950787401882, 1.198326771599779628 ) ) ;
#42845 = ORIENTED_EDGE ( 'NONE', *, *, #21093, .T. ) ;
#42846 = APPLICATION_CONTEXT ( 'automotive_design' ) ;
#42847 = CARTESIAN_POINT ( 'NONE',  ( -0.1787899950787401604, -1.105314960576158301, 0.07405724077823318263 ) ) ;
#42848 = B_SPLINE_CURVE_WITH_KNOTS ( 'NONE', 3,
 ( #28691, #36084, #3243, #17871, #32514, #47098, #28933, #43496, #10704, #25310, #44430, #9149, #22406, #37031, #27157, #11402, #40596, #16356, #26268, #15009, #22161 ),
 .UNSPECIFIED., .F., .F.,
 ( 4, 2, 1, 1, 2, 2, 2, 1, 1, 1, 2, 2, 4 ),
 ( 0.000000000000000000, 0.1249999999999968359, 0.1874999999999953648, 0.2187499999999947264, 0.2343749999999944766, 0.2499999999999942268, 0.3749999999999941713, 0.4374999999999943379, 0.4687499999999944489, 0.4843749999999945044, 0.4921874999999945599, 0.4999999999999945599, 1.000000000000000000 ),
 .UNSPECIFIED. ) ;
#42849 = CARTESIAN_POINT ( 'NONE',  ( -0.1787899950787401882, -1.299704724355684959, 0.000000000000000000 ) ) ;
#42850 = CARTESIAN_POINT ( 'NONE',  ( -0.1476377952755905387, 0.06415291647593697466, -0.1630605872086743346 ) ) ;
#42851 = SHAPE_REPRESENTATION_RELATIONSHIP ( 'NONE' , 'NONE' ,  #7769, #27304 ) ;
#42852 = CARTESIAN_POINT ( 'NONE',  ( -0.8759842519685039353, 0.1574803149606299191, 0.9547244093412913246 ) ) ;
#42853 = CARTESIAN_POINT ( 'NONE',  ( -0.7185039370078746268, -0.06523048226347956391, 0.6619094488188971281 ) ) ;
#42854 = CARTESIAN_POINT ( 'NONE',  ( 2.892866454678787531E-17, -0.1751968503937007815, 0.1574803149606299191 ) ) ;
#42855 = CARTESIAN_POINT ( 'NONE',  ( 0.7185039370078746268, 0.06523048226347956391, 1.867618110128693720 ) ) ;
#42856 = CARTESIAN_POINT ( 'NONE',  ( 0.7185039370078746268, -0.06523048226347956391, 0.7406496062992133922 ) ) ;
#42857 = CARTESIAN_POINT ( 'NONE',  ( -0.1113553986120547346, -0.06200787401574803237, 0.1113553986120547346 ) ) ;
#42858 = AXIS2_PLACEMENT_3D ( 'NONE', #35618, #43734, #6832 ) ;
#42860 = CARTESIAN_POINT ( 'NONE',  ( 1.033464566929133799, 1.928577636452524610E-17, 4.498031496062992574 ) ) ;
#42859 = CARTESIAN_POINT ( 'NONE',  ( 0.9873396505805591694, 0.1113553986120547346, 0.6053149606299212948 ) ) ;
#42861 = CARTESIAN_POINT ( 'NONE',  ( 0.9412147342319837628, 0.1574803149606300301, 0.2042322833570398011 ) ) ;
#42862 = ORIENTED_EDGE ( 'NONE', *, *, #38469, .T. ) ;
#42863 = ORIENTED_EDGE ( 'NONE', *, *, #8070, .F. ) ;
#42864 = DIRECTION ( 'NONE',  ( -1.000000000000000000, 3.469446951953614189E-15, 0.000000000000000000 ) ) ;
#42865 = CARTESIAN_POINT ( 'NONE',  ( 0.7185039370078739607, 1.928577636452523993E-17, 0.7283464565853858819 ) ) ;
#42866 = CARTESIAN_POINT ( 'NONE',  ( 3.284318927891251994E-17, -0.5861220471903307860, 0.1787899950787401882 ) ) ;
#42867 = CARTESIAN_POINT ( 'NONE',  ( -0.1377952755905511861, 0.1564960629921283985, -0.7066929133858274037 ) ) ;
#42868 = AXIS2_PLACEMENT_3D ( 'NONE', #31284, #12368, #4663 ) ;
#42869 = CARTESIAN_POINT ( 'NONE',  ( 0.07405724077823318263, -1.405511810969858999, 0.1787899950787401604 ) ) ;
#42870 = ( BOUNDED_CURVE ( )  B_SPLINE_CURVE ( 2, ( #5115, #38432, #23813, #45125, #24690, #39290, #16629, #41758, #30562 ),
 .UNSPECIFIED., .F., .F. ) 
 B_SPLINE_CURVE_WITH_KNOTS ( ( 3, 2, 2, 2, 3 ),
 ( 0.7800000000000000266, 0.7824999999999999734, 0.7850000000000000311, 0.7874999999999999778, 0.7900000000000000355 ),
 .UNSPECIFIED. ) 
 CURVE ( )  GEOMETRIC_REPRESENTATION_ITEM ( )  RATIONAL_B_SPLINE_CURVE ( ( 1.000000000000000000, 0.9238795325112869605, 1.000000000000000000, 0.9238795325112869605, 1.000000000000000000, 0.9238795325112869605, 1.000000000000000000, 0.9238795325112829637, 1.000000000000000000 ) ) 
 REPRESENTATION_ITEM ( '' )  ) ;
#42871 = EDGE_CURVE ( 'NONE', #25724, #30092, #42504, .T. ) ;
#42872 = CARTESIAN_POINT ( 'NONE',  ( -1.054774247047244540, 0.07405724077823318263, 1.914370078686394860 ) ) ;
#42873 = VERTEX_POINT ( 'NONE', #46522 ) ;
#42874 = CARTESIAN_POINT ( 'NONE',  ( -0.7495606340400177148, -0.1264236179284866091, 1.390255905458047447 ) ) ;
#42875 = CARTESIAN_POINT ( 'NONE',  ( 1.002407869896990045, 0.1264236179284866091, 1.488681102308440751 ) ) ;
#42876 = EDGE_LOOP ( 'NONE', ( #38512, #24672, #29314, #39904 ) ) ;
#42877 = CARTESIAN_POINT ( 'NONE',  ( 0.8075642843603819676, 0.1651804176431314886, 0.03937007863263043694 ) ) ;
#42878 = CARTESIAN_POINT ( 'NONE',  ( -1.054774247047244540, 0.07405724077823318263, 0.5807086613635594752 ) ) ;
#42879 = CARTESIAN_POINT ( 'NONE',  ( 0.8759842519685039353, 0.1787899950787401882, 0.1943897637257641919 ) ) ;
#42880 = CARTESIAN_POINT ( 'NONE',  ( 0.1727868965068283524, -0.09842808818411986904, -0.04689813055546866727 ) ) ;
#42881 = CARTESIAN_POINT ( 'NONE',  ( 0.6971942568897648851, 0.07405724077823318263, 0.7529527558517473684 ) ) ;
#42882 = CARTESIAN_POINT ( 'NONE',  ( -0.6971942568897648851, -0.07405724077823297447, 0.5561023621509617598 ) ) ;
#42883 = EDGE_CURVE ( 'NONE', #32338, #9031, #21867, .T. ) ;
#42884 = CARTESIAN_POINT ( 'NONE',  ( 0.7185039370078746268, -0.06523048226347956391, 0.6225393700787400508 ) ) ;
#42885 = CARTESIAN_POINT ( 'NONE',  ( 0.8759842519685039353, -0.1574803149606299191, 1.141732283464567121 ) ) ;
#42886 = ORIENTED_EDGE ( 'NONE', *, *, #1494, .F. ) ;
#42887 = CARTESIAN_POINT ( 'NONE',  ( 0.1113553986120547346, -0.1604330707586147375, 0.1113553986120547346 ) ) ;
#42888 = CARTESIAN_POINT ( 'NONE',  ( -1.054774247047244540, -0.07405724077823318263, 1.481299212544662680 ) ) ;
#42889 = CYLINDRICAL_SURFACE ( 'NONE', #29513, 0.1574803149606299191 ) ;
#42890 = CARTESIAN_POINT ( 'NONE',  ( -1.033464566929134687, -0.06523048226347956391, 1.503444881889762774 ) ) ;
#42891 = CARTESIAN_POINT ( 'NONE',  ( -0.9412147342319837628, -0.1574803149606297803, 0.4749015748031497064 ) ) ;
#42892 = CARTESIAN_POINT ( 'NONE',  ( 1.054774247047244096, 0.000000000000000000, 1.326279527505291433 ) ) ;
#42893 = CARTESIAN_POINT ( 'NONE',  ( 0.1908917291238539371, -0.09851384365687540501, -0.07079149662741023030 ) ) ;
#42894 = VERTEX_POINT ( 'NONE', #22075 ) ;
#42895 = CARTESIAN_POINT ( 'NONE',  ( -1.033464566929133799, 0.000000000000000000, 0.5610236220472440971 ) ) ;
#42896 = EDGE_LOOP ( 'NONE', ( #9212, #22689, #43550, #21173 ) ) ;
#42897 = ( BOUNDED_CURVE ( )  B_SPLINE_CURVE ( 2, ( #25047, #21934, #9968, #46607, #20966, #28917, #25295, #18337, #14031 ),
 .UNSPECIFIED., .F., .F. ) 
 B_SPLINE_CURVE_WITH_KNOTS ( ( 3, 2, 2, 2, 3 ),
 ( 0.5600000000000000533, 0.5625000000000000000, 0.5649999999999999467, 0.5675000000000000044, 0.5699999999999999512 ),
 .UNSPECIFIED. ) 
 CURVE ( )  GEOMETRIC_REPRESENTATION_ITEM ( )  RATIONAL_B_SPLINE_CURVE ( ( 1.000000000000000000, 0.9238795325112869605, 1.000000000000000000, 0.9238795325112869605, 1.000000000000000000, 0.9238795325112869605, 1.000000000000000000, 0.9238795325112829637, 1.000000000000000000 ) ) 
 REPRESENTATION_ITEM ( '' )  ) ;
#42898 = CIRCLE ( 'NONE', #37557, 0.7381889763779526659 ) ;
#42899 = CARTESIAN_POINT ( 'NONE',  ( 0.1787899950787401882, -1.689592472166246306, -2.189545951927503898E-17 ) ) ;
#42900 = ORIENTED_EDGE ( 'NONE', *, *, #16889, .F. ) ;
#42901 = CARTESIAN_POINT ( 'NONE',  ( -0.1787899950787401882, -0.5516732282926929409, 0.000000000000000000 ) ) ;
#42902 = CARTESIAN_POINT ( 'NONE',  ( 0.8759842519685039353, 0.1574803149606299191, 0.4921259842519685179 ) ) ;
#42903 = ORIENTED_EDGE ( 'NONE', *, *, #31992, .F. ) ;
#42904 = VECTOR ( 'NONE', #1576, 39.37007874015748143 ) ;
#42905 = AXIS2_PLACEMENT_3D ( 'NONE', #15573, #37584, #23222 ) ;
#42906 = FACE_OUTER_BOUND ( 'NONE', #40963, .T. ) ;
#42907 = CARTESIAN_POINT ( 'NONE',  ( -0.1787899950787401882, -0.2810039369541106336, 0.000000000000000000 ) ) ;
#42908 = CARTESIAN_POINT ( 'NONE',  ( 3.284318927891251994E-17, -0.7780511810485984947, 0.1787899950787401882 ) ) ;
#42909 = CARTESIAN_POINT ( 'NONE',  ( 0.4330708661417295158, 0.1864803149606300281, -1.186023622047243986 ) ) ;
#42910 = CARTESIAN_POINT ( 'NONE',  ( -0.7646288533564489232, -0.1113553986120547346, 0.9694881888688504645 ) ) ;
#42911 = CARTESIAN_POINT ( 'NONE',  ( 0.8019270111902717657, 0.1787899950787401604, 1.687992125930489307 ) ) ;
#42912 = CARTESIAN_POINT ( 'NONE',  ( 0.8019270111902717657, 0.1787899950787401604, 0.3100393700249766682 ) ) ;
#42913 = VECTOR ( 'NONE', #44409, 39.37007874015748143 ) ;
#42914 = CARTESIAN_POINT ( 'NONE',  ( -0.1787899950787401882, -0.01636412570955368337, 0.000000000000000000 ) ) ;
#42915 = DIRECTION ( 'NONE',  ( 0.000000000000000000, 0.000000000000000000, -1.000000000000000000 ) ) ;
#42916 = CARTESIAN_POINT ( 'NONE',  ( 0.8759842519685039353, 0.000000000000000000, 4.498031496062992574 ) ) ;
#42917 = CARTESIAN_POINT ( 'NONE',  ( 0.9500414927467378812, 0.1787899950787401604, 0.6200787401037165525 ) ) ;
#42918 = CARTESIAN_POINT ( 'NONE',  ( -0.7495606340400177148, 0.1264236179284866091, 0.7504921259304880854 ) ) ;
#42920 = CYLINDRICAL_SURFACE ( 'NONE', #10900, 0.009842519685039378616 ) ;
#42919 = CARTESIAN_POINT ( 'NONE',  ( 0.1113553986120547346, -0.9183070866141731514, 0.1113553986120547346 ) ) ;
#42922 = CARTESIAN_POINT ( 'NONE',  ( -0.8080376074351401927, -0.1583691422869495102, 1.986918182731025384 ) ) ;
#42921 = CARTESIAN_POINT ( 'NONE',  ( 0.1797182628040039087, -1.794827274149976004, 0.07444174185955046430 ) ) ;
#42923 = DIRECTION ( 'NONE',  ( -1.000000000000000000, 0.000000000000000000, 0.000000000000000000 ) ) ;
#42924 = CARTESIAN_POINT ( 'NONE',  ( 0.8759842519685039353, 0.1787899950787401882, 1.690452755851748146 ) ) ;
#42926 = CARTESIAN_POINT ( 'NONE',  ( -0.3161444924769509779, 1.209494567139720367, -1.479906699140297599 ) ) ;
#42925 = CARTESIAN_POINT ( 'NONE',  ( 0.6971942568897648851, 0.07405724077823318263, 1.968503936954110412 ) ) ;
#42927 = CARTESIAN_POINT ( 'NONE',  ( 1.002407869896990045, -0.1264236179284866091, 0.3715551180564728440 ) ) ;
#42928 = EDGE_CURVE ( 'NONE', #11388, #46575, #35756, .T. ) ;
#42929 = ORIENTED_EDGE ( 'NONE', *, *, #35882, .F. ) ;
#42931 = VERTEX_POINT ( 'NONE', #17533 ) ;
#42930 = CARTESIAN_POINT ( 'NONE',  ( -0.2090839795233657428, -0.06563552548624972116, -0.1647146447860223517 ) ) ;
#42932 = CARTESIAN_POINT ( 'NONE',  ( -0.1377952755905511584, 0.1574803149606320007, 0.7057086614173230243 ) ) ;
#42933 = CARTESIAN_POINT ( 'NONE',  ( -0.07405724077823318263, -0.09153543301710270752, -0.1787899950787401604 ) ) ;
#42934 = CARTESIAN_POINT ( 'NONE',  ( 1.002407869896990045, -0.1264236179284866091, 0.5684055117572598403 ) ) ;
#42935 = CARTESIAN_POINT ( 'NONE',  ( 0.1787899950787401882, -0.8863188975840314843, -2.189545951927503898E-17 ) ) ;
#42936 = CARTESIAN_POINT ( 'NONE',  ( 1.054774247047244540, 0.07405724077823318263, 0.1082677164816695514 ) ) ;
#42937 = DIRECTION ( 'NONE',  ( 0.000000000000000000, 0.000000000000000000, -1.000000000000000000 ) ) ;
#42938 = CARTESIAN_POINT ( 'NONE',  ( 0.9500414927467377701, 0.1787899950787401604, 0.5413385826234012876 ) ) ;
#42939 = CIRCLE ( 'NONE', #41388, 0.1574803149606299191 ) ;
#42940 = DIRECTION ( 'NONE',  ( -1.000000000000000000, 0.000000000000000000, 7.047314121155780399E-15 ) ) ;
#42941 = CARTESIAN_POINT ( 'NONE',  ( -0.7495606340400177148, 0.1264236179284866091, 1.454232283410803017 ) ) ;
#42942 = VERTEX_POINT ( 'NONE', #25459 ) ;
#42943 = CARTESIAN_POINT ( 'NONE',  ( -0.2644738720849209024, -0.1618167320693821298, -0.8319978239451156776 ) ) ;
#42944 = CARTESIAN_POINT ( 'NONE',  ( 0.8019270111902717657, 0.1787899950787401604, 1.220472440891118504 ) ) ;
#42945 = CARTESIAN_POINT ( 'NONE',  ( -0.8107537697050253289, -0.1574803149606297803, 0.7357283463491665065 ) ) ;
#42946 = AXIS2_PLACEMENT_3D ( 'NONE', #17281, #31917, #2875 ) ;
#42947 = CARTESIAN_POINT ( 'NONE',  ( 0.8107537697050254399, 0.1574803149606300301, 0.1008858267716536417 ) ) ;
#42948 = CARTESIAN_POINT ( 'NONE',  ( 1.002407869896990045, 0.1264236179284866091, 1.798720472387181024 ) ) ;
#42949 = CARTESIAN_POINT ( 'NONE',  ( -0.7185039370078739607, 1.928577636452523993E-17, 1.328740157480315043 ) ) ;
#42950 = CARTESIAN_POINT ( 'NONE',  ( -1.002407869896990045, 0.1264236179284866091, 0.8932086613635591421 ) ) ;
#42951 = DIRECTION ( 'NONE',  ( -1.000000000000000000, 0.000000000000000000, 0.000000000000000000 ) ) ;
#42952 = CARTESIAN_POINT ( 'NONE',  ( -0.7010411943706328364, 0.01421195604105837673, 0.03937007874015843734 ) ) ;
#42953 = CARTESIAN_POINT ( 'NONE',  ( 0.7495606340400177148, -0.1264236179284866091, 0.1304133857730082613 ) ) ;
#42954 = ADVANCED_FACE ( 'NONE', ( #43393 ), #39564, .T. ) ;
#42955 = CARTESIAN_POINT ( 'NONE',  ( 0.8759842519685039353, 0.1574803149606299191, 1.505905511703495847 ) ) ;
#42956 = ORIENTED_EDGE ( 'NONE', *, *, #12683, .T. ) ;
#42957 = EDGE_CURVE ( 'NONE', #18156, #10815, #33138, .T. ) ;
#42958 = CARTESIAN_POINT ( 'NONE',  ( -0.1264236179284866091, -0.04970472435568527164, -0.1264236179284866091 ) ) ;
#42959 = CARTESIAN_POINT ( 'NONE',  ( 0.7495606340400177148, 0.1264236179284866091, 0.8292322834108031282 ) ) ;
#42960 = CARTESIAN_POINT ( 'NONE',  ( -0.8019270111902716547, 0.1787899950787401604, 1.687992125930489307 ) ) ;
#42961 = EDGE_LOOP ( 'NONE', ( #44160, #26404, #11862, #45926 ) ) ;
#42962 = CARTESIAN_POINT ( 'NONE',  ( 0.000000000000000000, -5.122214988120488358E-16, -8.878505979408856939E-16 ) ) ;
#42963 = CYLINDRICAL_SURFACE ( 'NONE', #5307, 0.1003937007874011050 ) ;
#42964 = CARTESIAN_POINT ( 'NONE',  ( -0.07405724077823318263, -1.244218456418216601, -0.1787899950787401604 ) ) ;
#42965 = ORIENTED_EDGE ( 'NONE', *, *, #30668, .F. ) ;
#42966 = CARTESIAN_POINT ( 'NONE',  ( 0.1264236179284866091, -0.1333661416785200671, -0.1264236179284866091 ) ) ;
#42967 = VERTEX_POINT ( 'NONE', #17299 ) ;
#42968 = CARTESIAN_POINT ( 'NONE',  ( 0.6971942568897648851, 0.07405724077823318263, 1.102362204670646495 ) ) ;
#42969 = AXIS2_PLACEMENT_3D ( 'NONE', #20664, #27666, #2445 ) ;
#42970 = CARTESIAN_POINT ( 'NONE',  ( 0.7185039370078739607, 1.928577636452523993E-17, 0.8070866140657008136 ) ) ;
#42971 = VECTOR ( 'NONE', #34313, 39.37007874015748143 ) ;
#42972 = CARTESIAN_POINT ( 'NONE',  ( 0.9873396505805591694, 0.1113553986120547346, 1.943897637795275690 ) ) ;
#42973 = AXIS2_PLACEMENT_3D ( 'NONE', #8933, #12315, #34353 ) ;
#42974 = CONICAL_SURFACE ( 'NONE', #46820, 0.1377952755905511861, 1.047197551196598297 ) ;
#42975 = CARTESIAN_POINT ( 'NONE',  ( 0.07405724077823318263, -1.410433070812377565, 0.1787899950787401604 ) ) ;
#42976 = EDGE_CURVE ( 'NONE', #6860, #2262, #39433, .T. ) ;
#42977 = EDGE_CURVE ( 'NONE', #28080, #9213, #4990, .T. ) ;
#42978 = CARTESIAN_POINT ( 'NONE',  ( -0.8019270111902716547, 0.1787899950787401604, 0.3543307086076538659 ) ) ;
#42980 = CARTESIAN_POINT ( 'NONE',  ( -0.7287072466478243804, 0.07236760742655255763, 1.981831751466828884 ) ) ;
#42979 = CARTESIAN_POINT ( 'NONE',  ( -0.1797182628040039087, -1.258409951315329289, 0.07444174185955065859 ) ) ;
#42981 = CARTESIAN_POINT ( 'NONE',  ( -0.9412147342319837628, 0.1574803149606300301, 0.2140748031496061965 ) ) ;
#42982 = CARTESIAN_POINT ( 'NONE',  ( 1.054774247047244096, 0.000000000000000000, 1.208169291284818980 ) ) ;
#42983 = CARTESIAN_POINT ( 'NONE',  ( 0.6971942568897637749, 2.189545951927499583E-17, 1.459153543253322693 ) ) ;
#42984 = EDGE_CURVE ( 'NONE', #31435, #5631, #6523, .T. ) ;
#42985 = CARTESIAN_POINT ( 'NONE',  ( 0.8759842519685039353, -0.1574803149606299191, 1.653543307086614345 ) ) ;
#42987 = CARTESIAN_POINT ( 'NONE',  ( -0.7185039370078739607, 1.928577636452523993E-17, 1.092519685039370136 ) ) ;
#42986 = DIRECTION ( 'NONE',  ( -0.000000000000000000, 0.000000000000000000, -1.000000000000000000 ) ) ;
#42988 = CYLINDRICAL_SURFACE ( 'NONE', #33596, 0.1574803149606299191 ) ;
#42989 = CARTESIAN_POINT ( 'NONE',  ( -0.9873396505805591694, 0.1113553986120547346, 1.776574803042078488 ) ) ;
#42990 = CARTESIAN_POINT ( 'NONE',  ( 1.054774247047244540, -0.07405724077823318263, 0.1771653542769450751 ) ) ;
#42991 = CARTESIAN_POINT ( 'NONE',  ( 0.4620708661417345375, 0.6102362204724407491, 0.9891732283464566011 ) ) ;
#42993 = CARTESIAN_POINT ( 'NONE',  ( -0.9873396505805591694, 0.1113553986120547346, 1.943897637795275690 ) ) ;
#42992 = CARTESIAN_POINT ( 'NONE',  ( 1.054774247047244096, 0.000000000000000000, 1.085137795221826629 ) ) ;
#42994 = CARTESIAN_POINT ( 'NONE',  ( 0.8019270111902716547, -0.1787899950787401604, 1.983267716481668108 ) ) ;
#42995 = CARTESIAN_POINT ( 'NONE',  ( 0.7646288533564489232, 0.1113553986120547346, 0.5659448817822370081 ) ) ;
#42996 = ORIENTED_EDGE ( 'NONE', *, *, #29905, .F. ) ;
#42997 = DIRECTION ( 'NONE',  ( 0.000000000000000000, 0.7071067811867007835, 0.7071067811863941399 ) ) ;
#42998 = CARTESIAN_POINT ( 'NONE',  ( 0.9697133612655820523, 0.1395208940671603115, 0.03936960452481068351 ) ) ;
#42999 = CARTESIAN_POINT ( 'NONE',  ( -0.9873396505805591694, -0.1113553986120547346, 0.4281496061916850726 ) ) ;
#43000 = EDGE_LOOP ( 'NONE', ( #19227, #34033, #30520, #20940 ) ) ;
#43001 = CARTESIAN_POINT ( 'NONE',  ( 0.8759842519685039353, -0.1787899950787401882, 1.508366141678519678 ) ) ;
#43002 = MECHANICAL_DESIGN_GEOMETRIC_PRESENTATION_REPRESENTATION (  '', ( #22360 ), #33854 ) ;
#43004 = CARTESIAN_POINT ( 'NONE',  ( 0.000000000000000000, 0.000000000000000000, -0.2219368594840610276 ) ) ;
#43003 = CARTESIAN_POINT ( 'NONE',  ( -0.7185039370078739607, 1.928577636452523993E-17, 1.643700787401574992 ) ) ;
#43005 = CARTESIAN_POINT ( 'NONE',  ( -0.07405724077823318263, -0.04724409443442544737, -0.1787899950787401604 ) ) ;
#43006 = ORIENTED_EDGE ( 'NONE', *, *, #25746, .F. ) ;
#43007 = LINE ( 'NONE', #10216, #19932 ) ;
#43008 = VERTEX_POINT ( 'NONE', #8873 ) ;
#43009 = CARTESIAN_POINT ( 'NONE',  ( 0.1465299180647062771, 0.09658349877441903264, 0.2008339832271497927 ) ) ;
#43010 = ( NAMED_UNIT ( * ) PLANE_ANGLE_UNIT ( ) SI_UNIT ( $, .RADIAN. ) ) ;
#43011 = ORIENTED_EDGE ( 'NONE', *, *, #27138, .T. ) ;
#43012 = CARTESIAN_POINT ( 'NONE',  ( 0.7495606340400177148, -0.1264236179284866091, 0.4453740156942677664 ) ) ;
#43013 = VERTEX_POINT ( 'NONE', #40959 ) ;
#43014 = CARTESIAN_POINT ( 'NONE',  ( -0.9500414927467377701, -0.1787899950787401604, 1.432086614119464141 ) ) ;
#43016 = CARTESIAN_POINT ( 'NONE',  ( 3.284318927891251994E-17, -1.649114173174582643, 0.1787899950787401882 ) ) ;
#43015 = CARTESIAN_POINT ( 'NONE',  ( 0.1574803149606300301, -0.3892716534357800184, -0.06523048226347956391 ) ) ;
#43017 = CARTESIAN_POINT ( 'NONE',  ( -1.054774247047244540, 0.07405724077823318263, 1.131889763725763665 ) ) ;
#43018 = AXIS2_PLACEMENT_3D ( 'NONE', #13149, #16724, #31358 ) ;
#43019 = CARTESIAN_POINT ( 'NONE',  ( -1.054774247047244096, 0.000000000000000000, 1.951279527505291433 ) ) ;
#43020 = ORIENTED_EDGE ( 'NONE', *, *, #37217, .T. ) ;
#43021 = CARTESIAN_POINT ( 'NONE',  ( -0.7495606340400177148, -0.1264236179284866091, 1.109744094434425232 ) ) ;
#43022 = CARTESIAN_POINT ( 'NONE',  ( -0.8759842519685039353, -0.1787899950787401882, 0.7652559054580472253 ) ) ;
#43023 = DIRECTION ( 'NONE',  ( -0.5735764363510518216, -0.8191520442889876907, 0.000000000000000000 ) ) ;
#43024 = CARTESIAN_POINT ( 'NONE',  ( 1.033464566929133799, 0.000000000000000000, 0.8366141732283465249 ) ) ;
#43025 = CARTESIAN_POINT ( 'NONE',  ( -0.07405724077823318263, -0.6389034957882946397, 0.1787899950787401604 ) ) ;
#43026 = VECTOR ( 'NONE', #27956, 39.37007874015748143 ) ;
#43027 = VERTEX_POINT ( 'NONE', #30248 ) ;
#43028 = CARTESIAN_POINT ( 'NONE',  ( -0.1528862059369570925, -0.08956163382569545806, 0.06277908432128326277 ) ) ;
#43029 = CARTESIAN_POINT ( 'NONE',  ( 0.03372458374097397904, 0.7769110883301575399, -0.6069894663860452289 ) ) ;
#43030 = VERTEX_POINT ( 'NONE', #15852 ) ;
#43031 = ORIENTED_EDGE ( 'NONE', *, *, #13397, .T. ) ;
#43032 = CARTESIAN_POINT ( 'NONE',  ( -0.9873396505805591694, -0.1113553986120547346, 1.737204724409448842 ) ) ;
#43033 = CARTESIAN_POINT ( 'NONE',  ( -1.054774247047244096, 0.000000000000000000, 0.6520669290800944484 ) ) ;
#43034 = DIRECTION ( 'NONE',  ( 0.000000000000000000, 0.000000000000000000, -1.000000000000000000 ) ) ;
#43035 = CARTESIAN_POINT ( 'NONE',  ( -0.7495606340400177148, -0.1264236179284866091, 1.626476377898992132 ) ) ;
#43036 = EDGE_CURVE ( 'NONE', #5382, #17227, #24852, .T. ) ;
#43037 = DIRECTION ( 'NONE',  ( 0.000000000000000000, 0.000000000000000000, 1.000000000000000000 ) ) ;
#43038 = EDGE_CURVE ( 'NONE', #44478, #25373, #13254, .T. ) ;
#43039 = CIRCLE ( 'NONE', #44574, 0.04921259842519688094 ) ;
#43040 = CARTESIAN_POINT ( 'NONE',  ( 0.7646288533564489232, 0.1113553986120547346, 1.038385826664126155 ) ) ;
#43041 = FACE_OUTER_BOUND ( 'NONE', #35382, .T. ) ;
#43042 = CARTESIAN_POINT ( 'NONE',  ( 1.033464566929134687, 0.06523048226347956391, 0.6028543307086614567 ) ) ;
#43043 = CARTESIAN_POINT ( 'NONE',  ( 0.07444174185955065859, -0.8154965654885567572, 0.1797182628040039087 ) ) ;
#43044 = CARTESIAN_POINT ( 'NONE',  ( -0.1476377952755905387, -0.5010918323780657602, -0.8705539716229625524 ) ) ;
#43045 = CARTESIAN_POINT ( 'NONE',  ( 0.8019270111902717657, 0.1787899950787401604, 0.7480314960092282472 ) ) ;
#43046 = EDGE_CURVE ( 'NONE', #19079, #39641, #5510, .T. ) ;
#43047 = CARTESIAN_POINT ( 'NONE',  ( 0.1113553986120547346, -0.6427165354330708347, 0.1113553986120547346 ) ) ;
#43048 = CARTESIAN_POINT ( 'NONE',  ( 0.2395294000716134131, 2.049113738730802390E-17, 1.043307086614172929 ) ) ;
#43049 = ORIENTED_EDGE ( 'NONE', *, *, #22188, .T. ) ;
#43050 = EDGE_CURVE ( 'NONE', #40024, #31750, #27823, .T. ) ;
#43051 = FACE_OUTER_BOUND ( 'NONE', #482, .T. ) ;
#43052 = CARTESIAN_POINT ( 'NONE',  ( 0.9412147342319837628, 0.1574803149606300301, 1.237696850393701586 ) ) ;
#43054 = DIRECTION ( 'NONE',  ( -3.469446951953614978E-15, -1.000000000000000000, 3.995705278811693553E-31 ) ) ;
#43053 = CARTESIAN_POINT ( 'NONE',  ( 0.7550969956560203977, -0.1199135176416183252, 1.985721262792661257 ) ) ;
#43055 = CARTESIAN_POINT ( 'NONE',  ( 1.033464566929133799, 0.000000000000000000, 1.860236220472440971 ) ) ;
#43057 = LINE ( 'NONE', #3763, #36107 ) ;
#43056 = CARTESIAN_POINT ( 'NONE',  ( 1.054774247047244540, 0.07405724077823318263, 0.7332677164816705506 ) ) ;
#43058 = CARTESIAN_POINT ( 'NONE',  ( -0.1264236179284866091, -0.6254921259304881964, 0.1264236179284866091 ) ) ;
#43059 = CARTESIAN_POINT ( 'NONE',  ( 0.000000000000000000, 0.1473293504822046074, -0.9532488779249699284 ) ) ;
#43060 = VERTEX_POINT ( 'NONE', #5454 ) ;
#43061 = CARTESIAN_POINT ( 'NONE',  ( -0.1586641775163213364, 2.177585298233989164, -3.731703755406937439 ) ) ;
#43062 = CARTESIAN_POINT ( 'NONE',  ( 0.9873396505805591694, 0.1113553986120547346, 1.747047244094488194 ) ) ;
#43063 = CARTESIAN_POINT ( 'NONE',  ( 0.7646288533564489232, -0.1113553986120547346, 0.7037401574803149318 ) ) ;
#43064 = CARTESIAN_POINT ( 'NONE',  ( 1.002407869896990045, 0.1264236179284866091, 0.9325787401037164415 ) ) ;
#43065 = DIRECTION ( 'NONE',  ( -0.000000000000000000, 1.000000000000000000, -0.000000000000000000 ) ) ;
#43066 = CARTESIAN_POINT ( 'NONE',  ( 0.8107537697050254399, -0.1574803149606297803, 0.6963582676090083190 ) ) ;
#43067 = CARTESIAN_POINT ( 'NONE',  ( 0.1264236179284866091, -1.796751968450173376, 0.1264236179284866091 ) ) ;
#43068 = CARTESIAN_POINT ( 'NONE',  ( 0.1264236179284866091, -1.093011810969858333, 0.1264236179284866091 ) ) ;
#43069 = CARTESIAN_POINT ( 'NONE',  ( -0.06523048226347956391, -1.594980314960629419, 0.1574803149606297803 ) ) ;
#43070 = CARTESIAN_POINT ( 'NONE',  ( -0.1184675242425147629, -0.5708661417322835607, 1.161904259418922170 ) ) ;
#43071 = CARTESIAN_POINT ( 'NONE',  ( -0.7495606340400177148, -0.1264236179284866091, 0.1254921259304885850 ) ) ;
#43072 = EDGE_LOOP ( 'NONE', ( #4282, #29202, #9732, #43497 ) ) ;
#43073 = VERTEX_POINT ( 'NONE', #16493 ) ;
#43074 = DIRECTION ( 'NONE',  ( 1.000000000000000000, 0.000000000000000000, -1.822029033848725275E-16 ) ) ;
#43075 = ORIENTED_EDGE ( 'NONE', *, *, #5182, .T. ) ;
#43076 = CARTESIAN_POINT ( 'NONE',  ( 2.892866454678787531E-17, -1.425196850286173156, 0.1574803149606299191 ) ) ;
#43077 = CARTESIAN_POINT ( 'NONE',  ( -1.002407869896990045, -0.1264236179284866091, 1.990649606245448844 ) ) ;
#43078 = CARTESIAN_POINT ( 'NONE',  ( -0.9500414927467378812, 0.1787899950787401604, 1.486220472387181690 ) ) ;
#43079 = CARTESIAN_POINT ( 'NONE',  ( 1.002407869896990045, 0.1264236179284866091, 0.8587598424659212970 ) ) ;
#43080 = CARTESIAN_POINT ( 'NONE',  ( -0.8759842519685039353, 0.1787899950787401882, 0.8193897637257637756 ) ) ;
#43081 = CIRCLE ( 'NONE', #10193, 0.08090551181102362266 ) ;
#43082 = CARTESIAN_POINT ( 'NONE',  ( -0.8019270111902717657, -0.1787899950787401604, 1.072834645615528659 ) ) ;
#43083 = CARTESIAN_POINT ( 'NONE',  ( -1.054774247047244540, -0.07405724077823318263, 0.1820866141194649179 ) ) ;
#43084 = CIRCLE ( 'NONE', #39256, 0.1968503937007874405 ) ;
#43085 = DIRECTION ( 'NONE',  ( -1.000000000000000000, 0.000000000000000000, 0.000000000000000000 ) ) ;
#43086 = CARTESIAN_POINT ( 'NONE',  ( -0.6971942568897648851, 0.07405724077823318263, 1.973425196796630088 ) ) ;
#43087 = CARTESIAN_POINT ( 'NONE',  ( -0.7185039370078746268, -0.06523048226347956391, 1.843011811023621327 ) ) ;
#43088 = DIRECTION ( 'NONE',  ( 1.000000000000000000, 0.000000000000000000, -1.822029033848725275E-16 ) ) ;
#43089 = CARTESIAN_POINT ( 'NONE',  ( 0.07405724077823318263, -0.2009113698040420337, 0.1787899950787401604 ) ) ;
#43090 = CARTESIAN_POINT ( 'NONE',  ( 0.3980944881889795228, 0.9100161909011693639, 0.01858545845903165558 ) ) ;
#43091 = CARTESIAN_POINT ( 'NONE',  ( 0.1673228346456693549, 0.1005108776172154716, -0.1165245190822937205 ) ) ;
#43092 = AXIS2_PLACEMENT_3D ( 'NONE', #36773, #3932, #26241 ) ;
#43093 = CARTESIAN_POINT ( 'NONE',  ( -0.7495606340400177148, 0.1264236179284866091, 0.2337598424659216578 ) ) ;
#43094 = ORIENTED_EDGE ( 'NONE', *, *, #12298, .T. ) ;
#43095 = CARTESIAN_POINT ( 'NONE',  ( -0.7495606340400177148, -0.1264236179284866091, 1.232775590497417362 ) ) ;
#43096 = ORIENTED_EDGE ( 'NONE', *, *, #2428, .F. ) ;
#43097 = CARTESIAN_POINT ( 'NONE',  ( -0.1264236179284866091, -1.142224409395055096, 0.1264236179284866091 ) ) ;
#43098 = CARTESIAN_POINT ( 'NONE',  ( 0.1787899950787401604, -1.316929133804503937, -0.07405724077823318263 ) ) ;
#43099 = ADVANCED_FACE ( 'NONE', ( #20071 ), #23918, .T. ) ;
#43100 = CARTESIAN_POINT ( 'NONE',  ( -0.9873396505805591694, -0.1113553986120547346, 1.373031495955464587 ) ) ;
#43101 = CARTESIAN_POINT ( 'NONE',  ( -0.7646288533564489232, -0.1113553986120547346, 0.2312992125984252023 ) ) ;
#43102 = CARTESIAN_POINT ( 'NONE',  ( -0.9412147342319837628, 0.1574803149606300301, 0.6865157480314957317 ) ) ;
#43103 = CARTESIAN_POINT ( 'NONE',  ( 0.06523048226347956391, -0.2121062992125984648, 0.1574803149606297803 ) ) ;
#43104 = CARTESIAN_POINT ( 'NONE',  ( 0.8107537697050253289, 0.1574803149606300301, 1.783956692805858779 ) ) ;
#43105 = ORIENTED_EDGE ( 'NONE', *, *, #14679, .T. ) ;
#43106 = EDGE_CURVE ( 'NONE', #40003, #4077, #27998, .T. ) ;
#43107 = CARTESIAN_POINT ( 'NONE',  ( -0.9873396505805591694, 0.1113553986120547346, 1.422244094380661572 ) ) ;
#43108 = CARTESIAN_POINT ( 'NONE',  ( 0.7185039370078746268, 0.06523048226347956391, 0.7750984251968497940 ) ) ;
#43109 = DIRECTION ( 'NONE',  ( 1.000000000000000000, -3.469446951953625627E-15, -0.000000000000000000 ) ) ;
#43110 = CARTESIAN_POINT ( 'NONE',  ( -0.8107537697050254399, 0.1574803149606300301, 1.242618110236220819 ) ) ;
#43112 = CARTESIAN_POINT ( 'NONE',  ( 0.9873396505805591694, 0.1113553986120547346, 1.510826771653543288 ) ) ;
#43111 = CARTESIAN_POINT ( 'NONE',  ( 0.4330708661417327909, 0.1574803149606300301, -1.186023622047243986 ) ) ;
#43113 = CARTESIAN_POINT ( 'NONE',  ( 0.8107537697050234415, -0.1574803149606297803, 0.2239173227271187561 ) ) ;
#43114 = VECTOR ( 'NONE', #34246, 39.37007874015748143 ) ;
#43115 = ORIENTED_EDGE ( 'NONE', *, *, #28716, .T. ) ;
#43116 = ORIENTED_EDGE ( 'NONE', *, *, #3254, .F. ) ;
#43117 = CARTESIAN_POINT ( 'NONE',  ( -1.033464566929134687, -0.06523048226347956391, 0.6274606298137325178 ) ) ;
#43118 = CARTESIAN_POINT ( 'NONE',  ( 0.7185039370078739607, 1.928577636452523993E-17, 1.407480314960629864 ) ) ;
#43119 = CARTESIAN_POINT ( 'NONE',  ( -0.1113553986120547346, -1.508858267609007653, 0.1113553986120547346 ) ) ;
#43120 = CARTESIAN_POINT ( 'NONE',  ( -1.094772975963752103E-17, -0.5664370078202519698, -0.1787899950787401882 ) ) ;
#43121 = CARTESIAN_POINT ( 'NONE',  ( 2.892866454678787531E-17, -1.041338582677165503, 0.1574803149606299191 ) ) ;
#43122 = CARTESIAN_POINT ( 'NONE',  ( 1.033464566929134687, 0.06523048226347956391, 0.9473425195775121432 ) ) ;
#43123 = CYLINDRICAL_SURFACE ( 'NONE', #696, 0.3937007874015748254 ) ;
#43124 = CARTESIAN_POINT ( 'NONE',  ( -1.002407869896990045, 0.1264236179284866091, 0.4207677164816693294 ) ) ;
#43125 = ORIENTED_EDGE ( 'NONE', *, *, #30773, .F. ) ;
#43126 = VECTOR ( 'NONE', #46759, 39.37007874015748143 ) ;
#43127 = CARTESIAN_POINT ( 'NONE',  ( -0.7495606340400177148, 0.1264236179284866091, 1.498523621993480326 ) ) ;
#43128 = CARTESIAN_POINT ( 'NONE',  ( 0.6971942568897648851, 0.07405724077823318263, 1.540354330654897685 ) ) ;
#43129 = ORIENTED_EDGE ( 'NONE', *, *, #30410, .F. ) ;
#43130 = DIRECTION ( 'NONE',  ( -1.000000000000000000, 0.000000000000000000, 0.000000000000000000 ) ) ;
#43131 = CARTESIAN_POINT ( 'NONE',  ( -0.6971942568897626646, -0.07405724077823297447, 0.6003937007336389575 ) ) ;
#43132 = CARTESIAN_POINT ( 'NONE',  ( 0.6971942568897626646, -0.07405724077823297447, 0.2066929133320631329 ) ) ;
#43133 = CARTESIAN_POINT ( 'NONE',  ( -0.8070866141732283561, 0.000000000000000000, -0.8568897637795275246 ) ) ;
#43134 = CARTESIAN_POINT ( 'NONE',  ( 1.002407869896990045, 0.1264236179284866091, 0.7406496062454487328 ) ) ;
#43135 = CARTESIAN_POINT ( 'NONE',  ( -0.7495606340400177148, 0.1264236179284866091, 0.7062007873478109987 ) ) ;
#43136 = DIRECTION ( 'NONE',  ( 1.000000000000000000, -0.000000000000000000, -0.000000000000000000 ) ) ;
#43137 = CARTESIAN_POINT ( 'NONE',  ( 2.892866454678787531E-17, -0.2047244093412921295, 0.1574803149606299191 ) ) ;
#43138 = CARTESIAN_POINT ( 'NONE',  ( -1.002407869896990045, -0.1264236179284866091, 1.400098425143086800 ) ) ;
#43139 = DIRECTION ( 'NONE',  ( 1.822029033848725028E-16, 0.000000000000000000, 1.000000000000000000 ) ) ;
#43140 = CARTESIAN_POINT ( 'NONE',  ( -1.033464566929134687, -0.06523048226347956391, 0.4798228346456688831 ) ) ;
#43141 = CARTESIAN_POINT ( 'NONE',  ( 1.054774247047244540, -0.07405724077823318263, 1.284448818843874518 ) ) ;
#43142 = ( REPRESENTATION_RELATIONSHIP ('NONE','NONE', #9609, #1042 ) REPRESENTATION_RELATIONSHIP_WITH_TRANSFORMATION ( #32175 )SHAPE_REPRESENTATION_RELATIONSHIP( ) ) ;
#43143 = EDGE_LOOP ( 'NONE', ( #18364, #3259, #8260 ) ) ;
#43144 = CARTESIAN_POINT ( 'NONE',  ( -0.7646288533564489232, -0.1113553986120547346, 0.6250000000000000000 ) ) ;
#43145 = ORIENTED_EDGE ( 'NONE', *, *, #46836, .F. ) ;
#43146 = LINE ( 'NONE', #17295, #10907 ) ;
#43147 = VERTEX_POINT ( 'NONE', #5208 ) ;
#43148 = CARTESIAN_POINT ( 'NONE',  ( 1.054774247047244540, -0.07405724077823318263, 1.397637795221827295 ) ) ;
#43149 = EDGE_CURVE ( 'NONE', #42942, #39852, #46407, .T. ) ;
#43150 = CARTESIAN_POINT ( 'NONE',  ( -0.8759842519685039353, -0.1574803149606299191, 0.03937007874015843040 ) ) ;
#43151 = CARTESIAN_POINT ( 'NONE',  ( -0.1787899950787401604, -0.2834645668753703052, -0.07405724077823318263 ) ) ;
#43152 = CARTESIAN_POINT ( 'NONE',  ( 0.1787899950787401882, -0.9256889763241890057, -2.189545951927503898E-17 ) ) ;
#43153 = EDGE_CURVE ( 'NONE', #22330, #36803, #33359, .T. ) ;
#43154 = CARTESIAN_POINT ( 'NONE',  ( -0.2471922904502826812, -0.03219022224904098672, -0.1427165354330708902 ) ) ;
#43155 = CARTESIAN_POINT ( 'NONE',  ( 0.000000000000000000, 0.4003652867858621955, 0.7276473417831970103 ) ) ;
#43156 = CARTESIAN_POINT ( 'NONE',  ( 1.002407869896990045, -0.1264236179284866091, 0.2534448818360003908 ) ) ;
#43157 = CIRCLE ( 'NONE', #43928, 0.01968503937007875723 ) ;
#43158 = CARTESIAN_POINT ( 'NONE',  ( 0.1787899950787401604, -0.07295861389853010304, -0.07405724077823318263 ) ) ;
#43159 = CARTESIAN_POINT ( 'NONE',  ( 0.1787899950787401604, -0.2588582676627719792, 0.07405724077823318263 ) ) ;
#43160 = CARTESIAN_POINT ( 'NONE',  ( -0.07405724077823318263, 0.06594488194352733645, -0.1787899950787401604 ) ) ;
#43161 = CARTESIAN_POINT ( 'NONE',  ( 0.01656181348484438501, -0.09842519685039362309, 0.1616518427886418363 ) ) ;
#43162 = CARTESIAN_POINT ( 'NONE',  ( 0.01230737760510395781, 0.07955613945526338049, -0.1377952755905511861 ) ) ;
#43163 = EDGE_CURVE ( 'NONE', #37935, #16713, #5781, .T. ) ;
#43164 = CARTESIAN_POINT ( 'NONE',  ( 1.002407869896990045, 0.1264236179284866091, 0.6176181101824566033 ) ) ;
#43165 = ( BOUNDED_CURVE ( )  B_SPLINE_CURVE ( 2, ( #46913, #46671, #14103, #43792, #40181, #28504, #10517, #47398, #7382 ),
 .UNSPECIFIED., .F., .F. ) 
 B_SPLINE_CURVE_WITH_KNOTS ( ( 3, 2, 2, 2, 3 ),
 ( 0.6199999999999999956, 0.6225000000000000533, 0.6250000000000000000, 0.6274999999999999467, 0.6300000000000000044 ),
 .UNSPECIFIED. ) 
 CURVE ( )  GEOMETRIC_REPRESENTATION_ITEM ( )  RATIONAL_B_SPLINE_CURVE ( ( 1.000000000000000000, 0.9238795325112869605, 1.000000000000000000, 0.9238795325112869605, 1.000000000000000000, 0.9238795325112869605, 1.000000000000000000, 0.9238795325112869605, 1.000000000000000000 ) ) 
 REPRESENTATION_ITEM ( '' )  ) ;
#43166 = CARTESIAN_POINT ( 'NONE',  ( -0.8759842519685039353, -0.1787899950787401882, 0.9227362204186770889 ) ) ;
#43168 = CARTESIAN_POINT ( 'NONE',  ( 1.033464566929134687, 0.06523048226347956391, 1.695374015640504828 ) ) ;
#43167 = DIRECTION ( 'NONE',  ( 0.000000000000000000, 0.000000000000000000, 1.000000000000000000 ) ) ;
#43169 = CARTESIAN_POINT ( 'NONE',  ( -1.100456976456230270E-17, -1.743154045803517738, -0.1797182628040039365 ) ) ;
#43170 = CARTESIAN_POINT ( 'NONE',  ( 0.1377952755905512139, 0.1564960629921262614, 0.7066929133858274037 ) ) ;
#43171 = CARTESIAN_POINT ( 'NONE',  ( 1.054774247047244540, 0.07405724077823318263, 1.604330708607653921 ) ) ;
#43173 = CARTESIAN_POINT ( 'NONE',  ( 0.1611065205447556881, 0.1591792231633174792, 3.327488133692118618E-06 ) ) ;
#43172 = CARTESIAN_POINT ( 'NONE',  ( 1.054774247047244540, -0.07405724077823318263, 1.988188976324191781 ) ) ;
#43174 = CARTESIAN_POINT ( 'NONE',  ( 0.8759842519685039353, -0.1787899950787401882, 0.5241141731745827537 ) ) ;
#43175 = VERTEX_POINT ( 'NONE', #30897 ) ;
#43176 = DIRECTION ( 'NONE',  ( 0.000000000000000000, 1.000000000000000000, 0.000000000000000000 ) ) ;
#43177 = CARTESIAN_POINT ( 'NONE',  ( 0.07405724077823318263, -0.1899606298674962612, 0.1787899950787401604 ) ) ;
#43178 = CARTESIAN_POINT ( 'NONE',  ( 0.8019270111902717657, 0.1787899950787401604, 0.6643700786863951935 ) ) ;
#43179 = CARTESIAN_POINT ( 'NONE',  ( 0.1264236179284866091, -1.156988188922614125, -0.1264236179284866091 ) ) ;
#43180 = CARTESIAN_POINT ( 'NONE',  ( 0.6971942568897637749, 2.189545951927499583E-17, 0.1254921259304885850 ) ) ;
#43181 = LINE ( 'NONE', #36013, #39944 ) ;
#43182 = CARTESIAN_POINT ( 'NONE',  ( -1.002407869896990045, 0.1264236179284866091, 1.523129921206078707 ) ) ;
#43183 = EDGE_LOOP ( 'NONE', ( #12012, #10351, #957, #18642 ) ) ;
#43184 = CARTESIAN_POINT ( 'NONE',  ( 0.8107537697050234415, -0.1574803149606297803, 0.1550196850393702197 ) ) ;
#43185 = CARTESIAN_POINT ( 'NONE',  ( 0.8759842519685039353, 0.1787899950787401882, 1.218011810969858111 ) ) ;
#43186 = VERTEX_POINT ( 'NONE', #45453 ) ;
#43187 = CARTESIAN_POINT ( 'NONE',  ( 0.9500414927467378812, -0.1787899950787401604, 1.786417322780882388 ) ) ;
#43188 = CARTESIAN_POINT ( 'NONE',  ( -0.9873396505805591694, 0.1113553986120547346, 0.5659448818897637734 ) ) ;
#43189 = CARTESIAN_POINT ( 'NONE',  ( -0.9500414927467378812, 0.1787899950787401604, 0.9744094487651340231 ) ) ;
#43190 = CARTESIAN_POINT ( 'NONE',  ( -0.9412147342319837628, 0.1574803149606300301, 0.5191929132782994172 ) ) ;
#43191 = CARTESIAN_POINT ( 'NONE',  ( -0.7081935964228096569, -0.04031566679114802210, 0.03937007874015843040 ) ) ;
#43192 = CARTESIAN_POINT ( 'NONE',  ( 0.6971942568897626646, -0.07405724077823297447, 0.2460629920722207653 ) ) ;
#43193 = CARTESIAN_POINT ( 'NONE',  ( -0.8019270111902716547, -0.1787899950787401604, 0.2066929133320631329 ) ) ;
#43194 = PRODUCT_DEFINITION_CONTEXT ( 'detailed design', #27872, 'design' ) ;
#43195 = CARTESIAN_POINT ( 'NONE',  ( -0.6971942568897637749, 2.189545951927499583E-17, 0.5930118109698583329 ) ) ;
#43196 = CARTESIAN_POINT ( 'NONE',  ( 0.7646288533564489232, 0.1113553986120547346, 1.589566929026330566 ) ) ;
#43197 = EDGE_LOOP ( 'NONE', ( #22492, #46502, #1302, #24596 ) ) ;
#43198 = ( BOUNDED_CURVE ( )  B_SPLINE_CURVE ( 2, ( #26077, #40425, #29712, #1124, #14820, #7608, #40890, #8083, #174 ),
 .UNSPECIFIED., .F., .T. ) 
 B_SPLINE_CURVE_WITH_KNOTS ( ( 3, 2, 2, 2, 3 ),
 ( 0.02999999999999999889, 0.03250000000000000111, 0.03500000000000000333, 0.03749999999999999861, 0.04000000000000000083 ),
 .UNSPECIFIED. ) 
 CURVE ( )  GEOMETRIC_REPRESENTATION_ITEM ( )  RATIONAL_B_SPLINE_CURVE ( ( 1.000000000000000000, 0.9238795325112869605, 1.000000000000000000, 0.9238795325112869605, 1.000000000000000000, 0.9238795325112869605, 1.000000000000000000, 0.9238795325112869605, 1.000000000000000000 ) ) 
 REPRESENTATION_ITEM ( '' )  ) ;
#43199 = CARTESIAN_POINT ( 'NONE',  ( -0.1787899950787401604, -0.007874015694267974541, -0.07405724077823318263 ) ) ;
#43200 = CARTESIAN_POINT ( 'NONE',  ( 1.002407869896990045, 0.1264236179284866091, 0.8193897637257637756 ) ) ;
#43201 = CARTESIAN_POINT ( 'NONE',  ( -0.6971942568897648851, -0.07405724077823297447, 1.815944881835999780 ) ) ;
#43202 = CARTESIAN_POINT ( 'NONE',  ( -0.2471922904502826812, 0.09842519685039370636, 5.914624404477007554E-17 ) ) ;
#43203 = CARTESIAN_POINT ( 'NONE',  ( -0.2066929133858267931, -0.5192708129487060287, -0.8938220056861537755 ) ) ;
#43204 = CARTESIAN_POINT ( 'NONE',  ( -0.1787899950787401604, -1.352486172953647925, 0.07405724077823318263 ) ) ;
#43205 = VERTEX_POINT ( 'NONE', #31124 ) ;
#43206 = CARTESIAN_POINT ( 'NONE',  ( 0.1787899950787401604, -0.2194881889226144023, 0.07405724077823318263 ) ) ;
#43207 = EDGE_CURVE ( 'NONE', #31965, #30756, #43265, .T. ) ;
#43208 = EDGE_CURVE ( 'NONE', #22098, #23237, #9298, .T. ) ;
#43209 = CARTESIAN_POINT ( 'NONE',  ( -0.4330708661417322913, 0.1864803149606299448, 1.186023622047243986 ) ) ;
#43210 = EDGE_CURVE ( 'NONE', #2629, #41717, #16722, .T. ) ;
#43211 = VERTEX_POINT ( 'NONE', #20306 ) ;
#43212 = CARTESIAN_POINT ( 'NONE',  ( 0.8019270111902717657, 0.1787899950787401604, 1.058070866087969186 ) ) ;
#43213 = CARTESIAN_POINT ( 'NONE',  ( 0.4736248074375818407, 1.488499961090669288, -0.3513258257898456138 ) ) ;
#43214 = CARTESIAN_POINT ( 'NONE',  ( -0.2471922466704931376, -0.08138981793828348188, 0.07067796049273157577 ) ) ;
#43215 = EDGE_CURVE ( 'NONE', #21269, #9918, #12909, .T. ) ;
#43216 = CARTESIAN_POINT ( 'NONE',  ( 0.8759842519685039353, 0.1574803149606299191, 1.909448818897637956 ) ) ;
#43217 = AXIS2_PLACEMENT_3D ( 'NONE', #30000, #40941, #8136 ) ;
#43218 = AXIS2_PLACEMENT_3D ( 'NONE', #2086, #31585, #27776 ) ;
#43219 = CIRCLE ( 'NONE', #36390, 0.09842519685039370636 ) ;
#43220 = CARTESIAN_POINT ( 'NONE',  ( 0.1787899950787401882, -1.442421259788756016, -2.189545951927503898E-17 ) ) ;
#43221 = CARTESIAN_POINT ( 'NONE',  ( -0.1787899950787401882, -0.7928149605761574126, 0.000000000000000000 ) ) ;
#43222 = B_SPLINE_CURVE_WITH_KNOTS ( 'NONE', 3,
 ( #17606, #16683, #31310, #46364, #13544, #45888, #13100, #28180, #31548, #20497, #46126, #4162, #11379, #25990, #40571, #18785, #3702, #44404, #32729, #43469, #21685, #36316, #47321, #12092, #37720, #26239, #37959, #19732, #18137, #35594, #34900, #42980, #24796, #23861, #6574, #31302, #16900, #31540, #14490, #7518, #6806, #3696, #40102, #22139, #3925, #18319, #7756, #10668, #14975, #29149, #11372, #25983, #32957, #22374, #21426, #17600, #14260, #7296, #32243, #28902, #25276, #21916, #43463, #39864, #21679, #79, #38877, #35310, #28352, #38651, #5826, #2447, #31009, #46062, #31245, #17075, #9896, #6277, #46301, #13492, #42461, #20192, #27434, #34595, #41975, #28123, #1745, #39104, #9431, #27668, #45822, #42922, #9183, #20434, #5335, #9666, #23798, #24509, #31949, #19955, #46535, #10134, #38415, #5586, #35068, #24282, #13032, #32904, #29091, #11088, #35770, #2911, #28607, #17785, #6754, #21376, #14203, #5470, #27319, #16509, #15153, #30671, #38542, #25931, #33378, #45231, #16279, #12455, #1871, #34963, #16737, #45468, #5706, #7939, #41868, #1631 ),
 .UNSPECIFIED., .F., .F.,
 ( 4, 2, 2, 1, 1, 2, 2, 2, 2, 2, 1, 2, 2, 2, 2, 1, 2, 2, 2, 2, 2, 1, 1, 1, 2, 2, 2, 2, 2, 1, 1, 2, 2, 2, 2, 2, 1, 1, 1, 2, 2, 2, 2, 2, 1, 1, 1, 1, 2, 2, 2, 2, 2, 1, 1, 1, 2, 2, 2, 2, 1, 1, 1, 2, 2, 2, 2, 1, 1, 1, 1, 2, 2, 2, 2, 2, 2, 2, 2, 2, 4 ),
 ( 0.000000000000000000, 0.03125000000001836725, 0.04687500000002754741, 0.05468750000003212708, 0.05859375000003467365, 0.06054687500003567979, 0.06250000000003667899, 0.1250000000000644484, 0.1562500000000783540, 0.1718750000000852929, 0.1796875000000887623, 0.1835937500000907330, 0.1875000000000926759, 0.2187500000001105782, 0.2343750000001197653, 0.2421875000001245670, 0.2460937500001267597, 0.2500000000001290079, 0.3125000000001651457, 0.3437500000001831868, 0.3593750000001922351, 0.3671875000001968425, 0.3710937500001991185, 0.3730468750002002842, 0.3740234375002007838, 0.3750000000002012834, 0.4062500000002193801, 0.4218750000002284839, 0.4296875000002330913, 0.4335937500002354228, 0.4355468750002366995, 0.4365234375002373657, 0.4375000000002380318, 0.4687500000002480238, 0.4843750000002531308, 0.4921875000002556844, 0.4960937500002569611, 0.4980468750002575162, 0.4990234375002578493, 0.4995117187502580158, 0.5000000000002581269, 0.5625000000002646772, 0.5937500000002678968, 0.6093750000002693401, 0.6171875000002700062, 0.6210937500002703393, 0.6230468750002706724, 0.6240234375002710054, 0.6245117187502710054, 0.6250000000002711165, 0.6562500000002340350, 0.6718750000002152722, 0.6796875000002060574, 0.6835937500002017275, 0.6855468750001995071, 0.6865234375001983969, 0.6870117187501978417, 0.6875000000001972866, 0.7187500000001568745, 0.7343750000001364464, 0.7421875000001262324, 0.7460937500001215694, 0.7480468750001187939, 0.7490234375001173506, 0.7500000000001159073, 0.7812500000000520695, 0.7968750000000202061, 0.8046875000000038858, 0.8085937499999957812, 0.8105468749999913403, 0.8115234374999894529, 0.8120117187499882316, 0.8124999999999868994, 0.8437499999999894529, 0.8593749999999904521, 0.8671874999999908962, 0.8710937499999911182, 0.8749999999999912292, 0.9062499999999934497, 0.9374999999999955591, 1.000000000000000000 ),
 .UNSPECIFIED. ) ;
#43223 = ADVANCED_FACE ( 'NONE', ( #46174 ), #11925, .F. ) ;
#43224 = CARTESIAN_POINT ( 'NONE',  ( -0.6971942568897648851, -0.07405724077823297447, 0.4822834645131655606 ) ) ;
#43225 = CARTESIAN_POINT ( 'NONE',  ( 3.301370929368692659E-17, -1.290398140291706630, 0.1797182628040039365 ) ) ;
#43226 = CARTESIAN_POINT ( 'NONE',  ( 0.4142125984251969206, 3.008340040661385896E-17, 0.000000000000000000 ) ) ;
#43227 = CARTESIAN_POINT ( 'NONE',  ( 1.054774247047244096, 0.000000000000000000, 1.168799212544661348 ) ) ;
#43228 = CARTESIAN_POINT ( 'NONE',  ( 0.6971942568897637749, 2.189545951927499583E-17, 1.498523621993480326 ) ) ;
#43229 = CARTESIAN_POINT ( 'NONE',  ( -0.9873396505805591694, 0.1113553986120547346, 0.5954724408373543998 ) ) ;
#43230 = CARTESIAN_POINT ( 'NONE',  ( 0.8759842519685039353, 0.1574803149606299191, 1.712598425196850238 ) ) ;
#43231 = LINE ( 'NONE', #39395, #37847 ) ;
#43233 = CYLINDRICAL_SURFACE ( 'NONE', #4755, 0.02900000000000048025 ) ;
#43232 = CARTESIAN_POINT ( 'NONE',  ( 0.2395294000716133853, -0.1968503937007874127, -1.181102362204724310 ) ) ;
#43234 = CARTESIAN_POINT ( 'NONE',  ( 0.9412147342319837628, -0.1574803149606297803, 1.449311023514519681 ) ) ;
#43235 = DIRECTION ( 'NONE',  ( -1.000000000000000000, 0.000000000000000000, 0.000000000000000000 ) ) ;
#43236 = CARTESIAN_POINT ( 'NONE',  ( -0.8107537697050253289, 0.1574803149606300301, 1.744586614065703145 ) ) ;
#43237 = CARTESIAN_POINT ( 'NONE',  ( 0.1264236179284866091, -0.01525590545804753929, -0.1264236179284866091 ) ) ;
#43238 = CARTESIAN_POINT ( 'NONE',  ( 0.6971942568897626646, 0.07405724077823318263, 0.1181102361667090567 ) ) ;
#43239 = CARTESIAN_POINT ( 'NONE',  ( 0.7117210317037124812, -0.04900334798748854498, 0.03937011140070836857 ) ) ;
#43241 = CARTESIAN_POINT ( 'NONE',  ( -0.8107537697050254399, 0.1574803149606300301, 1.823326771546017078 ) ) ;
#43240 = CARTESIAN_POINT ( 'NONE',  ( 0.8019270111902716547, -0.1787899950787401604, 1.112204724355684959 ) ) ;
#43242 = DIRECTION ( 'NONE',  ( 0.000000000000000000, 0.000000000000000000, 1.000000000000000000 ) ) ;
#43243 = CARTESIAN_POINT ( 'NONE',  ( -0.8019270111902717657, 0.1787899950787401604, 1.136811023568283119 ) ) ;
#43244 = CARTESIAN_POINT ( 'NONE',  ( 0.8759842519685039353, 0.1574803149606299191, 0.4822834644594015674 ) ) ;
#43245 = ORIENTED_EDGE ( 'NONE', *, *, #13686, .F. ) ;
#43246 = DIRECTION ( 'NONE',  ( 1.000000000000000000, 0.000000000000000000, 0.000000000000000000 ) ) ;
#43247 = CARTESIAN_POINT ( 'NONE',  ( 0.9873396505805591694, -0.1113553986120547346, 0.2805118110236220486 ) ) ;
#43248 = PRODUCT_DEFINITION_SHAPE ( 'NONE', 'NONE',  #11944 ) ;
#43249 = CARTESIAN_POINT ( 'NONE',  ( -0.9412147342319837628, -0.1574803149606297803, 0.3863188975302684902 ) ) ;
#43250 = VERTEX_POINT ( 'NONE', #27540 ) ;
#43251 = CARTESIAN_POINT ( 'NONE',  ( 0.7495606340400177148, 0.1264236179284866091, 1.454232283410803017 ) ) ;
#43252 = AXIS2_PLACEMENT_3D ( 'NONE', #1885, #39012, #9799 ) ;
#43253 = DIRECTION ( 'NONE',  ( 0.000000000000000000, 1.000000000000000000, 0.000000000000000000 ) ) ;
#43254 = CARTESIAN_POINT ( 'NONE',  ( -0.6971942568897626646, -0.07405724077823297447, 0.04429133852891373180 ) ) ;
#43255 = CARTESIAN_POINT ( 'NONE',  ( 0.1264236179284866091, -0.02509842514308689362, 0.1264236179284866091 ) ) ;
#43256 = VERTEX_POINT ( 'NONE', #8811 ) ;
#43257 = DIRECTION ( 'NONE',  ( 1.000000000000000000, 0.000000000000000000, -1.822029033848725275E-16 ) ) ;
#43258 = ORIENTED_EDGE ( 'NONE', *, *, #41313, .T. ) ;
#43259 = CARTESIAN_POINT ( 'NONE',  ( 1.033464566929133799, 0.000000000000000000, 1.299212598317669221 ) ) ;
#43260 = PRESENTATION_STYLE_ASSIGNMENT (( #36342 ) ) ;
#43261 = CARTESIAN_POINT ( 'NONE',  ( 1.054774247047244540, 0.07405724077823318263, 0.6200787401037165525 ) ) ;
#43262 = EDGE_LOOP ( 'NONE', ( #7566, #7621, #5632, #42903 ) ) ;
#43263 = CARTESIAN_POINT ( 'NONE',  ( 0.07405724077823318263, -1.789370078686394194, -0.1787899950787401604 ) ) ;
#43264 = CARTESIAN_POINT ( 'NONE',  ( -1.054774247047244540, -0.07405724077823318263, 1.087598425143086578 ) ) ;
#43265 = CIRCLE ( 'NONE', #32597, 0.2952755905511806334 ) ;
#43266 = AXIS2_PLACEMENT_3D ( 'NONE', #37560, #12174, #26798 ) ;
#43267 = CARTESIAN_POINT ( 'NONE',  ( -0.7646288533564489232, 0.1113553986120547346, 0.1820866141732283561 ) ) ;
#43268 = VERTEX_POINT ( 'NONE', #13585 ) ;
#43269 = EDGE_CURVE ( 'NONE', #20097, #25251, #5696, .T. ) ;
#43270 = CARTESIAN_POINT ( 'NONE',  ( -1.002407869896990045, -0.1264236179284866091, 1.080216535379306952 ) ) ;
#43271 = CARTESIAN_POINT ( 'NONE',  ( -0.7495606340400177148, -0.1264236179284866091, 0.8390748030958424808 ) ) ;
#43272 = CARTESIAN_POINT ( 'NONE',  ( -1.054774247047244540, 0.07405724077823318263, 0.2263779527021421711 ) ) ;
#43273 = CARTESIAN_POINT ( 'NONE',  ( -0.1574803149606299191, -0.4410959923581754816, -0.9673892061308019263 ) ) ;
#43274 = FACE_OUTER_BOUND ( 'NONE', #44660, .T. ) ;
#43275 = CARTESIAN_POINT ( 'NONE',  ( 0.1264236179284866091, -0.7791594013001044150, -0.1264236179284866091 ) ) ;
#43276 = ORIENTED_EDGE ( 'NONE', *, *, #33416, .T. ) ;
#43277 = CARTESIAN_POINT ( 'NONE',  ( 0.05390907504427756153, -0.08956249738940257055, 0.1385839714854027738 ) ) ;
#43278 = CARTESIAN_POINT ( 'NONE',  ( -0.02421810057410377776, -0.08754923116810497952, 0.1560975693771988193 ) ) ;
#43279 = ORIENTED_EDGE ( 'NONE', *, *, #13405, .F. ) ;
#43280 = EDGE_CURVE ( 'NONE', #8074, #26592, #2093, .T. ) ;
#43281 = ORIENTED_EDGE ( 'NONE', *, *, #10473, .T. ) ;
#43282 = CARTESIAN_POINT ( 'NONE',  ( -1.033464566929134687, -0.06523048226347956391, 1.739665354330709235 ) ) ;
#43283 = CARTESIAN_POINT ( 'NONE',  ( 0.8759842519685039353, 0.000000000000000000, 4.498031496062992574 ) ) ;
#43284 = CARTESIAN_POINT ( 'NONE',  ( -0.8759842519685039353, -0.1787899950787401882, 0.6422244093950550958 ) ) ;
#43285 = CARTESIAN_POINT ( 'NONE',  ( -7.957671378281915615E-17, -8.878505979408855953E-16, -0.3937007874015748254 ) ) ;
#43286 = EDGE_LOOP ( 'NONE', ( #42124, #43096, #42322, #15831, #2252 ) ) ;
#43287 = CARTESIAN_POINT ( 'NONE',  ( -1.054774247047244540, -0.07405724077823318263, 1.756889763725764553 ) ) ;
#43288 = CARTESIAN_POINT ( 'NONE',  ( 0.03901279071809810040, -0.09842519685039370636, 1.713085361781125471 ) ) ;
#43289 = PRESENTATION_STYLE_ASSIGNMENT (( #6629 ) ) ;
#43290 = CARTESIAN_POINT ( 'NONE',  ( 0.7646288533564489232, 0.1113553986120547346, 0.6545275590551181688 ) ) ;
#43291 = CARTESIAN_POINT ( 'NONE',  ( -0.1797182628040039087, -0.7908902662759585978, -0.07444174185955065859 ) ) ;
#43292 = DIRECTION ( 'NONE',  ( 0.000000000000000000, 0.000000000000000000, -1.000000000000000000 ) ) ;
#43293 = CARTESIAN_POINT ( 'NONE',  ( -0.8759842519685039353, -0.1574803149606299191, 1.368110236112944911 ) ) ;
#43294 = CARTESIAN_POINT ( 'NONE',  ( 1.002407869896990045, 0.1264236179284866091, 0.7406496062454487328 ) ) ;
#43295 = CARTESIAN_POINT ( 'NONE',  ( 0.06523048226347956391, -0.5664370078740157410, 0.1574803149606297803 ) ) ;
#43296 = CARTESIAN_POINT ( 'NONE',  ( -0.08791145637253013068, 0.1224054518956866344, -0.1337190540265945915 ) ) ;
#43297 = ORIENTED_EDGE ( 'NONE', *, *, #26538, .F. ) ;
#43298 = CARTESIAN_POINT ( 'NONE',  ( 0.1574803149606299191, 0.5288907983920094757, -0.7507079620615707549 ) ) ;
#43299 = CARTESIAN_POINT ( 'NONE',  ( 0.9873396505805591694, 0.1113553986120547346, 1.313976377952756014 ) ) ;
#43300 = CARTESIAN_POINT ( 'NONE',  ( 0.8296574145072385109, -0.1668241634633925718, 1.987349479867523749 ) ) ;
#43301 = CARTESIAN_POINT ( 'NONE',  ( 0.8107537697050254399, -0.1574803149606297803, 1.729822834645670548 ) ) ;
#43303 = CARTESIAN_POINT ( 'NONE',  ( 0.3547871005709968273, 4.766607801171850497E-17, 0.000000000000000000 ) ) ;
#43302 = CARTESIAN_POINT ( 'NONE',  ( 0.8759842519685039353, -0.1787899950787401882, 0.6422244093950550958 ) ) ;
#43304 = ORIENTED_EDGE ( 'NONE', *, *, #4975, .F. ) ;
#43305 = CARTESIAN_POINT ( 'NONE',  ( 0.2471922904502826812, -0.09842519685039370636, -0.1427165354330708902 ) ) ;
#43306 = CARTESIAN_POINT ( 'NONE',  ( -0.2066929133858267931, -0.9875035750853327077, -1.463737590216208861 ) ) ;
#43307 = CARTESIAN_POINT ( 'NONE',  ( 0.8019270111902717657, -0.1787899950787401604, 0.9940944881352130613 ) ) ;
#43308 = CARTESIAN_POINT ( 'NONE',  ( 0.06801279071811515420, 0.3740157480314961203, 1.224299699984020551 ) ) ;
#43309 = DIRECTION ( 'NONE',  ( 0.000000000000000000, 0.000000000000000000, -1.000000000000000000 ) ) ;
#43310 = CARTESIAN_POINT ( 'NONE',  ( 0.1270800023317771588, 0.1023183951413639964, -0.1270800023317771588 ) ) ;
#43311 = CARTESIAN_POINT ( 'NONE',  ( 0.1787899950787401882, -1.166830708607653477, -2.189545951927503898E-17 ) ) ;
#43312 = CARTESIAN_POINT ( 'NONE',  ( 2.892866454678787531E-17, -1.513779527559055094, 0.1574803149606299191 ) ) ;
#43313 = DIRECTION ( 'NONE',  ( -8.890457814381144247E-15, 0.000000000000000000, 1.000000000000000000 ) ) ;
#43314 = ORIENTED_EDGE ( 'NONE', *, *, #33957, .F. ) ;
#43315 = CARTESIAN_POINT ( 'NONE',  ( -1.002407869896990045, 0.1264236179284866091, 0.1451771653005673179 ) ) ;
#43316 = ORIENTED_EDGE ( 'NONE', *, *, #46727, .T. ) ;
#43317 = CARTESIAN_POINT ( 'NONE',  ( 0.5057057357416000487, 4.766607801171850497E-17, 0.000000000000000000 ) ) ;
#43318 = ORIENTED_EDGE ( 'NONE', *, *, #19902, .T. ) ;
#43319 = CARTESIAN_POINT ( 'NONE',  ( -0.1113553986120547346, -1.400590551073574774, -0.1113553986120547346 ) ) ;
#43320 = CARTESIAN_POINT ( 'NONE',  ( 0.3000685424736224127, -3.032960542342102697E-32, 0.09842519685039370636 ) ) ;
#43321 = CARTESIAN_POINT ( 'NONE',  ( -0.8759842519685039353, 0.1787899950787401882, 1.488681102308440751 ) ) ;
#43322 = AXIS2_PLACEMENT_3D ( 'NONE', #4317, #18950, #36709 ) ;
#43323 = CARTESIAN_POINT ( 'NONE',  ( 1.054774247047244096, 0.000000000000000000, 0.8144685038832440993 ) ) ;
#43324 = EDGE_CURVE ( 'NONE', #18699, #28934, #46343, .T. ) ;
#43325 = CARTESIAN_POINT ( 'NONE',  ( -1.054774247047244540, 0.07405724077823318263, 0.8120078739619844832 ) ) ;
#43326 = CARTESIAN_POINT ( 'NONE',  ( -0.6971942568897626646, 0.07405724077823318263, 0.3986220471903312301 ) ) ;
#43327 = EDGE_CURVE ( 'NONE', #16549, #35433, #41065, .T. ) ;
#43328 = CARTESIAN_POINT ( 'NONE',  ( -0.2471922904502827090, 0.09255273792768342611, 0.04108768875596389286 ) ) ;
#43329 = CARTESIAN_POINT ( 'NONE',  ( -0.6971942568897648851, -0.07405724077823297447, 1.820866141678520789 ) ) ;
#43330 = CARTESIAN_POINT ( 'NONE',  ( -0.7646288533564489232, -0.1113553986120547346, 1.963582677165354395 ) ) ;
#43331 = DIRECTION ( 'NONE',  ( 0.000000000000000000, -1.000000000000000000, 0.000000000000000000 ) ) ;
#43332 = CARTESIAN_POINT ( 'NONE',  ( 3.284318927891251994E-17, -0.4395924721662464729, 0.1787899950787401882 ) ) ;
#43333 = CARTESIAN_POINT ( 'NONE',  ( -0.09634625429846278843, -0.09842519685039370636, -0.1571995980677732274 ) ) ;
#43334 = DIRECTION ( 'NONE',  ( -1.000000000000000000, 0.000000000000000000, 0.000000000000000000 ) ) ;
#43335 = DIRECTION ( 'NONE',  ( 0.000000000000000000, 0.000000000000000000, 1.000000000000000000 ) ) ;
#43336 = EDGE_CURVE ( 'NONE', #39913, #9031, #15016, .T. ) ;
#43337 = ADVANCED_FACE ( 'NONE', ( #3269 ), #10487, .F. ) ;
#43338 = CARTESIAN_POINT ( 'NONE',  ( -0.7495606340400177148, 0.1264236179284866091, 0.1156496062454492185 ) ) ;
#43339 = ORIENTED_EDGE ( 'NONE', *, *, #18645, .T. ) ;
#43340 = CARTESIAN_POINT ( 'NONE',  ( -0.9500414927467377701, 0.1787899950787401604, 1.373031496009229357 ) ) ;
#43341 = ORIENTED_EDGE ( 'NONE', *, *, #1611, .F. ) ;
#43342 = CARTESIAN_POINT ( 'NONE',  ( -0.1787899950787401604, -1.228346456639149542, -0.07405724077823318263 ) ) ;
#43343 = CARTESIAN_POINT ( 'NONE',  ( 0.1264236179284866091, -1.393208661363559031, -0.1264236179284866091 ) ) ;
#43344 = CARTESIAN_POINT ( 'NONE',  ( -0.7646288533564489232, 0.1113553986120547346, 1.550196850286173156 ) ) ;
#43345 = CARTESIAN_POINT ( 'NONE',  ( -1.033464566929133799, 0.000000000000000000, 1.387795275590551158 ) ) ;
#43346 = CARTESIAN_POINT ( 'NONE',  ( -1.033464566929133799, 0.000000000000000000, 0.9448818896562519720 ) ) ;
#43347 = CARTESIAN_POINT ( 'NONE',  ( -0.8107537697050253289, 0.1574803149606300301, 0.7701771653543306728 ) ) ;
#43348 = CARTESIAN_POINT ( 'NONE',  ( 2.892866454678787531E-17, -0.09645669291338582196, 0.1574803149606299191 ) ) ;
#43349 = CARTESIAN_POINT ( 'NONE',  ( 0.7185039370078739607, 1.928577636452523993E-17, 1.870078740049952559 ) ) ;
#43350 = VERTEX_POINT ( 'NONE', #13829 ) ;
#43351 = CARTESIAN_POINT ( 'NONE',  ( -0.07874015748031489015, 0.3740157480314960647, 0.9783464566929127582 ) ) ;
#43352 = CARTESIAN_POINT ( 'NONE',  ( 0.9412147342319837628, 0.1574803149606300301, 0.8439960629921254842 ) ) ;
#43353 = DIRECTION ( 'NONE',  ( 0.000000000000000000, -1.000000000000000000, 0.000000000000000000 ) ) ;
#43355 = LINE ( 'NONE', #42860, #39934 ) ;
#43354 = CARTESIAN_POINT ( 'NONE',  ( -0.9412147342319837628, -0.1574803149606297803, 0.4749015748031497064 ) ) ;
#43356 = CARTESIAN_POINT ( 'NONE',  ( 0.7185039370078746268, -0.06523048226347956391, 0.2583661416247562959 ) ) ;
#43357 = VERTEX_POINT ( 'NONE', #29851 ) ;
#43358 = ORIENTED_EDGE ( 'NONE', *, *, #21423, .T. ) ;
#43359 = FACE_OUTER_BOUND ( 'NONE', #7900, .T. ) ;
#43360 = CARTESIAN_POINT ( 'NONE',  ( 0.1574803149606300301, -1.491633858160189785, -0.06523048226347956391 ) ) ;
#43361 = CARTESIAN_POINT ( 'NONE',  ( -0.1787899950787401604, -0.5147637794737950356, 0.07405724077823318263 ) ) ;
#43362 = CARTESIAN_POINT ( 'NONE',  ( 0.1574803149606300301, -1.029035433070865535, -0.06523048226347956391 ) ) ;
#43363 = CARTESIAN_POINT ( 'NONE',  ( 0.9412147342319837628, 0.1574803149606300301, 0.9128937006798734100 ) ) ;
#43364 = CARTESIAN_POINT ( 'NONE',  ( 0.4509871776442260227, 4.466152701071653354E-17, 0.000000000000000000 ) ) ;
#43365 = CARTESIAN_POINT ( 'NONE',  ( -0.9500414927467378812, -0.1787899950787401604, 0.4478346456155276045 ) ) ;
#43366 = EDGE_LOOP ( 'NONE', ( #11195, #1160, #36898, #45082 ) ) ;
#43367 = CARTESIAN_POINT ( 'NONE',  ( -1.054774247047244096, 0.000000000000000000, 1.601870078686393750 ) ) ;
#43368 = ORIENTED_EDGE ( 'NONE', *, *, #38210, .F. ) ;
#43369 = CARTESIAN_POINT ( 'NONE',  ( 0.8759842519685039353, 0.1787899950787401882, 1.611712598371433103 ) ) ;
#43370 = ORIENTED_EDGE ( 'NONE', *, *, #14669, .F. ) ;
#43371 = CARTESIAN_POINT ( 'NONE',  ( -0.6971942568897626646, 0.07405724077823318263, 0.7529527558517473684 ) ) ;
#43372 = CARTESIAN_POINT ( 'NONE',  ( 1.054774247047244540, 0.07405724077823318263, 0.2263779527021421711 ) ) ;
#43373 = DIRECTION ( 'NONE',  ( 1.000000000000000000, 0.000000000000000000, 0.000000000000000000 ) ) ;
#43374 = CARTESIAN_POINT ( 'NONE',  ( 1.054774247047244096, 0.000000000000000000, 0.7750984251430865779 ) ) ;
#43375 = CARTESIAN_POINT ( 'NONE',  ( -1.054774247047244540, -0.07405724077823318263, 0.6496062991588353874 ) ) ;
#43376 = AXIS2_PLACEMENT_3D ( 'NONE', #4589, #1003, #44848 ) ;
#43377 = CARTESIAN_POINT ( 'NONE',  ( 0.06523048226347956391, -0.08415354319955967166, 0.1574803149606297803 ) ) ;
#43378 = EDGE_CURVE ( 'NONE', #33536, #27280, #5816, .T. ) ;
#43379 = DIRECTION ( 'NONE',  ( 1.822029033848725028E-16, 0.000000000000000000, 1.000000000000000000 ) ) ;
#43380 = CARTESIAN_POINT ( 'NONE',  ( -0.1113553986120547346, -0.1702755904436539236, 0.1113553986120547346 ) ) ;
#43381 = CARTESIAN_POINT ( 'NONE',  ( -0.8759842519685039353, 0.1787899950787401882, 1.454232283410803017 ) ) ;
#43382 = CARTESIAN_POINT ( 'NONE',  ( -0.8759842519685039353, 0.1574803149606299191, 0.4527559055118110520 ) ) ;
#43383 = CARTESIAN_POINT ( 'NONE',  ( 0.7495606340400177148, -0.1264236179284866091, 1.390255905458047447 ) ) ;
#43384 = DIRECTION ( 'NONE',  ( 0.000000000000000000, 0.000000000000000000, 1.000000000000000000 ) ) ;
#43385 = ORIENTED_EDGE ( 'NONE', *, *, #38508, .T. ) ;
#43386 = EDGE_CURVE ( 'NONE', #34618, #21958, #21482, .T. ) ;
#43387 = CARTESIAN_POINT ( 'NONE',  ( -1.094772975963752103E-17, -1.758490109961521775, -0.1787899950787401882 ) ) ;
#43388 = ORIENTED_EDGE ( 'NONE', *, *, #31097, .F. ) ;
#43389 = DIRECTION ( 'NONE',  ( 0.000000000000000000, 0.000000000000000000, -1.000000000000000000 ) ) ;
#43390 = ORIENTED_EDGE ( 'NONE', *, *, #2894, .T. ) ;
#43391 = CARTESIAN_POINT ( 'NONE',  ( -0.3980944881889726394, 1.194414586609142237, -0.06082000038405787484 ) ) ;
#43392 = CARTESIAN_POINT ( 'NONE',  ( 0.1264236179284866091, -0.9699803149068660924, 0.1264236179284866091 ) ) ;
#43393 = FACE_OUTER_BOUND ( 'NONE', #24029, .T. ) ;
#43394 = CARTESIAN_POINT ( 'NONE',  ( -0.8070866141732283561, -0.3937007874015746034, -0.7574803149606299524 ) ) ;
#43395 = CARTESIAN_POINT ( 'NONE',  ( 0.6971942568897626646, 0.07405724077823318263, 0.3149606298674962890 ) ) ;
#43396 = B_SPLINE_CURVE_WITH_KNOTS ( 'NONE', 3,
 ( #37185, #3884, #40755, #737, #3653, #281, #43661, #33391, #44132, #26187, #33622, #14926, #36497, #11330, #25942, #37 ),
 .UNSPECIFIED., .F., .F.,
 ( 4, 2, 2, 2, 2, 2, 2, 4 ),
 ( 0.000000000000000000, 0.1250000000000263956, 0.1875000000000336675, 0.2187500000000319467, 0.2500000000000301981, 0.3750000000000279776, 0.5000000000000257572, 1.000000000000000000 ),
 .UNSPECIFIED. ) ;
#43397 = CARTESIAN_POINT ( 'NONE',  ( -0.1787899950787401882, -0.1344743619300261817, 0.000000000000000000 ) ) ;
#43398 = CARTESIAN_POINT ( 'NONE',  ( -0.07405724077823318263, -0.3080708660879689087, 0.1787899950787401604 ) ) ;
#43399 = CARTESIAN_POINT ( 'NONE',  ( -0.1787899950787401882, -0.005413385773008132923, 0.000000000000000000 ) ) ;
#43400 = CARTESIAN_POINT ( 'NONE',  ( 0.2471920410536352364, -0.09140649424452929050, -0.04498895533762308635 ) ) ;
#43401 = CARTESIAN_POINT ( 'NONE',  ( 1.002407869896990045, 0.1264236179284866091, 0.6569881889226141247 ) ) ;
#43402 = EDGE_CURVE ( 'NONE', #10631, #16808, #33431, .T. ) ;
#43403 = CIRCLE ( 'NONE', #22008, 0.09842519685039310962 ) ;
#43404 = CARTESIAN_POINT ( 'NONE',  ( -0.9500414927467377701, 0.1787899950787401604, 0.9399606298674970661 ) ) ;
#43405 = CARTESIAN_POINT ( 'NONE',  ( -0.2066929133858267931, 0.09445121742700231249, -0.1242805304366906144 ) ) ;
#43406 = CARTESIAN_POINT ( 'NONE',  ( 0.1270800023317771588, -1.679177667850761724, 0.1270800023317771588 ) ) ;
#43407 = CARTESIAN_POINT ( 'NONE',  ( 0.1574803149606299746, -0.4872761608334559846, -0.8688576204587790119 ) ) ;
#43408 = CARTESIAN_POINT ( 'NONE',  ( 0.6971942568897648851, 0.07405724077823318263, 1.658464566875369472 ) ) ;
#43410 = CARTESIAN_POINT ( 'NONE',  ( -0.7185039370078739607, 0.000000000000000000, -2.869337061179095023E-17 ) ) ;
#43409 = CARTESIAN_POINT ( 'NONE',  ( 0.7185039370078739607, 0.000000000000000000, 4.498031496062992574 ) ) ;
#43411 = ORIENTED_EDGE ( 'NONE', *, *, #7036, .T. ) ;
#43412 = CARTESIAN_POINT ( 'NONE',  ( 0.8759842519685039353, 0.1574803149606299191, 0.01968503937007873988 ) ) ;
#43413 = DIRECTION ( 'NONE',  ( -1.000000000000000000, 0.000000000000000000, 0.000000000000000000 ) ) ;
#43414 = CARTESIAN_POINT ( 'NONE',  ( 0.7185039370078766252, -0.06523048226348168721, 1.321358267609009207 ) ) ;
#43415 = CARTESIAN_POINT ( 'NONE',  ( -0.1574803149606300301, -0.9256889762704257896, -0.06523048226347956391 ) ) ;
#43416 = CARTESIAN_POINT ( 'NONE',  ( -1.002407869896990045, 0.1264236179284866091, 0.4256889763241890057 ) ) ;
#43417 = CARTESIAN_POINT ( 'NONE',  ( 0.7495606340400177148, -0.1264236179284866091, 0.6766732282926929409 ) ) ;
#43418 = CARTESIAN_POINT ( 'NONE',  ( -0.1787899950787401882, -1.024114173174582643, 0.000000000000000000 ) ) ;
#43419 = CARTESIAN_POINT ( 'NONE',  ( 1.054774247047244540, -0.07405724077823318263, 0.1427165353793072855 ) ) ;
#43420 = DIRECTION ( 'NONE',  ( 0.000000000000000000, 0.000000000000000000, 1.000000000000000000 ) ) ;
#43421 = CARTESIAN_POINT ( 'NONE',  ( -0.8759842519685039353, 0.1787899950787401882, 1.646161417269070837 ) ) ;
#43422 = VERTEX_POINT ( 'NONE', #15201 ) ;
#43423 = CARTESIAN_POINT ( 'NONE',  ( 0.7646288533564489232, -0.1113553986120547346, 0.4281496062992125595 ) ) ;
#43424 = CARTESIAN_POINT ( 'NONE',  ( 0.7495606340400177148, 0.1264236179284866091, 1.222933070812378009 ) ) ;
#43425 = CARTESIAN_POINT ( 'NONE',  ( -0.8759842519685039353, -0.1574803149606299191, 0.6988188975302678241 ) ) ;
#43426 = CARTESIAN_POINT ( 'NONE',  ( -1.033464566929133799, 0.000000000000000000, 1.496062992018456494 ) ) ;
#43427 = CARTESIAN_POINT ( 'NONE',  ( 1.054774247047244540, 0.07405724077823318263, 1.796259842465923073 ) ) ;
#43428 = CARTESIAN_POINT ( 'NONE',  ( -0.8759842519685039353, 0.1574803149606299191, 0.5708661417322835607 ) ) ;
#43429 = CARTESIAN_POINT ( 'NONE',  ( -1.054774247047244096, 0.000000000000000000, 0.8489173227808819444 ) ) ;
#43430 = CARTESIAN_POINT ( 'NONE',  ( 0.4330708661417322913, -0.08090551181102362266, 0.000000000000000000 ) ) ;
#43431 = CARTESIAN_POINT ( 'NONE',  ( -0.08080321177267317523, -0.2488424761940687957, -0.03960523631939861372 ) ) ;
#43432 = CARTESIAN_POINT ( 'NONE',  ( 1.054774247047244540, -0.07405724077823318263, 0.2608267715997797387 ) ) ;
#43433 = CARTESIAN_POINT ( 'NONE',  ( -0.6971942568897626646, -0.07405724077823297447, 0.2805118109698587214 ) ) ;
#43434 = CARTESIAN_POINT ( 'NONE',  ( -0.8759842519685039353, 0.1787899950787401882, 0.7012795275052913224 ) ) ;
#43435 = CARTESIAN_POINT ( 'NONE',  ( 0.7185039370078746268, -0.06523048226347956391, 1.636318897530269156 ) ) ;
#43436 = EDGE_LOOP ( 'NONE', ( #14160, #15048, #30228, #42205 ) ) ;
#43437 = EDGE_CURVE ( 'NONE', #43073, #33230, #3446, .T. ) ;
#43438 = CONICAL_SURFACE ( 'NONE', #42660, 0.2431102362204724532, 0.4367866272367255109 ) ;
#43439 = CARTESIAN_POINT ( 'NONE',  ( -0.1787899950787401882, -0.005413385773008132923, 0.000000000000000000 ) ) ;
#43440 = ORIENTED_EDGE ( 'NONE', *, *, #45641, .T. ) ;
#43441 = ORIENTED_EDGE ( 'NONE', *, *, #23762, .F. ) ;
#43442 = CARTESIAN_POINT ( 'NONE',  ( 0.8759842519685039353, -0.1787899950787401882, 0.7652559054580472253 ) ) ;
#43443 = CARTESIAN_POINT ( 'NONE',  ( 1.002407869896990045, -0.1264236179284866091, 1.045767716481669440 ) ) ;
#43444 = CARTESIAN_POINT ( 'NONE',  ( -0.9500414927467377701, 0.1787899950787401604, 1.879921259788756016 ) ) ;
#43445 = EDGE_CURVE ( 'NONE', #14468, #44045, #37743, .T. ) ;
#43446 = CARTESIAN_POINT ( 'NONE',  ( 0.6971942568897637749, 2.189545951927499583E-17, 1.970964566875370139 ) ) ;
#43447 = AXIS2_PLACEMENT_3D ( 'NONE', #38906, #6067, #2711 ) ;
#43448 = CARTESIAN_POINT ( 'NONE',  ( 1.033464566929133799, 0.000000000000000000, 1.614173228238929170 ) ) ;
#43449 = CARTESIAN_POINT ( 'NONE',  ( 0.1787899950787401604, -1.254060976103255065, -0.07405724077823318263 ) ) ;
#43450 = VERTEX_POINT ( 'NONE', #36115 ) ;
#43451 = CARTESIAN_POINT ( 'NONE',  ( -0.1787899950787401882, -0.2760826771115909573, 0.000000000000000000 ) ) ;
#43452 = ORIENTED_EDGE ( 'NONE', *, *, #1193, .T. ) ;
#43453 = CYLINDRICAL_SURFACE ( 'NONE', #326, 0.1968503937007874127 ) ;
#43454 = CARTESIAN_POINT ( 'NONE',  ( 0.7185039370078739607, 1.928577636452523993E-17, 1.397637795168062969 ) ) ;
#43455 = ( BOUNDED_CURVE ( )  B_SPLINE_CURVE ( 2, ( #45890, #35605, #16912, #9728, #27959, #9961, #1815, #38483, #28186 ),
 .UNSPECIFIED., .F., .T. ) 
 B_SPLINE_CURVE_WITH_KNOTS ( ( 3, 2, 2, 2, 3 ),
 ( 0.3300000000000000155, 0.3325000000000000178, 0.3350000000000000200, 0.3375000000000000222, 0.3400000000000000244 ),
 .UNSPECIFIED. ) 
 CURVE ( )  GEOMETRIC_REPRESENTATION_ITEM ( )  RATIONAL_B_SPLINE_CURVE ( ( 1.000000000000000000, 0.9238795325112869605, 1.000000000000000000, 0.9238795325112869605, 1.000000000000000000, 0.9238795325112869605, 1.000000000000000000, 0.9238795325112869605, 1.000000000000000000 ) ) 
 REPRESENTATION_ITEM ( '' )  ) ;
#43456 = CARTESIAN_POINT ( 'NONE',  ( 0.6971942568897637749, 2.189545951927499583E-17, 0.08120078734781142893 ) ) ;
#43457 = CARTESIAN_POINT ( 'NONE',  ( -0.1264236179284866091, -1.575295275536787276, 0.1264236179284866091 ) ) ;
#43458 = CARTESIAN_POINT ( 'NONE',  ( -0.1787899950787401604, -0.7509842519147402751, 0.07405724077823318263 ) ) ;
#43459 = CARTESIAN_POINT ( 'NONE',  ( -1.054774247047244540, 0.07405724077823318263, 0.4232283464029293896 ) ) ;
#43460 = VECTOR ( 'NONE', #23937, 39.37007874015748143 ) ;
#43461 = DIRECTION ( 'NONE',  ( 0.000000000000000000, -1.000000000000000000, 0.000000000000000000 ) ) ;
#43463 = CARTESIAN_POINT ( 'NONE',  ( -0.7219032811190957410, -0.06759513565020623671, 1.984564416229634309 ) ) ;
#43462 = CARTESIAN_POINT ( 'NONE',  ( -0.1270800023317771588, -1.255949321394068674, 0.1270800023317771588 ) ) ;
#43464 = DIRECTION ( 'NONE',  ( -1.000000000000000000, 0.000000000000000000, 0.000000000000000000 ) ) ;
#43465 = CARTESIAN_POINT ( 'NONE',  ( 0.8019270111902717657, 0.1787899950787401604, 1.181102362150960428 ) ) ;
#43466 = CARTESIAN_POINT ( 'NONE',  ( 1.002407869896990045, 0.1264236179284866091, 1.483759842465921075 ) ) ;
#43467 = CARTESIAN_POINT ( 'NONE',  ( -0.7185039370078739607, 1.928577636452523993E-17, 0.6496062991050708391 ) ) ;
#43469 = CARTESIAN_POINT ( 'NONE',  ( -0.7653144731331090744, 0.1177361346232950190, 1.980714588250390706 ) ) ;
#43468 = CARTESIAN_POINT ( 'NONE',  ( 0.1377952755905512139, 0.1564960629921262614, 0.7066929133858274037 ) ) ;
#43470 = CARTESIAN_POINT ( 'NONE',  ( -0.1574803149606299191, 0.000000000000000000, -0.04012007874015743186 ) ) ;
#43471 = CARTESIAN_POINT ( 'NONE',  ( -0.7185039370078746268, -0.06523048226347956391, 1.675688976270425679 ) ) ;
#43472 = AXIS2_PLACEMENT_3D ( 'NONE', #42827, #23963, #17230 ) ;
#43474 = ( BOUNDED_CURVE ( )  B_SPLINE_CURVE ( 2, ( #45851, #20218, #13058, #6546, #24076, #17100, #42706, #28383, #38685 ),
 .UNSPECIFIED., .F., .F. ) 
 B_SPLINE_CURVE_WITH_KNOTS ( ( 3, 2, 2, 2, 3 ),
 ( 0.8900000000000000133, 0.8924999999999999600, 0.8950000000000000178, 0.8974999999999999645, 0.9000000000000000222 ),
 .UNSPECIFIED. ) 
 CURVE ( )  GEOMETRIC_REPRESENTATION_ITEM ( )  RATIONAL_B_SPLINE_CURVE ( ( 1.000000000000000000, 0.9238795325112899581, 1.000000000000000000, 0.9238795325112869605, 1.000000000000000000, 0.9238795325112869605, 1.000000000000000000, 0.9238795325112869605, 1.000000000000000000 ) ) 
 REPRESENTATION_ITEM ( '' )  ) ;
#43473 = CARTESIAN_POINT ( 'NONE',  ( 0.8759842519685039353, -0.1787899950787401882, 0.09104330703285078152 ) ) ;
#43476 = DIRECTION ( 'NONE',  ( -1.000000000000000000, -0.000000000000000000, 0.000000000000000000 ) ) ;
#43475 = CARTESIAN_POINT ( 'NONE',  ( 0.6971942568897648851, 0.07405724077823318263, 1.102362204670646495 ) ) ;
#43477 = CARTESIAN_POINT ( 'NONE',  ( -0.7495606340400177148, -0.1264236179284866091, 1.227854330654897685 ) ) ;
#43478 = CARTESIAN_POINT ( 'NONE',  ( 0.9412147342319837628, 0.1574803149606300301, 0.4798228345381422844 ) ) ;
#43479 = ORIENTED_EDGE ( 'NONE', *, *, #28615, .T. ) ;
#43480 = ADVANCED_FACE ( 'NONE', ( #32541 ), #34916, .F. ) ;
#43481 = CARTESIAN_POINT ( 'NONE',  ( -1.033464566929133799, 1.928577636452533546E-17, 4.498031496062992574 ) ) ;
#43482 = CARTESIAN_POINT ( 'NONE',  ( 0.9716762863782174575, 0.1379795071755416380, 0.03936908659436527680 ) ) ;
#43483 = CARTESIAN_POINT ( 'NONE',  ( 0.8759842519685039353, 0.1574803149606299191, 0.2559055118110236116 ) ) ;
#43484 = CARTESIAN_POINT ( 'NONE',  ( -0.9873396505805591694, 0.1113553986120547346, 0.4773622046168818911 ) ) ;
#43485 = ORIENTED_EDGE ( 'NONE', *, *, #7844, .T. ) ;
#43486 = CARTESIAN_POINT ( 'NONE',  ( 0.7495606340400177148, -0.1264236179284866091, 1.385334645615527549 ) ) ;
#43487 = CARTESIAN_POINT ( 'NONE',  ( -1.033464566929134687, -0.06523048226347956391, 1.149114173228346969 ) ) ;
#43489 = CARTESIAN_POINT ( 'NONE',  ( -0.1574803149606299191, 0.05639690512153988644, -0.1570009270184609673 ) ) ;
#43488 = CARTESIAN_POINT ( 'NONE',  ( -1.181102362204724310, -0.3937007874015748254, -0.9842519685039370358 ) ) ;
#43490 = CARTESIAN_POINT ( 'NONE',  ( -1.094772975963752103E-17, -0.01033464561552785432, -0.1787899950787401882 ) ) ;
#43491 = ORIENTED_EDGE ( 'NONE', *, *, #39049, .T. ) ;
#43492 = CARTESIAN_POINT ( 'NONE',  ( 0.7185039370078739607, 1.928577636452523993E-17, 0.4527559054042842868 ) ) ;
#43493 = EDGE_CURVE ( 'NONE', #40831, #32649, #44820, .T. ) ;
#43494 = ORIENTED_EDGE ( 'NONE', *, *, #13405, .T. ) ;
#43495 = CARTESIAN_POINT ( 'NONE',  ( 0.2064293380533964994, 0.06762482675899135487, 0.1662510369723770864 ) ) ;
#43496 = CARTESIAN_POINT ( 'NONE',  ( 0.1564674760228476069, -0.09340956239926176408, -0.1950964973271320235 ) ) ;
#43497 = ORIENTED_EDGE ( 'NONE', *, *, #23617, .T. ) ;
#43498 = ORIENTED_EDGE ( 'NONE', *, *, #16570, .F. ) ;
#43499 = CARTESIAN_POINT ( 'NONE',  ( 0.06523048226347956391, 0.1126968505012277688, 0.1574803149606297803 ) ) ;
#43500 = CARTESIAN_POINT ( 'NONE',  ( -1.054774247047244540, 0.07405724077823318263, 1.092519684985605810 ) ) ;
#43501 = CARTESIAN_POINT ( 'NONE',  ( -0.9873396505805591694, 0.1113553986120547346, 0.2116141732283464416 ) ) ;
#43502 = CARTESIAN_POINT ( 'NONE',  ( -0.7495606340400177148, 0.1264236179284866091, 1.099901574749385880 ) ) ;
#43503 = CARTESIAN_POINT ( 'NONE',  ( -0.8759842519685039353, -0.1787899950787401882, 0.8046259841982047467 ) ) ;
#43504 = ADVANCED_FACE ( 'NONE', ( #17895 ), #42786, .T. ) ;
#43505 = AXIS2_PLACEMENT_3D ( 'NONE', #34665, #34908, #31082 ) ;
#43506 = CARTESIAN_POINT ( 'NONE',  ( -0.8019270111902717657, 0.1787899950787401604, 0.2362204723871814960 ) ) ;
#43507 = FACE_OUTER_BOUND ( 'NONE', #3263, .T. ) ;
#43508 = CARTESIAN_POINT ( 'NONE',  ( -0.1787899950787401882, -0.8431357792528602069, 0.000000000000000000 ) ) ;
#43509 = VERTEX_POINT ( 'NONE', #35649 ) ;
#43510 = CARTESIAN_POINT ( 'NONE',  ( 0.06711304729538268565, -0.08956252386023248746, 0.1311275629080100313 ) ) ;
#43511 = CARTESIAN_POINT ( 'NONE',  ( -0.7646288533564489232, -0.1113553986120547346, 0.8513779526483780113 ) ) ;
#43512 = CIRCLE ( 'NONE', #23653, 0.03937007874015748671 ) ;
#43513 = EDGE_LOOP ( 'NONE', ( #26204, #2730, #43491, #8931 ) ) ;
#43514 = DIRECTION ( 'NONE',  ( 0.000000000000000000, 0.000000000000000000, 1.000000000000000000 ) ) ;
#43515 = DIRECTION ( 'NONE',  ( 0.000000000000000000, 0.000000000000000000, -1.000000000000000000 ) ) ;
#43516 = AXIS2_PLACEMENT_3D ( 'NONE', #18866, #44491, #29716 ) ;
#43517 = CARTESIAN_POINT ( 'NONE',  ( -0.8019270111902717657, -0.1787899950787401604, 0.7972440944344250102 ) ) ;
#43518 = EDGE_LOOP ( 'NONE', ( #5777, #21006, #16516, #45393, #34986 ) ) ;
#43519 = CARTESIAN_POINT ( 'NONE',  ( -0.8107537697050254399, -0.1574803149606297803, 1.129429133750740277 ) ) ;
#43520 = CARTESIAN_POINT ( 'NONE',  ( -1.002407869896990045, 0.1264236179284866091, 0.1107283464029293202 ) ) ;
#43521 = CARTESIAN_POINT ( 'NONE',  ( -0.1797182628040039087, -0.8647091639137531871, 0.07444174185955065859 ) ) ;
#43522 = CARTESIAN_POINT ( 'NONE',  ( 0.08471839801908884193, -0.2465807710536996322, -0.3122165016188270803 ) ) ;
#43523 = CARTESIAN_POINT ( 'NONE',  ( -0.7185039370078746268, -0.06523048226347956391, 1.439468503829481216 ) ) ;
#43524 = CARTESIAN_POINT ( 'NONE',  ( 0.6971942568897637749, 2.189545951927499583E-17, 0.7554133857730077617 ) ) ;
#43525 = CARTESIAN_POINT ( 'NONE',  ( 0.1574803149606300301, -0.5172244094488184230, -0.06523048226347956391 ) ) ;
#43526 = CARTESIAN_POINT ( 'NONE',  ( -0.1634885253152291440, 0.1261140749709542819, -0.008880672301011263703 ) ) ;
#43527 = ORIENTED_EDGE ( 'NONE', *, *, #32939, .T. ) ;
#43528 = DIRECTION ( 'NONE',  ( -0.000000000000000000, 0.000000000000000000, -1.000000000000000000 ) ) ;
#43529 = CARTESIAN_POINT ( 'NONE',  ( 0.8107537697050253289, 0.1574803149606300301, 1.242618110236220819 ) ) ;
#43531 = CARTESIAN_POINT ( 'NONE',  ( -0.4620708661417322616, 0.9842519685039375910, -0.7135826771653542844 ) ) ;
#43530 = CARTESIAN_POINT ( 'NONE',  ( 0.8777546437831791337, -0.1746983550445412314, 1.988227210017399882 ) ) ;
#43532 = CARTESIAN_POINT ( 'NONE',  ( 0.000000000000000000, 0.000000000000000000, 0.000000000000000000 ) ) ;
#43534 = FACE_BOUND ( 'NONE', #9526, .T. ) ;
#43533 = CARTESIAN_POINT ( 'NONE',  ( 0.7495606340400177148, -0.1264236179284866091, 0.7160433070328504623 ) ) ;
#43535 = VECTOR ( 'NONE', #13500, 39.37007874015748143 ) ;
#43536 = CARTESIAN_POINT ( 'NONE',  ( 0.1264236179284866091, -0.6451771653005667906, -0.1264236179284866091 ) ) ;
#43537 = DIRECTION ( 'NONE',  ( -0.000000000000000000, 0.7880107536067184615, -0.6156614753256628436 ) ) ;
#43538 = ORIENTED_EDGE ( 'NONE', *, *, #17583, .T. ) ;
#43539 = AXIS2_PLACEMENT_3D ( 'NONE', #26476, #26715, #8235 ) ;
#43540 = EDGE_CURVE ( 'NONE', #31291, #2480, #6628, .T. ) ;
#43541 = CARTESIAN_POINT ( 'NONE',  ( 1.033464566929133799, 0.000000000000000000, 0.6299212597349921339 ) ) ;
#43542 = DIRECTION ( 'NONE',  ( 1.000000000000000000, 0.000000000000000000, 0.000000000000000000 ) ) ;
#43543 = CARTESIAN_POINT ( 'NONE',  ( 0.9500414927467378812, 0.1787899950787401604, 0.9350393700249758355 ) ) ;
#43544 = DIRECTION ( 'NONE',  ( -1.000000000000000000, 0.000000000000000000, 0.000000000000000000 ) ) ;
#43545 = CARTESIAN_POINT ( 'NONE',  ( 0.1787899950787401604, -1.164370078686393306, -0.07405724077823318263 ) ) ;
#43547 = AXIS2_PLACEMENT_3D ( 'NONE', #42499, #9937, #2719 ) ;
#43546 = CARTESIAN_POINT ( 'NONE',  ( -0.06523048226347956391, -1.531003937007875182, -0.1574803149606300301 ) ) ;
#43548 = CARTESIAN_POINT ( 'NONE',  ( -0.1586641775163213364, 0.9382165298418959631, -1.070508272602717303 ) ) ;
#43549 = CARTESIAN_POINT ( 'NONE',  ( -1.054774247047244540, 0.07405724077823318263, 0.1033464566391498751 ) ) ;
#43550 = ORIENTED_EDGE ( 'NONE', *, *, #31519, .T. ) ;
#43551 = VECTOR ( 'NONE', #17001, 39.37007874015748143 ) ;
#43552 = CARTESIAN_POINT ( 'NONE',  ( 0.9500414927467378812, 0.1787899950787401604, 1.963582677111591401 ) ) ;
#43553 = ORIENTED_EDGE ( 'NONE', *, *, #10849, .F. ) ;
#43554 = CARTESIAN_POINT ( 'NONE',  ( 0.1787899950787401604, -1.405511810969858999, 0.07405724077823318263 ) ) ;
#43555 = CARTESIAN_POINT ( 'NONE',  ( -0.8759842519685039353, 0.1787899950787401882, 1.966043307032850462 ) ) ;
#43556 = CARTESIAN_POINT ( 'NONE',  ( -0.7495606340400177148, 0.1264236179284866091, 1.690452755851748146 ) ) ;
#43557 = EDGE_CURVE ( 'NONE', #32653, #18221, #46007, .T. ) ;
#43558 = CARTESIAN_POINT ( 'NONE',  ( -0.9500414927467378812, 0.1787899950787401604, 0.3887795275052913224 ) ) ;
#43559 = LINE ( 'NONE', #46681, #26814 ) ;
#43560 = CARTESIAN_POINT ( 'NONE',  ( -1.054774247047244540, -0.07405724077823318263, 1.993110236166711013 ) ) ;
#43561 = FACE_OUTER_BOUND ( 'NONE', #41338, .T. ) ;
#43562 = CARTESIAN_POINT ( 'NONE',  ( -0.8107537697050253289, -0.1574803149606297803, 1.847933070866143002 ) ) ;
#43563 = CARTESIAN_POINT ( 'NONE',  ( 0.1787899950787401882, -0.4691200312213645862, -2.189545951927503898E-17 ) ) ;
#43564 = CARTESIAN_POINT ( 'NONE',  ( -0.09424215950663268615, -0.09842519685039370636, 0.1330654084077543264 ) ) ;
#43565 = LINE ( 'NONE', #10536, #30279 ) ;
#43566 = DIRECTION ( 'NONE',  ( -1.000000000000000000, 0.000000000000000000, 0.000000000000000000 ) ) ;
#43567 = CARTESIAN_POINT ( 'NONE',  ( -1.054774247047244096, 0.000000000000000000, 0.1796259841982051075 ) ) ;
#43568 = VECTOR ( 'NONE', #22798, 39.37007874015748143 ) ;
#43569 = ORIENTED_EDGE ( 'NONE', *, *, #26274, .F. ) ;
#43570 = CARTESIAN_POINT ( 'NONE',  ( -1.002407869896990045, -0.1264236179284866091, 1.400098425143086800 ) ) ;
#43571 = ORIENTED_EDGE ( 'NONE', *, *, #37940, .T. ) ;
#43572 = CARTESIAN_POINT ( 'NONE',  ( -0.1264236179284866091, -1.230807086560409269, -0.1264236179284866091 ) ) ;
#43573 = AXIS2_PLACEMENT_3D ( 'NONE', #30295, #26677, #41226 ) ;
#43574 = CARTESIAN_POINT ( 'NONE',  ( 0.1787899950787401604, -1.395669291284819868, -0.07405724077823318263 ) ) ;
#43575 = DIRECTION ( 'NONE',  ( 1.000000000000000000, 0.000000000000000000, -0.000000000000000000 ) ) ;
#43576 = CARTESIAN_POINT ( 'NONE',  ( 1.001134792037362109, 0.9202755905601576192, 0.3161444924770078768 ) ) ;
#43577 = CARTESIAN_POINT ( 'NONE',  ( -1.100456976456230270E-17, -0.6014217623389507272, -0.1797182628040039365 ) ) ;
#43578 = FACE_OUTER_BOUND ( 'NONE', #7101, .T. ) ;
#43579 = CARTESIAN_POINT ( 'NONE',  ( -0.8107537697050253289, 0.1574803149606300301, 0.8784448817822366751 ) ) ;
#43580 = AXIS2_PLACEMENT_3D ( 'NONE', #3726, #29188, #29661 ) ;
#43581 = CARTESIAN_POINT ( 'NONE',  ( 0.1113553986120547346, -0.1702755905511811052, 0.1113553986120547346 ) ) ;
#43582 = CARTESIAN_POINT ( 'NONE',  ( 0.8107537697050253289, 0.1574803149606300301, 1.744586614065703145 ) ) ;
#43583 = VERTEX_POINT ( 'NONE', #8457 ) ;
#43584 = EDGE_CURVE ( 'NONE', #14779, #34930, #2723, .T. ) ;
#43585 = LINE ( 'NONE', #6930, #36060 ) ;
#43586 = CARTESIAN_POINT ( 'NONE',  ( 0.8107537697050253289, 0.1574803149606300301, 0.7701771653543306728 ) ) ;
#43587 = CARTESIAN_POINT ( 'NONE',  ( 0.1667418150844881541, -0.1992258004382128633, -0.03573910814354441107 ) ) ;
#43588 = CARTESIAN_POINT ( 'NONE',  ( -0.8759842519685039353, -0.1574803149606299191, 1.604330708553889595 ) ) ;
#43589 = SHAPE_REPRESENTATION ( 'Handle Arm Left', ( #20860 ), #187 ) ;
#43590 = EDGE_CURVE ( 'NONE', #11388, #157, #17274, .T. ) ;
#43592 = DIRECTION ( 'NONE',  ( 0.000000000000000000, 0.000000000000000000, -1.000000000000000000 ) ) ;
#43591 = DIRECTION ( 'NONE',  ( 1.000000000000000000, 0.000000000000000000, 0.000000000000000000 ) ) ;
#43593 = CARTESIAN_POINT ( 'NONE',  ( 1.033464566929133799, 0.000000000000000000, 0.1181102361129454797 ) ) ;
#43594 = EDGE_CURVE ( 'NONE', #30476, #3019, #1492, .T. ) ;
#43595 = EDGE_CURVE ( 'NONE', #46242, #26440, #42605, .T. ) ;
#43596 = DIRECTION ( 'NONE',  ( 0.000000000000000000, 0.000000000000000000, -1.000000000000000000 ) ) ;
#43597 = CARTESIAN_POINT ( 'NONE',  ( -0.1113553986120547346, -1.558070866034206858, -0.1113553986120547346 ) ) ;
#43598 = CARTESIAN_POINT ( 'NONE',  ( 0.1787899950787401604, -0.7362204723871804690, 0.07405724077823318263 ) ) ;
#43599 = CARTESIAN_POINT ( 'NONE',  ( 0.000000000000000000, 0.000000000000000000, 0.000000000000000000 ) ) ;
#43600 = CARTESIAN_POINT ( 'NONE',  ( -0.1574803149606297803, -1.127460629921260837, 0.06523048226347956391 ) ) ;
#43601 = CARTESIAN_POINT ( 'NONE',  ( 0.8107537697050253289, -0.1574803149606297803, 0.8932086613097963701 ) ) ;
#43602 = DIRECTION ( 'NONE',  ( 0.000000000000000000, -1.000000000000000000, 0.000000000000000000 ) ) ;
#43603 = VECTOR ( 'NONE', #45191, 39.37007874015748143 ) ;
#43604 = CARTESIAN_POINT ( 'NONE',  ( -0.8759842519685039353, 0.1787899950787401882, 0.4256889763241890057 ) ) ;
#43605 = VERTEX_POINT ( 'NONE', #19948 ) ;
#43606 = ORIENTED_EDGE ( 'NONE', *, *, #33052, .T. ) ;
#43607 = CARTESIAN_POINT ( 'NONE',  ( -0.6971942568897648851, -0.07405724077823297447, 1.584645669237574994 ) ) ;
#43608 = CARTESIAN_POINT ( 'NONE',  ( 0.8019270111902717657, 0.1787899950787401604, 1.496062992072220821 ) ) ;
#43609 = VERTEX_POINT ( 'NONE', #41491 ) ;
#43610 = CARTESIAN_POINT ( 'NONE',  ( -1.002407869896990045, -0.1264236179284866091, 0.8489173227808819444 ) ) ;
#43611 = LINE ( 'NONE', #10821, #35802 ) ;
#43612 = CARTESIAN_POINT ( 'NONE',  ( 0.6971942568897648851, -0.07405724077823297447, 0.7185039369541108556 ) ) ;
#43613 = CARTESIAN_POINT ( 'NONE',  ( -0.7495606340400177148, -0.1264236179284866091, 0.7554133857730077617 ) ) ;
#43614 = AXIS2_PLACEMENT_3D ( 'NONE', #40484, #19166, #943 ) ;
#43615 = CARTESIAN_POINT ( 'NONE',  ( 2.892866454678787531E-17, -0.08661417312081949593, 0.1574803149606299191 ) ) ;
#43616 = FACE_OUTER_BOUND ( 'NONE', #43970, .T. ) ;
#43617 = CARTESIAN_POINT ( 'NONE',  ( -9.642888182262618425E-18, -0.2637795274515279398, -0.1574803149606299191 ) ) ;
#43618 = CARTESIAN_POINT ( 'NONE',  ( -0.8759842519685039353, 0.1574803149606299191, 1.899606299105070839 ) ) ;
#43619 = ORIENTED_EDGE ( 'NONE', *, *, #44664, .F. ) ;
#43620 = CARTESIAN_POINT ( 'NONE',  ( -0.1476377952755905387, -0.4889725119976394141, -0.8550419489141689589 ) ) ;
#43621 = CARTESIAN_POINT ( 'NONE',  ( -0.7185039370078746268, 0.06523048226347956391, 1.483759842519686067 ) ) ;
#43622 = CARTESIAN_POINT ( 'NONE',  ( -0.7646288533564489232, 0.1113553986120547346, 0.4183070866141732624 ) ) ;
#43623 = CARTESIAN_POINT ( 'NONE',  ( 1.054774247047244096, 0.000000000000000000, 1.483759842465921075 ) ) ;
#43624 = CARTESIAN_POINT ( 'NONE',  ( 0.1101484706250415307, -0.09851384295070100827, -0.1631889973867482468 ) ) ;
#43625 = CARTESIAN_POINT ( 'NONE',  ( -0.8759842519685039353, 0.000000000000000000, 0.000000000000000000 ) ) ;
#43626 = ORIENTED_EDGE ( 'NONE', *, *, #38750, .T. ) ;
#43627 = CARTESIAN_POINT ( 'NONE',  ( 0.1787899950787401604, -1.692053102087505811, 0.07405724077823318263 ) ) ;
#43628 = EDGE_LOOP ( 'NONE', ( #23595, #11686, #3831, #39617 ) ) ;
#43629 = SHAPE_REPRESENTATION_RELATIONSHIP ( 'NONE' , 'NONE' ,  #30762, #27401 ) ;
#43630 = VERTEX_POINT ( 'NONE', #8697 ) ;
#43631 = CARTESIAN_POINT ( 'NONE',  ( -0.8759842519685039353, 0.000000000000000000, 0.000000000000000000 ) ) ;
#43632 = CARTESIAN_POINT ( 'NONE',  ( 3.284318927891251994E-17, -0.3892716534895436786, 0.1787899950787401882 ) ) ;
#43633 = CARTESIAN_POINT ( 'NONE',  ( 0.1264236179284866091, -0.9306102361667086820, 0.1264236179284866091 ) ) ;
#43634 = CONICAL_SURFACE ( 'NONE', #46709, 0.08090551181102362266, 0.9599310885968742602 ) ;
#43635 = CARTESIAN_POINT ( 'NONE',  ( 0.7185039370078746268, 0.06523048226347956391, 1.050688976377951889 ) ) ;
#43636 = CARTESIAN_POINT ( 'NONE',  ( 0.8759842519685039353, -0.1787899950787401882, 1.744586614119464807 ) ) ;
#43637 = CARTESIAN_POINT ( 'NONE',  ( 0.8759842519685039353, 0.1787899950787401882, 0.3469488188438744070 ) ) ;
#43638 = CARTESIAN_POINT ( 'NONE',  ( -1.100456976456230270E-17, -0.1289808174570614141, -0.1797182628040039365 ) ) ;
#43639 = CARTESIAN_POINT ( 'NONE',  ( -0.1264236179284866091, -0.1295531020875065054, 0.1264236179284866091 ) ) ;
#43641 = CIRCLE ( 'NONE', #29175, 0.1864803149606299448 ) ;
#43640 = CARTESIAN_POINT ( 'NONE',  ( 0.07405724077823318263, -0.2490157479777327099, -0.1787899950787401604 ) ) ;
#43642 = CARTESIAN_POINT ( 'NONE',  ( -0.1787899950787401604, -0.08169291333206318839, 0.07405724077823318263 ) ) ;
#43643 = CONTEXT_DEPENDENT_SHAPE_REPRESENTATION ( #30949, #37566 ) ;
#43644 = CARTESIAN_POINT ( 'NONE',  ( 0.2471886260749917852, -0.05069887331343050224, -0.1203475566266943436 ) ) ;
#43645 = CARTESIAN_POINT ( 'NONE',  ( 0.8019270111902717657, -0.1787899950787401604, 0.6003937007336380693 ) ) ;
#43646 = AXIS2_PLACEMENT_3D ( 'NONE', #30828, #42272, #23606 ) ;
#43647 = ADVANCED_FACE ( 'NONE', ( #33904 ), #16148, .T. ) ;
#43648 = DIRECTION ( 'NONE',  ( 1.000000000000000000, 0.000000000000000000, -1.822029033848725275E-16 ) ) ;
#43649 = CARTESIAN_POINT ( 'NONE',  ( 0.07444174185955065859, -1.681638297772022783, 0.1797182628040039087 ) ) ;
#43650 = CARTESIAN_POINT ( 'NONE',  ( 0.1574803149606299746, 0.3740157480314960647, 0.9783464566929134243 ) ) ;
#43651 = CARTESIAN_POINT ( 'NONE',  ( 0.7495606340400177148, -0.1264236179284866091, 1.705216535379307174 ) ) ;
#43653 = DIRECTION ( 'NONE',  ( 1.000000000000000000, 0.000000000000000000, 0.000000000000000000 ) ) ;
#43652 = LINE ( 'NONE', #43409, #38317 ) ;
#43654 = ADVANCED_FACE ( 'NONE', ( #15680 ), #23086, .T. ) ;
#43655 = VERTEX_POINT ( 'NONE', #37462 ) ;
#43656 = EDGE_CURVE ( 'NONE', #22098, #30017, #20362, .T. ) ;
#43657 = CARTESIAN_POINT ( 'NONE',  ( -0.1264236179284866091, -0.3154527558517483676, 0.1264236179284866091 ) ) ;
#43658 = CARTESIAN_POINT ( 'NONE',  ( 0.7185039370078737386, 0.06523048226348011902, 0.4896653542231809153 ) ) ;
#43659 = CARTESIAN_POINT ( 'NONE',  ( -0.1264236179284866091, -1.058562992072220377, 0.1264236179284866091 ) ) ;
#43660 = CARTESIAN_POINT ( 'NONE',  ( 1.002407869896990045, -0.1264236179284866091, 0.06151574797773248782 ) ) ;
#43661 = CARTESIAN_POINT ( 'NONE',  ( 0.1639941273279659495, 0.08071998019771058075, -0.1398093569819856552 ) ) ;
#43662 = CARTESIAN_POINT ( 'NONE',  ( -0.6971942568897648851, 0.07405724077823318263, 1.614173228292692386 ) ) ;
#43663 = EDGE_LOOP ( 'NONE', ( #29760, #249, #15580, #13200 ) ) ;
#43664 = CARTESIAN_POINT ( 'NONE',  ( -1.054774247047244540, 0.07405724077823318263, 1.131889763725763665 ) ) ;
#43665 = CARTESIAN_POINT ( 'NONE',  ( -0.2834275672170630811, -0.1259372798753285727, -0.7652988122780589597 ) ) ;
#43666 = CARTESIAN_POINT ( 'NONE',  ( 1.054774247047244540, 0.07405724077823318263, 1.835629921206078485 ) ) ;
#43667 = CARTESIAN_POINT ( 'NONE',  ( -1.033464566929133799, 0.000000000000000000, 0.6003937007874016185 ) ) ;
#43668 = CARTESIAN_POINT ( 'NONE',  ( -0.7495606340400177148, -0.1264236179284866091, 1.031003936954110189 ) ) ;
#43669 = DIRECTION ( 'NONE',  ( 1.000000000000000000, 0.000000000000000000, 0.000000000000000000 ) ) ;
#43670 = DIRECTION ( 'NONE',  ( -1.000000000000000000, 0.000000000000000000, 0.000000000000000000 ) ) ;
#43671 = CARTESIAN_POINT ( 'NONE',  ( 1.054774247047244540, -0.07405724077823318263, 0.3789370078202520253 ) ) ;
#43672 = CARTESIAN_POINT ( 'NONE',  ( -0.6971942568897626646, -0.07405724077823297447, 0.1624015747493861017 ) ) ;
#43673 = PRODUCT_DEFINITION_CONTEXT ( 'detailed design', #1504, 'design' ) ;
#43674 = CARTESIAN_POINT ( 'NONE',  ( -1.002407869896990045, 0.1264236179284866091, 0.6963582676627716461 ) ) ;
#43675 = CARTESIAN_POINT ( 'NONE',  ( 0.9873396505805591694, 0.1113553986120547346, 1.579724409341291214 ) ) ;
#43676 = ORIENTED_EDGE ( 'NONE', *, *, #6760, .F. ) ;
#43677 = AXIS2_PLACEMENT_3D ( 'NONE', #13549, #31085, #20959 ) ;
#43678 = CARTESIAN_POINT ( 'NONE',  ( -0.07405724077823318263, -0.05216535427694517224, -0.1787899950787401604 ) ) ;
#43679 = ORIENTED_EDGE ( 'NONE', *, *, #35575, .F. ) ;
#43680 = CARTESIAN_POINT ( 'NONE',  ( 0.8019270111902717657, 0.1787899950787401604, 0.8661417322297003674 ) ) ;
#43681 = CARTESIAN_POINT ( 'NONE',  ( 0.7495606340400177148, -0.1264236179284866091, 1.114665354276944909 ) ) ;
#43682 = CARTESIAN_POINT ( 'NONE',  ( -1.054774247047244540, 0.07405724077823318263, 1.914370078686394860 ) ) ;
#43683 = AXIS2_PLACEMENT_3D ( 'NONE', #17150, #38017, #46374 ) ;
#43684 = CARTESIAN_POINT ( 'NONE',  ( 0.7495606340400177148, 0.1264236179284866091, 1.887303149552535420 ) ) ;
#43685 = CIRCLE ( 'NONE', #7735, 0.2559055118110236116 ) ;
#43686 = EDGE_LOOP ( 'NONE', ( #23079, #9322, #15705, #8709 ) ) ;
#43687 = LINE ( 'NONE', #40083, #16043 ) ;
#43688 = CARTESIAN_POINT ( 'NONE',  ( 0.1787899950787401604, -1.377092472166246084, 0.07405724077823318263 ) ) ;
#43689 = ORIENTED_EDGE ( 'NONE', *, *, #582, .F. ) ;
#43690 = CARTESIAN_POINT ( 'NONE',  ( 0.07405724077823318263, -0.3031496062454492879, 0.1787899950787401604 ) ) ;
#43691 = CARTESIAN_POINT ( 'NONE',  ( -0.8107537697050254399, 0.1574803149606300301, 1.705216535325545069 ) ) ;
#43692 = VERTEX_POINT ( 'NONE', #12558 ) ;
#43693 = CARTESIAN_POINT ( 'NONE',  ( 1.054774247047244540, 0.07405724077823318263, 1.166338582623402509 ) ) ;
#43694 = CARTESIAN_POINT ( 'NONE',  ( -9.866766664128584110E-18, -0.1210185251470264484, -0.06598031696940066804 ) ) ;
#43695 = CARTESIAN_POINT ( 'NONE',  ( 0.7495606340400177148, 0.1264236179284866091, 1.493602362150960650 ) ) ;
#43696 = CARTESIAN_POINT ( 'NONE',  ( 1.054774247047244540, -0.07405724077823318263, 0.05905511805647267048 ) ) ;
#43697 = B_SPLINE_CURVE_WITH_KNOTS ( 'NONE', 3,
 ( #4672, #40380, #37760, #11898, #8275, #22902, #15972, #375, #37516, #25807, #33955, #29679, #19539 ),
 .UNSPECIFIED., .F., .F.,
 ( 4, 2, 2, 1, 2, 2, 4 ),
 ( 0.000000000000000000, 0.2500000000000000000, 0.3750000000000000000, 0.4374999999999998335, 0.4687499999999997780, 0.4999999999999997224, 1.000000000000000000 ),
 .UNSPECIFIED. ) ;
#43698 = CARTESIAN_POINT ( 'NONE',  ( -0.1264236179284866091, -1.585137795221826629, -0.1264236179284866091 ) ) ;
#43699 = CARTESIAN_POINT ( 'NONE',  ( 0.1264236179284866091, -1.639271653489543290, 0.1264236179284866091 ) ) ;
#43700 = EDGE_CURVE ( 'NONE', #44530, #30060, #44625, .T. ) ;
#43701 = AXIS2_PLACEMENT_3D ( 'NONE', #4992, #16275, #45463 ) ;
#43702 = CARTESIAN_POINT ( 'NONE',  ( -0.9500414927467377701, 0.1787899950787401604, 0.5462598424659214080 ) ) ;
#43703 = CARTESIAN_POINT ( 'NONE',  ( -0.9412147342319837628, 0.1574803149606300301, 0.6766732282389295028 ) ) ;
#43704 = CARTESIAN_POINT ( 'NONE',  ( -0.07444174185955065859, -1.307622549740526052, -0.1797182628040039087 ) ) ;
#43705 = CARTESIAN_POINT ( 'NONE',  ( -0.1184675242425147629, -0.09842519685039370636, 1.713085361781126803 ) ) ;
#43706 = B_SPLINE_CURVE_WITH_KNOTS ( 'NONE', 3,
 ( #20273, #2066, #5183, #13341, #19804, #27970, #9507, #34436, #31098, #45658, #12876, #30867, #27510, #45902, #13118, #24354, #1582, #34680, #42315, #23646, #9739 ),
 .UNSPECIFIED., .F., .F.,
 ( 4, 2, 1, 1, 2, 2, 2, 1, 1, 1, 2, 2, 4 ),
 ( 0.000000000000000000, 0.1249999999999996669, 0.1874999999999995004, 0.2187499999999994171, 0.2343749999999993894, 0.2499999999999993339, 0.3749999999999966693, 0.4374999999999952816, 0.4687499999999946709, 0.4843749999999945044, 0.4921874999999945044, 0.4999999999999945599, 1.000000000000000000 ),
 .UNSPECIFIED. ) ;
#43707 = CARTESIAN_POINT ( 'NONE',  ( 0.9500414927467378812, 0.1787899950787401604, 1.254921259788757348 ) ) ;
#43708 = CARTESIAN_POINT ( 'NONE',  ( 0.6971942568897637749, 2.189545951927499583E-17, 1.656003936954110412 ) ) ;
#43709 = AXIS2_PLACEMENT_3D ( 'NONE', #36819, #29681, #33009 ) ;
#43710 = CIRCLE ( 'NONE', #25377, 0.2559055118110236116 ) ;
#43711 = CARTESIAN_POINT ( 'NONE',  ( -0.7185039370078746268, 0.06523048226347956391, 1.916830708661418026 ) ) ;
#43712 = DIRECTION ( 'NONE',  ( 0.000000000000000000, 1.000000000000000000, 0.000000000000000000 ) ) ;
#43713 = AXIS2_PLACEMENT_3D ( 'NONE', #32554, #40163, #28479 ) ;
#43714 = CARTESIAN_POINT ( 'NONE',  ( 0.000000000000000000, 0.000000000000000000, -0.2610569382242185488 ) ) ;
#43715 = CARTESIAN_POINT ( 'NONE',  ( -1.033464566929133799, 0.000000000000000000, 1.771653543199558811 ) ) ;
#43716 = CARTESIAN_POINT ( 'NONE',  ( 0.8759842519685039353, 0.1787899950787401882, 0.1107283464029295283 ) ) ;
#43717 = CARTESIAN_POINT ( 'NONE',  ( 0.7092216557579411607, -0.04177231851234675108, 0.03937054267072845337 ) ) ;
#43718 = CARTESIAN_POINT ( 'NONE',  ( -0.7646288533564489232, 0.1113553986120547346, 1.953740157480315043 ) ) ;
#43719 = CARTESIAN_POINT ( 'NONE',  ( -0.7495606340400177148, 0.1264236179284866091, 1.178641732229700922 ) ) ;
#43720 = CARTESIAN_POINT ( 'NONE',  ( 0.9412147342319837628, 0.1574803149606300301, 0.5585629920184573827 ) ) ;
#43721 = ORIENTED_EDGE ( 'NONE', *, *, #9100, .T. ) ;
#43722 = FACE_OUTER_BOUND ( 'NONE', #8332, .T. ) ;
#43723 = CARTESIAN_POINT ( 'NONE',  ( 0.8687400033924506104, 0.1748083731305843380, 0.03936971248799488177 ) ) ;
#43724 = CARTESIAN_POINT ( 'NONE',  ( 0.8759842519685039353, 0.1574803149606299191, 0.8366141731208189825 ) ) ;
#43725 = CARTESIAN_POINT ( 'NONE',  ( -0.1574803149606297803, -1.038877952648378900, 0.06523048226347956391 ) ) ;
#43726 = CARTESIAN_POINT ( 'NONE',  ( -0.9412147342319837628, 0.1574803149606300301, 0.4404527557979849850 ) ) ;
#43727 = CARTESIAN_POINT ( 'NONE',  ( 0.002110188122406738646, 0.03198543007710048791, 0.1377961241629048206 ) ) ;
#43728 = CARTESIAN_POINT ( 'NONE',  ( 1.054774247047244540, -0.07405724077823318263, 1.397637795221827295 ) ) ;
#43729 = CARTESIAN_POINT ( 'NONE',  ( -0.8759842519685039353, -0.1574803149606299191, 1.092519684931842594 ) ) ;
#43731 = CARTESIAN_POINT ( 'NONE',  ( -0.7185039370078766252, -0.06523048226348168721, 1.370570866141733068 ) ) ;
#43730 = CARTESIAN_POINT ( 'NONE',  ( -0.9412147342319837628, 0.1574803149606300301, 0.09596456692913379882 ) ) ;
#43732 = CARTESIAN_POINT ( 'NONE',  ( -0.1264236179284866091, 0.004429133912031228346, 0.1264236179284866091 ) ) ;
#43733 = ORIENTED_EDGE ( 'NONE', *, *, #25714, .F. ) ;
#43734 = DIRECTION ( 'NONE',  ( -1.000000000000000000, 3.469446951953614189E-15, 1.144917494144692682E-16 ) ) ;
#43735 = ORIENTED_EDGE ( 'NONE', *, *, #966, .T. ) ;
#43736 = CARTESIAN_POINT ( 'NONE',  ( -0.8759842519685039353, 0.1574803149606299191, 0.3740157480314960647 ) ) ;
#43737 = DIRECTION ( 'NONE',  ( -1.000000000000000000, 0.000000000000000000, 0.000000000000000000 ) ) ;
#43738 = CARTESIAN_POINT ( 'NONE',  ( 0.8019270111902717657, -0.1787899950787401604, 0.6446850393163160442 ) ) ;
#43739 = ORIENTED_EDGE ( 'NONE', *, *, #42976, .T. ) ;
#43740 = CARTESIAN_POINT ( 'NONE',  ( 0.06523048226347956391, 0.08809055128862934569, -0.1574803149606300301 ) ) ;
#43741 = CARTESIAN_POINT ( 'NONE',  ( -0.8019270111902717657, 0.1787899950787401604, 1.141732283410804349 ) ) ;
#43742 = ORIENTED_EDGE ( 'NONE', *, *, #42616, .T. ) ;
#43743 = CARTESIAN_POINT ( 'NONE',  ( -0.9500414927467377701, -0.1787899950787401604, 1.117125984198203970 ) ) ;
#43744 = CARTESIAN_POINT ( 'NONE',  ( -1.002407869896990045, 0.1264236179284866091, 0.8587598424659212970 ) ) ;
#43745 = EDGE_CURVE ( 'NONE', #27408, #10456, #11838, .T. ) ;
#43746 = ( BOUNDED_CURVE ( )  B_SPLINE_CURVE ( 2, ( #4766, #15588, #22994, #16061, #29993, #44537, #22753, #19147, #33814 ),
 .UNSPECIFIED., .F., .T. ) 
 B_SPLINE_CURVE_WITH_KNOTS ( ( 3, 2, 2, 2, 3 ),
 ( 0.8299999999999999600, 0.8325000000000000178, 0.8349999999999999645, 0.8375000000000000222, 0.8399999999999999689 ),
 .UNSPECIFIED. ) 
 CURVE ( )  GEOMETRIC_REPRESENTATION_ITEM ( )  RATIONAL_B_SPLINE_CURVE ( ( 1.000000000000000000, 0.9238795325112899581, 1.000000000000000000, 0.9238795325112869605, 1.000000000000000000, 0.9238795325112869605, 1.000000000000000000, 0.9238795325112869605, 1.000000000000000000 ) ) 
 REPRESENTATION_ITEM ( '' )  ) ;
#43747 = AXIS2_PLACEMENT_3D ( 'NONE', #18023, #47258, #36487 ) ;
#43748 = CARTESIAN_POINT ( 'NONE',  ( -0.7495606340400177148, -0.1264236179284866091, 0.2485236219934806867 ) ) ;
#43749 = DIRECTION ( 'NONE',  ( 1.000000000000000000, 0.000000000000000000, -1.822029033848725275E-16 ) ) ;
#43750 = DIRECTION ( 'NONE',  ( 0.000000000000000000, 0.000000000000000000, 1.000000000000000000 ) ) ;
#43751 = CARTESIAN_POINT ( 'NONE',  ( 0.1264236179284866091, -0.8972696375205767572, -0.1264236179284866091 ) ) ;
#43752 = EDGE_LOOP ( 'NONE', ( #4130, #344, #1076, #27454 ) ) ;
#43753 = CARTESIAN_POINT ( 'NONE',  ( -0.1574803149606299191, -0.01771653532554381960, 0.000000000000000000 ) ) ;
#43754 = CARTESIAN_POINT ( 'NONE',  ( 0.7813541305413828075, 0.1521468885085573985, 0.03937552627153136087 ) ) ;
#43755 = ORIENTED_EDGE ( 'NONE', *, *, #41683, .F. ) ;
#43756 = CARTESIAN_POINT ( 'NONE',  ( -0.7646288533564489232, 0.1113553986120547346, 0.5659448817822370081 ) ) ;
#43757 = CARTESIAN_POINT ( 'NONE',  ( -0.8759842519685039353, 0.1787899950787401882, 0.7800196849856062542 ) ) ;
#43758 = CARTESIAN_POINT ( 'NONE',  ( -0.2066929133858267931, 0.7443365962042343131, -3.523993443072799270 ) ) ;
#43759 = EDGE_LOOP ( 'NONE', ( #36042, #13698, #32993, #38563 ) ) ;
#43760 = CARTESIAN_POINT ( 'NONE',  ( -0.6971942568897648851, 0.07405724077823318263, 1.855314960576157635 ) ) ;
#43761 = ( BOUNDED_CURVE ( )  B_SPLINE_CURVE ( 2, ( #20760, #10233, #15663, #12300, #21959, #44851, #23314, #23550, #34344 ),
 .UNSPECIFIED., .F., .T. ) 
 B_SPLINE_CURVE_WITH_KNOTS ( ( 3, 2, 2, 2, 3 ),
 ( 0.7199999999999999734, 0.7225000000000000311, 0.7249999999999999778, 0.7275000000000000355, 0.7299999999999999822 ),
 .UNSPECIFIED. ) 
 CURVE ( )  GEOMETRIC_REPRESENTATION_ITEM ( )  RATIONAL_B_SPLINE_CURVE ( ( 1.000000000000000000, 0.9238795325112869605, 1.000000000000000000, 0.9238795325112869605, 1.000000000000000000, 0.9238795325112869605, 1.000000000000000000, 0.9238795325112799661, 1.000000000000000000 ) ) 
 REPRESENTATION_ITEM ( '' )  ) ;
#43762 = EDGE_CURVE ( 'NONE', #33511, #32711, #44866, .T. ) ;
#43763 = CARTESIAN_POINT ( 'NONE',  ( -0.8075642815980649258, 0.1651804164989427171, 0.03937007874015843040 ) ) ;
#43764 = CARTESIAN_POINT ( 'NONE',  ( 0.9412147342319837628, -0.1574803149606297803, 0.6717519685039377020 ) ) ;
#43765 = CARTESIAN_POINT ( 'NONE',  ( -0.1797182628040039087, -0.7859690064334394766, 0.07444174185955065859 ) ) ;
#43766 = CARTESIAN_POINT ( 'NONE',  ( 0.1225179410730680984, -0.2247584660033122572, -0.3149606299212597826 ) ) ;
#43767 = CARTESIAN_POINT ( 'NONE',  ( 0.7495606340400177148, 0.1264236179284866091, 0.7898622046706456068 ) ) ;
#43768 = CARTESIAN_POINT ( 'NONE',  ( 0.6971942568897648851, 0.07405724077823318263, 1.377952755851748368 ) ) ;
#43769 = CARTESIAN_POINT ( 'NONE',  ( -0.1258674519624516375, 0.1236212482586854927, -0.1007786101663682155 ) ) ;
#43770 = EDGE_LOOP ( 'NONE', ( #39675, #8721, #13509, #1391, #30269, #23426, #36332, #28508, #9328, #5860, #3244, #19094 ) ) ;
#43771 = CARTESIAN_POINT ( 'NONE',  ( -0.2559055118110235560, 0.08170541745154620561, -0.05466765753244264003 ) ) ;
#43772 = EDGE_CURVE ( 'NONE', #1072, #13671, #19703, .T. ) ;
#43773 = CARTESIAN_POINT ( 'NONE',  ( 1.033464566929133799, 0.000000000000000000, 1.466535433070866201 ) ) ;
#43775 = LINE ( 'NONE', #10978, #23905 ) ;
#43774 = CARTESIAN_POINT ( 'NONE',  ( 0.8513189030870298435, -0.1720149802712487852, 1.987756617428876327 ) ) ;
#43776 = CARTESIAN_POINT ( 'NONE',  ( 0.9412147342319837628, -0.1574803149606297803, 1.488681102254677535 ) ) ;
#43777 = ORIENTED_EDGE ( 'NONE', *, *, #26865, .T. ) ;
#43778 = AXIS2_PLACEMENT_3D ( 'NONE', #43004, #42536, #9740 ) ;
#43780 = CARTESIAN_POINT ( 'NONE',  ( 0.8759842519685039353, -0.1574803149606299191, 0.2657480313885358103 ) ) ;
#43779 = CARTESIAN_POINT ( 'NONE',  ( 0.9500414927467377701, 0.1787899950787401604, 0.6988188975840318173 ) ) ;
#43781 = CARTESIAN_POINT ( 'NONE',  ( -0.1787899950787401604, -0.7116141731745821986, -0.07405724077823318263 ) ) ;
#43782 = CARTESIAN_POINT ( 'NONE',  ( 0.7646288533564489232, 0.1113553986120547346, 1.560039370078740273 ) ) ;
#43783 = ORIENTED_EDGE ( 'NONE', *, *, #26913, .F. ) ;
#43784 = CARTESIAN_POINT ( 'NONE',  ( -1.033464566929134687, 0.06523048226347956391, 1.154035433070866423 ) ) ;
#43785 = CIRCLE ( 'NONE', #28526, 0.2559055118110236116 ) ;
#43787 = LINE ( 'NONE', #44242, #32886 ) ;
#43786 = AXIS2_PLACEMENT_3D ( 'NONE', #2915, #14676, #11556 ) ;
#43788 = CARTESIAN_POINT ( 'NONE',  ( 0.7495606340400177148, 0.1264236179284866091, 1.060531496009228247 ) ) ;
#43789 = APPLICATION_CONTEXT ( 'automotive_design' ) ;
#43790 = LINE ( 'NONE', #6888, #16536 ) ;
#43791 = CARTESIAN_POINT ( 'NONE',  ( -0.1113553986120547346, -1.528543307086614123, -0.1113553986120547346 ) ) ;
#43792 = CARTESIAN_POINT ( 'NONE',  ( 0.9412147342319837628, 0.1574803149606300301, 1.237696850393701586 ) ) ;
#43793 = EDGE_LOOP ( 'NONE', ( #45956, #38339, #21665, #250, #25945 ) ) ;
#43794 = CARTESIAN_POINT ( 'NONE',  ( -1.054774247047244540, -0.07405724077823318263, 0.05905511805647267048 ) ) ;
#43795 = CARTESIAN_POINT ( 'NONE',  ( 2.892866454678787531E-17, 0.1003937007874015908, 0.1574803149606299191 ) ) ;
#43796 = ORIENTED_EDGE ( 'NONE', *, *, #29117, .T. ) ;
#43797 = CARTESIAN_POINT ( 'NONE',  ( -0.8107537697050254399, -0.1574803149606297803, 1.847933070866142780 ) ) ;
#43798 = CARTESIAN_POINT ( 'NONE',  ( -0.6971942568897648851, -0.07405724077823297447, 1.697834645615527771 ) ) ;
#43799 = CARTESIAN_POINT ( 'NONE',  ( 0.7185039370078739607, 0.000000000000000000, 4.498031496062992574 ) ) ;
#43800 = CARTESIAN_POINT ( 'NONE',  ( -0.8019270111902717657, -0.1787899950787401604, 1.983267716481667886 ) ) ;
#43801 = CARTESIAN_POINT ( 'NONE',  ( 0.8759842519685039353, 0.1574803149606299191, 0.2952755905511810774 ) ) ;
#43802 = CARTESIAN_POINT ( 'NONE',  ( 0.9500414927467378812, -0.1787899950787401604, 0.05413385821395302888 ) ) ;
#43803 = DIRECTION ( 'NONE',  ( 0.000000000000000000, 0.000000000000000000, -1.000000000000000000 ) ) ;
#43804 = CARTESIAN_POINT ( 'NONE',  ( 3.284318927891251994E-17, -0.3608523146859319297, 0.1787899950787401882 ) ) ;
#43805 = CYLINDRICAL_SURFACE ( 'NONE', #5778, 0.1574803149606299191 ) ;
#43806 = STYLED_ITEM ( 'NONE', ( #5284 ), #37046 ) ;
#43807 = CARTESIAN_POINT ( 'NONE',  ( -0.6971942568897637749, 2.189545951927499583E-17, 0.2386811023084413619 ) ) ;
#43808 = ADVANCED_BREP_SHAPE_REPRESENTATION ( 'Side Bracket', ( #36893, #20860 ), #29349 ) ;
#43809 = ORIENTED_EDGE ( 'NONE', *, *, #11577, .F. ) ;
#43810 = EDGE_CURVE ( 'NONE', #31906, #7313, #38561, .T. ) ;
#43811 = CARTESIAN_POINT ( 'NONE',  ( -0.7495606340400177148, 0.1264236179284866091, 1.380413385773007873 ) ) ;
#43812 = ORIENTED_EDGE ( 'NONE', *, *, #729, .F. ) ;
#43813 = ( GEOMETRIC_REPRESENTATION_CONTEXT ( 3 ) GLOBAL_UNCERTAINTY_ASSIGNED_CONTEXT ( ( #39834 ) ) GLOBAL_UNIT_ASSIGNED_CONTEXT ( ( #9122, #42155, #23985 ) ) REPRESENTATION_CONTEXT ( 'NONE', 'WORKASPACE' ) ) ;
#43814 = CIRCLE ( 'NONE', #41487, 0.7874015748031497619 ) ;
#43815 = CARTESIAN_POINT ( 'NONE',  ( 0.1787899950787401882, -1.245570866087968520, -2.189545951927503898E-17 ) ) ;
#43816 = CARTESIAN_POINT ( 'NONE',  ( 3.284318927891251994E-17, -1.447342519631275692, 0.1787899950787401882 ) ) ;
#43817 = ADVANCED_FACE ( 'NONE', ( #45814 ), #42678, .T. ) ;
#43818 = CARTESIAN_POINT ( 'NONE',  ( 1.964665320562165363, 0.9228240091143701251, 0.000000000000000000 ) ) ;
#43819 = CARTESIAN_POINT ( 'NONE',  ( -0.8070866141732283561, -0.0009842519685049383633, 0.6590551181102368705 ) ) ;
#43820 = CARTESIAN_POINT ( 'NONE',  ( -0.9873396505805591694, 0.1113553986120547346, 0.9104330707586141269 ) ) ;
#43821 = AXIS2_PLACEMENT_3D ( 'NONE', #39791, #38867, #14426 ) ;
#43822 = CARTESIAN_POINT ( 'NONE',  ( 1.054774247047244540, -0.07405724077823318263, 0.4576771653005669016 ) ) ;
#43823 = CARTESIAN_POINT ( 'NONE',  ( -0.1113553986120547346, -0.1112204724409448786, -0.1113553986120547346 ) ) ;
#43824 = CARTESIAN_POINT ( 'NONE',  ( 1.033464566929134687, 0.06523048226347956391, 1.774114173120818316 ) ) ;
#43825 = ORIENTED_EDGE ( 'NONE', *, *, #42398, .F. ) ;
#43826 = CARTESIAN_POINT ( 'NONE',  ( -1.033464566929131356, 0.06523048226348168721, 1.419783464459401845 ) ) ;
#43827 = CARTESIAN_POINT ( 'NONE',  ( 0.8759842519685039353, 0.1574803149606299191, 0.7283464566929134243 ) ) ;
#43828 = LINE ( 'NONE', #916, #14898 ) ;
#43829 = ADVANCED_FACE ( 'NONE', ( #27892 ), #31940, .T. ) ;
#43831 = DIRECTION ( 'NONE',  ( 0.000000000000000000, -1.000000000000000000, 0.000000000000000000 ) ) ;
#43830 = DIRECTION ( 'NONE',  ( 0.000000000000000000, 0.000000000000000000, 1.000000000000000000 ) ) ;
#43832 = CARTESIAN_POINT ( 'NONE',  ( 1.033464566929133799, 1.928577636452524610E-17, 4.498031496062992574 ) ) ;
#43833 = VERTEX_POINT ( 'NONE', #24043 ) ;
#43834 = CARTESIAN_POINT ( 'NONE',  ( -0.1787899950787401604, -0.03740157474938609478, 0.07405724077823318263 ) ) ;
#43835 = VERTEX_POINT ( 'NONE', #21128 ) ;
#43836 = DIRECTION ( 'NONE',  ( 1.000000000000000000, -3.532562060772751952E-15, 0.000000000000000000 ) ) ;
#43837 = CARTESIAN_POINT ( 'NONE',  ( 0.8107537697050254399, -0.1574803149606297803, 1.375492125984252745 ) ) ;
#43838 = CARTESIAN_POINT ( 'NONE',  ( 0.1264236179284866091, -1.639271653489543290, 0.1264236179284866091 ) ) ;
#43839 = CARTESIAN_POINT ( 'NONE',  ( 0.1574803149606299191, -1.494094488081448846, -1.928577636452523993E-17 ) ) ;
#43840 = CARTESIAN_POINT ( 'NONE',  ( 0.1787899950787401604, -0.7755905511273385455, 0.07405724077823318263 ) ) ;
#43841 = CARTESIAN_POINT ( 'NONE',  ( -1.033464566929133799, 0.000000000000000000, 0.1574803148531029595 ) ) ;
#43842 = CARTESIAN_POINT ( 'NONE',  ( 0.1113553986120547346, -0.9872047244094488416, -0.1113553986120547346 ) ) ;
#43843 = CARTESIAN_POINT ( 'NONE',  ( 1.033464566929134687, -0.06523048226347956391, 1.021161417215306955 ) ) ;
#43844 = AXIS2_PLACEMENT_3D ( 'NONE', #5931, #20548, #24391 ) ;
#43845 = CARTESIAN_POINT ( 'NONE',  ( -0.6971942568897637749, 2.189545951927499583E-17, 0.3961614172690708924 ) ) ;
#43846 = ORIENTED_EDGE ( 'NONE', *, *, #18066, .T. ) ;
#43847 = ORIENTED_EDGE ( 'NONE', *, *, #46510, .T. ) ;
#43848 = CARTESIAN_POINT ( 'NONE',  ( -1.054774247047244096, 0.000000000000000000, 1.680610236166708793 ) ) ;
#43849 = ORIENTED_EDGE ( 'NONE', *, *, #39590, .T. ) ;
#43850 = CARTESIAN_POINT ( 'NONE',  ( 0.6971942568897648851, -0.07405724077823297447, 1.624015747977732849 ) ) ;
#43851 = CARTESIAN_POINT ( 'NONE',  ( -0.9500414927467378812, 0.1787899950787401604, 0.7431102361667091261 ) ) ;
#43852 = CARTESIAN_POINT ( 'NONE',  ( 0.8019270111902717657, -0.1787899950787401604, 1.550196850339937926 ) ) ;
#43853 = VECTOR ( 'NONE', #28532, 39.37007874015748143 ) ;
#43854 = CARTESIAN_POINT ( 'NONE',  ( -1.033464566929133799, 0.000000000000000000, 0.4724409447743622148 ) ) ;
#43855 = CARTESIAN_POINT ( 'NONE',  ( -0.9500414927467377701, 0.1787899950787401604, 0.6988188975840318173 ) ) ;
#43856 = CARTESIAN_POINT ( 'NONE',  ( 0.1574803149606300301, -0.07431102351452013866, -0.06523048226347956391 ) ) ;
#43857 = VECTOR ( 'NONE', #13288, 39.37007874015748854 ) ;
#43858 = CARTESIAN_POINT ( 'NONE',  ( 0.7185039370078766252, -0.06523048226348168721, 1.134350393700787940 ) ) ;
#43859 = CARTESIAN_POINT ( 'NONE',  ( -0.8019270111902717657, 0.1787899950787401604, 1.574803149552536530 ) ) ;
#43860 = CARTESIAN_POINT ( 'NONE',  ( -0.9873396505805591694, -0.1113553986120547346, 1.963582677057826853 ) ) ;
#43861 = ORIENTED_EDGE ( 'NONE', *, *, #24269, .F. ) ;
#43862 = CARTESIAN_POINT ( 'NONE',  ( -0.7185039370078746268, -0.06523048226347956391, 1.528051181102361600 ) ) ;
#43863 = FACE_OUTER_BOUND ( 'NONE', #35923, .T. ) ;
#43864 = CARTESIAN_POINT ( 'NONE',  ( 1.002407869896990045, 0.1264236179284866091, 1.488681102308440751 ) ) ;
#43865 = CARTESIAN_POINT ( 'NONE',  ( -0.1205236854640061028, -0.09851384067577953485, -0.1371198999545033548 ) ) ;
#43866 = CYLINDRICAL_SURFACE ( 'NONE', #32563, 0.1574803149606299191 ) ;
#43867 = VERTEX_POINT ( 'NONE', #32176 ) ;
#43868 = EDGE_CURVE ( 'NONE', #12246, #12116, #37178, .T. ) ;
#43869 = ORIENTED_EDGE ( 'NONE', *, *, #16997, .T. ) ;
#43870 = ADVANCED_FACE ( 'NONE', ( #9890 ), #35762, .T. ) ;
#43871 = EDGE_LOOP ( 'NONE', ( #39850, #33224, #19127, #7923 ) ) ;
#43872 = DIRECTION ( 'NONE',  ( 0.000000000000000000, 0.000000000000000000, 1.000000000000000000 ) ) ;
#43873 = CARTESIAN_POINT ( 'NONE',  ( 0.1787899950787401604, -0.8444881889226140137, -0.07405724077823318263 ) ) ;
#43874 = CARTESIAN_POINT ( 'NONE',  ( -0.8759842519685039353, 0.000000000000000000, 0.000000000000000000 ) ) ;
#43875 = SURFACE_STYLE_FILL_AREA ( #19181 ) ;
#43876 = ( LENGTH_UNIT ( ) NAMED_UNIT ( * ) SI_UNIT ( $, .METRE. ) ) ;
#43877 = CARTESIAN_POINT ( 'NONE',  ( 0.6971942568897648851, -0.07405724077823297447, 1.776574803095843924 ) ) ;
#43878 = CARTESIAN_POINT ( 'NONE',  ( 0.1270800023317771588, -0.1831146757247779644, 0.1270800023317771588 ) ) ;
#43879 = CARTESIAN_POINT ( 'NONE',  ( -0.1787899950787401604, -0.1713838107489239204, 0.07405724077823318263 ) ) ;
#43880 = CARTESIAN_POINT ( 'NONE',  ( -0.1787899950787401604, -0.3179133857730082058, -0.07405724077823318263 ) ) ;
#43881 = CARTESIAN_POINT ( 'NONE',  ( 0.07405724077823318263, -0.1112204723871813017, 0.1787899950787401604 ) ) ;
#43882 = CONTEXT_DEPENDENT_SHAPE_REPRESENTATION ( #4867, #13787 ) ;
#43883 = CARTESIAN_POINT ( 'NONE',  ( 0.2471922967771570667, -0.09275221067063771363, -0.04038134086897739172 ) ) ;
#43884 = CARTESIAN_POINT ( 'NONE',  ( 1.002407869896990045, -0.1264236179284866091, 0.6865157479777322935 ) ) ;
#43886 = CARTESIAN_POINT ( 'NONE',  ( 0.7185039370078739607, 1.928577636452523993E-17, 1.131889763779527547 ) ) ;
#43885 = DIRECTION ( 'NONE',  ( -1.000000000000000000, 0.000000000000000000, 0.000000000000000000 ) ) ;
#43887 = DIRECTION ( 'NONE',  ( -0.000000000000000000, 1.000000000000000000, 0.000000000000000000 ) ) ;
#43888 = ( GEOMETRIC_REPRESENTATION_CONTEXT ( 3 ) GLOBAL_UNCERTAINTY_ASSIGNED_CONTEXT ( ( #22513 ) ) GLOBAL_UNIT_ASSIGNED_CONTEXT ( ( #7227, #30025, #40269 ) ) REPRESENTATION_CONTEXT ( 'NONE', 'WORKASPACE' ) ) ;
#43889 = DIRECTION ( 'NONE',  ( 0.000000000000000000, 0.000000000000000000, 1.000000000000000000 ) ) ;
#43890 = CARTESIAN_POINT ( 'NONE',  ( 0.8759842519685039353, -0.1787899950787401882, 1.828248031442299082 ) ) ;
#43892 = CYLINDRICAL_SURFACE ( 'NONE', #19329, 0.1574803149606299191 ) ;
#43891 = DIRECTION ( 'NONE',  ( 0.000000000000000000, -1.000000000000000000, 0.000000000000000000 ) ) ;
#43893 = CARTESIAN_POINT ( 'NONE',  ( 1.054774247047244540, 0.07405724077823318263, 0.4970472440407249226 ) ) ;
#43894 = ORIENTED_EDGE ( 'NONE', *, *, #43153, .T. ) ;
#43895 = CARTESIAN_POINT ( 'NONE',  ( 0.1526809758745832635, -0.1055212057016147592, 0.09282246162997874472 ) ) ;
#43896 = CARTESIAN_POINT ( 'NONE',  ( 0.07405724077823318263, -0.3474409448281265411, 0.1787899950787401604 ) ) ;
#43897 = CARTESIAN_POINT ( 'NONE',  ( -0.8019270111902717657, 0.1787899950787401604, 0.4724409448281262636 ) ) ;
#43898 = CARTESIAN_POINT ( 'NONE',  ( -1.094772975963752103E-17, -1.112696850339937038, -0.1787899950787401882 ) ) ;
#43899 = DIRECTION ( 'NONE',  ( -1.000000000000000000, 0.000000000000000000, 0.000000000000000000 ) ) ;
#43900 = CARTESIAN_POINT ( 'NONE',  ( 0.3727034120734909473, -0.08090551181102362266, 0.000000000000000000 ) ) ;
#43901 = CARTESIAN_POINT ( 'NONE',  ( -0.7495606340400177148, -0.1264236179284866091, 1.542814960576157413 ) ) ;
#43902 = EDGE_LOOP ( 'NONE', ( #36552, #17402, #15776, #20031, #40950, #37858, #13450 ) ) ;
#43903 = CARTESIAN_POINT ( 'NONE',  ( -1.002407869896990045, -0.1264236179284866091, 1.163877952702141672 ) ) ;
#43904 = DIRECTION ( 'NONE',  ( 0.000000000000000000, 0.000000000000000000, 1.000000000000000000 ) ) ;
#43905 = CARTESIAN_POINT ( 'NONE',  ( 0.06523048226347956391, -1.147145669183812222, 0.1574803149606297803 ) ) ;
#43906 = CARTESIAN_POINT ( 'NONE',  ( 1.002407869896990045, -0.1264236179284866091, 1.946358267662771757 ) ) ;
#43907 = CARTESIAN_POINT ( 'NONE',  ( -0.9873396505805591694, 0.1113553986120547346, 0.6053149606299212948 ) ) ;
#43908 = CARTESIAN_POINT ( 'NONE',  ( -0.9500414927467378812, 0.1787899950787401604, 1.053149606245450176 ) ) ;
#43909 = LINE ( 'NONE', #18046, #25886 ) ;
#43910 = CARTESIAN_POINT ( 'NONE',  ( -0.1985616933439231790, -0.1808545851595459442, -0.05455490385610407833 ) ) ;
#43911 = CARTESIAN_POINT ( 'NONE',  ( 0.9500414927467377701, 0.1787899950787401604, 0.3100393700249766682 ) ) ;
#43912 = CARTESIAN_POINT ( 'NONE',  ( -0.8019270111902716547, 0.1787899950787401604, 0.2706692912848194243 ) ) ;
#43913 = CARTESIAN_POINT ( 'NONE',  ( -0.8019270111902717657, -0.1787899950787401604, 0.7578740156942689321 ) ) ;
#43914 = CARTESIAN_POINT ( 'NONE',  ( 1.033464566929133799, 0.000000000000000000, 1.653543306979086580 ) ) ;
#43915 = ORIENTED_EDGE ( 'NONE', *, *, #41233, .F. ) ;
#43916 = CARTESIAN_POINT ( 'NONE',  ( 0.07405724077823318263, 0.04625984257344856188, 0.1787899950787401604 ) ) ;
#43917 = CARTESIAN_POINT ( 'NONE',  ( 1.054774247047244540, 0.07405724077823318263, 0.7381889763241898939 ) ) ;
#43918 = CARTESIAN_POINT ( 'NONE',  ( 0.9500414927467377701, -0.1787899950787401604, 1.043307086560409269 ) ) ;
#43919 = CARTESIAN_POINT ( 'NONE',  ( -1.054774247047244540, -0.07405724077823318263, 1.870078740103715331 ) ) ;
#43920 = AXIS2_PLACEMENT_3D ( 'NONE', #23454, #4737, #38057 ) ;
#43921 = VERTEX_POINT ( 'NONE', #10369 ) ;
#43922 = ADVANCED_FACE ( 'NONE', ( #6746 ), #20897, .F. ) ;
#43923 = B_SPLINE_CURVE_WITH_KNOTS ( 'NONE', 3,
 ( #21557, #17957, #14381, #44064, #915, #18429, #5707, #5402, #27496, #24568, #20727, #31781, #13326, #6340, #13775, #28419 ),
 .UNSPECIFIED., .F., .F.,
 ( 4, 2, 2, 2, 2, 2, 2, 4 ),
 ( 0.000000000000000000, 0.1250000000000247302, 0.1875000000000333900, 0.2187500000000407174, 0.2500000000000480171, 0.3750000000000456302, 0.5000000000000432987, 1.000000000000000000 ),
 .UNSPECIFIED. ) ;
#43924 = CARTESIAN_POINT ( 'NONE',  ( 1.054774247047244540, -0.07405724077823318263, 1.909448818843873186 ) ) ;
#43925 = EDGE_CURVE ( 'NONE', #29529, #32777, #17305, .T. ) ;
#43926 = FACE_OUTER_BOUND ( 'NONE', #25120, .T. ) ;
#43927 = CARTESIAN_POINT ( 'NONE',  ( -0.07405724077823318263, -1.283588535158372457, -0.1787899950787401604 ) ) ;
#43928 = AXIS2_PLACEMENT_3D ( 'NONE', #6921, #24440, #21301 ) ;
#43929 = EDGE_LOOP ( 'NONE', ( #35116, #41579, #8815, #13802 ) ) ;
#43930 = CARTESIAN_POINT ( 'NONE',  ( -0.1264236179284866091, -0.2317913385289138151, 0.1264236179284866091 ) ) ;
#43931 = ADVANCED_FACE ( 'NONE', ( #20656 ), #35535, .T. ) ;
#43932 = CARTESIAN_POINT ( 'NONE',  ( -0.2833820772873879568, -0.1260390447071885467, 0.7654149962237527527 ) ) ;
#43933 = ORIENTED_EDGE ( 'NONE', *, *, #47352, .T. ) ;
#43934 = CARTESIAN_POINT ( 'NONE',  ( 1.054774247047244096, 0.000000000000000000, 1.242618110182456714 ) ) ;
#43935 = EDGE_CURVE ( 'NONE', #41717, #21785, #39570, .T. ) ;
#43936 = LINE ( 'NONE', #7508, #33282 ) ;
#43937 = LINE ( 'NONE', #32951, #128 ) ;
#43938 = CARTESIAN_POINT ( 'NONE',  ( 0.7495606340400177148, 0.1264236179284866091, 0.07627952750529173875 ) ) ;
#43939 = CARTESIAN_POINT ( 'NONE',  ( -0.07405724077823318263, -1.705708661363559253, -0.1787899950787401604 ) ) ;
#43940 = CARTESIAN_POINT ( 'NONE',  ( 0.07405724077823318263, -1.626968503883244876, -0.1787899950787401604 ) ) ;
#43941 = CARTESIAN_POINT ( 'NONE',  ( -0.8759842519685039353, -0.1787899950787401882, 0.5684055117572598403 ) ) ;
#43942 = CARTESIAN_POINT ( 'NONE',  ( 0.4755220087074803481, 0.09842519685039370636, 0.000000000000000000 ) ) ;
#43943 = CARTESIAN_POINT ( 'NONE',  ( 3.301370929368692659E-17, -1.487248533992494126, 0.1797182628040039365 ) ) ;
#43944 = CARTESIAN_POINT ( 'NONE',  ( 2.219626494852212756E-16, 0.2954942322624074524, -0.1122047244094488277 ) ) ;
#43945 = VECTOR ( 'NONE', #16200, 39.37007874015748143 ) ;
#43946 = CARTESIAN_POINT ( 'NONE',  ( 0.9500414927467378812, -0.1787899950787401604, 1.279527559001355286 ) ) ;
#43947 = CARTESIAN_POINT ( 'NONE',  ( 1.054774247047244096, 0.000000000000000000, 1.636318897584031484 ) ) ;
#43948 = CIRCLE ( 'NONE', #40884, 0.09842519685039370636 ) ;
#43949 = CARTESIAN_POINT ( 'NONE',  ( -0.7185039370078766252, -0.06523048226348168721, 1.636318897530268490 ) ) ;
#43950 = DIRECTION ( 'NONE',  ( -1.000000000000000000, 0.000000000000000000, 0.000000000000000000 ) ) ;
#43951 = CARTESIAN_POINT ( 'NONE',  ( -0.7646288533564489232, -0.1113553986120547346, 1.924212598425196985 ) ) ;
#43952 = DIRECTION ( 'NONE',  ( 1.822029033848725028E-16, 0.000000000000000000, 1.000000000000000000 ) ) ;
#43953 = CARTESIAN_POINT ( 'NONE',  ( 0.7495606340400177148, -0.1264236179284866091, 0.2829724408911185041 ) ) ;
#43954 = CARTESIAN_POINT ( 'NONE',  ( 0.7326906711842074982, -0.08861378245919243613, 0.03937031356849532426 ) ) ;
#43955 = DIRECTION ( 'NONE',  ( -1.000000000000000000, 3.469446951953613794E-15, 1.144917494144684547E-16 ) ) ;
#43956 = CARTESIAN_POINT ( 'NONE',  ( 0.4028871391076110364, 4.616380251121755931E-17, 0.000000000000000000 ) ) ;
#43957 = DIRECTION ( 'NONE',  ( 5.724375810226260600E-16, 0.6156614753256579586, 0.7880107536067221252 ) ) ;
#43958 = CARTESIAN_POINT ( 'NONE',  ( -0.6971942568897648851, 0.07405724077823318263, 1.220472440891118504 ) ) ;
#43959 = CARTESIAN_POINT ( 'NONE',  ( 0.7646288533564489232, -0.1113553986120547346, 0.6151574802074331050 ) ) ;
#43960 = EDGE_LOOP ( 'NONE', ( #39124, #28281, #17468, #39811, #28715, #43894, #18823, #44305 ) ) ;
#43961 = CIRCLE ( 'NONE', #23317, 0.1574803149606292529 ) ;
#43962 = ( NAMED_UNIT ( * ) SI_UNIT ( $, .STERADIAN. ) SOLID_ANGLE_UNIT ( ) ) ;
#43963 = CARTESIAN_POINT ( 'NONE',  ( 0.9651124939922542945, 0.1429248741482666007, 0.03937007863209032038 ) ) ;
#43964 = CARTESIAN_POINT ( 'NONE',  ( 1.033464566929133799, 0.000000000000000000, 0.8267716534357796299 ) ) ;
#43965 = CARTESIAN_POINT ( 'NONE',  ( -0.9412147342319837628, 0.1574803149606300301, 1.109744094380661350 ) ) ;
#43966 = CARTESIAN_POINT ( 'NONE',  ( 0.7495606340400177148, 0.1264236179284866091, 1.493602362150960650 ) ) ;
#43968 = DIRECTION ( 'NONE',  ( -0.000000000000000000, -0.7880107536067200158, 0.6156614753256608452 ) ) ;
#43967 = CARTESIAN_POINT ( 'NONE',  ( -0.8107537697050254399, 0.1574803149606300301, 0.9276574803149607584 ) ) ;
#43969 = CARTESIAN_POINT ( 'NONE',  ( -0.1264236179284866091, -0.1530511810485988278, 0.1264236179284866091 ) ) ;
#43970 = EDGE_LOOP ( 'NONE', ( #41648, #36293, #34239, #28582 ) ) ;
#43971 = DIRECTION ( 'NONE',  ( -1.000000000000000000, 0.000000000000000000, 0.000000000000000000 ) ) ;
#43972 = CARTESIAN_POINT ( 'NONE',  ( -1.033464566929134687, 0.06523048226347956391, 0.3666338582677165503 ) ) ;
#43973 = SURFACE_SIDE_STYLE ('',( #32276 ) ) ;
#43974 = VERTEX_POINT ( 'NONE', #27663 ) ;
#43975 = CARTESIAN_POINT ( 'NONE',  ( 0.8019270111902717657, 0.1787899950787401604, 0.5511811023084406402 ) ) ;
#43976 = VERTEX_POINT ( 'NONE', #42221 ) ;
#43977 = CARTESIAN_POINT ( 'NONE',  ( 0.1574803149606300301, 0.03887795286343254109, 0.06523048226347956391 ) ) ;
#43978 = CARTESIAN_POINT ( 'NONE',  ( -0.6971942568897648851, 0.07405724077823318263, 1.107283464513165949 ) ) ;
#43979 = CARTESIAN_POINT ( 'NONE',  ( -1.033464566929134687, -0.06523048226347956391, 1.975885826771653475 ) ) ;
#43980 = CARTESIAN_POINT ( 'NONE',  ( -0.9500414927467378812, -0.1787899950787401604, 0.8070866141194653620 ) ) ;
#43981 = EDGE_CURVE ( 'NONE', #34250, #40379, #10853, .T. ) ;
#43982 = CARTESIAN_POINT ( 'NONE',  ( -0.1279527559055118058, 0.2216206741968047289, -0.3149606299212598381 ) ) ;
#43983 = CARTESIAN_POINT ( 'NONE',  ( -0.8759842519685039353, -0.1787899950787401882, 0.2534448818360003908 ) ) ;
#43984 = CARTESIAN_POINT ( 'NONE',  ( 0.9412147342319837628, -0.1574803149606297803, 0.6717519685039375910 ) ) ;
#43985 = VECTOR ( 'NONE', #4143, 39.37007874015748143 ) ;
#43986 = CYLINDRICAL_SURFACE ( 'NONE', #16012, 0.2204724409448818867 ) ;
#43987 = CARTESIAN_POINT ( 'NONE',  ( -0.1787899950787401604, -0.8849664879142767893, -0.07405724077823318263 ) ) ;
#43988 = ORIENTED_EDGE ( 'NONE', *, *, #26374, .F. ) ;
#43989 = CARTESIAN_POINT ( 'NONE',  ( -0.1264236179284866091, 0.1225393701325037388, 0.1264236179284866091 ) ) ;
#43990 = ORIENTED_EDGE ( 'NONE', *, *, #33900, .T. ) ;
#43991 = CIRCLE ( 'NONE', #23344, 0.1377952755905511861 ) ;
#43992 = CONICAL_SURFACE ( 'NONE', #20284, 0.1377952755905510196, 0.9599310885968940221 ) ;
#43993 = EDGE_LOOP ( 'NONE', ( #41619, #3451, #13360, #26679 ) ) ;
#43994 = ADVANCED_FACE ( 'NONE', ( #7235 ), #21855, .F. ) ;
#43995 = CARTESIAN_POINT ( 'NONE',  ( 0.3000685424736224127, 1.205361022782824954E-17, -0.09842519685039370636 ) ) ;
#43996 = CARTESIAN_POINT ( 'NONE',  ( -1.054774247047244096, 0.000000000000000000, 0.8095472440407244230 ) ) ;
#43997 = CARTESIAN_POINT ( 'NONE',  ( -0.9500414927467377701, 0.1787899950787401604, 1.806102362150961094 ) ) ;
#43998 = CARTESIAN_POINT ( 'NONE',  ( -1.054774247047244096, 0.000000000000000000, 0.06643700782025216411 ) ) ;
#43999 = CARTESIAN_POINT ( 'NONE',  ( 0.1270800023317771588, -0.8524060143074547735, 0.1270800023317771588 ) ) ;
#44000 = CYLINDRICAL_SURFACE ( 'NONE', #21768, 0.1574803149606299191 ) ;
#44001 = CARTESIAN_POINT ( 'NONE',  ( -1.033464566929134687, -0.06523048226347956391, 1.493602362097197211 ) ) ;
#44002 = CARTESIAN_POINT ( 'NONE',  ( 1.054774247047244096, 0.000000000000000000, 0.8144685038832440993 ) ) ;
#44003 = DIRECTION ( 'NONE',  ( 0.000000000000000000, -2.197428715927215401E-15, 1.000000000000000000 ) ) ;
#44004 = CARTESIAN_POINT ( 'NONE',  ( 0.9412147342319837628, -0.1574803149606297803, 1.380413385826771977 ) ) ;
#44006 = CARTESIAN_POINT ( 'NONE',  ( 0.06523048226347977208, 0.1126968505012277827, 0.1574803149606297803 ) ) ;
#44005 = CARTESIAN_POINT ( 'NONE',  ( 0.8673732830012496064, -0.1740754669566842439, 1.988051277661635474 ) ) ;
#44007 = ADVANCED_FACE ( 'NONE', ( #3153 ), #10611, .F. ) ;
#44008 = CARTESIAN_POINT ( 'NONE',  ( 1.054774247047244540, 0.07405724077823318263, 0.8513779527021426707 ) ) ;
#44009 = AXIS2_PLACEMENT_3D ( 'NONE', #15298, #44494, #11712 ) ;
#44011 = VECTOR ( 'NONE', #18180, 39.37007874015748854 ) ;
#44010 = CARTESIAN_POINT ( 'NONE',  ( -0.1787899950787401604, -0.7903543306548983516, -0.07405724077823318263 ) ) ;
#44012 = ORIENTED_EDGE ( 'NONE', *, *, #5186, .T. ) ;
#44013 = CARTESIAN_POINT ( 'NONE',  ( 0.1644020957507537628, 0.08115590401245550978, 0.1405661490837558925 ) ) ;
#44014 = CARTESIAN_POINT ( 'NONE',  ( 0.003457534521343483096, -0.1398629656505342711, 0.03335920195936160210 ) ) ;
#44015 = CARTESIAN_POINT ( 'NONE',  ( 0.7495606340400177148, 0.1264236179284866091, 0.9424212597887559051 ) ) ;
#44016 = DIRECTION ( 'NONE',  ( 0.000000000000000000, 0.000000000000000000, 1.000000000000000000 ) ) ;
#44017 = CARTESIAN_POINT ( 'NONE',  ( -0.1113553986120547346, -1.725393700787401841, -0.1113553986120547346 ) ) ;
#44018 = DIRECTION ( 'NONE',  ( 1.000000000000000000, 0.000000000000000000, 0.000000000000000000 ) ) ;
#44019 = ( BOUNDED_CURVE ( )  B_SPLINE_CURVE ( 2, ( #16390, #19956, #26472, #4863, #45109, #34596, #31010, #12084, #1746 ),
 .UNSPECIFIED., .F., .T. ) 
 B_SPLINE_CURVE_WITH_KNOTS ( ( 3, 2, 2, 2, 3 ),
 ( 0.09500000000000000111, 0.09750000000000000333, 0.1000000000000000056, 0.1024999999999999939, 0.1049999999999999961 ),
 .UNSPECIFIED. ) 
 CURVE ( )  GEOMETRIC_REPRESENTATION_ITEM ( )  RATIONAL_B_SPLINE_CURVE ( ( 1.000000000000000000, 0.9238795325112869605, 1.000000000000000000, 0.9238795325112869605, 1.000000000000000000, 0.9238795325112869605, 1.000000000000000000, 0.9238795325112869605, 1.000000000000000000 ) ) 
 REPRESENTATION_ITEM ( '' )  ) ;
#44020 = VERTEX_POINT ( 'NONE', #21615 ) ;
#44021 = CARTESIAN_POINT ( 'NONE',  ( -0.6195511811023656223, 0.9842519685039370358, -0.7135826771653542844 ) ) ;
#44022 = CARTESIAN_POINT ( 'NONE',  ( -0.9500414927467378812, 0.1787899950787401604, 0.02952755900135462311 ) ) ;
#44023 = CARTESIAN_POINT ( 'NONE',  ( -0.7185039370078760701, -0.06523048226348075740, 0.7012795275590564259 ) ) ;
#44024 = CARTESIAN_POINT ( 'NONE',  ( 0.1264236179284866091, -1.437499999946236340, -0.1264236179284866091 ) ) ;
#44025 = CARTESIAN_POINT ( 'NONE',  ( -0.6971942568897648851, 0.07405724077823318263, 1.732283464513166615 ) ) ;
#44026 = VERTEX_POINT ( 'NONE', #29085 ) ;
#44027 = CARTESIAN_POINT ( 'NONE',  ( -0.7495606340400177148, -0.1264236179284866091, 0.8735236219934803259 ) ) ;
#44028 = CARTESIAN_POINT ( 'NONE',  ( -1.054774247047244540, -0.07405724077823318263, 1.043307086560409269 ) ) ;
#44029 = CARTESIAN_POINT ( 'NONE',  ( -0.8759842519685039353, 0.1787899950787401882, 0.3518700786863940833 ) ) ;
#44030 = EDGE_CURVE ( 'NONE', #29781, #5626, #40984, .T. ) ;
#44031 = CARTESIAN_POINT ( 'NONE',  ( -0.7185039370078739607, 1.928577636452523993E-17, 0.1476377952755905387 ) ) ;
#44032 = LINE ( 'NONE', #11001, #18604 ) ;
#44033 = CARTESIAN_POINT ( 'NONE',  ( -0.9412147342319837628, 0.1574803149606300301, 0.3223425195775121432 ) ) ;
#44034 = CARTESIAN_POINT ( 'NONE',  ( 0.6971942568897626646, 0.07405724077823318263, 0.07874015742655145200 ) ) ;
#44035 = CARTESIAN_POINT ( 'NONE',  ( -0.2741699206993515880, 0.1449164722121961124, -0.7916449048462085303 ) ) ;
#44036 = CARTESIAN_POINT ( 'NONE',  ( 0.1787899950787401604, -0.3534704249221524153, 0.07405724077823318263 ) ) ;
#44037 = CARTESIAN_POINT ( 'NONE',  ( -0.2305915495022031469, -0.08955974388200925451, -0.07008671854853071315 ) ) ;
#44038 = DIRECTION ( 'NONE',  ( 0.000000000000000000, 0.000000000000000000, -1.000000000000000000 ) ) ;
#44039 = DIRECTION ( 'NONE',  ( 1.000000000000000000, 0.000000000000000000, 0.000000000000000000 ) ) ;
#44040 = PRODUCT ( 'Catch Plate', 'Catch Plate', '', ( #8939 ) ) ;
#44041 = EDGE_CURVE ( 'NONE', #3128, #47458, #6554, .T. ) ;
#44042 = ( BOUNDED_CURVE ( )  B_SPLINE_CURVE ( 2, ( #30351, #9207, #30119, #19515, #4404, #30574, #11871, #23591, #12595 ),
 .UNSPECIFIED., .F., .F. ) 
 B_SPLINE_CURVE_WITH_KNOTS ( ( 3, 2, 2, 2, 3 ),
 ( 0.1000000000000000056, 0.1024999999999999939, 0.1049999999999999961, 0.1074999999999999983, 0.1100000000000000006 ),
 .UNSPECIFIED. ) 
 CURVE ( )  GEOMETRIC_REPRESENTATION_ITEM ( )  RATIONAL_B_SPLINE_CURVE ( ( 1.000000000000000000, 0.9238795325112869605, 1.000000000000000000, 0.9238795325112869605, 1.000000000000000000, 0.9238795325112869605, 1.000000000000000000, 0.9238795325112869605, 1.000000000000000000 ) ) 
 REPRESENTATION_ITEM ( '' )  ) ;
#44043 = CARTESIAN_POINT ( 'NONE',  ( -1.002407869896990045, 0.1264236179284866091, 0.3813976377415121966 ) ) ;
#44044 = ORIENTED_EDGE ( 'NONE', *, *, #45214, .T. ) ;
#44045 = VERTEX_POINT ( 'NONE', #4091 ) ;
#44046 = CARTESIAN_POINT ( 'NONE',  ( -0.8759842519685039353, 0.1787899950787401882, 1.454232283410803017 ) ) ;
#44047 = EDGE_LOOP ( 'NONE', ( #27477, #8297, #25914, #14182 ) ) ;
#44048 = AXIS2_PLACEMENT_3D ( 'NONE', #40274, #14432, #29569 ) ;
#44049 = CARTESIAN_POINT ( 'NONE',  ( 3.284318927891251994E-17, -1.294783464513165283, 0.1787899950787401882 ) ) ;
#44050 = CARTESIAN_POINT ( 'NONE',  ( 0.1787899950787401882, -1.358759842465921297, -2.189545951927503898E-17 ) ) ;
#44051 = ( LENGTH_UNIT ( ) NAMED_UNIT ( * ) SI_UNIT ( $, .METRE. ) ) ;
#44052 = DIRECTION ( 'NONE',  ( 0.000000000000000000, 8.000000000000000622E-15, -1.000000000000000000 ) ) ;
#44053 = CARTESIAN_POINT ( 'NONE',  ( 1.033464566929134687, -0.06523048226347956391, 0.4010826771653545619 ) ) ;
#44054 = FACE_OUTER_BOUND ( 'NONE', #24082, .T. ) ;
#44055 = CARTESIAN_POINT ( 'NONE',  ( -0.7185039370078739607, 1.928577636452523993E-17, 1.043307086506645831 ) ) ;
#44056 = CARTESIAN_POINT ( 'NONE',  ( 1.054774247047244096, 0.000000000000000000, 0.4207677164816693294 ) ) ;
#44057 = CARTESIAN_POINT ( 'NONE',  ( -0.9412147342319837628, -0.1574803149606297803, 1.488681102254677535 ) ) ;
#44058 = APPLICATION_CONTEXT ( 'automotive_design' ) ;
#44059 = CARTESIAN_POINT ( 'NONE',  ( -9.642888182262618425E-18, -0.3523622047244094335, -0.1574803149606299191 ) ) ;
#44060 = DIRECTION ( 'NONE',  ( -1.000000000000000000, 0.000000000000000000, 0.000000000000000000 ) ) ;
#44061 = ORIENTED_EDGE ( 'NONE', *, *, #33199, .T. ) ;
#44062 = DIRECTION ( 'NONE',  ( -0.000000000000000000, 0.2126700594527843047, -0.9771240687918547607 ) ) ;
#44063 = CARTESIAN_POINT ( 'NONE',  ( 1.033464566929134687, -0.06523048226347956391, 0.8735236220472449853 ) ) ;
#44064 = CARTESIAN_POINT ( 'NONE',  ( 0.1642211331208078551, -0.08093396052748196012, -0.1401860130076740540 ) ) ;
#44065 = LINE ( 'NONE', #32847, #27448 ) ;
#44066 = EDGE_CURVE ( 'NONE', #19512, #24526, #62, .T. ) ;
#44068 = DIRECTION ( 'NONE',  ( 0.000000000000000000, -1.000000000000000000, 0.000000000000000000 ) ) ;
#44067 = CARTESIAN_POINT ( 'NONE',  ( 0.1574803149606299191, 0.6241017553149685870, 0.3240160679609070948 ) ) ;
#44069 = CARTESIAN_POINT ( 'NONE',  ( 0.3161444924769527542, 1.025704337919492115, -1.138861239548320858 ) ) ;
#44070 = VERTEX_POINT ( 'NONE', #32100 ) ;
#44071 = CARTESIAN_POINT ( 'NONE',  ( 1.033464566929133355, 0.06523048226348168721, 1.892224409341292546 ) ) ;
#44072 = CARTESIAN_POINT ( 'NONE',  ( -0.1377952755905511584, -1.331775896911328393E-15, 0.7066929133858274037 ) ) ;
#44073 = CARTESIAN_POINT ( 'NONE',  ( 0.07405724077823318263, -1.587598425143086800, -0.1787899950787401604 ) ) ;
#44074 = CARTESIAN_POINT ( 'NONE',  ( 0.1574803149606299191, -1.572834645561763667, -1.928577636452523993E-17 ) ) ;
#44075 = CARTESIAN_POINT ( 'NONE',  ( -0.07405724077823318263, -0.8001968503399367050, -0.1787899950787401604 ) ) ;
#44076 = CARTESIAN_POINT ( 'NONE',  ( -9.642888182262618425E-18, -1.100393700787401619, -0.1574803149606299191 ) ) ;
#44077 = CARTESIAN_POINT ( 'NONE',  ( 0.7646288533564489232, 0.1113553986120547346, 0.9990157479239685223 ) ) ;
#44078 = CARTESIAN_POINT ( 'NONE',  ( 0.1184675242425320824, -0.09842519685039370636, 1.713085361781127913 ) ) ;
#44079 = CARTESIAN_POINT ( 'NONE',  ( -0.6971942568897626646, -0.07405724077823297447, 0.3592519684501735977 ) ) ;
#44080 = EDGE_LOOP ( 'NONE', ( #46385, #34381, #12543, #4829, #41994, #16774 ) ) ;
#44081 = EDGE_LOOP ( 'NONE', ( #24216, #31769, #29324, #8483, #1755, #11352, #44903, #35389 ) ) ;
#44082 = ORIENTED_EDGE ( 'NONE', *, *, #13330, .T. ) ;
#44083 = CARTESIAN_POINT ( 'NONE',  ( -0.8019270111902717657, 0.1787899950787401604, 1.574803149552536530 ) ) ;
#44084 = EDGE_CURVE ( 'NONE', #6378, #3012, #34175, .T. ) ;
#44085 = CARTESIAN_POINT ( 'NONE',  ( 0.8019270111902717657, 0.1787899950787401604, 1.771653543253322249 ) ) ;
#44086 = CARTESIAN_POINT ( 'NONE',  ( -0.7495606340400177148, 0.1264236179284866091, 0.8292322834108031282 ) ) ;
#44087 = CARTESIAN_POINT ( 'NONE',  ( -0.1063536270749164125, -0.2340938383370582132, -0.3144333452974441556 ) ) ;
#44088 = CARTESIAN_POINT ( 'NONE',  ( 1.054774247047244540, -0.07405724077823318263, 0.3001968503399373711 ) ) ;
#44089 = CARTESIAN_POINT ( 'NONE',  ( -1.033464566929134687, 0.06523048226347956391, 0.2485236220472441526 ) ) ;
#44090 = CARTESIAN_POINT ( 'NONE',  ( -0.7495606340400177148, -0.1264236179284866091, 1.267224409395055096 ) ) ;
#44091 = CARTESIAN_POINT ( 'NONE',  ( -1.054774247047244096, 0.000000000000000000, 0.7701771653005669016 ) ) ;
#44092 = DIRECTION ( 'NONE',  ( 1.822029033848725028E-16, 0.000000000000000000, 1.000000000000000000 ) ) ;
#44093 = EDGE_CURVE ( 'NONE', #41784, #35698, #4970, .T. ) ;
#44094 = CARTESIAN_POINT ( 'NONE',  ( 0.8759842519685039353, 0.000000000000000000, 4.498031496062992574 ) ) ;
#44095 = CARTESIAN_POINT ( 'NONE',  ( -0.6971942568897648851, 0.07405724077823318263, 1.579724409395055318 ) ) ;
#44096 = CARTESIAN_POINT ( 'NONE',  ( -1.033464566929133799, 0.000000000000000000, 1.929133858160188897 ) ) ;
#44097 = ORIENTED_EDGE ( 'NONE', *, *, #31884, .F. ) ;
#44098 = CARTESIAN_POINT ( 'NONE',  ( 0.000000000000000000, 0.1102362204724409434, 0.000000000000000000 ) ) ;
#44099 = CARTESIAN_POINT ( 'NONE',  ( -1.033464566929133799, 0.000000000000000000, 1.584645669291338654 ) ) ;
#44100 = CARTESIAN_POINT ( 'NONE',  ( 0.8070866141732283561, -0.0009842519685049383633, -0.6590551181102368705 ) ) ;
#44101 = CARTESIAN_POINT ( 'NONE',  ( 1.002407869896990045, 0.1264236179284866091, 1.449311023568283341 ) ) ;
#44102 = CARTESIAN_POINT ( 'NONE',  ( -0.009589690922603031839, -0.09851384308256634637, -0.1896418766835074876 ) ) ;
#44103 = CARTESIAN_POINT ( 'NONE',  ( -0.7185039370078746268, -0.06523048226347956391, 1.567421259842519454 ) ) ;
#44104 = VERTEX_POINT ( 'NONE', #46222 ) ;
#44105 = EDGE_CURVE ( 'NONE', #35698, #29740, #17240, .T. ) ;
#44106 = CARTESIAN_POINT ( 'NONE',  ( -0.2471922904502826535, 0.05203836715090711523, -0.1197978718290576422 ) ) ;
#44107 = EDGE_CURVE ( 'NONE', #34169, #8469, #22185, .T. ) ;
#44108 = ORIENTED_EDGE ( 'NONE', *, *, #44030, .F. ) ;
#44109 = ORIENTED_EDGE ( 'NONE', *, *, #24244, .F. ) ;
#44110 = CARTESIAN_POINT ( 'NONE',  ( -0.1787899950787401882, -0.8715551180564724554, 0.000000000000000000 ) ) ;
#44111 = CARTESIAN_POINT ( 'NONE',  ( -0.1264236179284866091, -0.4335629920722205433, 0.1264236179284866091 ) ) ;
#44112 = CARTESIAN_POINT ( 'NONE',  ( -0.1787899950787401604, -0.9429133857730090940, 0.07405724077823318263 ) ) ;
#44113 = CARTESIAN_POINT ( 'NONE',  ( -0.4330708661417337901, 0.1574803149606330277, 1.186023622047244208 ) ) ;
#44114 = CARTESIAN_POINT ( 'NONE',  ( 0.1797182628040039365, -0.1388233371421006002, -2.200913952912460540E-17 ) ) ;
#44115 = CARTESIAN_POINT ( 'NONE',  ( 0.1264236179284866091, -0.02017716530056720692, -0.1264236179284866091 ) ) ;
#44116 = CARTESIAN_POINT ( 'NONE',  ( 0.000000000000000000, -0.09842519685039370636, 0.000000000000000000 ) ) ;
#44117 = CARTESIAN_POINT ( 'NONE',  ( 0.6971942568897626646, 0.07405724077823318263, 0.7480314960092282472 ) ) ;
#44119 = CARTESIAN_POINT ( 'NONE',  ( 0.5358894627757212481, 4.766607801171850497E-17, 0.000000000000000000 ) ) ;
#44118 = DIRECTION ( 'NONE',  ( 0.000000000000000000, -1.000000000000000000, 0.000000000000000000 ) ) ;
#44120 = DIRECTION ( 'NONE',  ( 0.000000000000000000, -0.7880107536067207930, 0.6156614753256597350 ) ) ;
#44121 = CARTESIAN_POINT ( 'NONE',  ( 0.6971942568897648851, 0.07405724077823318263, 1.894685039316315489 ) ) ;
#44123 = DIRECTION ( 'NONE',  ( 1.822029033848725028E-16, 0.000000000000000000, 1.000000000000000000 ) ) ;
#44122 = LINE ( 'NONE', #8355, #11538 ) ;
#44124 = ADVANCED_FACE ( 'NONE', ( #28277 ), #28054, .T. ) ;
#44125 = CARTESIAN_POINT ( 'NONE',  ( 0.9873396505805591694, 0.1113553986120547346, 0.1328740157480315098 ) ) ;
#44126 = CARTESIAN_POINT ( 'NONE',  ( 4.681852760415787419E-17, -0.03219022224904102836, 0.2854330708661417804 ) ) ;
#44127 = CARTESIAN_POINT ( 'NONE',  ( 0.1264236179284866091, -0.2662401574265516047, 0.1264236179284866091 ) ) ;
#44129 = CARTESIAN_POINT ( 'NONE',  ( 0.5962569168439626477, 0.09842519685039370636, 0.000000000000000000 ) ) ;
#44128 = CARTESIAN_POINT ( 'NONE',  ( -0.8759842519685039353, -0.1787899950787401882, 0.4896653542769449086 ) ) ;
#44130 = CARTESIAN_POINT ( 'NONE',  ( 0.1787899950787401604, -1.001968503883243988, -0.07405724077823318263 ) ) ;
#44131 = CARTESIAN_POINT ( 'NONE',  ( 0.8019270111902717657, 0.1787899950787401604, 0.3149606298674962890 ) ) ;
#44132 = CARTESIAN_POINT ( 'NONE',  ( 0.1638066842825940672, 0.08057053547025881668, -0.1395522881968654649 ) ) ;
#44133 = CARTESIAN_POINT ( 'NONE',  ( 0.8019270111902716547, -0.1787899950787401604, 0.5610236219934807700 ) ) ;
#44134 = ADVANCED_FACE ( 'NONE', ( #6674 ), #13197, .T. ) ;
#44135 = CARTESIAN_POINT ( 'NONE',  ( -0.9500414927467378812, 0.1787899950787401604, 1.604330708607653921 ) ) ;
#44136 = EDGE_LOOP ( 'NONE', ( #35905, #43796, #40867, #4305 ) ) ;
#44137 = ADVANCED_FACE ( 'NONE', ( #21292 ), #40244, .T. ) ;
#44138 = CARTESIAN_POINT ( 'NONE',  ( 0.7495606340400177148, 0.1264236179284866091, 1.262303149552535420 ) ) ;
#44139 = CARTESIAN_POINT ( 'NONE',  ( 2.892866454678787531E-17, -1.188976377845228471, 0.1574803149606299191 ) ) ;
#44140 = CARTESIAN_POINT ( 'NONE',  ( -0.8759842519685039353, -0.1787899950787401882, 1.035925196796629866 ) ) ;
#44141 = CARTESIAN_POINT ( 'NONE',  ( 0.1644020957507537628, 0.08115590401245532937, -0.1405661490837558925 ) ) ;
#44142 = CARTESIAN_POINT ( 'NONE',  ( -0.1964094517284886710, -0.1820971824355780422, -0.05295753290290854814 ) ) ;
#44143 = CARTESIAN_POINT ( 'NONE',  ( -0.7495606340400177148, 0.1264236179284866091, 0.1943897637257641919 ) ) ;
#44144 = PRODUCT_DEFINITION_CONTEXT ( 'detailed design', #20485, 'design' ) ;
#44145 = CARTESIAN_POINT ( 'NONE',  ( -1.054774247047244540, 0.07405724077823318263, 0.7332677164816707727 ) ) ;
#44146 = CARTESIAN_POINT ( 'NONE',  ( 0.7185039370078739607, 1.928577636452523993E-17, 1.673228346349165285 ) ) ;
#44147 = VERTEX_POINT ( 'NONE', #45989 ) ;
#44148 = DIRECTION ( 'NONE',  ( 0.000000000000000000, 0.000000000000000000, 1.000000000000000000 ) ) ;
#44149 = VERTEX_POINT ( 'NONE', #20824 ) ;
#44150 = CARTESIAN_POINT ( 'NONE',  ( 1.054774247047244540, -0.07405724077823318263, 1.126968503883244654 ) ) ;
#44151 = CARTESIAN_POINT ( 'NONE',  ( -0.8759842519685039353, 0.1787899950787401882, 1.803641732229700700 ) ) ;
#44152 = ORIENTED_EDGE ( 'NONE', *, *, #14197, .F. ) ;
#44153 = CARTESIAN_POINT ( 'NONE',  ( 0.8019270111902717657, 0.1787899950787401604, 1.963582677111591401 ) ) ;
#44154 = ( BOUNDED_CURVE ( )  B_SPLINE_CURVE ( 2, ( #17382, #577, #26735, #1057, #353, #43967, #33701, #7782, #8017 ),
 .UNSPECIFIED., .F., .T. ) 
 B_SPLINE_CURVE_WITH_KNOTS ( ( 3, 2, 2, 2, 3 ),
 ( 0.4600000000000000200, 0.4625000000000000222, 0.4650000000000000244, 0.4675000000000000266, 0.4699999999999999734 ),
 .UNSPECIFIED. ) 
 CURVE ( )  GEOMETRIC_REPRESENTATION_ITEM ( )  RATIONAL_B_SPLINE_CURVE ( ( 1.000000000000000000, 0.9238795325112869605, 1.000000000000000000, 0.9238795325112869605, 1.000000000000000000, 0.9238795325112869605, 1.000000000000000000, 0.9238795325112849621, 1.000000000000000000 ) ) 
 REPRESENTATION_ITEM ( '' )  ) ;
#44155 = CARTESIAN_POINT ( 'NONE',  ( 0.7185039370078739607, 1.928577636452523993E-17, 0.7381889763779527769 ) ) ;
#44156 = CARTESIAN_POINT ( 'NONE',  ( 0.1787899950787401604, -1.411541291063884929, -0.07405724077823318263 ) ) ;
#44157 = ORIENTED_EDGE ( 'NONE', *, *, #13985, .F. ) ;
#44158 = CARTESIAN_POINT ( 'NONE',  ( -1.094772975963752103E-17, -0.2859251967966303098, -0.1787899950787401882 ) ) ;
#44159 = DIRECTION ( 'NONE',  ( 0.000000000000000000, -1.000000000000000000, 0.000000000000000000 ) ) ;
#44160 = ORIENTED_EDGE ( 'NONE', *, *, #37703, .F. ) ;
#44161 = CARTESIAN_POINT ( 'NONE',  ( 1.054774247047244540, -0.07405724077823318263, 1.200787401521039355 ) ) ;
#44162 = AXIS2_PLACEMENT_3D ( 'NONE', #33446, #561, #22385 ) ;
#44163 = DIRECTION ( 'NONE',  ( -0.000000000000000000, -0.000000000000000000, -1.000000000000000000 ) ) ;
#44164 = CARTESIAN_POINT ( 'NONE',  ( 0.9500414927467378812, 0.1787899950787401604, 0.1476377952218271561 ) ) ;
#44165 = APPLICATION_PROTOCOL_DEFINITION ( 'draft international standard', 'automotive_design', 1998, #37994 ) ;
#44166 = CARTESIAN_POINT ( 'NONE',  ( -0.8019270111902716547, -0.1787899950787401604, 0.4478346456155276045 ) ) ;
#44167 = B_SPLINE_CURVE_WITH_KNOTS ( 'NONE', 3,
 ( #45524, #12748, #15863, #5769, #45049, #20374, #27611, #9612, #23521, #38126, #41920, #26886, #9129 ),
 .UNSPECIFIED., .F., .F.,
 ( 4, 2, 2, 1, 2, 2, 4 ),
 ( 0.000000000000000000, 0.2499999999999980016, 0.3749999999999974465, 0.4374999999999968914, 0.4687499999999968359, 0.4999999999999968914, 1.000000000000000000 ),
 .UNSPECIFIED. ) ;
#44168 = CARTESIAN_POINT ( 'NONE',  ( 0.7185039370078746268, 0.06523048226347956391, 0.3813976377952755237 ) ) ;
#44169 = CARTESIAN_POINT ( 'NONE',  ( -0.1270800023317771588, -1.413429636354698760, 0.1270800023317771588 ) ) ;
#44170 = CARTESIAN_POINT ( 'NONE',  ( 1.033464566929133799, 0.000000000000000000, 0.7480314959554645871 ) ) ;
#44171 = CARTESIAN_POINT ( 'NONE',  ( 0.6971942568897648851, -0.07405724077823297447, 1.387795275536786610 ) ) ;
#44172 = CARTESIAN_POINT ( 'NONE',  ( 0.8759842519685039353, -0.1787899950787401882, 1.744586614119464807 ) ) ;
#44174 = ADVANCED_FACE ( 'NONE', ( #24212 ), #35238, .T. ) ;
#44173 = CARTESIAN_POINT ( 'NONE',  ( -0.7185039370078739607, 0.000000000000000000, -2.869337061179095023E-17 ) ) ;
#44175 = FACE_OUTER_BOUND ( 'NONE', #2650, .T. ) ;
#44176 = CARTESIAN_POINT ( 'NONE',  ( -0.8759842519685039353, 0.000000000000000000, 0.000000000000000000 ) ) ;
#44177 = CARTESIAN_POINT ( 'NONE',  ( -0.8107537697050254399, -0.1574803149606297803, 1.021161417322834497 ) ) ;
#44178 = CARTESIAN_POINT ( 'NONE',  ( 1.033464566929134687, 0.06523048226347956391, 0.7504921258767240921 ) ) ;
#44179 = CARTESIAN_POINT ( 'NONE',  ( 1.002407869896990045, -0.1264236179284866091, 0.2534448818360003908 ) ) ;
#44180 = EDGE_CURVE ( 'NONE', #21943, #28102, #45567, .T. ) ;
#44181 = CARTESIAN_POINT ( 'NONE',  ( 0.7020369131201283919, 0.02831345972461313948, 0.03937007867491748581 ) ) ;
#44182 = DIRECTION ( 'NONE',  ( 0.000000000000000000, -1.000000000000000000, 0.000000000000000000 ) ) ;
#44183 = LINE ( 'NONE', #37726, #34536 ) ;
#44184 = CARTESIAN_POINT ( 'NONE',  ( -0.9500414927467378812, -0.1787899950787401604, 1.274606299158834277 ) ) ;
#44185 = CARTESIAN_POINT ( 'NONE',  ( 0.7185039370078746268, -0.06523048226347956391, 0.6914370077664893088 ) ) ;
#44186 = ORIENTED_EDGE ( 'NONE', *, *, #11662, .T. ) ;
#44187 = EDGE_CURVE ( 'NONE', #21109, #21208, #28765, .T. ) ;
#44188 = CARTESIAN_POINT ( 'NONE',  ( -0.1775997780303593676, -0.4232972401690973108, -0.9812951153858839870 ) ) ;
#44189 = EDGE_LOOP ( 'NONE', ( #38396, #29097, #6058, #32684, #39137 ) ) ;
#44190 = CARTESIAN_POINT ( 'NONE',  ( 0.1797182628040039087, -0.1019138883232029447, 0.07444174185955046430 ) ) ;
#44191 = FACE_OUTER_BOUND ( 'NONE', #3203, .T. ) ;
#44192 = CARTESIAN_POINT ( 'NONE',  ( 0.1113553986120547346, -1.065944881782236342, 0.1113553986120547346 ) ) ;
#44193 = CARTESIAN_POINT ( 'NONE',  ( -1.033464566929133799, 0.000000000000000000, 0.03937007874015843040 ) ) ;
#44194 = CARTESIAN_POINT ( 'NONE',  ( 0.8759842519685039353, 0.1787899950787401882, 1.646161417269070837 ) ) ;
#44195 = EDGE_CURVE ( 'NONE', #2533, #9932, #8874, .T. ) ;
#44196 = DIRECTION ( 'NONE',  ( 0.000000000000000000, 0.000000000000000000, 1.000000000000000000 ) ) ;
#44197 = CARTESIAN_POINT ( 'NONE',  ( 0.1571385178022373375, -0.1334669528785105419, 0.04962495032677907009 ) ) ;
#44198 = CARTESIAN_POINT ( 'NONE',  ( 3.284318927891251994E-17, -0.1481299212060791237, 0.1787899950787401882 ) ) ;
#44199 = EDGE_LOOP ( 'NONE', ( #21642, #10827, #34632, #22515 ) ) ;
#44200 = AXIS2_PLACEMENT_3D ( 'NONE', #13552, #28188, #17375 ) ;
#44201 = CYLINDRICAL_SURFACE ( 'NONE', #47433, 0.1574803149606299191 ) ;
#44202 = DIRECTION ( 'NONE',  ( -1.000000000000000000, 1.776356839400250070E-15, 0.000000000000000000 ) ) ;
#44203 = ORIENTED_EDGE ( 'NONE', *, *, #11607, .F. ) ;
#44204 = VERTEX_POINT ( 'NONE', #17936 ) ;
#44205 = CARTESIAN_POINT ( 'NONE',  ( -1.054774247047244540, -0.07405724077823318263, 1.476377952702141449 ) ) ;
#44206 = CARTESIAN_POINT ( 'NONE',  ( -0.06523048226347956391, 0.1323818898713065573, -0.1574803149606300301 ) ) ;
#44207 = CARTESIAN_POINT ( 'NONE',  ( -1.054774247047244540, -0.07405724077823318263, 1.284448818843874740 ) ) ;
#44208 = CARTESIAN_POINT ( 'NONE',  ( -0.2559055118110236116, -0.08272504999148638793, -0.05533579728309570567 ) ) ;
#44209 = DIRECTION ( 'NONE',  ( 0.000000000000000000, 0.000000000000000000, -1.000000000000000000 ) ) ;
#44210 = CARTESIAN_POINT ( 'NONE',  ( -1.054774247047244540, 0.07405724077823318263, 0.2657480314422993595 ) ) ;
#44211 = CARTESIAN_POINT ( 'NONE',  ( 0.006378642920472008850, 0.1475107277141399220, -0.02009854774567082850 ) ) ;
#44212 = DIRECTION ( 'NONE',  ( 0.000000000000000000, 0.000000000000000000, -1.000000000000000000 ) ) ;
#44213 = CARTESIAN_POINT ( 'NONE',  ( 0.1787899950787401604, -0.7816200312213649193, -0.07405724077823318263 ) ) ;
#44214 = ORIENTED_EDGE ( 'NONE', *, *, #4698, .T. ) ;
#44215 = CARTESIAN_POINT ( 'NONE',  ( 0.9873396505805591694, -0.1113553986120547346, 1.067913385826771755 ) ) ;
#44216 = ORIENTED_EDGE ( 'NONE', *, *, #27476, .T. ) ;
#44217 = CARTESIAN_POINT ( 'NONE',  ( 0.9500414927467378812, 0.1787899950787401604, 1.013779527505291878 ) ) ;
#44218 = DIRECTION ( 'NONE',  ( -1.000000000000000000, 3.469446951953613794E-15, 0.000000000000000000 ) ) ;
#44219 = CARTESIAN_POINT ( 'NONE',  ( -0.8759842519685039353, -0.1787899950787401882, 0.7997047243556849594 ) ) ;
#44220 = AXIS2_PLACEMENT_3D ( 'NONE', #5471, #9314, #4997 ) ;
#44221 = CARTESIAN_POINT ( 'NONE',  ( -0.8759842519685039353, -0.1787899950787401882, 1.828248031442299082 ) ) ;
#44222 = CARTESIAN_POINT ( 'NONE',  ( -0.1787899950787401882, -0.5172244093950552069, 0.000000000000000000 ) ) ;
#44223 = DIRECTION ( 'NONE',  ( 0.5735764363510447161, -0.8191520442889925757, 1.003171929053525486E-16 ) ) ;
#44224 = CARTESIAN_POINT ( 'NONE',  ( -0.7646288533564489232, -0.1113553986120547346, 0.8612204724409449064 ) ) ;
#44225 = CARTESIAN_POINT ( 'NONE',  ( 0.1476377952755906220, 0.07021257666615010606, -0.1553045758542774823 ) ) ;
#44226 = CARTESIAN_POINT ( 'NONE',  ( -0.1270800023317771588, -1.068941447378320975, -0.1270800023317771588 ) ) ;
#44227 = LINE ( 'NONE', #26049, #6454 ) ;
#44228 = CARTESIAN_POINT ( 'NONE',  ( -0.7185039370078739607, 1.928577636452523993E-17, 1.476377952648377789 ) ) ;
#44229 = CARTESIAN_POINT ( 'NONE',  ( 1.054774247047244540, -0.07405724077823318263, 0.8513779527021426707 ) ) ;
#44230 = DIRECTION ( 'NONE',  ( 0.000000000000000000, -0.6156614753256584027, -0.7880107536067220142 ) ) ;
#44231 = CARTESIAN_POINT ( 'NONE',  ( 0.7185039370078746268, -0.06523048226347956391, 1.370570866141733291 ) ) ;
#44233 = CARTESIAN_POINT ( 'NONE',  ( 0.7185039370078739607, 1.928577636452523993E-17, 1.555118110128692832 ) ) ;
#44232 = CARTESIAN_POINT ( 'NONE',  ( 0.7316628141368787253, 0.07653111172288938613, 1.981731121241584015 ) ) ;
#44234 = CARTESIAN_POINT ( 'NONE',  ( 0.3123359580052492146, 4.616380251121755931E-17, 0.000000000000000000 ) ) ;
#44235 = ADVANCED_FACE ( 'NONE', ( #22713 ), #3793, .T. ) ;
#44237 = CARTESIAN_POINT ( 'NONE',  ( 0.1596650774283338570, 0.09389790430995964554, 0.1183119828675037455 ) ) ;
#44236 = CARTESIAN_POINT ( 'NONE',  ( 1.054774247047244540, 0.07405724077823318263, 0.8907480314422985268 ) ) ;
#44238 = CARTESIAN_POINT ( 'NONE',  ( -0.1787899950787401882, -0.7485236219934803259, 0.000000000000000000 ) ) ;
#44239 = LINE ( 'NONE', #11921, #35352 ) ;
#44240 = ORIENTED_EDGE ( 'NONE', *, *, #36817, .T. ) ;
#44241 = CARTESIAN_POINT ( 'NONE',  ( 0.8759842519685039353, 0.1574803149606299191, 1.082677165354330784 ) ) ;
#44242 = CARTESIAN_POINT ( 'NONE',  ( -0.1574803149606299191, -0.4014847039200427070, -0.9233949158597744011 ) ) ;
#44243 = CARTESIAN_POINT ( 'NONE',  ( 1.054774247047244540, -0.07405724077823318263, 1.200787401521039355 ) ) ;
#44244 = EDGE_CURVE ( 'NONE', #3165, #11388, #18839, .T. ) ;
#44245 = CARTESIAN_POINT ( 'NONE',  ( -0.9412147342319837628, 0.1574803149606300301, 1.040846456692913424 ) ) ;
#44246 = CARTESIAN_POINT ( 'NONE',  ( 0.06523048226347956391, -1.747539370078740717, 0.1574803149606297803 ) ) ;
#44247 = CARTESIAN_POINT ( 'NONE',  ( 0.1555687797274982465, 0.1458529223346496095, -0.02296587926509184932 ) ) ;
#44248 = AXIS2_PLACEMENT_3D ( 'NONE', #25540, #36317, #43950 ) ;
#44249 = VERTEX_POINT ( 'NONE', #22231 ) ;
#44250 = CARTESIAN_POINT ( 'NONE',  ( 0.8759842519685039353, 0.000000000000000000, 4.498031496062992574 ) ) ;
#44251 = CARTESIAN_POINT ( 'NONE',  ( -1.054774247047244540, -0.07405724077823318263, 0.1771653542769450751 ) ) ;
#44252 = EDGE_LOOP ( 'NONE', ( #20999, #36784 ) ) ;
#44253 = CARTESIAN_POINT ( 'NONE',  ( 0.8759842519685039353, 0.1574803149606299191, 0.3346456692913385988 ) ) ;
#44254 = B_SPLINE_CURVE_WITH_KNOTS ( 'NONE', 3,
 ( #46214, #45979, #16540, #30700, #45265, #27588, #7150, #21285, #28758, #46926, #14354, #20818, #10045, #47170, #6902, #35457, #9820, #32092, #39257, #31868 ),
 .UNSPECIFIED., .F., .F.,
 ( 4, 1, 1, 1, 1, 1, 2, 2, 1, 1, 1, 2, 2, 4 ),
 ( 0.000000000000000000, 0.2499999999999940048, 0.3749999999999910072, 0.4374999999999891753, 0.4687499999999880096, 0.4843749999999875655, 0.4921874999999874545, 0.4999999999999873990, 0.6249999999999876765, 0.6874999999999874545, 0.7187499999999875655, 0.7343749999999877875, 0.7499999999999881206, 1.000000000000000000 ),
 .UNSPECIFIED. ) ;
#44255 = CARTESIAN_POINT ( 'NONE',  ( -0.8759842519685039353, -0.1787899950787401882, 1.665846456639149764 ) ) ;
#44256 = CARTESIAN_POINT ( 'NONE',  ( -1.054774247047244540, -0.07405724077823318263, 0.9251968503399373711 ) ) ;
#44257 = VECTOR ( 'NONE', #41900, 39.37007874015748143 ) ;
#44258 = CARTESIAN_POINT ( 'NONE',  ( -1.002407869896990045, -0.1264236179284866091, 0.3371062991588349989 ) ) ;
#44259 = DIRECTION ( 'NONE',  ( 0.000000000000000000, 0.000000000000000000, -1.000000000000000000 ) ) ;
#44260 = DIRECTION ( 'NONE',  ( -0.000000000000000000, -0.000000000000000000, -1.000000000000000000 ) ) ;
#44261 = DIRECTION ( 'NONE',  ( -0.000000000000000000, -0.000000000000000000, -1.000000000000000000 ) ) ;
#44262 = CARTESIAN_POINT ( 'NONE',  ( -8.354793841626791791E-17, 0.03219022224904082713, -0.2854330708661417804 ) ) ;
#44263 = CARTESIAN_POINT ( 'NONE',  ( -0.5555748031496026140, 1.194414586609142903, -0.06082000038405787484 ) ) ;
#44264 = CARTESIAN_POINT ( 'NONE',  ( -0.08276828494985000173, -0.08956000829960196474, 0.2091008467216779743 ) ) ;
#44265 = CARTESIAN_POINT ( 'NONE',  ( -0.2471922904502826812, -0.09842519685039370636, 0.1427165354330708902 ) ) ;
#44266 = DIRECTION ( 'NONE',  ( 0.000000000000000000, 1.000000000000000000, 0.000000000000000000 ) ) ;
#44267 = CARTESIAN_POINT ( 'NONE',  ( -1.002407869896990045, 0.1264236179284866091, 0.2632874015210397434 ) ) ;
#44268 = ORIENTED_EDGE ( 'NONE', *, *, #34263, .T. ) ;
#44269 = CARTESIAN_POINT ( 'NONE',  ( -1.054774247047244096, 0.000000000000000000, 1.326279527505291433 ) ) ;
#44270 = ORIENTED_EDGE ( 'NONE', *, *, #10580, .F. ) ;
#44271 = CARTESIAN_POINT ( 'NONE',  ( -0.1264236179284866091, -1.339074803095842592, 0.1264236179284866091 ) ) ;
#44272 = CARTESIAN_POINT ( 'NONE',  ( 0.1787899950787401604, -1.553149606245448178, -0.07405724077823318263 ) ) ;
#44273 = DIRECTION ( 'NONE',  ( -1.000000000000000000, 0.000000000000000000, 0.000000000000000000 ) ) ;
#44274 = CARTESIAN_POINT ( 'NONE',  ( 0.7185039370078746268, -0.06523048226347956391, 0.4256889763779528324 ) ) ;
#44275 = CARTESIAN_POINT ( 'NONE',  ( 1.181102362204724310, -0.3937007874015748254, 0.9842519685039370358 ) ) ;
#44276 = CARTESIAN_POINT ( 'NONE',  ( -1.033464566929134687, 0.06523048226347956391, 1.065452755797984041 ) ) ;
#44277 = CONICAL_SURFACE ( 'NONE', #18280, 0.09842519685039370636, 0.9599310885968824758 ) ;
#44278 = CARTESIAN_POINT ( 'NONE',  ( 0.9500414927467378812, -0.1787899950787401604, 0.4527559054580477249 ) ) ;
#44279 = CARTESIAN_POINT ( 'NONE',  ( 0.7185039370078746268, 0.06523048226347956391, 0.5684055117034967353 ) ) ;
#44280 = CARTESIAN_POINT ( 'NONE',  ( 0.1113553986120547346, -0.2490157480314960647, 0.1113553986120547346 ) ) ;
#44281 = CARTESIAN_POINT ( 'NONE',  ( 0.9873396505805591694, -0.1113553986120547346, 1.924212598317669221 ) ) ;
#44282 = ORIENTED_EDGE ( 'NONE', *, *, #3693, .T. ) ;
#44283 = FACE_OUTER_BOUND ( 'NONE', #13065, .T. ) ;
#44284 = CARTESIAN_POINT ( 'NONE',  ( -0.9500414927467377701, 0.1787899950787401604, 0.9005905511273391006 ) ) ;
#44285 = CARTESIAN_POINT ( 'NONE',  ( 0.8107537697050253289, 0.1574803149606300301, 0.9276574803149607584 ) ) ;
#44286 = VECTOR ( 'NONE', #30882, 39.37007874015748143 ) ;
#44287 = DIRECTION ( 'NONE',  ( 1.000000000000000000, -3.368395098984090098E-15, 0.000000000000000000 ) ) ;
#44288 = CARTESIAN_POINT ( 'NONE',  ( -0.1113553986120547346, -0.5639763778452283605, 0.1113553986120547346 ) ) ;
#44289 = EDGE_CURVE ( 'NONE', #28784, #31929, #36864, .T. ) ;
#44290 = CARTESIAN_POINT ( 'NONE',  ( -0.7185039370078760701, -0.06523048226348075740, 0.8193897637795283240 ) ) ;
#44291 = CARTESIAN_POINT ( 'NONE',  ( -0.1694883852340978991, -0.08955000340450794405, 0.001402097216817517434 ) ) ;
#44292 = CARTESIAN_POINT ( 'NONE',  ( 0.000000000000000000, 0.000000000000000000, -0.3149606299212598381 ) ) ;
#44293 = VERTEX_POINT ( 'NONE', #14589 ) ;
#44294 = CARTESIAN_POINT ( 'NONE',  ( 0.8759842519685039353, 0.1787899950787401882, 0.6619094487651338010 ) ) ;
#44295 = ADVANCED_FACE ( 'NONE', ( #14828 ), #37091, .T. ) ;
#44296 = ORIENTED_EDGE ( 'NONE', *, *, #14723, .F. ) ;
#44297 = CARTESIAN_POINT ( 'NONE',  ( -0.8759842519685039353, 0.1574803149606299191, 1.781496062884598164 ) ) ;
#44298 = DIRECTION ( 'NONE',  ( 0.000000000000000000, 0.000000000000000000, -1.000000000000000000 ) ) ;
#44299 = CARTESIAN_POINT ( 'NONE',  ( 3.284318927891251994E-17, -1.604822834591905556, 0.1787899950787401882 ) ) ;
#44300 = CARTESIAN_POINT ( 'NONE',  ( 0.1787899950787401604, -0.7312992125446612368, -0.07405724077823318263 ) ) ;
#44301 = CARTESIAN_POINT ( 'NONE',  ( 0.1113553986120547346, -1.184055118110236338, -0.1113553986120547346 ) ) ;
#44302 = CARTESIAN_POINT ( 'NONE',  ( 0.7185039370078746268, 0.06523048226347956391, 1.080216535325543958 ) ) ;
#44303 = CARTESIAN_POINT ( 'NONE',  ( 0.000000000000000000, 0.000000000000000000, 1.181102362204724310 ) ) ;
#44304 = CARTESIAN_POINT ( 'NONE',  ( -0.6971942568897626646, -0.07405724077823297447, 0.4773622046706456068 ) ) ;
#44305 = ORIENTED_EDGE ( 'NONE', *, *, #41233, .T. ) ;
#44306 = ORIENTED_EDGE ( 'NONE', *, *, #21420, .F. ) ;
#44307 = ORIENTED_EDGE ( 'NONE', *, *, #24160, .F. ) ;
#44308 = CARTESIAN_POINT ( 'NONE',  ( -1.054774247047244540, -0.07405724077823318263, 1.717519684985606476 ) ) ;
#44309 = CARTESIAN_POINT ( 'NONE',  ( 1.054774247047244096, 0.000000000000000000, 1.680610236166708793 ) ) ;
#44310 = CARTESIAN_POINT ( 'NONE',  ( -0.1574803149606297803, -1.314468503829480550, 0.06523048226347956391 ) ) ;
#44311 = CARTESIAN_POINT ( 'NONE',  ( -0.8759842519685039353, -0.1787899950787401882, 0.7258858267178898149 ) ) ;
#44312 = CARTESIAN_POINT ( 'NONE',  ( 0.2759478392031586291, 0.3740157480314960647, 1.224299699984019663 ) ) ;
#44313 = CARTESIAN_POINT ( 'NONE',  ( 0.7495606340400177148, -0.1264236179284866091, 0.2485236219934806867 ) ) ;
#44314 = CARTESIAN_POINT ( 'NONE',  ( -0.9500414927467377701, -0.1787899950787401604, 1.195866141678520345 ) ) ;
#44315 = CARTESIAN_POINT ( 'NONE',  ( -0.9500414927467377701, -0.1787899950787401604, 0.8021653542769462408 ) ) ;
#44316 = CARTESIAN_POINT ( 'NONE',  ( 0.1113553986120547346, -0.07185039359326043928, -0.1113553986120547346 ) ) ;
#44317 = ( BOUNDED_CURVE ( )  B_SPLINE_CURVE ( 2, ( #29894, #33001, #44913, #123, #33242, #43984, #44672, #25800, #29673 ),
 .UNSPECIFIED., .F., .T. ) 
 B_SPLINE_CURVE_WITH_KNOTS ( ( 3, 2, 2, 2, 3 ),
 ( 0.3300000000000000155, 0.3325000000000000178, 0.3350000000000000200, 0.3375000000000000222, 0.3400000000000000244 ),
 .UNSPECIFIED. ) 
 CURVE ( )  GEOMETRIC_REPRESENTATION_ITEM ( )  RATIONAL_B_SPLINE_CURVE ( ( 1.000000000000000000, 0.9238795325112869605, 1.000000000000000000, 0.9238795325112869605, 1.000000000000000000, 0.9238795325112869605, 1.000000000000000000, 0.9238795325112869605, 1.000000000000000000 ) ) 
 REPRESENTATION_ITEM ( '' )  ) ;
#44318 = AXIS2_PLACEMENT_3D ( 'NONE', #40987, #30495, #12266 ) ;
#44319 = CARTESIAN_POINT ( 'NONE',  ( 0.05729443792182561251, 0.07836113345104780969, 0.2523541117089074803 ) ) ;
#44320 = CARTESIAN_POINT ( 'NONE',  ( -0.8019270111902717657, -0.1787899950787401604, 1.628937007820252303 ) ) ;
#44321 = CARTESIAN_POINT ( 'NONE',  ( -0.9873396505805591694, 0.1113553986120547346, 1.815944881782236120 ) ) ;
#44322 = EDGE_LOOP ( 'NONE', ( #27174, #16406, #9738, #31148 ) ) ;
#44323 = CARTESIAN_POINT ( 'NONE',  ( -0.8759842519685039353, 0.1574803149606299191, 1.555118110236220597 ) ) ;
#44324 = CARTESIAN_POINT ( 'NONE',  ( 0.000000000000000000, 0.000000000000000000, 0.000000000000000000 ) ) ;
#44325 = CARTESIAN_POINT ( 'NONE',  ( 0.7495606340400177148, 0.1264236179284866091, 1.459153543253322693 ) ) ;
#44326 = CARTESIAN_POINT ( 'NONE',  ( 0.09778643531992912974, -0.09851382616417500571, 0.1118397558297255928 ) ) ;
#44327 = CARTESIAN_POINT ( 'NONE',  ( 0.1574803149606299191, 0.000000000000000000, 0.000000000000000000 ) ) ;
#44328 = AXIS2_PLACEMENT_3D ( 'NONE', #10651, #3676, #14952 ) ;
#44329 = EDGE_CURVE ( 'NONE', #10268, #47403, #40200, .T. ) ;
#44330 = EDGE_LOOP ( 'NONE', ( #21537, #37982, #13183, #2130 ) ) ;
#44331 = AXIS2_PLACEMENT_3D ( 'NONE', #11935, #22937, #4707 ) ;
#44332 = ORIENTED_EDGE ( 'NONE', *, *, #34652, .T. ) ;
#44333 = CARTESIAN_POINT ( 'NONE',  ( 0.07405724077823318263, -0.8838582676627719792, -0.1787899950787401604 ) ) ;
#44334 = CARTESIAN_POINT ( 'NONE',  ( 0.1787899950787401882, -1.122539370024976391, -2.189545951927503898E-17 ) ) ;
#44335 = CARTESIAN_POINT ( 'NONE',  ( 0.1574803149606299746, -0.5708661417322835607, 0.9783464566929124251 ) ) ;
#44336 = CARTESIAN_POINT ( 'NONE',  ( 1.002407869896990045, 0.1264236179284866091, 1.759350393647023614 ) ) ;
#44337 = CARTESIAN_POINT ( 'NONE',  ( -0.1270800023317771588, -0.1240595576145415435, -0.1270800023317771588 ) ) ;
#44338 = DIRECTION ( 'NONE',  ( 0.000000000000000000, 0.000000000000000000, 1.000000000000000000 ) ) ;
#44339 = CARTESIAN_POINT ( 'NONE',  ( -0.7646288533564489232, 0.1113553986120547346, 1.077755905404283565 ) ) ;
#44340 = CARTESIAN_POINT ( 'NONE',  ( 0.8759842519685039353, -0.1787899950787401882, 0.7209645668753701386 ) ) ;
#44341 = EDGE_CURVE ( 'NONE', #30008, #22975, #11240, .T. ) ;
#44342 = CARTESIAN_POINT ( 'NONE',  ( 0.1574803149606299191, 0.1473293504822035527, -0.9532488779249704836 ) ) ;
#44344 = CARTESIAN_POINT ( 'NONE',  ( -0.2066929133858267931, -0.5253304731389190074, -0.9015780170405504057 ) ) ;
#44343 = DIRECTION ( 'NONE',  ( -0.000000000000000000, 1.000000000000000000, -0.000000000000000000 ) ) ;
#44345 = CARTESIAN_POINT ( 'NONE',  ( 1.033464566929134687, 0.06523048226347956391, 0.4453740157480309270 ) ) ;
#44346 = CARTESIAN_POINT ( 'NONE',  ( 0.1126279540338996077, -0.5708661417322835607, 1.206847064312610129 ) ) ;
#44347 = ORIENTED_EDGE ( 'NONE', *, *, #34007, .T. ) ;
#44348 = EDGE_CURVE ( 'NONE', #580, #28644, #18181, .T. ) ;
#44349 = CARTESIAN_POINT ( 'NONE',  ( 0.8107537697050253289, 0.1574803149606300301, 0.1008858267716536417 ) ) ;
#44350 = CARTESIAN_POINT ( 'NONE',  ( 0.1595442748538452582, -0.09421994677688858011, 0.1177495158649726342 ) ) ;
#44351 = CARTESIAN_POINT ( 'NONE',  ( 0.1787899950787401604, -0.2194881889226144023, -0.07405724077823318263 ) ) ;
#44352 = CARTESIAN_POINT ( 'NONE',  ( -0.7646288533564489232, 0.1113553986120547346, 0.1820866141732283561 ) ) ;
#44353 = CARTESIAN_POINT ( 'NONE',  ( 0.07405724077823318263, -1.233267716481668774, -0.1787899950787401604 ) ) ;
#44354 = CARTESIAN_POINT ( 'NONE',  ( 1.054774247047244096, 0.000000000000000000, 0.1845472440407248116 ) ) ;
#44355 = CARTESIAN_POINT ( 'NONE',  ( 0.7185039370078739607, 1.928577636452523993E-17, 0.06889763779527559306 ) ) ;
#44356 = CARTESIAN_POINT ( 'NONE',  ( -1.002407869896990045, 0.1264236179284866091, 1.798720472387181024 ) ) ;
#44357 = VERTEX_POINT ( 'NONE', #3567 ) ;
#44358 = CARTESIAN_POINT ( 'NONE',  ( -0.7495606340400177148, 0.1264236179284866091, 1.183562992072220599 ) ) ;
#44359 = DIRECTION ( 'NONE',  ( 1.822029033848725028E-16, 0.000000000000000000, 1.000000000000000000 ) ) ;
#44360 = CARTESIAN_POINT ( 'NONE',  ( 0.6971942568897648851, -0.07405724077823297447, 1.269685039316314601 ) ) ;
#44361 = CARTESIAN_POINT ( 'NONE',  ( 0.1574803149606300301, -1.176673228238929614, -0.06523048226347956391 ) ) ;
#44362 = CARTESIAN_POINT ( 'NONE',  ( 0.9500414927467378812, -0.1787899950787401604, 1.983267716481667886 ) ) ;
#44363 = CARTESIAN_POINT ( 'NONE',  ( -0.8759842519685039353, 0.1787899950787401882, 1.134350393647023614 ) ) ;
#44364 = CARTESIAN_POINT ( 'NONE',  ( -0.1519198807041087229, -0.09842519685039373412, -0.09441072998970326258 ) ) ;
#44365 = DIRECTION ( 'NONE',  ( 0.000000000000000000, 0.000000000000000000, -1.000000000000000000 ) ) ;
#44366 = CARTESIAN_POINT ( 'NONE',  ( 0.6971942568897637749, 2.189545951927499583E-17, 0.4798228345919055560 ) ) ;
#44367 = CARTESIAN_POINT ( 'NONE',  ( -0.8759842519685039353, -0.1787899950787401882, 0.3666338582139531677 ) ) ;
#44368 = CARTESIAN_POINT ( 'NONE',  ( -0.9500414927467378812, 0.1787899950787401604, 0.7775590550643479704 ) ) ;
#44369 = ORIENTED_EDGE ( 'NONE', *, *, #40441, .F. ) ;
#44370 = CARTESIAN_POINT ( 'NONE',  ( -0.7185039370078739607, 1.928577636452523993E-17, 0.8858267715460158565 ) ) ;
#44371 = ORIENTED_EDGE ( 'NONE', *, *, #16889, .T. ) ;
#44372 = CARTESIAN_POINT ( 'NONE',  ( -1.033464566929133799, 0.000000000000000000, 0.2066929133858267931 ) ) ;
#44373 = CARTESIAN_POINT ( 'NONE',  ( 0.6971942568897637749, 2.189545951927499583E-17, 1.070374015694267600 ) ) ;
#44374 = CARTESIAN_POINT ( 'NONE',  ( -0.8019270111902716547, -0.1787899950787401604, 1.938976377898990799 ) ) ;
#44375 = ORIENTED_EDGE ( 'NONE', *, *, #38885, .T. ) ;
#44376 = CARTESIAN_POINT ( 'NONE',  ( 0.6971942568897637749, 2.189545951927499583E-17, 1.931594488135212728 ) ) ;
#44377 = AXIS2_PLACEMENT_3D ( 'NONE', #31857, #46436, #42594 ) ;
#44378 = DIRECTION ( 'NONE',  ( 0.000000000000000000, 0.000000000000000000, -1.000000000000000000 ) ) ;
#44379 = CARTESIAN_POINT ( 'NONE',  ( -0.1787899950787401604, -1.514887747756799019, -0.07405724077823318263 ) ) ;
#44380 = ORIENTED_EDGE ( 'NONE', *, *, #31241, .T. ) ;
#44381 = CARTESIAN_POINT ( 'NONE',  ( 0.07405724077823318263, -0.4999999999462365619, 0.1787899950787401604 ) ) ;
#44382 = CARTESIAN_POINT ( 'NONE',  ( -0.3070839322311865738, -0.04408052624949979070, 0.7141926273478177434 ) ) ;
#44383 = ORIENTED_EDGE ( 'NONE', *, *, #6701, .T. ) ;
#44384 = CARTESIAN_POINT ( 'NONE',  ( 1.054774247047244096, 0.000000000000000000, 1.203248031442299304 ) ) ;
#44385 = DIRECTION ( 'NONE',  ( -1.000000000000000000, 3.469446951953625233E-15, 0.000000000000000000 ) ) ;
#44386 = FACE_OUTER_BOUND ( 'NONE', #30526, .T. ) ;
#44387 = CARTESIAN_POINT ( 'NONE',  ( 1.054774247047244096, 0.000000000000000000, 1.478838582623401399 ) ) ;
#44388 = CARTESIAN_POINT ( 'NONE',  ( 1.054774247047244096, 0.000000000000000000, 0.1402559054580474474 ) ) ;
#44389 = EDGE_CURVE ( 'NONE', #20413, #33274, #2754, .T. ) ;
#44390 = CARTESIAN_POINT ( 'NONE',  ( -0.1787899950787401882, -1.580216535379306952, 0.000000000000000000 ) ) ;
#44391 = CARTESIAN_POINT ( 'NONE',  ( 0.1787899950787401604, -1.671259842465922407, -0.07405724077823318263 ) ) ;
#44392 = DIRECTION ( 'NONE',  ( 3.478357113474434231E-15, 1.000000000000000000, 0.000000000000000000 ) ) ;
#44393 = CARTESIAN_POINT ( 'NONE',  ( -1.002407869896990045, 0.1264236179284866091, 0.5831692912848189803 ) ) ;
#44394 = EDGE_CURVE ( 'NONE', #13286, #41713, #20277, .T. ) ;
#44395 = CARTESIAN_POINT ( 'NONE',  ( -0.06523048226347956391, -0.5713582677165348622, 0.1574803149606297803 ) ) ;
#44396 = CARTESIAN_POINT ( 'NONE',  ( -0.07444174185955065859, -1.386362707220842205, -0.1797182628040039087 ) ) ;
#44397 = CARTESIAN_POINT ( 'NONE',  ( -0.8759842519685039353, 0.1574803149606299191, 1.200787401574803237 ) ) ;
#44398 = CARTESIAN_POINT ( 'NONE',  ( 0.8019270111902717657, 0.1787899950787401604, 1.417322834591906222 ) ) ;
#44399 = CARTESIAN_POINT ( 'NONE',  ( 0.8019270111902716547, -0.1787899950787401604, 1.702755905458047003 ) ) ;
#44400 = CARTESIAN_POINT ( 'NONE',  ( 1.002407869896990045, -0.1264236179284866091, 0.2928149605761578567 ) ) ;
#44401 = CARTESIAN_POINT ( 'NONE',  ( 0.9873396505805591694, 0.1113553986120547346, 0.1328740157480315098 ) ) ;
#44402 = ADVANCED_FACE ( 'NONE', ( #29949 ), #421, .T. ) ;
#44404 = CARTESIAN_POINT ( 'NONE',  ( -0.7692685849603985160, 0.1211171519384340173, 1.980616872294691522 ) ) ;
#44403 = CARTESIAN_POINT ( 'NONE',  ( -0.7185039370078778465, -0.06523048226348396317, 1.439468503829480772 ) ) ;
#44405 = LINE ( 'NONE', #11620, #5226 ) ;
#44406 = CARTESIAN_POINT ( 'NONE',  ( 0.1787899950787401604, 0.1348425197388028463, -0.07405724077823318263 ) ) ;
#44407 = DIRECTION ( 'NONE',  ( 0.000000000000000000, 0.000000000000000000, -1.000000000000000000 ) ) ;
#44408 = CARTESIAN_POINT ( 'NONE',  ( -0.4330708661417343452, 3.105646754637359143E-15, 0.9891732283464568232 ) ) ;
#44409 = DIRECTION ( 'NONE',  ( 0.000000000000000000, -1.000000000000000000, 0.000000000000000000 ) ) ;
#44410 = CARTESIAN_POINT ( 'NONE',  ( -0.8759842519685039353, -0.1787899950787401882, 1.232775590497417362 ) ) ;
#44411 = CARTESIAN_POINT ( 'NONE',  ( 0.7646288533564489232, 0.1113553986120547346, 0.6446850392625511628 ) ) ;
#44412 = ORIENTED_EDGE ( 'NONE', *, *, #2320, .T. ) ;
#44413 = DIRECTION ( 'NONE',  ( 0.000000000000000000, -1.000000000000000000, 0.000000000000000000 ) ) ;
#44414 = CARTESIAN_POINT ( 'NONE',  ( 0.8075642843603819676, 0.1651804176431314886, 0.03937007863263043694 ) ) ;
#44415 = ORIENTED_EDGE ( 'NONE', *, *, #321, .F. ) ;
#44416 = CARTESIAN_POINT ( 'NONE',  ( -0.1270800023317771588, -0.04531940013422661173, -0.1270800023317771588 ) ) ;
#44417 = CARTESIAN_POINT ( 'NONE',  ( -0.7646288533564489232, -0.1113553986120547346, 0.3001968502861740440 ) ) ;
#44418 = CARTESIAN_POINT ( 'NONE',  ( -0.1264236179284866091, -1.230807086560409269, -0.1264236179284866091 ) ) ;
#44419 = ORIENTED_EDGE ( 'NONE', *, *, #10130, .F. ) ;
#44420 = FACE_OUTER_BOUND ( 'NONE', #13825, .T. ) ;
#44421 = CARTESIAN_POINT ( 'NONE',  ( 0.9500414927467378812, 0.1787899950787401604, 1.564960629867495845 ) ) ;
#44422 = DIRECTION ( 'NONE',  ( -0.8191520442889873577, 1.003171929053519323E-16, 0.5735764363510523767 ) ) ;
#44424 = CARTESIAN_POINT ( 'NONE',  ( -0.7646288533564489232, -0.1113553986120547346, 0.1131889763779527630 ) ) ;
#44423 = CARTESIAN_POINT ( 'NONE',  ( 0.1644020957507537628, -0.08115590401245532937, 0.1405661490837558925 ) ) ;
#44425 = CARTESIAN_POINT ( 'NONE',  ( 0.7646288533564489232, 0.1113553986120547346, 0.3690944880814492901 ) ) ;
#44426 = CARTESIAN_POINT ( 'NONE',  ( -0.8759842519685039353, -0.1787899950787401882, 0.05167322829269314910 ) ) ;
#44427 = CARTESIAN_POINT ( 'NONE',  ( 0.07405724077823318263, -0.1850393700249766959, 0.1787899950787401604 ) ) ;
#44428 = ORIENTED_EDGE ( 'NONE', *, *, #22234, .F. ) ;
#44429 = ( BOUNDED_CURVE ( )  B_SPLINE_CURVE ( 2, ( #25880, #36899, #4053, #3591, #32381, #10322, #47447, #43117, #24934 ),
 .UNSPECIFIED., .F., .T. ) 
 B_SPLINE_CURVE_WITH_KNOTS ( ( 3, 2, 2, 2, 3 ),
 ( 0.2899999999999999800, 0.2924999999999999822, 0.2949999999999999845, 0.2974999999999999867, 0.2999999999999999889 ),
 .UNSPECIFIED. ) 
 CURVE ( )  GEOMETRIC_REPRESENTATION_ITEM ( )  RATIONAL_B_SPLINE_CURVE ( ( 1.000000000000000000, 0.9238795325112869605, 1.000000000000000000, 0.9238795325112869605, 1.000000000000000000, 0.9238795325112869605, 1.000000000000000000, 0.9238795325112869605, 1.000000000000000000 ) ) 
 REPRESENTATION_ITEM ( '' )  ) ;
#44430 = CARTESIAN_POINT ( 'NONE',  ( 0.1686160743796767669, -0.08918665060135554101, -0.1880811715460162514 ) ) ;
#44431 = VECTOR ( 'NONE', #32971, 39.37007874015748143 ) ;
#44432 = CARTESIAN_POINT ( 'NONE',  ( 0.6971942568897637749, 2.189545951927499583E-17, 0.8341535432533228045 ) ) ;
#44433 = CARTESIAN_POINT ( 'NONE',  ( -0.7495606340400177148, 0.1264236179284866091, 1.493602362150960650 ) ) ;
#44434 = CARTESIAN_POINT ( 'NONE',  ( -0.1574803149606299191, -0.09645669280585884853, 0.000000000000000000 ) ) ;
#44435 = CARTESIAN_POINT ( 'NONE',  ( -0.7495606340400177148, 0.1264236179284866091, 1.341043307032850462 ) ) ;
#44436 = VERTEX_POINT ( 'NONE', #18638 ) ;
#44437 = CARTESIAN_POINT ( 'NONE',  ( -0.8759842519685039353, 0.1787899950787401882, 0.3124999999462365619 ) ) ;
#44438 = CARTESIAN_POINT ( 'NONE',  ( 0.1574803149606299746, 0.7443365962042343131, -3.964450923140766303 ) ) ;
#44439 = DIRECTION ( 'NONE',  ( -0.000000000000000000, 1.000000000000000000, -3.995705278811693553E-31 ) ) ;
#44440 = CARTESIAN_POINT ( 'NONE',  ( -1.094772975963752103E-17, -0.9710885351583720126, -0.1787899950787401882 ) ) ;
#44441 = ORIENTED_EDGE ( 'NONE', *, *, #37169, .F. ) ;
#44442 = CARTESIAN_POINT ( 'NONE',  ( -1.033464566929133799, 0.000000000000000000, 0.8661417321759370402 ) ) ;
#44443 = ORIENTED_EDGE ( 'NONE', *, *, #10237, .F. ) ;
#44444 = VERTEX_POINT ( 'NONE', #29263 ) ;
#44445 = CARTESIAN_POINT ( 'NONE',  ( 0.7495606340400177148, -0.1264236179284866091, 1.031003936954110189 ) ) ;
#44446 = EDGE_CURVE ( 'NONE', #32777, #9016, #12650, .T. ) ;
#44447 = CARTESIAN_POINT ( 'NONE',  ( -0.1574803149606299191, -0.2714884749021747590, -1.284167712019358198 ) ) ;
#44448 = DIRECTION ( 'NONE',  ( -1.000000000000000000, 0.000000000000000000, 0.000000000000000000 ) ) ;
#44449 = VECTOR ( 'NONE', #5709, 39.37007874015748143 ) ;
#44450 = ADVANCED_FACE ( 'NONE', ( #11465 ), #40659, .F. ) ;
#44451 = CARTESIAN_POINT ( 'NONE',  ( 0.2204724409448818867, 0.000000000000000000, 0.000000000000000000 ) ) ;
#44452 = AXIS2_PLACEMENT_3D ( 'NONE', #3840, #469, #21583 ) ;
#44453 = CARTESIAN_POINT ( 'NONE',  ( -0.1264236179284866091, -0.5123031495525355306, 0.1264236179284866091 ) ) ;
#44454 = CIRCLE ( 'NONE', #20012, 0.7874015748031496509 ) ;
#44455 = CARTESIAN_POINT ( 'NONE',  ( -0.6971942568897626646, -0.07405724077823297447, 0.1673228345919059168 ) ) ;
#44456 = CARTESIAN_POINT ( 'NONE',  ( -0.9873396505805591694, 0.1113553986120547346, 0.8415354330708662012 ) ) ;
#44457 = CARTESIAN_POINT ( 'NONE',  ( -0.4338976377952755703, -0.2460629921259842590, 3.073670608096212368E-17 ) ) ;
#44458 = DIRECTION ( 'NONE',  ( 0.000000000000000000, 0.000000000000000000, 1.000000000000000000 ) ) ;
#44459 = CARTESIAN_POINT ( 'NONE',  ( -0.1797182628040039087, -0.9434493213940695622, 0.07444174185955065859 ) ) ;
#44460 = CARTESIAN_POINT ( 'NONE',  ( 0.8759842519685039353, -0.1787899950787401882, 0.9621062991588346103 ) ) ;
#44461 = CARTESIAN_POINT ( 'NONE',  ( 0.6971942568897648851, -0.07405724077823297447, 1.382874015694267822 ) ) ;
#44462 = CARTESIAN_POINT ( 'NONE',  ( 0.9500414927467377701, 0.1787899950787401604, 0.1082677164816695514 ) ) ;
#44463 = CARTESIAN_POINT ( 'NONE',  ( 0.3161444924769519216, 1.495705267341507883, -0.3569552279982047271 ) ) ;
#44464 = CARTESIAN_POINT ( 'NONE',  ( 1.033464566929134687, 0.06523048226347956391, 1.468996062992126150 ) ) ;
#44466 = DIRECTION ( 'NONE',  ( 3.469446951953614583E-15, 1.000000000000000000, 1.751623080406021339E-46 ) ) ;
#44465 = CARTESIAN_POINT ( 'NONE',  ( 0.7132418682741867855, -0.03858023259734958549, 1.983985632872960592 ) ) ;
#44467 = CARTESIAN_POINT ( 'NONE',  ( 0.4632545931758527691, 0.08090551181102362266, 9.908067607274841931E-18 ) ) ;
#44469 = FACE_OUTER_BOUND ( 'NONE', #19416, .T. ) ;
#44468 = CARTESIAN_POINT ( 'NONE',  ( 0.7495606340400177148, 0.1264236179284866091, 0.8243110235682834519 ) ) ;
#44470 = CARTESIAN_POINT ( 'NONE',  ( 0.1787899950787401604, -0.8444881889226140137, -0.07405724077823318263 ) ) ;
#44471 = EDGE_LOOP ( 'NONE', ( #22177, #16276, #15589, #44716, #37330, #2306, #33832, #7442 ) ) ;
#44472 = CARTESIAN_POINT ( 'NONE',  ( 0.8107537697050254399, -0.1574803149606297803, 0.4207677164279060578 ) ) ;
#44473 = DIRECTION ( 'NONE',  ( 1.000000000000000000, 0.000000000000000000, 0.000000000000000000 ) ) ;
#44474 = CARTESIAN_POINT ( 'NONE',  ( 0.6971942568897648851, -0.07405724077823297447, 1.186023621993481658 ) ) ;
#44475 = CARTESIAN_POINT ( 'NONE',  ( -0.8107537697050254399, 0.1574803149606300301, 1.045767716535432879 ) ) ;
#44476 = CARTESIAN_POINT ( 'NONE',  ( 0.06523048226347956391, -1.693405511811024944, -0.1574803149606300301 ) ) ;
#44477 = CARTESIAN_POINT ( 'NONE',  ( 0.1574803149606300023, -0.2237541348899642346, -1.272196386806234925 ) ) ;
#44478 = VERTEX_POINT ( 'NONE', #644 ) ;
#44479 = DIRECTION ( 'NONE',  ( 1.000000000000000000, 0.000000000000000000, 0.000000000000000000 ) ) ;
#44480 = CARTESIAN_POINT ( 'NONE',  ( -0.7495606340400177148, -0.1264236179284866091, 0.2436023621509610382 ) ) ;
#44481 = CARTESIAN_POINT ( 'NONE',  ( -0.1574803149606300301, -0.2957677164279057802, -0.06523048226347956391 ) ) ;
#44482 = VECTOR ( 'NONE', #36529, 39.37007874015748143 ) ;
#44483 = VECTOR ( 'NONE', #13801, 39.37007874015748143 ) ;
#44484 = CARTESIAN_POINT ( 'NONE',  ( -0.6971942568897637749, 2.189545951927499583E-17, 1.852854330654897685 ) ) ;
#44485 = CARTESIAN_POINT ( 'NONE',  ( -0.8019270111902716547, 0.1787899950787401604, 0.9005905511273391006 ) ) ;
#44486 = VECTOR ( 'NONE', #3282, 39.37007874015748143 ) ;
#44487 = CARTESIAN_POINT ( 'NONE',  ( -1.002407869896990045, -0.1264236179284866091, 0.4945866141194645849 ) ) ;
#44488 = LINE ( 'NONE', #40193, #4566 ) ;
#44489 = CARTESIAN_POINT ( 'NONE',  ( 0.1631243713103937287, 0.07417819129889609286, 0.1405411351623389871 ) ) ;
#44490 = CARTESIAN_POINT ( 'NONE',  ( 0.1006623723854972452, 0.09658349877441904652, -0.2273156230721085636 ) ) ;
#44491 = DIRECTION ( 'NONE',  ( 0.000000000000000000, 1.000000000000000000, 0.000000000000000000 ) ) ;
#44492 = CARTESIAN_POINT ( 'NONE',  ( -0.1264236179284866091, -0.4838838107489236706, 0.1264236179284866091 ) ) ;
#44493 = CARTESIAN_POINT ( 'NONE',  ( 0.09776075193326634605, -0.09842519685039370636, 0.1118142777513527475 ) ) ;
#44494 = DIRECTION ( 'NONE',  ( 0.000000000000000000, -0.000000000000000000, -1.000000000000000000 ) ) ;
#44495 = EDGE_CURVE ( 'NONE', #42566, #18058, #17242, .T. ) ;
#44496 = DIRECTION ( 'NONE',  ( -1.000000000000000000, 3.469446951953613794E-15, 0.000000000000000000 ) ) ;
#44497 = CARTESIAN_POINT ( 'NONE',  ( -0.7495606340400177148, -0.1264236179284866091, 0.2436023621509610382 ) ) ;
#44498 = CARTESIAN_POINT ( 'NONE',  ( -0.1264236179284866091, -1.704356251693805335, 0.1264236179284866091 ) ) ;
#44499 = EDGE_CURVE ( 'NONE', #7899, #398, #9038, .T. ) ;
#44500 = VERTEX_POINT ( 'NONE', #15790 ) ;
#44501 = DIRECTION ( 'NONE',  ( 0.000000000000000000, -1.020425574104001164E-16, 1.000000000000000000 ) ) ;
#44502 = ORIENTED_EDGE ( 'NONE', *, *, #37835, .F. ) ;
#44503 = ADVANCED_FACE ( 'NONE', ( #16484 ), #886, .T. ) ;
#44504 = ORIENTED_EDGE ( 'NONE', *, *, #23109, .T. ) ;
#44505 = EDGE_CURVE ( 'NONE', #39972, #23980, #8563, .T. ) ;
#44506 = AXIS2_PLACEMENT_3D ( 'NONE', #46009, #1928, #12511 ) ;
#44507 = CARTESIAN_POINT ( 'NONE',  ( 0.1787899950787401604, -1.321850393647023392, -0.07405724077823318263 ) ) ;
#44508 = CARTESIAN_POINT ( 'NONE',  ( 0.1787899950787401882, -1.594980314906866203, -2.189545951927503898E-17 ) ) ;
#44509 = CIRCLE ( 'NONE', #7009, 0.07874015748031489015 ) ;
#44510 = ( NAMED_UNIT ( * ) SI_UNIT ( $, .STERADIAN. ) SOLID_ANGLE_UNIT ( ) ) ;
#44511 = CARTESIAN_POINT ( 'NONE',  ( 0.8070866141732283561, 0.3779527559055118058, -0.7574803149606299524 ) ) ;
#44512 = CARTESIAN_POINT ( 'NONE',  ( 0.9873396505805591694, -0.1113553986120547346, 0.4773622047244094890 ) ) ;
#44513 = LINE ( 'NONE', #43819, #36292 ) ;
#44514 = CARTESIAN_POINT ( 'NONE',  ( -0.7646288533564489232, -0.1113553986120547346, 1.087598425089322918 ) ) ;
#44515 = CARTESIAN_POINT ( 'NONE',  ( 1.002407869896990045, 0.1264236179284866091, 0.6225393700249762796 ) ) ;
#44516 = CYLINDRICAL_SURFACE ( 'NONE', #22995, 0.1624015748031501782 ) ;
#44517 = CARTESIAN_POINT ( 'NONE',  ( 0.1574803149606299191, -0.2834645669291338543, -1.928577636452523993E-17 ) ) ;
#44518 = VECTOR ( 'NONE', #38055, 39.37007874015748854 ) ;
#44519 = VECTOR ( 'NONE', #43955, 39.37007874015748143 ) ;
#44520 = FACE_OUTER_BOUND ( 'NONE', #43770, .T. ) ;
#44521 = ORIENTED_EDGE ( 'NONE', *, *, #11592, .F. ) ;
#44522 = CARTESIAN_POINT ( 'NONE',  ( -0.1363753864968494101, -0.09373322739561565364, -0.1156200648374353240 ) ) ;
#44523 = CARTESIAN_POINT ( 'NONE',  ( -1.054774247047244540, 0.07405724077823318263, 0.9350393700249758355 ) ) ;
#44524 = CARTESIAN_POINT ( 'NONE',  ( 0.9873396505805591694, -0.1113553986120547346, 0.9104330708661417804 ) ) ;
#44525 = CARTESIAN_POINT ( 'NONE',  ( -0.5555748031496045014, 0.6449983665207589256, -0.06082000038405668829 ) ) ;
#44526 = CARTESIAN_POINT ( 'NONE',  ( -0.1064406243220434034, -0.08956136075716661371, 0.1198387747093381250 ) ) ;
#44527 = ORIENTED_EDGE ( 'NONE', *, *, #38095, .F. ) ;
#44528 = FACE_BOUND ( 'NONE', #12463, .T. ) ;
#44529 = CARTESIAN_POINT ( 'NONE',  ( 1.033464566929133799, 0.000000000000000000, 1.466535433070866201 ) ) ;
#44530 = VERTEX_POINT ( 'NONE', #37565 ) ;
#44531 = CARTESIAN_POINT ( 'NONE',  ( 0.8107537697050254399, 0.1574803149606300301, 1.281988188976378895 ) ) ;
#44532 = DIRECTION ( 'NONE',  ( -1.000000000000000000, 0.000000000000000000, 0.000000000000000000 ) ) ;
#44533 = CARTESIAN_POINT ( 'NONE',  ( -0.1787899950787401882, -1.535925196796629866, 0.000000000000000000 ) ) ;
#44534 = CARTESIAN_POINT ( 'NONE',  ( 0.07405724077823318263, -0.7411417322297018107, 0.1787899950787401604 ) ) ;
#44535 = CARTESIAN_POINT ( 'NONE',  ( 2.892866454678787531E-17, -1.159448818897637956, 0.1574803149606299191 ) ) ;
#44536 = CARTESIAN_POINT ( 'NONE',  ( 0.8107537697050253289, 0.1574803149606300301, 1.154035432963338659 ) ) ;
#44537 = CARTESIAN_POINT ( 'NONE',  ( -0.9412147342319837628, -0.1574803149606297803, 1.656003937007873628 ) ) ;
#44538 = ORIENTED_EDGE ( 'NONE', *, *, #17593, .F. ) ;
#44539 = EDGE_LOOP ( 'NONE', ( #35470, #36152, #1248, #41185 ) ) ;
#44540 = CARTESIAN_POINT ( 'NONE',  ( -0.8019270111902717657, -0.1787899950787401604, 1.707677165300566235 ) ) ;
#44541 = CARTESIAN_POINT ( 'NONE',  ( 0.9500414927467378812, 0.1787899950787401604, 1.766732283410803461 ) ) ;
#44542 = ORIENTED_EDGE ( 'NONE', *, *, #15497, .T. ) ;
#44543 = CARTESIAN_POINT ( 'NONE',  ( -0.7495606340400177148, 0.1264236179284866091, 0.9079724408911180600 ) ) ;
#44544 = CARTESIAN_POINT ( 'NONE',  ( -0.08209939101897356650, -0.2480946695746812369, -0.3118411609178720068 ) ) ;
#44545 = FACE_OUTER_BOUND ( 'NONE', #41243, .T. ) ;
#44546 = CARTESIAN_POINT ( 'NONE',  ( -0.9500414927467377701, 0.1787899950787401604, 1.210629921206079818 ) ) ;
#44547 = CARTESIAN_POINT ( 'NONE',  ( -0.7495606340400177148, -0.1264236179284866091, 0.8735236219934803259 ) ) ;
#44548 = CARTESIAN_POINT ( 'NONE',  ( -0.7495606340400177148, 0.1264236179284866091, 0.1599409448281264023 ) ) ;
#44549 = VECTOR ( 'NONE', #33085, 39.37007874015748143 ) ;
#44550 = CARTESIAN_POINT ( 'NONE',  ( 0.2944196465027555387, 4.766607801171850497E-17, 0.000000000000000000 ) ) ;
#44551 = CARTESIAN_POINT ( 'NONE',  ( -0.7495606340400177148, 0.1264236179284866091, 1.616633858213952779 ) ) ;
#44552 = CARTESIAN_POINT ( 'NONE',  ( -0.9412147342319837628, 0.1574803149606300301, 1.857775590443653257 ) ) ;
#44553 = ORIENTED_EDGE ( 'NONE', *, *, #11792, .F. ) ;
#44554 = DIRECTION ( 'NONE',  ( 0.000000000000000000, 1.000000000000000000, 0.000000000000000000 ) ) ;
#44555 = CARTESIAN_POINT ( 'NONE',  ( -0.9873396505805591694, -0.1113553986120547346, 1.579724409448818978 ) ) ;
#44556 = CARTESIAN_POINT ( 'NONE',  ( 0.9873396505805591694, 0.1113553986120547346, 1.628937007874015963 ) ) ;
#44557 = CARTESIAN_POINT ( 'NONE',  ( 0.7495606340400177148, -0.1264236179284866091, 1.626476377898992132 ) ) ;
#44558 = CARTESIAN_POINT ( 'NONE',  ( -0.06612450700486259547, -0.09851382860064350488, 0.1467596715283011888 ) ) ;
#44559 = CARTESIAN_POINT ( 'NONE',  ( -1.033464566929133799, 0.000000000000000000, 0.7972440944881890035 ) ) ;
#44560 = CARTESIAN_POINT ( 'NONE',  ( -0.2559058759996818422, 0.01250272378134492310, -0.3148280614481966388 ) ) ;
#44561 = VERTEX_POINT ( 'NONE', #12179 ) ;
#44562 = CONICAL_SURFACE ( 'NONE', #36140, 0.1003937007874010356, 0.7853981633978559529 ) ;
#44563 = ADVANCED_FACE ( 'NONE', ( #9046 ), #31114, .T. ) ;
#44564 = ORIENTED_EDGE ( 'NONE', *, *, #3692, .T. ) ;
#44565 = ORIENTED_EDGE ( 'NONE', *, *, #15725, .T. ) ;
#44566 = VERTEX_POINT ( 'NONE', #4725 ) ;
#44567 = EDGE_CURVE ( 'NONE', #9478, #29301, #25680, .T. ) ;
#44568 = CARTESIAN_POINT ( 'NONE',  ( -0.07405724077823318263, -0.9183070865604088251, -0.1787899950787401604 ) ) ;
#44569 = CARTESIAN_POINT ( 'NONE',  ( 0.07405724077823318263, -1.051181102308440529, 0.1787899950787401604 ) ) ;
#44570 = CARTESIAN_POINT ( 'NONE',  ( -0.1270800023317771588, -0.3209099513153291783, -0.1270800023317771588 ) ) ;
#44571 = CARTESIAN_POINT ( 'NONE',  ( -0.06523048226347956391, 0.1619094488188975167, -0.1574803149606300301 ) ) ;
#44572 = CARTESIAN_POINT ( 'NONE',  ( 0.07405724077823318263, -0.05708661411946481384, -0.1787899950787401604 ) ) ;
#44573 = CARTESIAN_POINT ( 'NONE',  ( 0.9500414927467378812, -0.1787899950787401604, 0.7234251967966300878 ) ) ;
#44574 = AXIS2_PLACEMENT_3D ( 'NONE', #19215, #19686, #41708 ) ;
#44575 = ( CONVERSION_BASED_UNIT ( 'INCH', #33142 ) LENGTH_UNIT ( ) NAMED_UNIT ( #28348 ) ) ;
#44576 = LINE ( 'NONE', #15628, #30552 ) ;
#44577 = LINE ( 'NONE', #726, #16970 ) ;
#44578 = CARTESIAN_POINT ( 'NONE',  ( 0.8759842519685039353, 0.1787899950787401882, 1.847933070812378009 ) ) ;
#44579 = AXIS2_PLACEMENT_3D ( 'NONE', #40340, #32966, #40806 ) ;
#44580 = CARTESIAN_POINT ( 'NONE',  ( 0.7646288533564489232, 0.1113553986120547346, 0.06397637795275590289 ) ) ;
#44581 = DIRECTION ( 'NONE',  ( 1.000000000000000000, 0.000000000000000000, 0.000000000000000000 ) ) ;
#44582 = CARTESIAN_POINT ( 'NONE',  ( 3.284318927891251994E-17, -0.2711614172690712810, 0.1787899950787401882 ) ) ;
#44583 = DIRECTION ( 'NONE',  ( -0.000000000000000000, -0.000000000000000000, -1.000000000000000000 ) ) ;
#44584 = ADVANCED_FACE ( 'NONE', ( #30418 ), #20059, .T. ) ;
#44585 = CARTESIAN_POINT ( 'NONE',  ( 0.07405724077823318263, -1.193897637741512696, -0.1787899950787401604 ) ) ;
#44586 = ( BOUNDED_CURVE ( )  B_SPLINE_CURVE ( 2, ( #13162, #17203, #45950, #35664, #46422, #31838, #38997, #42800, #46655 ),
 .UNSPECIFIED., .F., .F. ) 
 B_SPLINE_CURVE_WITH_KNOTS ( ( 3, 2, 2, 2, 3 ),
 ( 0.6700000000000000400, 0.6724999999999999867, 0.6750000000000000444, 0.6774999999999999911, 0.6800000000000000488 ),
 .UNSPECIFIED. ) 
 CURVE ( )  GEOMETRIC_REPRESENTATION_ITEM ( )  RATIONAL_B_SPLINE_CURVE ( ( 1.000000000000000000, 0.9238795325112869605, 1.000000000000000000, 0.9238795325112869605, 1.000000000000000000, 0.9238795325112869605, 1.000000000000000000, 0.9238795325112869605, 1.000000000000000000 ) ) 
 REPRESENTATION_ITEM ( '' )  ) ;
#44587 = CARTESIAN_POINT ( 'NONE',  ( 0.6971942568897626646, 0.07405724077823318263, 0.2411417322297011168 ) ) ;
#44588 = CARTESIAN_POINT ( 'NONE',  ( 1.033464566929133799, 0.000000000000000000, 1.742125984251968518 ) ) ;
#44589 = CARTESIAN_POINT ( 'NONE',  ( -1.054774247047244096, 0.000000000000000000, 1.793799212544661348 ) ) ;
#44590 = ORIENTED_EDGE ( 'NONE', *, *, #16350, .F. ) ;
#44591 = CIRCLE ( 'NONE', #39981, 0.09842519685039370636 ) ;
#44592 = CARTESIAN_POINT ( 'NONE',  ( -0.7495606340400177148, 0.1264236179284866091, 1.301673228292692830 ) ) ;
#44593 = CARTESIAN_POINT ( 'NONE',  ( 0.3849708276051176936, 4.766607801171850497E-17, 0.000000000000000000 ) ) ;
#44594 = CARTESIAN_POINT ( 'NONE',  ( 0.8759842519685039353, 0.1787899950787401882, 1.961122047190330786 ) ) ;
#44595 = CARTESIAN_POINT ( 'NONE',  ( -0.9500414927467378812, 0.1787899950787401604, 1.013779527505291878 ) ) ;
#44596 = CARTESIAN_POINT ( 'NONE',  ( -0.1187775451116823144, -0.09842519684033429472, -0.1336329292046753159 ) ) ;
#44597 = DIRECTION ( 'NONE',  ( 0.000000000000000000, 1.000000000000000000, 0.000000000000000000 ) ) ;
#44598 = CARTESIAN_POINT ( 'NONE',  ( 0.6971942568897648851, 0.07405724077823318263, 0.5167322834108035723 ) ) ;
#44599 = CARTESIAN_POINT ( 'NONE',  ( -1.002407869896990045, -0.1264236179284866091, 0.4109251967966299213 ) ) ;
#44600 = CARTESIAN_POINT ( 'NONE',  ( 0.7646288533564489232, 0.1113553986120547346, 1.668307086506645609 ) ) ;
#44601 = CARTESIAN_POINT ( 'NONE',  ( -1.033464566929133799, 0.000000000000000000, 1.348425196850393748 ) ) ;
#44602 = CARTESIAN_POINT ( 'NONE',  ( 0.6971942568897626646, -0.07405724077823297447, 0.8759842519147408302 ) ) ;
#44603 = CARTESIAN_POINT ( 'NONE',  ( -0.9412147342319837628, -0.1574803149606297803, 0.08120078740157485320 ) ) ;
#44604 = CARTESIAN_POINT ( 'NONE',  ( -0.2112885751001251922, -0.09851385201003405589, -0.1284757149005590626 ) ) ;
#44605 = ORIENTED_EDGE ( 'NONE', *, *, #264, .T. ) ;
#44606 = VECTOR ( 'NONE', #26941, 39.37007874015748143 ) ;
#44607 = ADVANCED_FACE ( 'NONE', ( #34702 ), #8817, .T. ) ;
#44608 = CARTESIAN_POINT ( 'NONE',  ( 0.1527640389977631963, -0.1049476924225413443, -0.09381581576814961021 ) ) ;
#44609 = CARTESIAN_POINT ( 'NONE',  ( -0.8759842519685039353, 0.1787899950787401882, 0.03198818892261445085 ) ) ;
#44610 = CARTESIAN_POINT ( 'NONE',  ( -0.1264236179284866091, -1.438608220197742149, -0.1264236179284866091 ) ) ;
#44611 = VERTEX_POINT ( 'NONE', #16253 ) ;
#44612 = CARTESIAN_POINT ( 'NONE',  ( 0.1787899950787401604, -0.3769685038832444324, 0.07405724077823318263 ) ) ;
#44613 = CARTESIAN_POINT ( 'NONE',  ( -0.06523048226347956391, 0.01427165365083412490, -0.1574803149606300301 ) ) ;
#44614 = ORIENTED_EDGE ( 'NONE', *, *, #41575, .T. ) ;
#44615 = CARTESIAN_POINT ( 'NONE',  ( 0.8759842519685039353, -0.1787899950787401882, 1.154035433017102319 ) ) ;
#44616 = EDGE_CURVE ( 'NONE', #1642, #12322, #35292, .T. ) ;
#44617 = CIRCLE ( 'NONE', #32423, 0.7874015748031497619 ) ;
#44618 = EDGE_CURVE ( 'NONE', #23610, #12346, #22955, .T. ) ;
#44619 = LINE ( 'NONE', #37215, #29476 ) ;
#44620 = DIRECTION ( 'NONE',  ( 1.822029033848725028E-16, 0.000000000000000000, 1.000000000000000000 ) ) ;
#44621 = CARTESIAN_POINT ( 'NONE',  ( 0.8759842519685039353, 0.1787899950787401882, 1.528051181048598384 ) ) ;
#44622 = CARTESIAN_POINT ( 'NONE',  ( 0.8019270111902717657, -0.1787899950787401604, 0.2066929133320631329 ) ) ;
#44623 = CARTESIAN_POINT ( 'NONE',  ( -0.1787899950787401604, -1.779527559001355952, -0.07405724077823318263 ) ) ;
#44624 = APPLICATION_PROTOCOL_DEFINITION ( 'draft international standard', 'automotive_design', 1998, #30329 ) ;
#44625 = LINE ( 'NONE', #30318, #31092 ) ;
#44626 = CARTESIAN_POINT ( 'NONE',  ( -0.8759842519685039353, -0.1787899950787401882, 0.7258858267178898149 ) ) ;
#44628 = CARTESIAN_POINT ( 'NONE',  ( 0.7646288533564489232, -0.1113553986120547346, 0.3001968502861740440 ) ) ;
#44627 = CARTESIAN_POINT ( 'NONE',  ( -0.06523048226347956391, -0.7682086614173235795, 0.1574803149606297803 ) ) ;
#44629 = CARTESIAN_POINT ( 'NONE',  ( -0.1797182628040039087, -1.460181604858636906, -0.07444174185955065859 ) ) ;
#44630 = CARTESIAN_POINT ( 'NONE',  ( 0.2395294000716133853, 3.218313930830148909E-16, -0.8759842519685039353 ) ) ;
#44631 = CARTESIAN_POINT ( 'NONE',  ( 0.2471922904502825424, 0.07319706521782758102, -0.08615678709746438235 ) ) ;
#44632 = CARTESIAN_POINT ( 'NONE',  ( 0.8019270111902717657, 0.1787899950787401604, 1.299212598371432215 ) ) ;
#44633 = CARTESIAN_POINT ( 'NONE',  ( 0.8759842519685039353, 0.1787899950787401882, 1.764271653489543290 ) ) ;
#44634 = CARTESIAN_POINT ( 'NONE',  ( 1.002407869896990045, -0.1264236179284866091, 0.2534448818360003908 ) ) ;
#44635 = CARTESIAN_POINT ( 'NONE',  ( -0.5555748031496040573, 0.7681739484881661140, -0.04983111751016786051 ) ) ;
#44636 = CARTESIAN_POINT ( 'NONE',  ( 0.7185039370078739607, 1.928577636452523993E-17, 1.161417322727118284 ) ) ;
#44637 = CARTESIAN_POINT ( 'NONE',  ( 1.033464566929133799, 0.000000000000000000, 1.899606299212598604 ) ) ;
#44639 = CARTESIAN_POINT ( 'NONE',  ( -0.1574803149606299191, -0.4008464425712929824, -0.9238935802775073425 ) ) ;
#44638 = CARTESIAN_POINT ( 'NONE',  ( 2.892866454678787531E-17, -0.8346456691838110009, 0.1574803149606299191 ) ) ;
#44640 = CARTESIAN_POINT ( 'NONE',  ( 0.8107537697050254399, -0.1574803149606297803, 0.5388779526483779003 ) ) ;
#44642 = DIRECTION ( 'NONE',  ( -1.000000000000000000, 0.000000000000000000, 7.049916206369740876E-15 ) ) ;
#44641 = CARTESIAN_POINT ( 'NONE',  ( 1.054774247047244096, 0.000000000000000000, 1.242618110182456714 ) ) ;
#44643 = CARTESIAN_POINT ( 'NONE',  ( 0.2066929133858268486, 0.3648440108500937140, -3.619166627704267114 ) ) ;
#44644 = CARTESIAN_POINT ( 'NONE',  ( 0.9873396505805591694, -0.1113553986120547346, 0.6249999998924724576 ) ) ;
#44645 = ORIENTED_EDGE ( 'NONE', *, *, #220, .T. ) ;
#44646 = CARTESIAN_POINT ( 'NONE',  ( -1.033464566929134687, 0.06523048226347956391, 1.744586614173228245 ) ) ;
#44647 = ORIENTED_EDGE ( 'NONE', *, *, #39860, .T. ) ;
#44648 = CARTESIAN_POINT ( 'NONE',  ( -0.1797182628040039087, -0.04285877021296678052, -0.07444174185955065859 ) ) ;
#44649 = VECTOR ( 'NONE', #14843, 39.37007874015748143 ) ;
#44650 = CARTESIAN_POINT ( 'NONE',  ( -0.1787899950787401882, -1.147145669237574772, 0.000000000000000000 ) ) ;
#44651 = CARTESIAN_POINT ( 'NONE',  ( 0.002815489457238504883, 0.03701807430643332120, 0.1377953632175518695 ) ) ;
#44652 = CARTESIAN_POINT ( 'NONE',  ( 1.054774247047244540, 0.07405724077823318263, 1.560039370024977057 ) ) ;
#44653 = CARTESIAN_POINT ( 'NONE',  ( -0.7185039370078746268, 0.06523048226347956391, 1.286909448818898127 ) ) ;
#44654 = CARTESIAN_POINT ( 'NONE',  ( 1.033464566929133799, 0.000000000000000000, 0.5610236220472440971 ) ) ;
#44656 = DIRECTION ( 'NONE',  ( 0.8191520442890001252, 1.003171929053535101E-16, -0.5735764363510340580 ) ) ;
#44655 = CARTESIAN_POINT ( 'NONE',  ( -0.1574803149606297803, 0.05364173228346463818, 0.06523048226347956391 ) ) ;
#44657 = CARTESIAN_POINT ( 'NONE',  ( -0.1184675242425147906, -0.09842519685039370636, 1.713085361781125471 ) ) ;
#44658 = UNCERTAINTY_MEASURE_WITH_UNIT (LENGTH_MEASURE( 1.000000000000000082E-05 ), #39792, 'distance_accuracy_value', 'NONE') ;
#44659 = CARTESIAN_POINT ( 'NONE',  ( 0.07405724077823318263, -0.1702755904974175283, -0.1787899950787401604 ) ) ;
#44660 = EDGE_LOOP ( 'NONE', ( #2353, #26004, #15939, #1286 ) ) ;
#44661 = CARTESIAN_POINT ( 'NONE',  ( -0.06523048226347956391, 0.08316929133858273759, -0.1574803149606300301 ) ) ;
#44662 = ORIENTED_EDGE ( 'NONE', *, *, #911, .F. ) ;
#44663 = CARTESIAN_POINT ( 'NONE',  ( 0.7495606340400177148, 0.1264236179284866091, 0.6717519684501732646 ) ) ;
#44664 = EDGE_CURVE ( 'NONE', #27388, #2356, #17577, .T. ) ;
#44665 = CARTESIAN_POINT ( 'NONE',  ( -1.002407869896990045, -0.1264236179284866091, 1.552657480261196765 ) ) ;
#44666 = CARTESIAN_POINT ( 'NONE',  ( 0.1574803149606299191, -0.1161417321759375954, -1.928577636452523993E-17 ) ) ;
#44667 = CARTESIAN_POINT ( 'NONE',  ( -0.9500414927467378812, -0.1787899950787401604, 1.240157480261197431 ) ) ;
#44668 = EDGE_CURVE ( 'NONE', #46488, #8568, #22464, .T. ) ;
#44669 = ORIENTED_EDGE ( 'NONE', *, *, #152, .T. ) ;
#44670 = EDGE_CURVE ( 'NONE', #32806, #36286, #35862, .T. ) ;
#44671 = CARTESIAN_POINT ( 'NONE',  ( -1.002407869896990045, -0.1264236179284866091, 0.3371062991588349989 ) ) ;
#44672 = CARTESIAN_POINT ( 'NONE',  ( 0.9873396505805591694, -0.1113553986120547346, 0.6742125984251968740 ) ) ;
#44673 = CARTESIAN_POINT ( 'NONE',  ( -0.8759842519685039353, -0.1574803149606299191, 1.879921259734992134 ) ) ;
#44674 = CARTESIAN_POINT ( 'NONE',  ( 0.1787899950787401604, -1.057210582402466903, -0.07405724077823318263 ) ) ;
#44675 = ORIENTED_EDGE ( 'NONE', *, *, #26090, .F. ) ;
#44676 = CARTESIAN_POINT ( 'NONE',  ( 0.1787899950787401604, 0.02165354336085011100, -0.07405724077823318263 ) ) ;
#44677 = ORIENTED_EDGE ( 'NONE', *, *, #29963, .F. ) ;
#44678 = CARTESIAN_POINT ( 'NONE',  ( 0.8759842519685039353, -0.1787899950787401882, 1.035925196796629866 ) ) ;
#44679 = DIRECTION ( 'NONE',  ( 1.000000000000000000, 0.000000000000000000, 0.000000000000000000 ) ) ;
#44680 = CYLINDRICAL_SURFACE ( 'NONE', #28462, 0.09842519685039370636 ) ;
#44681 = EDGE_CURVE ( 'NONE', #45189, #40667, #20761, .T. ) ;
#44682 = CARTESIAN_POINT ( 'NONE',  ( 0.8759842519685039353, 0.1574803149606299191, 1.427165354223181248 ) ) ;
#44683 = CARTESIAN_POINT ( 'NONE',  ( -0.8019270111902716547, 0.1787899950787401604, 0.1574803149068664809 ) ) ;
#44684 = CARTESIAN_POINT ( 'NONE',  ( -0.7185039370078746268, -0.06523048226347956391, 0.8981299212598431447 ) ) ;
#44685 = DIRECTION ( 'NONE',  ( 7.065124121545350864E-15, -0.7880107536067211260, 0.6156614753256594019 ) ) ;
#44686 = CARTESIAN_POINT ( 'NONE',  ( 0.5555748031496091643, 0.4370297686271511495, 0.6367018223237037589 ) ) ;
#44687 = CARTESIAN_POINT ( 'NONE',  ( -0.1797182628040039087, -1.066480817457060581, -0.07444174185955065859 ) ) ;
#44688 = CARTESIAN_POINT ( 'NONE',  ( 0.8759842519685039353, 0.000000000000000000, 4.498031496062992574 ) ) ;
#44689 = CARTESIAN_POINT ( 'NONE',  ( -1.033464566929134687, 0.06523048226347956391, 1.498523621939716444 ) ) ;
#44690 = COLOUR_RGB ( '', 0.31764706, 0.68627451, 0.89019608) ;
#44691 = CARTESIAN_POINT ( 'NONE',  ( 1.002407869896990045, -0.1264236179284866091, 0.8882874015210394658 ) ) ;
#44692 = CARTESIAN_POINT ( 'NONE',  ( 1.033464566929134687, 0.06523048226347956391, 0.5142716534357801850 ) ) ;
#44693 = CARTESIAN_POINT ( 'NONE',  ( 0.8107537697050253289, -0.1574803149606297803, 1.414862204724410377 ) ) ;
#44695 = CARTESIAN_POINT ( 'NONE',  ( -0.1792139591741687965, -0.1920237930723998898, -0.3110703821948138659 ) ) ;
#44694 = CARTESIAN_POINT ( 'NONE',  ( 0.7114281668690185523, 0.01826851868682138544, 1.982933749348845032 ) ) ;
#44696 = CARTESIAN_POINT ( 'NONE',  ( 0.9412147342319837628, -0.1574803149606297803, 1.724901574695621775 ) ) ;
#44697 = ( BOUNDED_CURVE ( )  B_SPLINE_CURVE ( 2, ( #41103, #208, #37346, #4047, #11494, #29745, #11741, #3588, #40223 ),
 .UNSPECIFIED., .F., .T. ) 
 B_SPLINE_CURVE_WITH_KNOTS ( ( 3, 2, 2, 2, 3 ),
 ( 0.3699999999999999956, 0.3724999999999999978, 0.3750000000000000000, 0.3775000000000000022, 0.3800000000000000044 ),
 .UNSPECIFIED. ) 
 CURVE ( )  GEOMETRIC_REPRESENTATION_ITEM ( )  RATIONAL_B_SPLINE_CURVE ( ( 1.000000000000000000, 0.9238795325112869605, 1.000000000000000000, 0.9238795325112869605, 1.000000000000000000, 0.9238795325112869605, 1.000000000000000000, 0.9238795325112869605, 1.000000000000000000 ) ) 
 REPRESENTATION_ITEM ( '' )  ) ;
#44698 = CARTESIAN_POINT ( 'NONE',  ( 0.1574803149606300023, -0.2274162997038010614, -0.9219983537151217323 ) ) ;
#44699 = CARTESIAN_POINT ( 'NONE',  ( 0.8019270111902716547, -0.1787899950787401604, 0.7972440944344248992 ) ) ;
#44700 = CARTESIAN_POINT ( 'NONE',  ( 0.8759842519685039353, 0.1787899950787401882, 1.808562992072220377 ) ) ;
#44701 = CARTESIAN_POINT ( 'NONE',  ( 0.07405724077823318263, -0.7608267715997808489, -0.1787899950787401604 ) ) ;
#44702 = ORIENTED_EDGE ( 'NONE', *, *, #37998, .F. ) ;
#44703 = CARTESIAN_POINT ( 'NONE',  ( -0.7646288533564489232, 0.1113553986120547346, 0.8513779527559054427 ) ) ;
#44704 = CARTESIAN_POINT ( 'NONE',  ( 0.2066929133858268486, 0.2573565155132531701, -0.3015174453633727714 ) ) ;
#44705 = FACE_OUTER_BOUND ( 'NONE', #8605, .T. ) ;
#44706 = CARTESIAN_POINT ( 'NONE',  ( 0.9500414927467378812, -0.1787899950787401604, 1.117125984198206412 ) ) ;
#44707 = ADVANCED_FACE ( 'NONE', ( #34938 ), #46166, .T. ) ;
#44708 = CARTESIAN_POINT ( 'NONE',  ( -1.033464566929133799, 0.000000000000000000, 1.033464566929133799 ) ) ;
#44709 = CARTESIAN_POINT ( 'NONE',  ( 0.1574803149606300301, -1.737696850393700032, -0.06523048226347956391 ) ) ;
#44710 = CARTESIAN_POINT ( 'NONE',  ( 0.4736248074375866701, -0.09842519685039370636, 1.713085361781129690 ) ) ;
#44711 = CARTESIAN_POINT ( 'NONE',  ( -0.6971942568897626646, 0.07405724077823318263, 0.5118110235682844511 ) ) ;
#44712 = ORIENTED_EDGE ( 'NONE', *, *, #15948, .T. ) ;
#44714 = CYLINDRICAL_SURFACE ( 'NONE', #34410, 0.7874015748031497619 ) ;
#44713 = CIRCLE ( 'NONE', #37103, 0.04921259842519686012 ) ;
#44715 = CARTESIAN_POINT ( 'NONE',  ( -1.054774247047244540, 0.07405724077823318263, 0.2214566928596220785 ) ) ;
#44716 = ORIENTED_EDGE ( 'NONE', *, *, #2315, .T. ) ;
#44717 = EDGE_CURVE ( 'NONE', #29582, #20867, #24152, .T. ) ;
#44718 = FACE_OUTER_BOUND ( 'NONE', #6115, .T. ) ;
#44720 = CARTESIAN_POINT ( 'NONE',  ( 0.1787899950787401604, -1.602362204670647161, 0.07405724077823318263 ) ) ;
#44719 = CARTESIAN_POINT ( 'NONE',  ( -0.1574803149606297803, -0.2908464565853862149, 0.06523048226347956391 ) ) ;
#44721 = AXIS2_PLACEMENT_3D ( 'NONE', #12386, #30147, #4431 ) ;
#44723 = CARTESIAN_POINT ( 'NONE',  ( 0.7646288533564489232, -0.1113553986120547346, 0.3395669290263311213 ) ) ;
#44722 = CIRCLE ( 'NONE', #15692, 0.2007874015748031815 ) ;
#44724 = CARTESIAN_POINT ( 'NONE',  ( -0.8019270111902716547, -0.1787899950787401604, 0.9153543306548987957 ) ) ;
#44725 = CARTESIAN_POINT ( 'NONE',  ( -1.054774247047244540, -0.07405724077823318263, 1.122047244040725644 ) ) ;
#44726 = CARTESIAN_POINT ( 'NONE',  ( -0.8019270111902717657, 0.1787899950787401604, 0.4724409448281262636 ) ) ;
#44727 = ( BOUNDED_SURFACE ( )  B_SPLINE_SURFACE ( 3, 2, ( 
 ( #19861, #22504, #447 ),
 ( #30444, #29747, #11744 ),
 ( #34034, #7883, #37120 ),
 ( #15816, #33556, #26364 ),
 ( #40925, #8119, #37349 ),
 ( #15581, #4502, #922 ) ),
 .UNSPECIFIED., .F., .F., .F. ) 
 B_SPLINE_SURFACE_WITH_KNOTS ( ( 4, 2, 4 ),
 ( 3, 3 ),
 ( 0.01652267773200355103, 0.01858309280828994783, 0.02064350788457639668 ),
 ( 0.000000000000000000, 1.000000000000000000 ),
 .UNSPECIFIED. ) 
 GEOMETRIC_REPRESENTATION_ITEM ( )  RATIONAL_B_SPLINE_SURFACE ( (
 ( 1.000000000000000000, 0.8047780975688290095, 1.000000000000000000),
 ( 1.000000000000000000, 0.8123789546321300570, 1.000000000000000000),
 ( 1.000000000000000000, 0.8190677982993119777, 1.000000000000000000),
 ( 1.000000000000000000, 0.8192346069547790099, 1.000000000000000000),
 ( 1.000000000000000000, 0.8126126759772189789, 1.000000000000000000),
 ( 1.000000000000000000, 0.8047712639312000205, 1.000000000000000000) ) ) 
 REPRESENTATION_ITEM ( '' )  SURFACE ( )  ) ;
#44728 = CARTESIAN_POINT ( 'NONE',  ( -0.9412147342319837628, -0.1574803149606297803, 0.1599409448818898405 ) ) ;
#44729 = CARTESIAN_POINT ( 'NONE',  ( -0.1574803149606299191, 1.928577636452524610E-17, 2.731847993664263218E-16 ) ) ;
#44730 = CARTESIAN_POINT ( 'NONE',  ( 0.5236220472440944462, 0.08090551181102362266, 0.000000000000000000 ) ) ;
#44731 = CARTESIAN_POINT ( 'NONE',  ( 0.3604359965418638123, -0.09842519685039370636, 0.000000000000000000 ) ) ;
#44732 = CARTESIAN_POINT ( 'NONE',  ( -0.1787899950787401604, -0.5257145194103405306, 0.07405724077823318263 ) ) ;
#44733 = CARTESIAN_POINT ( 'NONE',  ( -0.2055635559985952709, -0.08955966668076850712, -0.1312247587652915493 ) ) ;
#44734 = DIRECTION ( 'NONE',  ( 0.000000000000000000, 0.000000000000000000, -1.000000000000000000 ) ) ;
#44735 = DIRECTION ( 'NONE',  ( 0.000000000000000000, 0.000000000000000000, 1.000000000000000000 ) ) ;
#44736 = CARTESIAN_POINT ( 'NONE',  ( -0.6971942568897626646, 0.07405724077823318263, 0.2755905511273391006 ) ) ;
#44737 = CARTESIAN_POINT ( 'NONE',  ( -0.1264236179284866091, -1.822466487914279565, 0.1264236179284866091 ) ) ;
#44738 = ORIENTED_EDGE ( 'NONE', *, *, #23162, .F. ) ;
#44739 = FACE_OUTER_BOUND ( 'NONE', #15467, .T. ) ;
#44740 = ORIENTED_EDGE ( 'NONE', *, *, #23614, .F. ) ;
#44741 = CARTESIAN_POINT ( 'NONE',  ( -1.054774247047244096, 0.000000000000000000, 1.483759842465921075 ) ) ;
#44742 = ORIENTED_EDGE ( 'NONE', *, *, #11017, .T. ) ;
#44743 = CARTESIAN_POINT ( 'NONE',  ( -0.1787899950787401604, -1.267716535379307619, -0.07405724077823318263 ) ) ;
#44744 = CARTESIAN_POINT ( 'NONE',  ( 0.07405724077823318263, -1.548228346402928723, -0.1787899950787401604 ) ) ;
#44745 = CARTESIAN_POINT ( 'NONE',  ( 0.4028871391076110364, 4.616380251121755931E-17, 0.000000000000000000 ) ) ;
#44746 = DIRECTION ( 'NONE',  ( 0.000000000000000000, 0.000000000000000000, -1.000000000000000000 ) ) ;
#44747 = VECTOR ( 'NONE', #32043, 39.37007874015748143 ) ;
#44748 = AXIS2_PLACEMENT_3D ( 'NONE', #7677, #32648, #29067 ) ;
#44749 = FACE_OUTER_BOUND ( 'NONE', #9529, .T. ) ;
#44750 = CARTESIAN_POINT ( 'NONE',  ( -0.9412147342319837628, -0.1574803149606297803, 1.016240157372787722 ) ) ;
#44751 = CARTESIAN_POINT ( 'NONE',  ( 0.8759842519685039353, -0.1787899950787401882, 0.05167322829269314910 ) ) ;
#44753 = CARTESIAN_POINT ( 'NONE',  ( 1.033464566929133799, 0.000000000000000000, 1.771653543199558811 ) ) ;
#44752 = CARTESIAN_POINT ( 'NONE',  ( 0.06523048226347956391, -0.3302165354330710012, 0.1574803149606297803 ) ) ;
#44754 = ( GEOMETRIC_REPRESENTATION_CONTEXT ( 3 ) GLOBAL_UNCERTAINTY_ASSIGNED_CONTEXT ( ( #18675 ) ) GLOBAL_UNIT_ASSIGNED_CONTEXT ( ( #33257, #3271, #18134 ) ) REPRESENTATION_CONTEXT ( 'NONE', 'WORKASPACE' ) ) ;
#44755 = CARTESIAN_POINT ( 'NONE',  ( 0.8107537697050253289, -0.1574803149606297803, 1.956200787294048338 ) ) ;
#44756 = ORIENTED_EDGE ( 'NONE', *, *, #15494, .F. ) ;
#44757 = CARTESIAN_POINT ( 'NONE',  ( -0.1331022545968926496, -0.09301241491031153608, -0.1193785939374830685 ) ) ;
#44758 = CARTESIAN_POINT ( 'NONE',  ( -0.7495606340400177148, -0.1264236179284866091, 0.9178149605761574126 ) ) ;
#44759 = CARTESIAN_POINT ( 'NONE',  ( 0.9412147342319837628, 0.1574803149606300301, 1.001476377952755348 ) ) ;
#44760 = FACE_BOUND ( 'NONE', #32947, .T. ) ;
#44761 = CARTESIAN_POINT ( 'NONE',  ( -0.2066929133858267931, -0.9654866319674424435, -1.480939111413832610 ) ) ;
#44762 = CARTESIAN_POINT ( 'NONE',  ( -0.1692806188707426940, -0.08955568274170122578, -0.02334579719831987241 ) ) ;
#44763 = VERTEX_POINT ( 'NONE', #38973 ) ;
#44764 = FACE_OUTER_BOUND ( 'NONE', #19762, .T. ) ;
#44765 = ADVANCED_FACE ( 'NONE', ( #2548 ), #6137, .T. ) ;
#44766 = ORIENTED_EDGE ( 'NONE', *, *, #42126, .F. ) ;
#44767 = CARTESIAN_POINT ( 'NONE',  ( -1.033464566929133799, 0.000000000000000000, 1.938976377952756014 ) ) ;
#44768 = CARTESIAN_POINT ( 'NONE',  ( 0.000000000000000000, 0.000000000000000000, -0.2748405511811023438 ) ) ;
#44769 = CARTESIAN_POINT ( 'NONE',  ( -1.094772975963752103E-17, -1.624507873961984261, -0.1787899950787401882 ) ) ;
#44770 = CARTESIAN_POINT ( 'NONE',  ( -0.1264236179284866091, -0.9060039369541103005, 0.1264236179284866091 ) ) ;
#44771 = CARTESIAN_POINT ( 'NONE',  ( -9.642888182262618425E-18, -1.179133858267716661, -0.1574803149606299191 ) ) ;
#44772 = CARTESIAN_POINT ( 'NONE',  ( 1.033464566929133799, 0.000000000000000000, 1.102362204616881947 ) ) ;
#44773 = EDGE_CURVE ( 'NONE', #30751, #2574, #22595, .T. ) ;
#44774 = CYLINDRICAL_SURFACE ( 'NONE', #28337, 0.1574803149606299191 ) ;
#44775 = ORIENTED_EDGE ( 'NONE', *, *, #30651, .T. ) ;
#44776 = ORIENTED_EDGE ( 'NONE', *, *, #44920, .T. ) ;
#44777 = CARTESIAN_POINT ( 'NONE',  ( -1.002407869896990045, 0.1264236179284866091, 1.764271653489543290 ) ) ;
#44778 = CARTESIAN_POINT ( 'NONE',  ( -0.7646288533564489232, 0.1113553986120547346, 0.5364173228346457156 ) ) ;
#44779 = EDGE_CURVE ( 'NONE', #29186, #19046, #12678, .T. ) ;
#44780 = CARTESIAN_POINT ( 'NONE',  ( 0.6971942568897648851, -0.07405724077823297447, 1.742125984198204858 ) ) ;
#44781 = CARTESIAN_POINT ( 'NONE',  ( 0.06523048226347956391, -1.304625984144440309, 0.1574803149606297803 ) ) ;
#44782 = CARTESIAN_POINT ( 'NONE',  ( 0.7185039370078692977, 0.06523048226347515077, 1.473917322727118506 ) ) ;
#44783 = CARTESIAN_POINT ( 'NONE',  ( 0.8759842519685039353, -0.1787899950787401882, 0.2928149605761578567 ) ) ;
#44784 = CARTESIAN_POINT ( 'NONE',  ( -1.002407869896990045, -0.1264236179284866091, 1.355807086560409491 ) ) ;
#44785 = EDGE_CURVE ( 'NONE', #24545, #26852, #27410, .T. ) ;
#44786 = DIRECTION ( 'NONE',  ( -1.000000000000000000, 0.000000000000000000, 0.000000000000000000 ) ) ;
#44787 = CARTESIAN_POINT ( 'NONE',  ( -0.6971942568897637749, 2.189545951927499583E-17, 1.183562992072220599 ) ) ;
#44788 = CARTESIAN_POINT ( 'NONE',  ( -1.002407869896990045, 0.1264236179284866091, 0.8932086613635591421 ) ) ;
#44789 = DIRECTION ( 'NONE',  ( 0.000000000000000000, 0.000000000000000000, -1.000000000000000000 ) ) ;
#44790 = CARTESIAN_POINT ( 'NONE',  ( -1.054774247047244096, 0.000000000000000000, 1.641240157426551161 ) ) ;
#44791 = CARTESIAN_POINT ( 'NONE',  ( -0.8759842519685039353, 0.1787899950787401882, 0.03690944876513417572 ) ) ;
#44792 = AXIS2_PLACEMENT_3D ( 'NONE', #25077, #20295, #27774 ) ;
#44793 = AXIS2_PLACEMENT_3D ( 'NONE', #45087, #12549, #24026 ) ;
#44794 = CARTESIAN_POINT ( 'NONE',  ( -1.033464566929133799, 0.000000000000000000, 1.545275590551181244 ) ) ;
#44795 = CARTESIAN_POINT ( 'NONE',  ( 0.7185039370078714072, 0.06523048226347728795, 1.641240157480314377 ) ) ;
#44796 = CARTESIAN_POINT ( 'NONE',  ( 0.6971942568897637749, 2.189545951927499583E-17, 1.621555118056472455 ) ) ;
#44797 = CARTESIAN_POINT ( 'NONE',  ( -0.01524196446234527512, -0.09851383026906693208, 0.1563901584214165141 ) ) ;
#44798 = CARTESIAN_POINT ( 'NONE',  ( 1.033464566929134687, 0.06523048226347956391, 0.1993110235145201248 ) ) ;
#44799 = CARTESIAN_POINT ( 'NONE',  ( -1.033464566929133799, 0.000000000000000000, 1.781496062992125928 ) ) ;
#44800 = AXIS2_PLACEMENT_3D ( 'NONE', #38285, #9771, #35414 ) ;
#44801 = VERTEX_POINT ( 'NONE', #9763 ) ;
#44802 = ORIENTED_EDGE ( 'NONE', *, *, #5293, .T. ) ;
#44803 = VERTEX_POINT ( 'NONE', #46401 ) ;
#44804 = ORIENTED_EDGE ( 'NONE', *, *, #4041, .F. ) ;
#44805 = CARTESIAN_POINT ( 'NONE',  ( -1.094772975963752103E-17, -0.8813976377415118080, -0.1787899950787401882 ) ) ;
#44806 = CARTESIAN_POINT ( 'NONE',  ( 0.1264236179284866091, -1.009350393647023614, 0.1264236179284866091 ) ) ;
#44807 = EDGE_CURVE ( 'NONE', #44831, #39516, #24136, .T. ) ;
#44808 = CARTESIAN_POINT ( 'NONE',  ( 0.1377952755905511861, 0.1574803149606299191, 0.8070866141732283561 ) ) ;
#44809 = CARTESIAN_POINT ( 'NONE',  ( -0.1797182628040039087, -0.3135280615515493308, 0.07444174185955065859 ) ) ;
#44810 = CARTESIAN_POINT ( 'NONE',  ( 0.1574803149606299191, 0.1496062992125984370, -1.928577636452523993E-17 ) ) ;
#44811 = PRODUCT_DEFINITION_SHAPE ( 'NONE', 'NONE',  #47466 ) ;
#44812 = CARTESIAN_POINT ( 'NONE',  ( -0.07405724077823318263, -0.1555118109698585271, 0.1787899950787401604 ) ) ;
#44813 = VECTOR ( 'NONE', #40634, 39.37007874015748143 ) ;
#44814 = CARTESIAN_POINT ( 'NONE',  ( -1.033464566929133799, 0.000000000000000000, 0.1279527559055118058 ) ) ;
#44815 = CARTESIAN_POINT ( 'NONE',  ( 1.002407869896990045, -0.1264236179284866091, 0.7258858267178898149 ) ) ;
#44816 = LINE ( 'NONE', #968, #7857 ) ;
#44817 = DIRECTION ( 'NONE',  ( 1.000000000000000000, 0.000000000000000000, -0.000000000000000000 ) ) ;
#44818 = CARTESIAN_POINT ( 'NONE',  ( -0.7185039370078714072, 0.06523048226347728795, 1.316437007766489531 ) ) ;
#44819 = CARTESIAN_POINT ( 'NONE',  ( 0.8759842519685039353, -0.1787899950787401882, 1.788877952702141672 ) ) ;
#44820 = CIRCLE ( 'NONE', #24944, 0.1574803149606292529 ) ;
#44821 = ORIENTED_EDGE ( 'NONE', *, *, #38804, .F. ) ;
#44822 = CARTESIAN_POINT ( 'NONE',  ( 0.9873396505805591694, -0.1113553986120547346, 0.1230314960629921295 ) ) ;
#44823 = DIRECTION ( 'NONE',  ( -1.000000000000000000, 0.000000000000000000, 0.000000000000000000 ) ) ;
#44824 = CARTESIAN_POINT ( 'NONE',  ( -0.1787899950787401604, -0.4803149605761579677, -0.07405724077823318263 ) ) ;
#44825 = DIRECTION ( 'NONE',  ( -1.000000000000000000, 0.000000000000000000, 0.000000000000000000 ) ) ;
#44826 = CARTESIAN_POINT ( 'NONE',  ( -0.07405724077823318263, -1.267716535379307619, -0.1787899950787401604 ) ) ;
#44827 = CARTESIAN_POINT ( 'NONE',  ( 0.6971942568897637749, 2.189545951927499583E-17, 0.2436023621509610382 ) ) ;
#44828 = ADVANCED_FACE ( 'NONE', ( #24604 ), #45924, .F. ) ;
#44829 = DIRECTION ( 'NONE',  ( 1.822029033848725028E-16, 0.000000000000000000, 1.000000000000000000 ) ) ;
#44830 = CARTESIAN_POINT ( 'NONE',  ( -1.054774247047244096, 0.000000000000000000, 1.715059055064346527 ) ) ;
#44831 = VERTEX_POINT ( 'NONE', #28705 ) ;
#44832 = CARTESIAN_POINT ( 'NONE',  ( -0.6971942568897648851, 0.07405724077823318263, 1.304133858213953667 ) ) ;
#44833 = CARTESIAN_POINT ( 'NONE',  ( 0.8759842519685039353, -0.1787899950787401882, 1.237696850339937038 ) ) ;
#44834 = CARTESIAN_POINT ( 'NONE',  ( -0.8019270111902717657, 0.1787899950787401604, 0.5511811023084406402 ) ) ;
#44835 = CARTESIAN_POINT ( 'NONE',  ( 1.054774247047244096, 0.000000000000000000, 1.911909448765133801 ) ) ;
#44836 = CARTESIAN_POINT ( 'NONE',  ( -0.9500414927467378812, -0.1787899950787401604, 1.156496062938362046 ) ) ;
#44837 = CARTESIAN_POINT ( 'NONE',  ( -0.8759842519685039353, 0.000000000000000000, 0.000000000000000000 ) ) ;
#44838 = ADVANCED_FACE ( 'NONE', ( #10478 ), #15759, .T. ) ;
#44839 = CARTESIAN_POINT ( 'NONE',  ( 0.03891730292714078859, -0.09842393336832859496, -0.1745031462337006123 ) ) ;
#44840 = CARTESIAN_POINT ( 'NONE',  ( 0.7185039370078746268, 0.06523048226347956391, 1.208169291338584417 ) ) ;
#44841 = CARTESIAN_POINT ( 'NONE',  ( 0.8019270111902716547, -0.1787899950787401604, 0.5265748030958428139 ) ) ;
#44842 = CARTESIAN_POINT ( 'NONE',  ( -0.8019270111902716547, 0.1787899950787401604, 0.4281496062454490659 ) ) ;
#44843 = CARTESIAN_POINT ( 'NONE',  ( -0.8759842519685039353, 0.1787899950787401882, 0.8587598424659212970 ) ) ;
#44844 = ORIENTED_EDGE ( 'NONE', *, *, #8070, .T. ) ;
#44845 = DIRECTION ( 'NONE',  ( -0.5000000000000007772, -0.8660254037844382635, 0.000000000000000000 ) ) ;
#44846 = ORIENTED_EDGE ( 'NONE', *, *, #12788, .T. ) ;
#44847 = CARTESIAN_POINT ( 'NONE',  ( -1.033464566929134687, -0.06523048226347956391, 0.1254921259842518844 ) ) ;
#44848 = DIRECTION ( 'NONE',  ( 0.000000000000000000, 0.000000000000000000, -1.000000000000000000 ) ) ;
#44849 = ORIENTED_EDGE ( 'NONE', *, *, #35453, .T. ) ;
#44850 = CARTESIAN_POINT ( 'NONE',  ( -0.8759842519685039353, 0.000000000000000000, 1.978346456692913646 ) ) ;
#44851 = CARTESIAN_POINT ( 'NONE',  ( -0.8107537697050254399, 0.1574803149606300301, 1.468996062884598830 ) ) ;
#44852 = CARTESIAN_POINT ( 'NONE',  ( -0.9500414927467378812, 0.1787899950787401604, 0.06889763774151215492 ) ) ;
#44853 = CARTESIAN_POINT ( 'NONE',  ( -0.1787899950787401882, -1.394316881615065284, 0.000000000000000000 ) ) ;
#44854 = ORIENTED_EDGE ( 'NONE', *, *, #10694, .F. ) ;
#44855 = CARTESIAN_POINT ( 'NONE',  ( -0.1264236179284866091, -0.4384842519147402196, -0.1264236179284866091 ) ) ;
#44856 = DIRECTION ( 'NONE',  ( -1.000000000000000000, 0.000000000000000000, -6.938893903907220489E-15 ) ) ;
#44857 = ORIENTED_EDGE ( 'NONE', *, *, #13253, .F. ) ;
#44858 = CARTESIAN_POINT ( 'NONE',  ( 0.6971942568897648851, -0.07405724077823297447, 1.343503936954111744 ) ) ;
#44859 = CARTESIAN_POINT ( 'NONE',  ( 0.1377952755905511861, 0.1564960629921262614, 0.9074803149606294195 ) ) ;
#44860 = EDGE_CURVE ( 'NONE', #26440, #43205, #28950, .T. ) ;
#44861 = DIRECTION ( 'NONE',  ( -3.469446951953613794E-15, -1.000000000000000000, 0.000000000000000000 ) ) ;
#44862 = CARTESIAN_POINT ( 'NONE',  ( 0.6971942568897637749, 2.189545951927499583E-17, 1.656003936954110412 ) ) ;
#44863 = CARTESIAN_POINT ( 'NONE',  ( 0.7495606340400177148, 0.1264236179284866091, 0.2337598424659216578 ) ) ;
#44864 = CARTESIAN_POINT ( 'NONE',  ( 3.284318927891251994E-17, -1.767224409395055318, 0.1787899950787401882 ) ) ;
#44865 = CARTESIAN_POINT ( 'NONE',  ( -0.1787899950787401604, 0.1151574803687242243, 0.07405724077823318263 ) ) ;
#44866 = LINE ( 'NONE', #26701, #32632 ) ;
#44867 = CARTESIAN_POINT ( 'NONE',  ( -0.9500414927467377701, 0.1787899950787401604, 0.7037401574265510495 ) ) ;
#44868 = DIRECTION ( 'NONE',  ( 0.000000000000000000, 0.000000000000000000, -1.000000000000000000 ) ) ;
#44870 = CARTESIAN_POINT ( 'NONE',  ( 0.4330708661417322913, 0.1574803149606299191, -1.186023622047243986 ) ) ;
#44869 = CARTESIAN_POINT ( 'NONE',  ( 0.06523048226347956391, -0.7485236220472446522, -0.1574803149606300301 ) ) ;
#44871 = CARTESIAN_POINT ( 'NONE',  ( 0.1270800023317771588, -1.393744596984620054, -0.1270800023317771588 ) ) ;
#44872 = CARTESIAN_POINT ( 'NONE',  ( 0.2471922904502826257, 0.07780974138651140792, -0.07762775726530279918 ) ) ;
#44873 = CARTESIAN_POINT ( 'NONE',  ( 0.9500414927467378812, -0.1787899950787401604, 1.358267716481669662 ) ) ;
#44874 = CARTESIAN_POINT ( 'NONE',  ( 1.054774247047244096, 0.000000000000000000, 1.911909448765133801 ) ) ;
#44875 = CONICAL_SURFACE ( 'NONE', #34971, 0.09842519685039320676, 0.7853981633972574317 ) ;
#44877 = ORIENTED_EDGE ( 'NONE', *, *, #35015, .T. ) ;
#44876 = CYLINDRICAL_SURFACE ( 'NONE', #769, 0.1574803149606299191 ) ;
#44878 = CARTESIAN_POINT ( 'NONE',  ( -0.8759842519685039353, 0.1574803149606299191, 1.515748031496062964 ) ) ;
#44879 = CYLINDRICAL_SURFACE ( 'NONE', #41971, 0.1864803149606298338 ) ;
#44881 = CYLINDRICAL_SURFACE ( 'NONE', #43092, 0.1574803149606299191 ) ;
#44880 = CARTESIAN_POINT ( 'NONE',  ( -9.642888182262618425E-18, -0.8149606298137322957, -0.1574803149606299191 ) ) ;
#44882 = DIRECTION ( 'NONE',  ( -1.000000000000000000, 0.000000000000000000, 6.123233995736769734E-17 ) ) ;
#44883 = CARTESIAN_POINT ( 'NONE',  ( 0.8019270111902717657, 0.1787899950787401604, 0.2706692912848194243 ) ) ;
#44884 = EDGE_CURVE ( 'NONE', #10815, #19533, #7491, .T. ) ;
#44885 = CARTESIAN_POINT ( 'NONE',  ( 0.2642359194686346169, 4.766607801171850497E-17, 0.000000000000000000 ) ) ;
#44886 = DIRECTION ( 'NONE',  ( 0.000000000000000000, -1.000000000000000000, 0.000000000000000000 ) ) ;
#44887 = CARTESIAN_POINT ( 'NONE',  ( -1.033464566929134687, 0.06523048226347956391, 0.9473425195775121432 ) ) ;
#44888 = CARTESIAN_POINT ( 'NONE',  ( 0.7646288533564489232, 0.1113553986120547346, 0.6840551180027086842 ) ) ;
#44889 = ORIENTED_EDGE ( 'NONE', *, *, #9710, .T. ) ;
#44890 = ( CONVERSION_BASED_UNIT ( 'INCH', #3941 ) LENGTH_UNIT ( ) NAMED_UNIT ( #31711 ) ) ;
#44891 = CARTESIAN_POINT ( 'NONE',  ( 0.8498898284424959426, 0.1741572742611180169, 0.03937012805171165308 ) ) ;
#44892 = ORIENTED_EDGE ( 'NONE', *, *, #39795, .T. ) ;
#44893 = CARTESIAN_POINT ( 'NONE',  ( 3.301370929368692659E-17, -0.1092957780869824730, 0.1797182628040039365 ) ) ;
#44894 = CARTESIAN_POINT ( 'NONE',  ( -0.07405724077823318263, -1.139763779473794925, 0.1787899950787401604 ) ) ;
#44895 = CARTESIAN_POINT ( 'NONE',  ( -0.7185039370078739607, 1.928577636452523993E-17, 1.210629921259842590 ) ) ;
#44896 = CARTESIAN_POINT ( 'NONE',  ( 0.6971942568897648851, 0.07405724077823318263, 1.535433070812378675 ) ) ;
#44897 = CARTESIAN_POINT ( 'NONE',  ( -0.7646288533564489232, 0.1113553986120547346, 1.245078740157480324 ) ) ;
#44898 = ADVANCED_FACE ( 'NONE', ( #25574 ), #11415, .F. ) ;
#44899 = CARTESIAN_POINT ( 'NONE',  ( -0.7185039370078714072, 0.06523048226347728795, 1.158956692805858779 ) ) ;
#44901 = DIRECTION ( 'NONE',  ( -1.000000000000000000, 0.000000000000000000, 0.000000000000000000 ) ) ;
#44900 = DIRECTION ( 'NONE',  ( 3.469446951953613794E-15, 1.000000000000000000, 0.000000000000000000 ) ) ;
#44902 = LINE ( 'NONE', #12598, #12071 ) ;
#44903 = ORIENTED_EDGE ( 'NONE', *, *, #46571, .F. ) ;
#44904 = DIRECTION ( 'NONE',  ( 0.000000000000000000, -0.7880107536067212370, 0.6156614753256591799 ) ) ;
#44905 = VERTEX_POINT ( 'NONE', #39912 ) ;
#44906 = CARTESIAN_POINT ( 'NONE',  ( -0.7495606340400177148, -0.1264236179284866091, 1.542814960576157413 ) ) ;
#44907 = CARTESIAN_POINT ( 'NONE',  ( 0.1574803149606300301, 0.004429133965794757564, -0.06523048226347956391 ) ) ;
#44908 = CARTESIAN_POINT ( 'NONE',  ( -0.6971942568897648851, -0.07405724077823297447, 1.348425196796630976 ) ) ;
#44909 = VERTEX_POINT ( 'NONE', #26033 ) ;
#44910 = VECTOR ( 'NONE', #30527, 39.37007874015748143 ) ;
#44911 = DIRECTION ( 'NONE',  ( 0.000000000000000000, 0.000000000000000000, -1.000000000000000000 ) ) ;
#44912 = CARTESIAN_POINT ( 'NONE',  ( -0.8019270111902717657, -0.1787899950787401604, 0.2903543306548980185 ) ) ;
#44913 = CARTESIAN_POINT ( 'NONE',  ( 0.7646288533564489232, -0.1113553986120547346, 0.6643700787401575214 ) ) ;
#44914 = CARTESIAN_POINT ( 'NONE',  ( 0.7185039370078739607, 1.928577636452523993E-17, 0.5807086614173228023 ) ) ;
#44915 = CARTESIAN_POINT ( 'NONE',  ( -0.07405724077823318263, -1.032604283189868521, 0.1787899950787401604 ) ) ;
#44916 = ORIENTED_EDGE ( 'NONE', *, *, #24552, .F. ) ;
#44917 = CARTESIAN_POINT ( 'NONE',  ( 0.1787899950787401604, 0.09547244099864542199, 0.07405724077823318263 ) ) ;
#44918 = EDGE_LOOP ( 'NONE', ( #27877, #10057, #40607, #18064 ) ) ;
#44919 = CARTESIAN_POINT ( 'NONE',  ( -0.8759842519685039353, -0.1574803149606299191, 0.2657480313885358103 ) ) ;
#44920 = EDGE_CURVE ( 'NONE', #1283, #42583, #25413, .T. ) ;
#44921 = CARTESIAN_POINT ( 'NONE',  ( -0.4620708661417322616, 1.354170115732555191, -0.4197102375732078561 ) ) ;
#44922 = CARTESIAN_POINT ( 'NONE',  ( 0.9412147342319837628, 0.1574803149606300301, 1.818405511703497845 ) ) ;
#44923 = CARTESIAN_POINT ( 'NONE',  ( -1.002407869896990045, 0.1264236179284866091, 0.2288385826234019815 ) ) ;
#44924 = CARTESIAN_POINT ( 'NONE',  ( -0.8107537697050253289, -0.1574803149606297803, 0.9030511811023627100 ) ) ;
#44925 = CARTESIAN_POINT ( 'NONE',  ( -0.1270800023317771588, -0.9803587702129665793, 0.1270800023317771588 ) ) ;
#44926 = CARTESIAN_POINT ( 'NONE',  ( 0.1748756820900291831, 0.1299212598425196763, 0.008513987618672504490 ) ) ;
#44927 = EDGE_CURVE ( 'NONE', #43250, #44104, #45122, .T. ) ;
#44928 = CARTESIAN_POINT ( 'NONE',  ( 1.054774247047244096, 0.000000000000000000, 0.9325787401037164415 ) ) ;
#44929 = CARTESIAN_POINT ( 'NONE',  ( 0.8019270111902716547, -0.1787899950787401604, 1.427165354276944687 ) ) ;
#44930 = CARTESIAN_POINT ( 'NONE',  ( -0.8107537697050254399, 0.1574803149606300301, 0.4552165354330711677 ) ) ;
#44931 = CARTESIAN_POINT ( 'NONE',  ( 0.7185039370078746268, 0.06523048226347956391, 1.641240157480315931 ) ) ;
#44933 = CARTESIAN_POINT ( 'NONE',  ( 0.2204724409448818867, 0.07955613945526338049, -0.1377952755905511861 ) ) ;
#44932 = CARTESIAN_POINT ( 'NONE',  ( 0.7108616290341307486, -0.02448449591372561102, 1.983713913184816713 ) ) ;
#44934 = DIRECTION ( 'NONE',  ( -7.005971165215254420E-15, 0.7880107536067203489, -0.6156614753256602901 ) ) ;
#44935 = CIRCLE ( 'NONE', #35765, 0.1574803149606292529 ) ;
#44936 = CARTESIAN_POINT ( 'NONE',  ( 0.1264236179284866091, 0.09301181107738563936, 0.1264236179284866091 ) ) ;
#44937 = DIRECTION ( 'NONE',  ( 0.000000000000000000, 0.7071067811865965336, 0.7071067811864983899 ) ) ;
#44938 = ADVANCED_FACE ( 'NONE', ( #11661 ), #32301, .T. ) ;
#44940 = CARTESIAN_POINT ( 'NONE',  ( 0.3727034120734909473, 0.08090551181102362266, 0.000000000000000000 ) ) ;
#44939 = CARTESIAN_POINT ( 'NONE',  ( 0.7495606340400177148, -0.1264236179284866091, 0.7554133857730077617 ) ) ;
#44941 = CARTESIAN_POINT ( 'NONE',  ( 0.6971942568897637749, 2.189545951927499583E-17, 1.857775590497417362 ) ) ;
#44942 = CARTESIAN_POINT ( 'NONE',  ( 0.1787899950787401604, -0.9281496062454495100, 0.07405724077823318263 ) ) ;
#44943 = ORIENTED_EDGE ( 'NONE', *, *, #43745, .T. ) ;
#44944 = CARTESIAN_POINT ( 'NONE',  ( 0.9412147342319837628, 0.1574803149606300301, 0.9227362204724415262 ) ) ;
#44945 = CARTESIAN_POINT ( 'NONE',  ( 0.000000000000000000, 0.000000000000000000, -0.2886241641379866385 ) ) ;
#44946 = CARTESIAN_POINT ( 'NONE',  ( -0.1113553986120547346, -1.745078740049952781, 0.1113553986120547346 ) ) ;
#44947 = DIRECTION ( 'NONE',  ( 0.000000000000000000, 0.000000000000000000, -1.000000000000000000 ) ) ;
#44948 = CARTESIAN_POINT ( 'NONE',  ( 0.7495606340400177148, 0.1264236179284866091, 1.099901574749385880 ) ) ;
#44949 = EDGE_CURVE ( 'NONE', #7704, #44149, #3493, .T. ) ;
#44950 = CYLINDRICAL_SURFACE ( 'NONE', #28792, 0.1574803149606299191 ) ;
#44951 = CARTESIAN_POINT ( 'NONE',  ( 0.1113553986120547346, -1.656496062992126150, -0.1113553986120547346 ) ) ;
#44952 = DIRECTION ( 'NONE',  ( 0.000000000000000000, -0.000000000000000000, 1.000000000000000000 ) ) ;
#44953 = FACE_OUTER_BOUND ( 'NONE', #24314, .T. ) ;
#44954 = CARTESIAN_POINT ( 'NONE',  ( -0.6971942568897637749, 2.189545951927499583E-17, 0.3174212597887562382 ) ) ;
#44955 = VERTEX_POINT ( 'NONE', #889 ) ;
#44956 = CARTESIAN_POINT ( 'NONE',  ( 0.1787899950787401604, -1.558070866087969630, -0.07405724077823318263 ) ) ;
#44957 = CARTESIAN_POINT ( 'NONE',  ( -1.054774247047244096, 0.000000000000000000, 1.833169291284818758 ) ) ;
#44958 = CARTESIAN_POINT ( 'NONE',  ( -0.7495606340400177148, -0.1264236179284866091, 0.9128937007336377363 ) ) ;
#44959 = CARTESIAN_POINT ( 'NONE',  ( -1.054774247047244540, 0.07405724077823318263, 0.5413385826234012876 ) ) ;
#44960 = LINE ( 'NONE', #34448, #16108 ) ;
#44961 = CIRCLE ( 'NONE', #12855, 0.4724409448818896462 ) ;
#44962 = CARTESIAN_POINT ( 'NONE',  ( -0.7185039370078739607, 1.928577636452523993E-17, 1.919291338582677309 ) ) ;
#44963 = FACE_BOUND ( 'NONE', #29443, .T. ) ;
#44964 = DIRECTION ( 'NONE',  ( 0.000000000000000000, -0.6156614753256619554, -0.7880107536067190166 ) ) ;
#44965 = CARTESIAN_POINT ( 'NONE',  ( 0.1787899950787401882, -0.5084901099615219966, -2.189545951927503898E-17 ) ) ;
#44966 = CARTESIAN_POINT ( 'NONE',  ( -0.1080892699026834713, -0.08955964444840118499, -0.2261462449159996335 ) ) ;
#44967 = DIRECTION ( 'NONE',  ( 0.000000000000000000, -1.000000000000000000, 0.000000000000000000 ) ) ;
#44968 = DIRECTION ( 'NONE',  ( -0.000000000000000000, 1.000000000000000000, -3.995705278811693553E-31 ) ) ;
#44969 = CARTESIAN_POINT ( 'NONE',  ( -1.054774247047244540, -0.07405724077823318263, 0.4133858267178901480 ) ) ;
#44970 = CARTESIAN_POINT ( 'NONE',  ( -0.8759842519685039353, -0.1574803149606299191, 0.3937007874015748254 ) ) ;
#44971 = ORIENTED_EDGE ( 'NONE', *, *, #25577, .F. ) ;
#44972 = DIRECTION ( 'NONE',  ( -1.000000000000000000, 0.000000000000000000, 0.000000000000000000 ) ) ;
#44973 = CARTESIAN_POINT ( 'NONE',  ( -1.002407869896990045, -0.1264236179284866091, 1.518208661363559031 ) ) ;
#44974 = CARTESIAN_POINT ( 'NONE',  ( -0.1264236179284866091, -1.378444881836000002, 0.1264236179284866091 ) ) ;
#44975 = CARTESIAN_POINT ( 'NONE',  ( -0.1264236179284866091, -1.570374015694267600, 0.1264236179284866091 ) ) ;
#44976 = ( BOUNDED_CURVE ( )  B_SPLINE_CURVE ( 2, ( #15685, #40564, #7754, #8226, #22372, #25981, #22617, #44168, #30545 ),
 .UNSPECIFIED., .F., .F. ) 
 B_SPLINE_CURVE_WITH_KNOTS ( ( 3, 2, 2, 2, 3 ),
 ( 0.1799999999999999933, 0.1824999999999999956, 0.1849999999999999978, 0.1875000000000000000, 0.1900000000000000022 ),
 .UNSPECIFIED. ) 
 CURVE ( )  GEOMETRIC_REPRESENTATION_ITEM ( )  RATIONAL_B_SPLINE_CURVE ( ( 1.000000000000000000, 0.9238795325112869605, 1.000000000000000000, 0.9238795325112869605, 1.000000000000000000, 0.9238795325112869605, 1.000000000000000000, 0.9238795325112869605, 1.000000000000000000 ) ) 
 REPRESENTATION_ITEM ( '' )  ) ;
#44977 = ( NAMED_UNIT ( * ) SI_UNIT ( $, .STERADIAN. ) SOLID_ANGLE_UNIT ( ) ) ;
#44978 = DIRECTION ( 'NONE',  ( 0.000000000000000000, 0.000000000000000000, 1.000000000000000000 ) ) ;
#44979 = ADVANCED_BREP_SHAPE_REPRESENTATION ( 'Pivot Shaft', ( #20411, #20860 ), #43813 ) ;
#44980 = CARTESIAN_POINT ( 'NONE',  ( 1.033464566929133799, 0.000000000000000000, 0.4822834645669291653 ) ) ;
#44981 = DIRECTION ( 'NONE',  ( 3.469446951953631938E-15, 1.000000000000000000, 0.000000000000000000 ) ) ;
#44982 = CARTESIAN_POINT ( 'NONE',  ( -0.8759842519685039353, -0.1574803149606299191, 1.131889763672000004 ) ) ;
#44983 = EDGE_CURVE ( 'NONE', #36086, #11894, #8330, .T. ) ;
#44984 = CARTESIAN_POINT ( 'NONE',  ( 0.6971942568897626646, -0.07405724077823297447, 0.6003937007336389575 ) ) ;
#44985 = CARTESIAN_POINT ( 'NONE',  ( 0.8759842519685039353, -0.1787899950787401882, 0.09104330703285078152 ) ) ;
#44987 = DIRECTION ( 'NONE',  ( 1.000000000000000000, 0.000000000000000000, 0.000000000000000000 ) ) ;
#44986 = CARTESIAN_POINT ( 'NONE',  ( -0.1574803149606300301, -0.2268700787401574381, -0.06523048226347956391 ) ) ;
#44988 = CARTESIAN_POINT ( 'NONE',  ( 0.7185039370078746268, -0.06523048226347956391, 1.911909448711371917 ) ) ;
#44989 = EDGE_LOOP ( 'NONE', ( #923, #2465, #19139, #23186 ) ) ;
#44990 = FACE_OUTER_BOUND ( 'NONE', #4170, .T. ) ;
#44991 = CARTESIAN_POINT ( 'NONE',  ( 0.8107537697050253289, -0.1574803149606297803, 0.9817913385826764205 ) ) ;
#44992 = CARTESIAN_POINT ( 'NONE',  ( -0.8759842519685039353, 0.000000000000000000, 0.000000000000000000 ) ) ;
#44993 = CARTESIAN_POINT ( 'NONE',  ( -0.4330708661417356775, 0.1864803149606299171, 1.186023622047243986 ) ) ;
#44994 = VECTOR ( 'NONE', #12205, 39.37007874015748143 ) ;
#44995 = CARTESIAN_POINT ( 'NONE',  ( 0.7185039370078739607, 1.928577636452523993E-17, 0.6102362203649134287 ) ) ;
#44996 = CARTESIAN_POINT ( 'NONE',  ( -0.1688682454601131422, -0.08956111721935616776, 0.008132950095326338738 ) ) ;
#44997 = ORIENTED_EDGE ( 'NONE', *, *, #4046, .F. ) ;
#44998 = CARTESIAN_POINT ( 'NONE',  ( 0.1574803149606299746, -5.122214988120488358E-16, 0.9783464566929127582 ) ) ;
#44999 = CARTESIAN_POINT ( 'NONE',  ( -0.3070313825494069282, 0.04447134000132128145, 0.7142919828228455614 ) ) ;
#45000 = ORIENTED_EDGE ( 'NONE', *, *, #25210, .T. ) ;
#45001 = CARTESIAN_POINT ( 'NONE',  ( 0.8759842519685039353, 0.1787899950787401882, 0.7406496062454487328 ) ) ;
#45002 = EDGE_LOOP ( 'NONE', ( #14002, #4791, #10898, #38145, #7624 ) ) ;
#45003 = DIRECTION ( 'NONE',  ( -1.000000000000000000, -0.000000000000000000, -0.000000000000000000 ) ) ;
#45004 = DIRECTION ( 'NONE',  ( 1.822029033848725028E-16, 0.000000000000000000, 1.000000000000000000 ) ) ;
#45005 = CARTESIAN_POINT ( 'NONE',  ( -0.1787899950787401604, -1.730314960576156968, 0.07405724077823318263 ) ) ;
#45006 = CARTESIAN_POINT ( 'NONE',  ( 3.284318927891251994E-17, -0.8223425196312754704, 0.1787899950787401882 ) ) ;
#45007 = CARTESIAN_POINT ( 'NONE',  ( 0.06523048226347956391, -1.181594488188976610, -0.1574803149606300301 ) ) ;
#45009 = ( BOUNDED_CURVE ( )  B_SPLINE_CURVE ( 2, ( #26250, #34156, #24361, #2535, #20520, #13347, #38959, #17163, #5906 ),
 .UNSPECIFIED., .F., .T. ) 
 B_SPLINE_CURVE_WITH_KNOTS ( ( 3, 2, 2, 2, 3 ),
 ( 0.08000000000000000167, 0.08250000000000000389, 0.08500000000000000611, 0.08749999999999999445, 0.08999999999999999667 ),
 .UNSPECIFIED. ) 
 CURVE ( )  GEOMETRIC_REPRESENTATION_ITEM ( )  RATIONAL_B_SPLINE_CURVE ( ( 1.000000000000000000, 0.9238795325112869605, 1.000000000000000000, 0.9238795325112869605, 1.000000000000000000, 0.9238795325112869605, 1.000000000000000000, 0.9238795325112869605, 1.000000000000000000 ) ) 
 REPRESENTATION_ITEM ( '' )  ) ;
#45008 = CARTESIAN_POINT ( 'NONE',  ( 0.9873396505805591694, -0.1113553986120547346, 1.176181102254677313 ) ) ;
#45010 = CARTESIAN_POINT ( 'NONE',  ( 0.7646288533564489232, 0.1113553986120547346, 1.835629921259842590 ) ) ;
#45011 = VERTEX_POINT ( 'NONE', #27296 ) ;
#45012 = ORIENTED_EDGE ( 'NONE', *, *, #25988, .T. ) ;
#45013 = CARTESIAN_POINT ( 'NONE',  ( -1.054774247047244540, -0.07405724077823318263, 1.756889763725764553 ) ) ;
#45014 = CARTESIAN_POINT ( 'NONE',  ( 0.8019270111902717657, 0.1787899950787401604, 1.889763779473794258 ) ) ;
#45015 = EDGE_LOOP ( 'NONE', ( #35614, #20480, #7132, #43316 ) ) ;
#45016 = CARTESIAN_POINT ( 'NONE',  ( -0.6971942568897637749, 2.189545951927499583E-17, 0.9128937007336377363 ) ) ;
#45017 = CARTESIAN_POINT ( 'NONE',  ( -0.01090721357322046656, -0.2891969495697969683, -0.2957398093695223773 ) ) ;
#45018 = CARTESIAN_POINT ( 'NONE',  ( 0.8759842519685039353, -0.1787899950787401882, 0.4896653542769449086 ) ) ;
#45019 = CARTESIAN_POINT ( 'NONE',  ( -0.8019270111902717657, -0.1787899950787401604, 1.348425196796630976 ) ) ;
#45020 = CARTESIAN_POINT ( 'NONE',  ( -0.7185039370078714072, 0.06523048226347728795, 1.513287401467276583 ) ) ;
#45021 = CARTESIAN_POINT ( 'NONE',  ( -1.054774247047244540, -0.07405724077823318263, 1.240157480261197875 ) ) ;
#45022 = CARTESIAN_POINT ( 'NONE',  ( -0.7185039370078739607, 0.000000000000000000, -2.869337061179095023E-17 ) ) ;
#45023 = CARTESIAN_POINT ( 'NONE',  ( -1.002407869896990045, 0.1264236179284866091, 1.724901574749385880 ) ) ;
#45024 = CARTESIAN_POINT ( 'NONE',  ( -1.002407869896990045, 0.1264236179284866091, 0.07135826766277185429 ) ) ;
#45025 = DIRECTION ( 'NONE',  ( -1.000000000000000000, 0.000000000000000000, 0.000000000000000000 ) ) ;
#45026 = CARTESIAN_POINT ( 'NONE',  ( -0.7646288533564489232, 0.1113553986120547346, 1.717519685039369914 ) ) ;
#45027 = CARTESIAN_POINT ( 'NONE',  ( -0.1184675242425147629, -0.09842519685039370636, 1.713085361781125471 ) ) ;
#45028 = CARTESIAN_POINT ( 'NONE',  ( 0.7495606340400177148, 0.1264236179284866091, 1.656003936954110412 ) ) ;
#45029 = CARTESIAN_POINT ( 'NONE',  ( 0.08605959628751140567, -0.09851382450317322514, 0.1221410806743637861 ) ) ;
#45030 = DIRECTION ( 'NONE',  ( 1.822029033848725028E-16, 0.000000000000000000, 1.000000000000000000 ) ) ;
#45031 = CIRCLE ( 'NONE', #22096, 0.09842519685039370636 ) ;
#45032 = ORIENTED_EDGE ( 'NONE', *, *, #15224, .F. ) ;
#45033 = CIRCLE ( 'NONE', #21344, 0.1013779527559055538 ) ;
#45034 = VERTEX_POINT ( 'NONE', #22959 ) ;
#45035 = ADVANCED_FACE ( 'NONE', ( #37324 ), #41845, .T. ) ;
#45036 = CARTESIAN_POINT ( 'NONE',  ( 0.1787899950787401604, -0.8149606298674965110, 0.07405724077823318263 ) ) ;
#45037 = AXIS2_PLACEMENT_3D ( 'NONE', #40605, #47112, #43750 ) ;
#45038 = EDGE_CURVE ( 'NONE', #11471, #22426, #23672, .T. ) ;
#45039 = CARTESIAN_POINT ( 'NONE',  ( 3.284318927891251994E-17, -1.093011810969858333, 0.1787899950787401882 ) ) ;
#45040 = CARTESIAN_POINT ( 'NONE',  ( -0.7185039370078739607, 1.928577636452523993E-17, 1.289370078740157632 ) ) ;
#45041 = CARTESIAN_POINT ( 'NONE',  ( 1.054774247047244540, 0.07405724077823318263, 1.835629921206078485 ) ) ;
#45042 = CARTESIAN_POINT ( 'NONE',  ( -0.07444174185955065859, -0.3873469591893448083, 0.1797182628040039087 ) ) ;
#45043 = EDGE_CURVE ( 'NONE', #28863, #6112, #37569, .T. ) ;
#45044 = CARTESIAN_POINT ( 'NONE',  ( 0.000000000000000000, -0.5708661417322835607, -6.991093932140394160E-17 ) ) ;
#45045 = CARTESIAN_POINT ( 'NONE',  ( -0.7185039370078739607, 1.928577636452523993E-17, 0.1476377952755905387 ) ) ;
#45046 = CARTESIAN_POINT ( 'NONE',  ( 1.002407869896990045, 0.1264236179284866091, 0.8144685038832440993 ) ) ;
#45047 = B_SPLINE_CURVE_WITH_KNOTS ( 'NONE', 3,
 ( #30845, #26528, #27009, #15746, #1559, #38236, #20017, #12625, #45412, #1806, #44926, #41553, #27248, #844, #8761, #9002 ),
 .UNSPECIFIED., .F., .F.,
 ( 4, 1, 2, 2, 2, 1, 2, 2, 4 ),
 ( 0.000000000000000000, 0.1250000000000000000, 0.1874999999999999445, 0.2499999999999999167, 0.5000000000000000000, 0.6250000000000000000, 0.6875000000000000000, 0.7500000000000000000, 1.000000000000000000 ),
 .UNSPECIFIED. ) ;
#45049 = CARTESIAN_POINT ( 'NONE',  ( 0.005686768416191418166, 0.09278660394097182351, 0.1148867573884606030 ) ) ;
#45048 = CARTESIAN_POINT ( 'NONE',  ( 0.04877781748284810287, 0.2673323462082016211, -0.06129781628411318933 ) ) ;
#45050 = CARTESIAN_POINT ( 'NONE',  ( -0.7646288533564489232, -0.1113553986120547346, 0.06397637784522892945 ) ) ;
#45051 = CARTESIAN_POINT ( 'NONE',  ( 0.8759842519685039353, 0.1574803149606299191, 0.08858267705782735257 ) ) ;
#45052 = ORIENTED_EDGE ( 'NONE', *, *, #9903, .F. ) ;
#45053 = CARTESIAN_POINT ( 'NONE',  ( 1.033464566929133799, 0.000000000000000000, 0.1673228346456692994 ) ) ;
#45054 = CARTESIAN_POINT ( 'NONE',  ( 0.000000000000000000, 0.000000000000000000, 0.09842519685039370636 ) ) ;
#45056 = CARTESIAN_POINT ( 'NONE',  ( 0.1787899950787401882, -0.4187992125446614589, -2.189545951927503898E-17 ) ) ;
#45055 = CARTESIAN_POINT ( 'NONE',  ( 0.1574803149606300301, -0.9847440943806630154, 0.06523048226347956391 ) ) ;
#45057 = LINE ( 'NONE', #12037, #9422 ) ;
#45058 = CARTESIAN_POINT ( 'NONE',  ( 0.07405724077823318263, -1.312007873961984705, -0.1787899950787401604 ) ) ;
#45059 = CARTESIAN_POINT ( 'NONE',  ( 0.9500414927467378812, -0.1787899950787401604, 0.2952755904974176393 ) ) ;
#45060 = FACE_OUTER_BOUND ( 'NONE', #17105, .T. ) ;
#45061 = AXIS2_PLACEMENT_3D ( 'NONE', #18725, #6765, #14444 ) ;
#45062 = CARTESIAN_POINT ( 'NONE',  ( -0.8759842519685039353, -0.1787899950787401882, 1.823326771599779406 ) ) ;
#45063 = ORIENTED_EDGE ( 'NONE', *, *, #41927, .T. ) ;
#45064 = CARTESIAN_POINT ( 'NONE',  ( -0.8759842519685039353, -0.1787899950787401882, 1.355807086560409491 ) ) ;
#45065 = CARTESIAN_POINT ( 'NONE',  ( 0.8759842519685039353, -0.1787899950787401882, 1.316437007820252081 ) ) ;
#45066 = CARTESIAN_POINT ( 'NONE',  ( 0.9500414927467378812, -0.1787899950787401604, 0.09842519679663024046 ) ) ;
#45067 = CARTESIAN_POINT ( 'NONE',  ( -1.002407869896990045, 0.1264236179284866091, 1.247539370024976391 ) ) ;
#45068 = CYLINDRICAL_SURFACE ( 'NONE', #25291, 0.2362204724409449064 ) ;
#45069 = CARTESIAN_POINT ( 'NONE',  ( 0.05727803307417802386, -0.09842527607325883554, -0.1693749438220764070 ) ) ;
#45070 = LINE ( 'NONE', #23539, #17034 ) ;
#45071 = CARTESIAN_POINT ( 'NONE',  ( 1.054774247047244096, 0.000000000000000000, 0.4207677164816693294 ) ) ;
#45072 = CARTESIAN_POINT ( 'NONE',  ( -0.8759842519685039353, -0.1787899950787401882, 0.3272637794737956463 ) ) ;
#45073 = CARTESIAN_POINT ( 'NONE',  ( -0.8019270111902717657, 0.1787899950787401604, 0.8612204723871809131 ) ) ;
#45074 = AXIS2_PLACEMENT_3D ( 'NONE', #9228, #17350, #38456 ) ;
#45075 = DIRECTION ( 'NONE',  ( 1.000000000000000000, 0.000000000000000000, -1.822029033848725275E-16 ) ) ;
#45076 = ORIENTED_EDGE ( 'NONE', *, *, #152, .F. ) ;
#45077 = CARTESIAN_POINT ( 'NONE',  ( 0.6971942568897637749, 2.189545951927499583E-17, 0.9128937007336377363 ) ) ;
#45078 = CARTESIAN_POINT ( 'NONE',  ( -1.033464566929133799, 0.000000000000000000, 0.2854330708661417804 ) ) ;
#45079 = CIRCLE ( 'NONE', #42778, 0.09842519685039370636 ) ;
#45080 = CARTESIAN_POINT ( 'NONE',  ( 0.6971942568897648851, -0.07405724077823297447, 1.230314960576158967 ) ) ;
#45081 = CARTESIAN_POINT ( 'NONE',  ( -0.7495606340400177148, 0.1264236179284866091, 1.966043307032850462 ) ) ;
#45082 = ORIENTED_EDGE ( 'NONE', *, *, #19218, .F. ) ;
#45083 = CARTESIAN_POINT ( 'NONE',  ( -7.957671378281915615E-17, 0.1564960629921311464, -0.3937007874015748254 ) ) ;
#45084 = CARTESIAN_POINT ( 'NONE',  ( 1.033464566929133799, 1.928577636452524610E-17, 4.498031496062992574 ) ) ;
#45085 = CARTESIAN_POINT ( 'NONE',  ( 0.07405724077823318263, -1.460753889489081692, 0.1787899950787401604 ) ) ;
#45086 = ORIENTED_EDGE ( 'NONE', *, *, #21480, .T. ) ;
#45087 = CARTESIAN_POINT ( 'NONE',  ( 0.1574803149606299191, 0.1473293504822035527, -0.9532488779249704836 ) ) ;
#45088 = CARTESIAN_POINT ( 'NONE',  ( 0.1787899950787401604, -0.4114173227808823330, -0.07405724077823318263 ) ) ;
#45089 = CARTESIAN_POINT ( 'NONE',  ( -0.7185039370078739607, 0.000000000000000000, -2.869337061179095023E-17 ) ) ;
#45090 = ORIENTED_EDGE ( 'NONE', *, *, #10794, .T. ) ;
#45091 = EDGE_CURVE ( 'NONE', #35775, #37979, #35645, .T. ) ;
#45092 = CARTESIAN_POINT ( 'NONE',  ( 4.268512490100409430E-16, 0.2954942322624074524, -0.2921040715117803055 ) ) ;
#45093 = CARTESIAN_POINT ( 'NONE',  ( -0.1377952755905510751, 0.000000000000000000, -0.02633646578327370619 ) ) ;
#45094 = EDGE_CURVE ( 'NONE', #38209, #13767, #30648, .T. ) ;
#45095 = AXIS2_PLACEMENT_3D ( 'NONE', #38596, #39057, #6226 ) ;
#45096 = CARTESIAN_POINT ( 'NONE',  ( -0.7185039370078739607, 1.928577636452523993E-17, 1.446850393700787274 ) ) ;
#45097 = CARTESIAN_POINT ( 'NONE',  ( 1.002407869896990045, -0.1264236179284866091, 1.552657480261196765 ) ) ;
#45098 = CARTESIAN_POINT ( 'NONE',  ( 0.6971942568897626646, 0.07405724077823318263, 0.1968503936470238913 ) ) ;
#45099 = EDGE_CURVE ( 'NONE', #13693, #12042, #24023, .T. ) ;
#45100 = CARTESIAN_POINT ( 'NONE',  ( -0.1787899950787401604, 0.1386555593298164635, -0.07405724077823318263 ) ) ;
#45101 = CARTESIAN_POINT ( 'NONE',  ( 0.1787899950787401882, 0.1323818898175431191, -2.189545951927503898E-17 ) ) ;
#45102 = CARTESIAN_POINT ( 'NONE',  ( -0.8759842519685039353, 0.1574803149606299191, 1.742125984144440975 ) ) ;
#45103 = EDGE_CURVE ( 'NONE', #46609, #35410, #47241, .T. ) ;
#45104 = VECTOR ( 'NONE', #21831, 39.37007874015748854 ) ;
#45105 = CARTESIAN_POINT ( 'NONE',  ( -1.054774247047244096, 0.000000000000000000, 0.5782480314422993040 ) ) ;
#45107 = ( CONVERSION_BASED_UNIT ( 'INCH', #1029 ) LENGTH_UNIT ( ) NAMED_UNIT ( #31413 ) ) ;
#45106 = CARTESIAN_POINT ( 'NONE',  ( 0.1113553986120547346, -0.6722440944881890035, -0.1113553986120547346 ) ) ;
#45108 = CARTESIAN_POINT ( 'NONE',  ( 0.07444174185955065859, -1.602898140291707074, 0.1797182628040039087 ) ) ;
#45109 = CARTESIAN_POINT ( 'NONE',  ( -0.1574803149606299191, -0.05708661406570126468, 0.000000000000000000 ) ) ;
#45110 = DIRECTION ( 'NONE',  ( 1.822029033848725028E-16, 0.000000000000000000, 1.000000000000000000 ) ) ;
#45111 = CARTESIAN_POINT ( 'NONE',  ( 1.054774247047244540, -0.07405724077823318263, 1.402559055064346971 ) ) ;
#45112 = VECTOR ( 'NONE', #112, 39.37007874015748143 ) ;
#45113 = CARTESIAN_POINT ( 'NONE',  ( 0.6971942568897637749, 2.189545951927499583E-17, 1.852854330654897685 ) ) ;
#45114 = CARTESIAN_POINT ( 'NONE',  ( 1.002407869896990045, 0.1264236179284866091, 0.3026574802611972648 ) ) ;
#45115 = ORIENTED_EDGE ( 'NONE', *, *, #20502, .T. ) ;
#45117 = VERTEX_POINT ( 'NONE', #38979 ) ;
#45116 = DIRECTION ( 'NONE',  ( 1.000000000000000000, -3.469446951953626022E-15, -0.000000000000000000 ) ) ;
#45118 = DIRECTION ( 'NONE',  ( 0.000000000000000000, 0.000000000000000000, 1.000000000000000000 ) ) ;
#45119 = DIRECTION ( 'NONE',  ( 0.000000000000000000, 0.000000000000000000, 1.000000000000000000 ) ) ;
#45120 = CARTESIAN_POINT ( 'NONE',  ( 3.284318927891251994E-17, 0.08316929139234625901, 0.1787899950787401882 ) ) ;
#45121 = CARTESIAN_POINT ( 'NONE',  ( 0.8019270111902717657, 0.1787899950787401604, 0.5068897637257642197 ) ) ;
#45122 = ( BOUNDED_CURVE ( )  B_SPLINE_CURVE ( 2, ( #37043, #14307, #43511, #29677, #32769, #25326, #7565, #18363, #44442 ),
 .UNSPECIFIED., .F., .T. ) 
 B_SPLINE_CURVE_WITH_KNOTS ( ( 3, 2, 2, 2, 3 ),
 ( 0.4099999999999999756, 0.4124999999999999778, 0.4149999999999999800, 0.4174999999999999822, 0.4199999999999999845 ),
 .UNSPECIFIED. ) 
 CURVE ( )  GEOMETRIC_REPRESENTATION_ITEM ( )  RATIONAL_B_SPLINE_CURVE ( ( 1.000000000000000000, 0.9238795325112879597, 1.000000000000000000, 0.9238795325112869605, 1.000000000000000000, 0.9238795325112869605, 1.000000000000000000, 0.9238795325112869605, 1.000000000000000000 ) ) 
 REPRESENTATION_ITEM ( '' )  ) ;
#45123 = CARTESIAN_POINT ( 'NONE',  ( 0.7330905279855389756, -0.08917163514578783923, 0.03937008531791959948 ) ) ;
#45124 = CARTESIAN_POINT ( 'NONE',  ( 1.033464566929133799, 0.000000000000000000, 1.968503936900346529 ) ) ;
#45125 = CARTESIAN_POINT ( 'NONE',  ( -0.9412147342319837628, 0.1574803149606300301, 1.582185039262551607 ) ) ;
#45126 = CARTESIAN_POINT ( 'NONE',  ( 0.9412147342319837628, 0.1574803149606300301, 0.7947834644594014009 ) ) ;
#45127 = ORIENTED_EDGE ( 'NONE', *, *, #4623, .F. ) ;
#45128 = CARTESIAN_POINT ( 'NONE',  ( 0.01230737760510393873, -0.07955613945526318620, 0.1377952755905511861 ) ) ;
#45129 = ORIENTED_EDGE ( 'NONE', *, *, #43656, .F. ) ;
#45130 = CARTESIAN_POINT ( 'NONE',  ( -1.100456976456230270E-17, -0.05024065997674630191, -0.1797182628040039365 ) ) ;
#45131 = CARTESIAN_POINT ( 'NONE',  ( -0.8759842519685039353, 0.1574803149606299191, 0.6003937006798740761 ) ) ;
#45132 = CARTESIAN_POINT ( 'NONE',  ( -1.033464566929133799, 0.000000000000000000, 1.230314960629921295 ) ) ;
#45133 = CARTESIAN_POINT ( 'NONE',  ( 1.002407869896990045, -0.1264236179284866091, 1.631397637741511808 ) ) ;
#45134 = CARTESIAN_POINT ( 'NONE',  ( -0.7185039370078739607, 1.928577636452523993E-17, 1.289370078740157632 ) ) ;
#45135 = CYLINDRICAL_SURFACE ( 'NONE', #28961, 0.4724409448818896462 ) ;
#45137 = CARTESIAN_POINT ( 'NONE',  ( -0.9873396505805591694, -0.1113553986120547346, 0.4379921259842519676 ) ) ;
#45136 = CARTESIAN_POINT ( 'NONE',  ( -1.033464566929133799, 0.000000000000000000, 0.7185039370078739607 ) ) ;
#45138 = CARTESIAN_POINT ( 'NONE',  ( 1.033464566929134687, 0.06523048226347956391, 0.3567913384751500994 ) ) ;
#45139 = CARTESIAN_POINT ( 'NONE',  ( 1.033464566929134687, -0.06523048226347956391, 1.375492125876724980 ) ) ;
#45140 = EDGE_LOOP ( 'NONE', ( #17588, #13394, #24722 ) ) ;
#45141 = ORIENTED_EDGE ( 'NONE', *, *, #16377, .T. ) ;
#45142 = VECTOR ( 'NONE', #41585, 39.37007874015748143 ) ;
#45143 = CARTESIAN_POINT ( 'NONE',  ( 0.000000000000000000, 0.000000000000000000, -0.02633646578327370619 ) ) ;
#45144 = CARTESIAN_POINT ( 'NONE',  ( -0.8019270111902716547, -0.1787899950787401604, 1.584645669237574994 ) ) ;
#45145 = CARTESIAN_POINT ( 'NONE',  ( -0.1113553986120547346, -0.1013779526483785387, -0.1113553986120547346 ) ) ;
#45146 = CARTESIAN_POINT ( 'NONE',  ( -1.002407869896990045, 0.1264236179284866091, 1.213090551127338435 ) ) ;
#45147 = EDGE_CURVE ( 'NONE', #42931, #21023, #5479, .T. ) ;
#45148 = AXIS2_PLACEMENT_3D ( 'NONE', #31336, #9523, #12891 ) ;
#45149 = CARTESIAN_POINT ( 'NONE',  ( 0.8759842519685039353, 0.000000000000000000, 4.498031496062992574 ) ) ;
#45150 = CARTESIAN_POINT ( 'NONE',  ( -0.8019270111902717657, 0.1787899950787401604, 0.2755905511273391006 ) ) ;
#45151 = DIRECTION ( 'NONE',  ( -1.000000000000000000, 0.000000000000000000, 0.000000000000000000 ) ) ;
#45152 = DIRECTION ( 'NONE',  ( -1.000000000000000000, 0.000000000000000000, 0.000000000000000000 ) ) ;
#45153 = CARTESIAN_POINT ( 'NONE',  ( 3.284318927891251994E-17, -0.9907735745284508289, 0.1787899950787401882 ) ) ;
#45154 = VERTEX_POINT ( 'NONE', #35174 ) ;
#45155 = CARTESIAN_POINT ( 'NONE',  ( 0.1787899950787401604, -0.01771653537930737918, -0.07405724077823318263 ) ) ;
#45156 = EDGE_LOOP ( 'NONE', ( #12417, #24654, #35807, #14687 ) ) ;
#45157 = CARTESIAN_POINT ( 'NONE',  ( -0.7185039370078739607, 1.928577636452523993E-17, 1.397637795168062969 ) ) ;
#45158 = CARTESIAN_POINT ( 'NONE',  ( 0.6195511811023612925, 0.6102362204724403050, 0.5854071585544579071 ) ) ;
#45159 = EDGE_CURVE ( 'NONE', #36569, #8914, #25580, .T. ) ;
#45160 = CARTESIAN_POINT ( 'NONE',  ( -0.1787899950787401604, -0.6328740156942683770, 0.07405724077823318263 ) ) ;
#45161 = EDGE_CURVE ( 'NONE', #23021, #4670, #30478, .T. ) ;
#45162 = CARTESIAN_POINT ( 'NONE',  ( -0.8759842519685039353, -0.1787899950787401882, 0.1353346456155279653 ) ) ;
#45163 = CARTESIAN_POINT ( 'NONE',  ( -0.7185039370078746268, -0.06523048226347956391, 0.9374999999999991118 ) ) ;
#45164 = CARTESIAN_POINT ( 'NONE',  ( 0.2698848154395015464, 4.466152701071653354E-17, 0.000000000000000000 ) ) ;
#45165 = CARTESIAN_POINT ( 'NONE',  ( 0.07444174185955065859, -0.9336068017090288773, 0.1797182628040039087 ) ) ;
#45166 = CARTESIAN_POINT ( 'NONE',  ( 1.033464566929133799, 0.000000000000000000, 1.112204724409448842 ) ) ;
#45167 = CARTESIAN_POINT ( 'NONE',  ( 0.9500414927467378812, -0.1787899950787401604, 0.9251968503399374821 ) ) ;
#45168 = CARTESIAN_POINT ( 'NONE',  ( 0.9500414927467377701, 0.1787899950787401604, 1.407480314906865981 ) ) ;
#45169 = VECTOR ( 'NONE', #25877, 39.37007874015748143 ) ;
#45170 = FACE_OUTER_BOUND ( 'NONE', #3353, .T. ) ;
#45171 = CARTESIAN_POINT ( 'NONE',  ( 0.8759842519685039353, -0.1574803149606299191, 1.496062992125984259 ) ) ;
#45173 = CARTESIAN_POINT ( 'NONE',  ( -0.1913749512857115809, -0.1850038654769096402, -0.3090319486758666412 ) ) ;
#45172 = CARTESIAN_POINT ( 'NONE',  ( 0.7199145177299522969, -0.06352406682034270058, 1.984478708794018775 ) ) ;
#45174 = AXIS2_PLACEMENT_3D ( 'NONE', #7559, #44209, #11410 ) ;
#45175 = LINE ( 'NONE', #30851, #28243 ) ;
#45176 = CARTESIAN_POINT ( 'NONE',  ( -0.8759842519685039353, 0.1574803149606299191, 1.624015747923968522 ) ) ;
#45177 = CARTESIAN_POINT ( 'NONE',  ( 0.07405724077823318263, 0.09055118115612578733, 0.1787899950787401604 ) ) ;
#45178 = CARTESIAN_POINT ( 'NONE',  ( 0.8759842519685039353, -0.1787899950787401882, 1.035925196796629866 ) ) ;
#45179 = CARTESIAN_POINT ( 'NONE',  ( 1.054774247047244540, 0.07405724077823318263, 1.879921259788756016 ) ) ;
#45180 = CARTESIAN_POINT ( 'NONE',  ( -0.1787899950787401882, -0.9847440944344251212, 0.000000000000000000 ) ) ;
#45181 = CARTESIAN_POINT ( 'NONE',  ( 0.7185039370078746268, 0.06523048226347956391, 0.4109251967428667052 ) ) ;
#45182 = ORIENTED_EDGE ( 'NONE', *, *, #1123, .T. ) ;
#45183 = CARTESIAN_POINT ( 'NONE',  ( -0.7185039370078739607, 1.928577636452523993E-17, 0.8070866140657008136 ) ) ;
#45184 = CARTESIAN_POINT ( 'NONE',  ( 1.033464566929134687, -0.06523048226347956391, 1.897145669291339543 ) ) ;
#45185 = CARTESIAN_POINT ( 'NONE',  ( -0.06523048226347956391, -1.624507873908221489, 0.1574803149606297803 ) ) ;
#45186 = CARTESIAN_POINT ( 'NONE',  ( -0.8107537697050253289, 0.1574803149606300301, 0.1304133857192446289 ) ) ;
#45187 = LINE ( 'NONE', #37792, #29072 ) ;
#45188 = CARTESIAN_POINT ( 'NONE',  ( 1.002407869896990045, -0.1264236179284866091, 1.119586614119464585 ) ) ;
#45189 = VERTEX_POINT ( 'NONE', #6626 ) ;
#45190 = DIRECTION ( 'NONE',  ( 0.000000000000000000, 6.980778575359379259E-17, -1.000000000000000000 ) ) ;
#45191 = DIRECTION ( 'NONE',  ( 0.000000000000000000, -1.000000000000000000, 0.000000000000000000 ) ) ;
#45192 = CARTESIAN_POINT ( 'NONE',  ( -1.054774247047244540, -0.07405724077823318263, 0.5314960629383620461 ) ) ;
#45193 = CARTESIAN_POINT ( 'NONE',  ( -0.7646288533564489232, -0.1113553986120547346, 0.2706692913385826960 ) ) ;
#45194 = CARTESIAN_POINT ( 'NONE',  ( -0.8019270111902717657, -0.1787899950787401604, 0.2854330708123783422 ) ) ;
#45195 = ORIENTED_EDGE ( 'NONE', *, *, #41432, .T. ) ;
#45197 = CARTESIAN_POINT ( 'NONE',  ( 0.1264236179284866091, -1.516240157426551161, -0.1264236179284866091 ) ) ;
#45196 = CARTESIAN_POINT ( 'NONE',  ( 0.1574803149606299191, -0.3523622046168823352, -1.928577636452523993E-17 ) ) ;
#45198 = CARTESIAN_POINT ( 'NONE',  ( -0.7495606340400177148, 0.1264236179284866091, 1.769192913332062966 ) ) ;
#45199 = CARTESIAN_POINT ( 'NONE',  ( -1.002407869896990045, 0.1264236179284866091, 1.011318897584031484 ) ) ;
#45200 = CARTESIAN_POINT ( 'NONE',  ( -0.6971942568897637749, 2.189545951927499583E-17, 0.5191929133320630774 ) ) ;
#45201 = CARTESIAN_POINT ( 'NONE',  ( -0.7185039370078746268, 0.06523048226347956391, 1.680610236220472009 ) ) ;
#45202 = CARTESIAN_POINT ( 'NONE',  ( 0.07405724077823318263, -0.5158719997253020662, 0.1787899950787401604 ) ) ;
#45203 = CARTESIAN_POINT ( 'NONE',  ( 0.0008909177745428464943, -0.08956047734530078741, -0.1867918148680964563 ) ) ;
#45204 = CARTESIAN_POINT ( 'NONE',  ( -0.1968503937007874127, 0.07021257666614941217, -0.1553045758542781762 ) ) ;
#45205 = DIRECTION ( 'NONE',  ( -0.8660254037844389297, 0.000000000000000000, -0.4999999999999994449 ) ) ;
#45206 = VECTOR ( 'NONE', #42997, 39.37007874015748854 ) ;
#45207 = EDGE_CURVE ( 'NONE', #31651, #46614, #3140, .T. ) ;
#45209 = CARTESIAN_POINT ( 'NONE',  ( -0.7646288533564489232, -0.1113553986120547346, 1.166338582569637961 ) ) ;
#45208 = CIRCLE ( 'NONE', #42164, 0.1003937007874010356 ) ;
#45210 = CARTESIAN_POINT ( 'NONE',  ( -0.8759842519685039353, -0.1787899950787401882, 0.4847440944344252323 ) ) ;
#45211 = CARTESIAN_POINT ( 'NONE',  ( -0.7185039370078739607, 1.928577636452523993E-17, 0.3838582677165354173 ) ) ;
#45212 = EDGE_CURVE ( 'NONE', #44149, #32266, #13824, .T. ) ;
#45213 = AXIS2_PLACEMENT_3D ( 'NONE', #14338, #32075, #28983 ) ;
#45214 = EDGE_CURVE ( 'NONE', #19863, #15025, #33046, .T. ) ;
#45215 = CARTESIAN_POINT ( 'NONE',  ( -0.1787899950787401882, -1.462106299158834721, 0.000000000000000000 ) ) ;
#45216 = CARTESIAN_POINT ( 'NONE',  ( 0.07405724077823318263, -1.602362204670647161, 0.1787899950787401604 ) ) ;
#45217 = CARTESIAN_POINT ( 'NONE',  ( 0.9873396505805591694, -0.1113553986120547346, 0.2017716535433070890 ) ) ;
#45218 = CARTESIAN_POINT ( 'NONE',  ( 0.9412147342319837628, 0.1574803149606300301, 0.9621062992125994917 ) ) ;
#45219 = CARTESIAN_POINT ( 'NONE',  ( 0.9412147342319837628, -0.1574803149606297803, 0.5142716535433068392 ) ) ;
#45220 = CYLINDRICAL_SURFACE ( 'NONE', #46960, 0.4724409448818900348 ) ;
#45221 = CARTESIAN_POINT ( 'NONE',  ( -0.9873396505805591694, -0.1113553986120547346, 1.294291338475149544 ) ) ;
#45222 = CARTESIAN_POINT ( 'NONE',  ( 1.002407869896990045, 0.1264236179284866091, 0.5044291338045039375 ) ) ;
#45223 = CARTESIAN_POINT ( 'NONE',  ( 1.054774247047244540, 0.07405724077823318263, 0.06397637789899228433 ) ) ;
#45225 = CYLINDRICAL_SURFACE ( 'NONE', #41531, 0.1574803149606299191 ) ;
#45224 = CARTESIAN_POINT ( 'NONE',  ( -9.642888182262618425E-18, -0.4311023622047244208, -0.1574803149606299191 ) ) ;
#45226 = CARTESIAN_POINT ( 'NONE',  ( 0.1574803149606299191, -5.122214988120488358E-16, -8.878505979408856939E-16 ) ) ;
#45227 = ORIENTED_EDGE ( 'NONE', *, *, #43590, .T. ) ;
#45228 = CARTESIAN_POINT ( 'NONE',  ( -0.1259245010770292383, -0.09152579912861666389, -0.1269212964996754567 ) ) ;
#45229 = CARTESIAN_POINT ( 'NONE',  ( -0.7495606340400177148, -0.1264236179284866091, 1.075295275536787276 ) ) ;
#45230 = CARTESIAN_POINT ( 'NONE',  ( 0.8759842519685039353, 0.1574803149606299191, 1.082677165354330784 ) ) ;
#45231 = CARTESIAN_POINT ( 'NONE',  ( -0.9251144371765599450, -0.1690582487949516266, 1.989066791630040187 ) ) ;
#45232 = CARTESIAN_POINT ( 'NONE',  ( 0.1574803149606299746, 0.4265678656643324129, 0.4783464566929144235 ) ) ;
#45233 = VECTOR ( 'NONE', #36710, 39.37007874015748854 ) ;
#45235 = CARTESIAN_POINT ( 'NONE',  ( -0.8759842519685039353, 0.000000000000000000, 0.000000000000000000 ) ) ;
#45234 = CARTESIAN_POINT ( 'NONE',  ( 0.7185039370078739607, 1.928577636452523993E-17, 0.5708661416247566844 ) ) ;
#45236 = CARTESIAN_POINT ( 'NONE',  ( 1.033464566929134909, 0.06523048226347841205, 0.5930118109160948947 ) ) ;
#45237 = CARTESIAN_POINT ( 'NONE',  ( -0.1057326532622849119, -0.08956134917853916799, 0.1203865889276477807 ) ) ;
#45238 = CARTESIAN_POINT ( 'NONE',  ( -0.07405724077823318263, -0.4803149605761579677, -0.1787899950787401604 ) ) ;
#45239 = ORIENTED_EDGE ( 'NONE', *, *, #3841, .F. ) ;
#45240 = AXIS2_PLACEMENT_3D ( 'NONE', #31348, #9533, #38761 ) ;
#45242 = CARTESIAN_POINT ( 'NONE',  ( -0.1377952755905511861, -1.331775896911328393E-15, 0.9074803149606294195 ) ) ;
#45241 = CIRCLE ( 'NONE', #38386, 0.3937007874015747699 ) ;
#45243 = CARTESIAN_POINT ( 'NONE',  ( -0.9412147342319837628, 0.1574803149606300301, 1.119586614173229577 ) ) ;
#45244 = ORIENTED_EDGE ( 'NONE', *, *, #17416, .T. ) ;
#45245 = DIRECTION ( 'NONE',  ( 0.000000000000000000, 0.000000000000000000, 1.000000000000000000 ) ) ;
#45246 = DIRECTION ( 'NONE',  ( 0.000000000000000000, 1.000000000000000000, 0.000000000000000000 ) ) ;
#45247 = CARTESIAN_POINT ( 'NONE',  ( -0.1787899950787401604, -1.769685039316315267, 0.07405724077823318263 ) ) ;
#45248 = CARTESIAN_POINT ( 'NONE',  ( -0.1787899950787401882, -0.9109251967966299768, 0.000000000000000000 ) ) ;
#45249 = VECTOR ( 'NONE', #35366, 39.37007874015748143 ) ;
#45250 = CARTESIAN_POINT ( 'NONE',  ( -0.1574803149606299191, -1.326771653543307172, 0.000000000000000000 ) ) ;
#45251 = CARTESIAN_POINT ( 'NONE',  ( 0.7185039370078746268, 0.06523048226347956391, 1.119586614065702035 ) ) ;
#45252 = DIRECTION ( 'NONE',  ( 0.000000000000000000, -0.000000000000000000, 1.000000000000000000 ) ) ;
#45253 = EDGE_LOOP ( 'NONE', ( #42506, #37980, #39645, #4598, #30254 ) ) ;
#45254 = ORIENTED_EDGE ( 'NONE', *, *, #1719, .F. ) ;
#45255 = CARTESIAN_POINT ( 'NONE',  ( -0.9500414927467378812, 0.1787899950787401604, 1.727362204670645385 ) ) ;
#45256 = CARTESIAN_POINT ( 'NONE',  ( 0.6971942568897648851, 0.07405724077823318263, 1.815944881835999558 ) ) ;
#45257 = ORIENTED_EDGE ( 'NONE', *, *, #11110, .F. ) ;
#45258 = DIRECTION ( 'NONE',  ( -1.000000000000000000, 0.000000000000000000, 0.000000000000000000 ) ) ;
#45259 = CARTESIAN_POINT ( 'NONE',  ( 0.8759842519685039353, 0.1787899950787401882, 0.4699803149068661479 ) ) ;
#45260 = CARTESIAN_POINT ( 'NONE',  ( -0.8019270111902717657, -0.1787899950787401604, 1.427165354276944687 ) ) ;
#45261 = DIRECTION ( 'NONE',  ( -1.000000000000000000, 0.000000000000000000, 7.049916206369740876E-15 ) ) ;
#45262 = CARTESIAN_POINT ( 'NONE',  ( -0.6971942568897648851, -0.07405724077823297447, 1.343503936954111966 ) ) ;
#45263 = CARTESIAN_POINT ( 'NONE',  ( -0.7495606340400177148, -0.1264236179284866091, 0.7947834645131652831 ) ) ;
#45264 = CARTESIAN_POINT ( 'NONE',  ( -0.6971942568897626646, -0.07405724077823297447, 0.08858267711159097113 ) ) ;
#45265 = CARTESIAN_POINT ( 'NONE',  ( -0.1984097999861051398, 0.07306521771079745042, -0.1708811194343041739 ) ) ;
#45266 = CARTESIAN_POINT ( 'NONE',  ( -0.9500414927467378812, 0.1787899950787401604, 1.727362204670645385 ) ) ;
#45267 = CARTESIAN_POINT ( 'NONE',  ( -0.7185039370078746268, 0.06523048226347956391, 1.985728346349167950 ) ) ;
#45268 = CARTESIAN_POINT ( 'NONE',  ( -0.7185039370078746268, -0.06523048226347956391, 1.685531496062990797 ) ) ;
#45269 = CYLINDRICAL_SURFACE ( 'NONE', #41917, 0.1574803149606299191 ) ;
#45270 = ADVANCED_FACE ( 'NONE', ( #24612 ), #13142, .T. ) ;
#45271 = CARTESIAN_POINT ( 'NONE',  ( 0.7495606340400177148, 0.1264236179284866091, 1.616633858213952779 ) ) ;
#45272 = CARTESIAN_POINT ( 'NONE',  ( -0.2112569658035661491, -0.09842519685039370636, -0.1284583705656232311 ) ) ;
#45273 = LINE ( 'NONE', #41429, #16466 ) ;
#45274 = ( BOUNDED_CURVE ( )  B_SPLINE_CURVE ( 2, ( #41207, #23041, #23287, #37659, #45301, #5291, #23527, #37900, #34317 ),
 .UNSPECIFIED., .F., .T. ) 
 B_SPLINE_CURVE_WITH_KNOTS ( ( 3, 2, 2, 2, 3 ),
 ( 0.05000000000000000278, 0.05249999999999999806, 0.05500000000000000028, 0.05750000000000000250, 0.05999999999999999778 ),
 .UNSPECIFIED. ) 
 CURVE ( )  GEOMETRIC_REPRESENTATION_ITEM ( )  RATIONAL_B_SPLINE_CURVE ( ( 1.000000000000000000, 0.9238795325112859613, 1.000000000000000000, 0.9238795325112869605, 1.000000000000000000, 0.9238795325112869605, 1.000000000000000000, 0.9238795325112869605, 1.000000000000000000 ) ) 
 REPRESENTATION_ITEM ( '' )  ) ;
#45275 = AXIS2_PLACEMENT_3D ( 'NONE', #3292, #18155, #6646 ) ;
#45276 = EDGE_CURVE ( 'NONE', #6613, #39, #32302, .T. ) ;
#45277 = ORIENTED_EDGE ( 'NONE', *, *, #9307, .F. ) ;
#45278 = ORIENTED_EDGE ( 'NONE', *, *, #25337, .F. ) ;
#45279 = AXIS2_PLACEMENT_3D ( 'NONE', #14005, #21672, #21907 ) ;
#45280 = AXIS2_PLACEMENT_3D ( 'NONE', #38190, #34856, #41512 ) ;
#45281 = EDGE_CURVE ( 'NONE', #4590, #11117, #2785, .T. ) ;
#45282 = CARTESIAN_POINT ( 'NONE',  ( 0.07405724077823318263, -1.056102362150961982, 0.1787899950787401604 ) ) ;
#45283 = CARTESIAN_POINT ( 'NONE',  ( -0.1787899950787401604, -1.061023621993481214, 0.07405724077823318263 ) ) ;
#45284 = EDGE_CURVE ( 'NONE', #22900, #110, #17411, .T. ) ;
#45285 = PRODUCT_RELATED_PRODUCT_CATEGORY ( 'part', '', ( #44040 ) ) ;
#45286 = DIRECTION ( 'NONE',  ( 0.000000000000000000, 0.000000000000000000, 1.000000000000000000 ) ) ;
#45287 = CARTESIAN_POINT ( 'NONE',  ( 0.8759842519685039353, -0.1787899950787401882, 1.823326771599779406 ) ) ;
#45288 = CARTESIAN_POINT ( 'NONE',  ( -1.100456976456230270E-17, -0.4045713686381637308, -0.1797182628040039365 ) ) ;
#45289 = CARTESIAN_POINT ( 'NONE',  ( -0.8107537697050253289, 0.1574803149606300301, 0.7997047243019228535 ) ) ;
#45290 = CARTESIAN_POINT ( 'NONE',  ( 0.1574803149606300301, 0.03395669291338582890, -0.06523048226347956391 ) ) ;
#45291 = LINE ( 'NONE', #27132, #5446 ) ;
#45292 = CARTESIAN_POINT ( 'NONE',  ( 0.8759842519685039353, 0.1787899950787401882, 0.9374999999462362288 ) ) ;
#45293 = ( BOUNDED_CURVE ( )  B_SPLINE_CURVE ( 2, ( #11641, #12355, #578, #5129, #8259, #41061, #30122, #4178, #29881 ),
 .UNSPECIFIED., .F., .F. ) 
 B_SPLINE_CURVE_WITH_KNOTS ( ( 3, 2, 2, 2, 3 ),
 ( 0.9499999999999999556, 0.9525000000000000133, 0.9549999999999999600, 0.9575000000000000178, 0.9599999999999999645 ),
 .UNSPECIFIED. ) 
 CURVE ( )  GEOMETRIC_REPRESENTATION_ITEM ( )  RATIONAL_B_SPLINE_CURVE ( ( 1.000000000000000000, 0.9238795325112939549, 1.000000000000000000, 0.9238795325112869605, 1.000000000000000000, 0.9238795325112869605, 1.000000000000000000, 0.9238795325112869605, 1.000000000000000000 ) ) 
 REPRESENTATION_ITEM ( '' )  ) ;
#45295 = CARTESIAN_POINT ( 'NONE',  ( 0.1571288672381034868, -0.02360035419889824210, 0.1403980133540951303 ) ) ;
#45294 = CARTESIAN_POINT ( 'NONE',  ( -1.002407869896990045, -0.1264236179284866091, 1.990649606245448844 ) ) ;
#45296 = CARTESIAN_POINT ( 'NONE',  ( 0.8759842519685039353, -0.1787899950787401882, 1.906988188922614125 ) ) ;
#45297 = ( GEOMETRIC_REPRESENTATION_CONTEXT ( 3 ) GLOBAL_UNCERTAINTY_ASSIGNED_CONTEXT ( ( #33040 ) ) GLOBAL_UNIT_ASSIGNED_CONTEXT ( ( #21619, #22084, #25213 ) ) REPRESENTATION_CONTEXT ( 'NONE', 'WORKASPACE' ) ) ;
#45298 = CARTESIAN_POINT ( 'NONE',  ( 0.7646288533564489232, 0.1113553986120547346, 0.1820866141732283561 ) ) ;
#45299 = CARTESIAN_POINT ( 'NONE',  ( 0.7185039370078739607, 0.000000000000000000, 4.498031496062992574 ) ) ;
#45300 = CARTESIAN_POINT ( 'NONE',  ( -1.094772975963752103E-17, -0.3695866141194649179, -0.1787899950787401882 ) ) ;
#45301 = CARTESIAN_POINT ( 'NONE',  ( 0.8759842519685039353, -0.1574803149606299191, 0.1181102362204724532 ) ) ;
#45302 = CARTESIAN_POINT ( 'NONE',  ( 0.07405724077823318263, -1.248031496009228913, 0.1787899950787401604 ) ) ;
#45303 = AXIS2_PLACEMENT_3D ( 'NONE', #34967, #1636, #2111 ) ;
#45304 = CARTESIAN_POINT ( 'NONE',  ( -1.054774247047244096, 0.000000000000000000, 1.754429133804503715 ) ) ;
#45305 = ORIENTED_EDGE ( 'NONE', *, *, #3131, .T. ) ;
#45306 = CARTESIAN_POINT ( 'NONE',  ( -0.8019270111902717657, -0.1787899950787401604, 1.274606299158834277 ) ) ;
#45307 = DIRECTION ( 'NONE',  ( 0.000000000000000000, 0.9699617890481115889, 0.2432573283306930789 ) ) ;
#45308 = CARTESIAN_POINT ( 'NONE',  ( -0.6971942568897626646, -0.07405724077823297447, 0.5610236219934807700 ) ) ;
#45309 = CIRCLE ( 'NONE', #24673, 0.1864803149606299448 ) ;
#45310 = AXIS2_PLACEMENT_3D ( 'NONE', #26425, #40992, #10869 ) ;
#45311 = CARTESIAN_POINT ( 'NONE',  ( -1.054774247047244096, 0.000000000000000000, 1.203248031442299304 ) ) ;
#45312 = EDGE_CURVE ( 'NONE', #5631, #31435, #6980, .T. ) ;
#45313 = DIRECTION ( 'NONE',  ( 1.822029033848725028E-16, 0.000000000000000000, 1.000000000000000000 ) ) ;
#45314 = CARTESIAN_POINT ( 'NONE',  ( -0.07153359775988563096, -0.09842519684882801434, -0.1638561172960870671 ) ) ;
#45315 = DIRECTION ( 'NONE',  ( 1.000000000000000000, -0.000000000000000000, -0.000000000000000000 ) ) ;
#45316 = CARTESIAN_POINT ( 'NONE',  ( 1.054774247047244540, -0.07405724077823318263, 0.5757874015210393548 ) ) ;
#45317 = CARTESIAN_POINT ( 'NONE',  ( -0.9500414927467377701, -0.1787899950787401604, 0.4478346456155276045 ) ) ;
#45318 = ORIENTED_EDGE ( 'NONE', *, *, #7797, .F. ) ;
#45319 = LINE ( 'NONE', #9151, #5330 ) ;
#45320 = EDGE_CURVE ( 'NONE', #19846, #41516, #42037, .T. ) ;
#45321 = ORIENTED_EDGE ( 'NONE', *, *, #5759, .T. ) ;
#45322 = CARTESIAN_POINT ( 'NONE',  ( -1.033464566929134687, -0.06523048226347956391, 0.2436023622047244763 ) ) ;
#45323 = ADVANCED_FACE ( 'NONE', ( #17891 ), #15029, .T. ) ;
#45324 = CARTESIAN_POINT ( 'NONE',  ( 1.002407869896990045, 0.1264236179284866091, 1.134350393647023614 ) ) ;
#45325 = CARTESIAN_POINT ( 'NONE',  ( 0.8759842519685039353, 0.1574803149606299191, 1.309055118002708573 ) ) ;
#45326 = ORIENTED_EDGE ( 'NONE', *, *, #26152, .F. ) ;
#45327 = CARTESIAN_POINT ( 'NONE',  ( -1.002407869896990045, 0.1264236179284866091, 0.9374999999462362288 ) ) ;
#45328 = DIRECTION ( 'NONE',  ( 0.000000000000000000, -1.000000000000000000, 0.000000000000000000 ) ) ;
#45329 = CARTESIAN_POINT ( 'NONE',  ( -0.9873396505805591694, -0.1113553986120547346, 0.2017716535433070890 ) ) ;
#45330 = CARTESIAN_POINT ( 'NONE',  ( -0.1787899950787401604, -1.588706645394593719, 0.07405724077823318263 ) ) ;
#45331 = ORIENTED_EDGE ( 'NONE', *, *, #39963, .F. ) ;
#45332 = LINE ( 'NONE', #20173, #44910 ) ;
#45333 = CARTESIAN_POINT ( 'NONE',  ( -0.1787899950787401604, -0.3572834645131658382, -0.07405724077823318263 ) ) ;
#45334 = CARTESIAN_POINT ( 'NONE',  ( -0.2610081115717080569, -0.1673295453843250680, 0.8813693982766842572 ) ) ;
#45335 = ORIENTED_EDGE ( 'NONE', *, *, #4967, .T. ) ;
#45336 = PRODUCT_DEFINITION ( 'UNKNOWN', '', #35466, #44144 ) ;
#45337 = CARTESIAN_POINT ( 'NONE',  ( 0.000000000000000000, -0.09842519685039370636, 0.1574803149606299191 ) ) ;
#45338 = CARTESIAN_POINT ( 'NONE',  ( -0.8759842519685039353, 0.000000000000000000, 0.000000000000000000 ) ) ;
#45339 = CARTESIAN_POINT ( 'NONE',  ( 3.284318927891251994E-17, -0.2317913385289138151, 0.1787899950787401882 ) ) ;
#45340 = AXIS2_PLACEMENT_3D ( 'NONE', #7023, #36281, #3432 ) ;
#45341 = CARTESIAN_POINT ( 'NONE',  ( 0.8070866141732283561, 0.000000000000000000, -0.7574803149606299524 ) ) ;
#45342 = CARTESIAN_POINT ( 'NONE',  ( 0.7495606340400177148, -0.1264236179284866091, 1.582185039316315045 ) ) ;
#45343 = CARTESIAN_POINT ( 'NONE',  ( 0.1264236179284866091, -1.791830708607653699, -0.1264236179284866091 ) ) ;
#45344 = CARTESIAN_POINT ( 'NONE',  ( -0.1264236179284866091, -1.777066929080094670, -0.1264236179284866091 ) ) ;
#45345 = ITEM_DEFINED_TRANSFORMATION ( 'NONE', 'NONE', #31647,  #20860 ) ;
#45346 = CARTESIAN_POINT ( 'NONE',  ( 0.1457398918270421118, -0.09842519685039370636, 0.09125884461778420442 ) ) ;
#45347 = CARTESIAN_POINT ( 'NONE',  ( 1.054774247047244096, 0.000000000000000000, 0.5339566928596221063 ) ) ;
#45348 = CARTESIAN_POINT ( 'NONE',  ( -0.6971942568897637749, 2.189545951927499583E-17, 0.6373031495525354195 ) ) ;
#45350 = CARTESIAN_POINT ( 'NONE',  ( -1.033464566929133799, 1.928577636452524610E-17, 2.869337061179095023E-17 ) ) ;
#45349 = CARTESIAN_POINT ( 'NONE',  ( -0.1574803149606299191, -0.7755905511811023167, 0.000000000000000000 ) ) ;
#45351 = CARTESIAN_POINT ( 'NONE',  ( 0.07444174185955046430, -1.509394203283832780, -0.1797182628040039087 ) ) ;
#45352 = CARTESIAN_POINT ( 'NONE',  ( 0.000000000000000000, -0.09842519685039370636, 0.000000000000000000 ) ) ;
#45353 = COLOUR_RGB ( '', 0.09019608, 0.27058824, 0.51372549) ;
#45354 = CARTESIAN_POINT ( 'NONE',  ( 0.2471922904502826257, 0.08140987345727848656, -0.07064030526713212244 ) ) ;
#45355 = CARTESIAN_POINT ( 'NONE',  ( 0.9500414927467378812, 0.1787899950787401604, 1.530511810969859443 ) ) ;
#45356 = CARTESIAN_POINT ( 'NONE',  ( 0.6971942568897648851, -0.07405724077823297447, 1.815944881835999780 ) ) ;
#45358 = EDGE_LOOP ( 'NONE', ( #12853, #8983, #25742, #16296, #46937 ) ) ;
#45357 = CYLINDRICAL_SURFACE ( 'NONE', #11516, 0.1574803149606299191 ) ;
#45359 = LINE ( 'NONE', #27907, #28171 ) ;
#45360 = CARTESIAN_POINT ( 'NONE',  ( 0.8759842519685039353, 0.000000000000000000, 4.498031496062992574 ) ) ;
#45362 = CARTESIAN_POINT ( 'NONE',  ( -0.1787899950787401882, 0.07332677170730689253, 0.000000000000000000 ) ) ;
#45361 = CARTESIAN_POINT ( 'NONE',  ( 0.06523048226347956391, -0.8715551180027079070, 0.1574803149606297803 ) ) ;
#45363 = CARTESIAN_POINT ( 'NONE',  ( -1.033464566929134687, 0.06523048226347956391, 0.1697834645669291653 ) ) ;
#45364 = CARTESIAN_POINT ( 'NONE',  ( 0.9500414927467378812, 0.1787899950787401604, 0.4232283464029293896 ) ) ;
#45365 = CARTESIAN_POINT ( 'NONE',  ( 0.8215752181199765802, -0.1517888380884206134, 0.03937426606394420214 ) ) ;
#45366 = CARTESIAN_POINT ( 'NONE',  ( 0.7185039370078778465, -0.06523048226348396317, 1.951279527451527329 ) ) ;
#45367 = DIRECTION ( 'NONE',  ( 1.000000000000000000, 0.000000000000000000, 0.000000000000000000 ) ) ;
#45368 = CARTESIAN_POINT ( 'NONE',  ( -1.054774247047244540, -0.07405724077823318263, 1.358267716481669662 ) ) ;
#45369 = CARTESIAN_POINT ( 'NONE',  ( 1.033464566929133799, 0.000000000000000000, 0.8267716534357796299 ) ) ;
#45370 = EDGE_LOOP ( 'NONE', ( #28782, #24656, #16691, #18051 ) ) ;
#45371 = CARTESIAN_POINT ( 'NONE',  ( -0.9500414927467378812, -0.1787899950787401604, 1.082677165300567346 ) ) ;
#45372 = DIRECTION ( 'NONE',  ( 1.822029033848725028E-16, 0.000000000000000000, 1.000000000000000000 ) ) ;
#45373 = CARTESIAN_POINT ( 'NONE',  ( 1.002407869896990045, 0.1264236179284866091, 1.055610236166708793 ) ) ;
#45374 = ORIENTED_EDGE ( 'NONE', *, *, #13144, .F. ) ;
#45375 = CARTESIAN_POINT ( 'NONE',  ( -0.1787899950787401604, -1.385826771599779184, -0.07405724077823318263 ) ) ;
#45376 = CARTESIAN_POINT ( 'NONE',  ( -1.033464566929134687, -0.06523048226347956391, 0.5487204723334181411 ) ) ;
#45377 = CARTESIAN_POINT ( 'NONE',  ( -0.7646288533564489232, -0.1113553986120547346, 1.215551181102362266 ) ) ;
#45378 = CARTESIAN_POINT ( 'NONE',  ( 0.7495606340400177148, 0.1264236179284866091, 1.729822834591905556 ) ) ;
#45379 = CARTESIAN_POINT ( 'NONE',  ( -0.9873396505805591694, 0.1113553986120547346, 1.313976377952756014 ) ) ;
#45380 = ADVANCED_FACE ( 'NONE', ( #7572 ), #18592, .T. ) ;
#45381 = CARTESIAN_POINT ( 'NONE',  ( 1.033464566929134687, 0.06523048226347956391, 0.5634842519685042683 ) ) ;
#45382 = CARTESIAN_POINT ( 'NONE',  ( 0.5555748031496083872, 0.1864803149606324151, 0.01858545845903139190 ) ) ;
#45383 = CARTESIAN_POINT ( 'NONE',  ( 1.054774247047244540, -0.07405724077823318263, 0.06397637789899228433 ) ) ;
#45384 = CARTESIAN_POINT ( 'NONE',  ( 0.7185039370078746268, -0.06523048226347956391, 1.439468503829481216 ) ) ;
#45385 = EDGE_LOOP ( 'NONE', ( #8306, #8838, #12105, #27363 ) ) ;
#45386 = EDGE_CURVE ( 'NONE', #28305, #17869, #32296, .T. ) ;
#45387 = VECTOR ( 'NONE', #36308, 39.37007874015748854 ) ;
#45388 = VERTEX_POINT ( 'NONE', #21731 ) ;
#45389 = EDGE_CURVE ( 'NONE', #33534, #16814, #23067, .T. ) ;
#45390 = CARTESIAN_POINT ( 'NONE',  ( -1.002407869896990045, -0.1264236179284866091, 1.513287401521039355 ) ) ;
#45391 = CARTESIAN_POINT ( 'NONE',  ( -9.642888182262618425E-18, -0.06692913375074074911, -0.1574803149606299191 ) ) ;
#45392 = CARTESIAN_POINT ( 'NONE',  ( -0.9500414927467378812, -0.1787899950787401604, 1.476377952702141449 ) ) ;
#45393 = ORIENTED_EDGE ( 'NONE', *, *, #13885, .T. ) ;
#45394 = AXIS2_PLACEMENT_3D ( 'NONE', #11234, #15292, #15541 ) ;
#45395 = ADVANCED_FACE ( 'NONE', ( #28955 ), #18825, .T. ) ;
#45396 = CLOSED_SHELL ( 'NONE', ( #653, #848, #25626, #28767, #25668, #3794, #39923, #15276, #14506, #3313, #38143, #6696, #45526, #8122 ) ) ;
#45397 = FACE_OUTER_BOUND ( 'NONE', #10211, .T. ) ;
#45398 = LINE ( 'NONE', #22897, #32108 ) ;
#45399 = CARTESIAN_POINT ( 'NONE',  ( -0.1787899950787401604, -1.003076724134751130, -0.07405724077823318263 ) ) ;
#45400 = ORIENTED_EDGE ( 'NONE', *, *, #23850, .T. ) ;
#45401 = CARTESIAN_POINT ( 'NONE',  ( -0.1787899950787401604, 0.001968503990771383692, 0.07405724077823318263 ) ) ;
#45402 = EDGE_LOOP ( 'NONE', ( #44702, #30018, #37862, #38950 ) ) ;
#45403 = ORIENTED_EDGE ( 'NONE', *, *, #46580, .F. ) ;
#45404 = CARTESIAN_POINT ( 'NONE',  ( -0.7185039370078746268, -0.06523048226347956391, 1.203248031388535200 ) ) ;
#45405 = CARTESIAN_POINT ( 'NONE',  ( 0.000000000000000000, 0.000000000000000000, 0.000000000000000000 ) ) ;
#45406 = CARTESIAN_POINT ( 'NONE',  ( 0.8107537697050253289, -0.1574803149606297803, 1.769192913385826404 ) ) ;
#45407 = CARTESIAN_POINT ( 'NONE',  ( 0.1787899950787401604, -0.6131889763241887836, -0.07405724077823318263 ) ) ;
#45408 = SHAPE_REPRESENTATION ( 'Threaded Bushing', ( #20860 ), #22411 ) ;
#45409 = CARTESIAN_POINT ( 'NONE',  ( -1.054774247047244540, 0.07405724077823318263, 0.1870078739619845110 ) ) ;
#45410 = CARTESIAN_POINT ( 'NONE',  ( -1.033464566929134687, -0.06523048226347956391, 1.031003937007875182 ) ) ;
#45411 = CARTESIAN_POINT ( 'NONE',  ( -0.1270800023317771588, -1.108311526118478385, -0.1270800023317771588 ) ) ;
#45412 = CARTESIAN_POINT ( 'NONE',  ( 0.1732685356795573284, 0.1299212598425196763, -0.01414958902434325198 ) ) ;
#45413 = CARTESIAN_POINT ( 'NONE',  ( 0.6971942568897637749, 2.189545951927499583E-17, 1.031003936954110189 ) ) ;
#45414 = FACE_OUTER_BOUND ( 'NONE', #29899, .T. ) ;
#45415 = CARTESIAN_POINT ( 'NONE',  ( 0.8107537697050253289, 0.1574803149606300301, 1.518208661417322469 ) ) ;
#45417 = DIRECTION ( 'NONE',  ( 0.000000000000000000, 0.000000000000000000, -1.000000000000000000 ) ) ;
#45416 = CARTESIAN_POINT ( 'NONE',  ( 0.9873396505805591694, -0.1113553986120547346, 1.422244094488188892 ) ) ;
#45418 = LINE ( 'NONE', #47444, #3897 ) ;
#45419 = CARTESIAN_POINT ( 'NONE',  ( 1.054774247047244096, 0.000000000000000000, 1.006397637741511808 ) ) ;
#45420 = CARTESIAN_POINT ( 'NONE',  ( 0.8759842519685039353, 0.1787899950787401882, 1.887303149552535420 ) ) ;
#45421 = CARTESIAN_POINT ( 'NONE',  ( 0.8107537697050234415, -0.1574803149606297803, 0.3420275589475912925 ) ) ;
#45422 = EDGE_LOOP ( 'NONE', ( #24122, #8851, #19353, #12334 ) ) ;
#45423 = CARTESIAN_POINT ( 'NONE',  ( 0.8759842519685039353, -0.1574803149606299191, 1.249999999892472236 ) ) ;
#45424 = DIRECTION ( 'NONE',  ( -0.5735764363510518216, 0.8191520442889876907, 1.003171929053519693E-16 ) ) ;
#45425 = CARTESIAN_POINT ( 'NONE',  ( 0.1574803149606300301, -1.727854330601133581, -0.06523048226347956391 ) ) ;
#45426 = CARTESIAN_POINT ( 'NONE',  ( -0.7646288533564489232, 0.1113553986120547346, 0.2509842518609771700 ) ) ;
#45427 = CARTESIAN_POINT ( 'NONE',  ( 1.002407869896990045, 0.1264236179284866091, 1.326279527505291433 ) ) ;
#45428 = CARTESIAN_POINT ( 'NONE',  ( 1.033464566929133799, 0.000000000000000000, 1.417322834538141674 ) ) ;
#45429 = CARTESIAN_POINT ( 'NONE',  ( 0.1113553986120547346, -1.774606299212598381, -0.1113553986120547346 ) ) ;
#45430 = DIRECTION ( 'NONE',  ( 1.822029033848725028E-16, 0.000000000000000000, 1.000000000000000000 ) ) ;
#45431 = EDGE_CURVE ( 'NONE', #35669, #1467, #6857, .T. ) ;
#45432 = CARTESIAN_POINT ( 'NONE',  ( -1.002407869896990045, 0.1264236179284866091, 0.6176181101824566033 ) ) ;
#45433 = CARTESIAN_POINT ( 'NONE',  ( -0.1574803149606299191, 0.2512968553230417457, -0.3092734567177703453 ) ) ;
#45434 = LINE ( 'NONE', #27516, #39869 ) ;
#45435 = ORIENTED_EDGE ( 'NONE', *, *, #26379, .T. ) ;
#45436 = CARTESIAN_POINT ( 'NONE',  ( -0.1264236179284866091, -1.535925196796629866, 0.1264236179284866091 ) ) ;
#45437 = VERTEX_POINT ( 'NONE', #47121 ) ;
#45438 = EDGE_CURVE ( 'NONE', #6624, #5180, #7107, .T. ) ;
#45439 = CARTESIAN_POINT ( 'NONE',  ( -0.9500414927467378812, -0.1787899950787401604, 0.5314960629383620461 ) ) ;
#45440 = ORIENTED_EDGE ( 'NONE', *, *, #23441, .F. ) ;
#45441 = CARTESIAN_POINT ( 'NONE',  ( 0.06523048226347956391, -0.04478346445940203924, 0.1574803149606297803 ) ) ;
#45442 = FACE_OUTER_BOUND ( 'NONE', #25608, .T. ) ;
#45443 = CARTESIAN_POINT ( 'NONE',  ( 0.1264236179284866091, -0.5823090075993173631, -0.1264236179284866091 ) ) ;
#45444 = CARTESIAN_POINT ( 'NONE',  ( 0.06147065055149940338, -0.08956076283990217768, -0.1800941195595248401 ) ) ;
#45445 = CARTESIAN_POINT ( 'NONE',  ( 0.8759842519685039353, -0.1574803149606299191, 0.4724409448818898127 ) ) ;
#45446 = AXIS2_PLACEMENT_3D ( 'NONE', #39928, #14320, #25344 ) ;
#45447 = CARTESIAN_POINT ( 'NONE',  ( 0.2559055118110236116, 0.1477471161312027548, -0.3149606299212598381 ) ) ;
#45448 = CARTESIAN_POINT ( 'NONE',  ( -0.7495606340400177148, -0.1264236179284866091, 0.4798228345919055560 ) ) ;
#45449 = DIRECTION ( 'NONE',  ( 1.822029033848725028E-16, 0.000000000000000000, 1.000000000000000000 ) ) ;
#45450 = ORIENTED_EDGE ( 'NONE', *, *, #753, .T. ) ;
#45451 = CARTESIAN_POINT ( 'NONE',  ( -0.3100393700787401619, 3.218313930830148909E-16, -1.043307086614172707 ) ) ;
#45452 = CARTESIAN_POINT ( 'NONE',  ( -0.07405724077823318263, -1.430118110182456714, -0.1787899950787401604 ) ) ;
#45453 = CARTESIAN_POINT ( 'NONE',  ( 0.4151545546392377273, -3.032960542342102697E-32, 0.09842519685039370636 ) ) ;
#45454 = CARTESIAN_POINT ( 'NONE',  ( 0.9412147342319837628, 0.1574803149606300301, 1.031003936900347639 ) ) ;
#45455 = CARTESIAN_POINT ( 'NONE',  ( 0.1636082376614000078, -0.08043368169713546734, 0.1393148943341546153 ) ) ;
#45456 = CARTESIAN_POINT ( 'NONE',  ( 0.07444174185955065859, -0.6973863292680846371, 0.1797182628040039087 ) ) ;
#45457 = CARTESIAN_POINT ( 'NONE',  ( 0.8759842519685039353, -0.1574803149606299191, 0.9448818897637796255 ) ) ;
#45458 = CARTESIAN_POINT ( 'NONE',  ( -0.8107537697050253289, -0.1574803149606297803, 1.286909448711370585 ) ) ;
#45459 = CARTESIAN_POINT ( 'NONE',  ( 0.6971942568897637749, 2.189545951927499583E-17, 0.5979330708123780092 ) ) ;
#45460 = CARTESIAN_POINT ( 'NONE',  ( 0.8019270111902716547, -0.1787899950787401604, 0.04921259837143338728 ) ) ;
#45462 = FACE_OUTER_BOUND ( 'NONE', #1795, .T. ) ;
#45461 = CARTESIAN_POINT ( 'NONE',  ( -0.06523048226347956391, -0.4138779527559053317, 0.1574803149606297803 ) ) ;
#45463 = DIRECTION ( 'NONE',  ( 0.000000000000000000, -0.6156614753256597350, -0.7880107536067206819 ) ) ;
#45464 = EDGE_LOOP ( 'NONE', ( #1655, #46987 ) ) ;
#45465 = CARTESIAN_POINT ( 'NONE',  ( 0.7185039370078739607, 1.928577636452523993E-17, 1.594488188868850242 ) ) ;
#45466 = CARTESIAN_POINT ( 'NONE',  ( -0.8019270111902716547, 0.1787899950787401604, 1.141732283410804349 ) ) ;
#45467 = CARTESIAN_POINT ( 'NONE',  ( 0.7185039370078739607, 1.928577636452523993E-17, 1.053149606299212504 ) ) ;
#45468 = CARTESIAN_POINT ( 'NONE',  ( -0.9653136480190166457, -0.1535042515562757837, 1.989856082496901601 ) ) ;
#45469 = DIRECTION ( 'NONE',  ( 1.000000000000000000, 0.000000000000000000, 0.000000000000000000 ) ) ;
#45471 = CARTESIAN_POINT ( 'NONE',  ( -0.7185039370078739607, 1.928577636452523993E-17, 1.948818897530267602 ) ) ;
#45470 = DIRECTION ( 'NONE',  ( 5.392424630175478286E-15, -0.2432573283306889156, 0.9699617890481125881 ) ) ;
#45472 = CARTESIAN_POINT ( 'NONE',  ( 0.000000000000000000, -0.1193342091828950846, -0.06889763779527559306 ) ) ;
#45474 = CIRCLE ( 'NONE', #14894, 0.2471922904502826812 ) ;
#45473 = CARTESIAN_POINT ( 'NONE',  ( 0.1264236179284866091, -0.5664370078202519698, -0.1264236179284866091 ) ) ;
#45475 = ORIENTED_EDGE ( 'NONE', *, *, #28240, .T. ) ;
#45476 = AXIS2_PLACEMENT_3D ( 'NONE', #44850, #18984, #5080 ) ;
#45477 = CARTESIAN_POINT ( 'NONE',  ( 1.054774247047244540, 0.07405724077823318263, 0.6938976377415123631 ) ) ;
#45478 = ORIENTED_EDGE ( 'NONE', *, *, #43163, .T. ) ;
#45479 = CARTESIAN_POINT ( 'NONE',  ( -0.7185039370078739607, 1.928577636452523993E-17, 1.200787401467275695 ) ) ;
#45480 = DIRECTION ( 'NONE',  ( 0.000000000000000000, 0.000000000000000000, 1.000000000000000000 ) ) ;
#45481 = CARTESIAN_POINT ( 'NONE',  ( 0.07405724077823318263, -1.759842519631276581, 0.1787899950787401604 ) ) ;
#45482 = CARTESIAN_POINT ( 'NONE',  ( -1.094772975963752103E-17, -0.8420275590013542866, -0.1787899950787401882 ) ) ;
#45483 = CARTESIAN_POINT ( 'NONE',  ( 0.1113553986120547346, -1.430118110236220597, 0.1113553986120547346 ) ) ;
#45484 = CARTESIAN_POINT ( 'NONE',  ( 0.1595442748538490330, 0.09421994677690039011, -0.1177495158649775608 ) ) ;
#45485 = ADVANCED_FACE ( 'NONE', ( #132 ), #11583, .T. ) ;
#45486 = EDGE_LOOP ( 'NONE', ( #12373, #36635, #38461, #26976 ) ) ;
#45487 = ORIENTED_EDGE ( 'NONE', *, *, #47008, .F. ) ;
#45488 = CARTESIAN_POINT ( 'NONE',  ( -1.002407869896990045, -0.1264236179284866091, 1.951279527505291433 ) ) ;
#45489 = CARTESIAN_POINT ( 'NONE',  ( 1.054774247047244540, -0.07405724077823318263, 1.874999999946236784 ) ) ;
#45490 = ORIENTED_EDGE ( 'NONE', *, *, #39428, .F. ) ;
#45491 = CARTESIAN_POINT ( 'NONE',  ( -9.642888182262618425E-18, 0.01181102372957427288, -0.1574803149606299191 ) ) ;
#45492 = CARTESIAN_POINT ( 'NONE',  ( 0.6971942568897626646, -0.07405724077823297447, 0.4822834645131655606 ) ) ;
#45493 = CARTESIAN_POINT ( 'NONE',  ( -0.9500414927467378812, 0.1787899950787401604, 1.368110236166710125 ) ) ;
#45494 = CARTESIAN_POINT ( 'NONE',  ( 0.000000000000000000, 1.205361022782826802E-17, -0.09842519685039370636 ) ) ;
#45495 = EDGE_CURVE ( 'NONE', #39969, #27120, #23391, .T. ) ;
#45496 = CARTESIAN_POINT ( 'NONE',  ( -0.9500414927467378812, -0.1787899950787401604, 0.1377952755367876370 ) ) ;
#45497 = B_SPLINE_CURVE_WITH_KNOTS ( 'NONE', 3,
 ( #11601, #22843, #26222, #1489, #29624, #12316, #30084, #26933, #41485, #4366, #11363, #33898, #33657 ),
 .UNSPECIFIED., .F., .F.,
 ( 4, 2, 2, 1, 2, 2, 4 ),
 ( 0.000000000000000000, 0.2500000000000000000, 0.3750000000000002776, 0.4375000000000008327, 0.4687500000000012768, 0.5000000000000016653, 1.000000000000000000 ),
 .UNSPECIFIED. ) ;
#45498 = CARTESIAN_POINT ( 'NONE',  ( 0.3980944881889786346, 0.6449983665207558170, -0.7480314960629921295 ) ) ;
#45499 = CARTESIAN_POINT ( 'NONE',  ( -0.8759842519685039353, 0.1787899950787401882, 1.729822834591905556 ) ) ;
#45500 = CARTESIAN_POINT ( 'NONE',  ( -1.033464566929134687, -0.06523048226347956391, 2.005413385719245323 ) ) ;
#45501 = CARTESIAN_POINT ( 'NONE',  ( 0.7646288533564489232, -0.1113553986120547346, 1.402559055010582645 ) ) ;
#45502 = CARTESIAN_POINT ( 'NONE',  ( -0.9412147342319837628, 0.1574803149606300301, 1.749507874015747699 ) ) ;
#45503 = DIRECTION ( 'NONE',  ( 1.822029033848725028E-16, 0.000000000000000000, 1.000000000000000000 ) ) ;
#45504 = CARTESIAN_POINT ( 'NONE',  ( 1.054774247047244096, 0.000000000000000000, 1.601870078686393750 ) ) ;
#45505 = CARTESIAN_POINT ( 'NONE',  ( 0.02848443417738397848, -0.09842519685039370636, 0.2212455112941330848 ) ) ;
#45506 = LINE ( 'NONE', #38336, #20311 ) ;
#45507 = ORIENTED_EDGE ( 'NONE', *, *, #2894, .F. ) ;
#45508 = CARTESIAN_POINT ( 'NONE',  ( -0.8759842519685039353, 0.1574803149606299191, 1.791338582677165281 ) ) ;
#45509 = EDGE_LOOP ( 'NONE', ( #22160, #4051, #39235, #24959 ) ) ;
#45510 = ORIENTED_EDGE ( 'NONE', *, *, #26639, .F. ) ;
#45511 = CIRCLE ( 'NONE', #36354, 0.09940944881889707263 ) ;
#45512 = ORIENTED_EDGE ( 'NONE', *, *, #32883, .F. ) ;
#45513 = AXIS2_PLACEMENT_3D ( 'NONE', #1962, #39317, #31695 ) ;
#45514 = VECTOR ( 'NONE', #40716, 39.37007874015748143 ) ;
#45515 = CARTESIAN_POINT ( 'NONE',  ( 0.07405724077823318263, -1.041338582623402287, -0.1787899950787401604 ) ) ;
#45516 = CARTESIAN_POINT ( 'NONE',  ( -0.1787899950787401882, -1.181594488135212506, 0.000000000000000000 ) ) ;
#45517 = FACE_OUTER_BOUND ( 'NONE', #30948, .T. ) ;
#45518 = CARTESIAN_POINT ( 'NONE',  ( 0.07444174185955065859, -0.4611658568271400083, 0.1797182628040039087 ) ) ;
#45519 = CARTESIAN_POINT ( 'NONE',  ( -0.9412147342319837628, 0.1574803149606300301, 0.8341535431995593664 ) ) ;
#45520 = CARTESIAN_POINT ( 'NONE',  ( -0.1574803149606297803, -0.06446850393700798154, 0.06523048226347956391 ) ) ;
#45521 = CARTESIAN_POINT ( 'NONE',  ( -1.094772975963752103E-17, -0.1333661416785198728, -0.1787899950787401882 ) ) ;
#45522 = CARTESIAN_POINT ( 'NONE',  ( 0.8759842519685039353, 0.1787899950787401882, 0.8587598424659212970 ) ) ;
#45524 = CARTESIAN_POINT ( 'NONE',  ( 0.01230737760510397689, 0.07955613945526338049, 0.1377952755905511861 ) ) ;
#45523 = CARTESIAN_POINT ( 'NONE',  ( 0.08916369672653763623, 0.2440155479553977047, -0.03573910814354051141 ) ) ;
#45525 = CARTESIAN_POINT ( 'NONE',  ( 1.054774247047244540, 0.07405724077823318263, 1.958661417269071947 ) ) ;
#45526 = ADVANCED_FACE ( 'NONE', ( #34648 ), #8040, .T. ) ;
#45527 = CARTESIAN_POINT ( 'NONE',  ( 0.9412147342319837628, 0.1574803149606300301, 0.2140748031496061687 ) ) ;
#45528 = CARTESIAN_POINT ( 'NONE',  ( 2.458936486476969154E-17, 0.1102362204724409434, -0.2007874015748031815 ) ) ;
#45529 = CARTESIAN_POINT ( 'NONE',  ( 0.1787899950787401604, -0.4950787401037172186, -0.07405724077823318263 ) ) ;
#45530 = CARTESIAN_POINT ( 'NONE',  ( 0.6195511811023590720, -5.463695987328343027E-16, 1.186023622047243986 ) ) ;
#45531 = CARTESIAN_POINT ( 'NONE',  ( 3.284318927891251994E-17, -1.447342519631275692, 0.1787899950787401882 ) ) ;
#45532 = EDGE_CURVE ( 'NONE', #2118, #22349, #20006, .T. ) ;
#45533 = CARTESIAN_POINT ( 'NONE',  ( -1.054774247047244540, -0.07405724077823318263, 1.909448818843873186 ) ) ;
#45534 = ORIENTED_EDGE ( 'NONE', *, *, #13121, .T. ) ;
#45535 = CARTESIAN_POINT ( 'NONE',  ( -0.7495606340400177148, -0.1264236179284866091, 1.311515747977732405 ) ) ;
#45536 = CARTESIAN_POINT ( 'NONE',  ( 0.08946752424252873981, -0.5708661417322835607, 1.224299699984019663 ) ) ;
#45537 = CARTESIAN_POINT ( 'NONE',  ( 0.6971942568897648851, -0.07405724077823297447, 1.466535433017102763 ) ) ;
#45538 = VECTOR ( 'NONE', #27178, 39.37007874015748143 ) ;
#45539 = AXIS2_PLACEMENT_3D ( 'NONE', #35111, #38455, #31285 ) ;
#45540 = CARTESIAN_POINT ( 'NONE',  ( -1.002407869896990045, 0.1264236179284866091, 1.286909448765133801 ) ) ;
#45541 = CARTESIAN_POINT ( 'NONE',  ( 0.09142434311106251155, -0.09842519841270444547, -0.1536472792661565945 ) ) ;
#45542 = CARTESIAN_POINT ( 'NONE',  ( 0.6971942568897648851, -0.07405724077823297447, 0.6397637794737947026 ) ) ;
#45543 = CARTESIAN_POINT ( 'NONE',  ( -0.7495606340400177148, 0.1264236179284866091, 0.4699803149068661479 ) ) ;
#45544 = EDGE_CURVE ( 'NONE', #15682, #21809, #11667, .T. ) ;
#45545 = ( BOUNDED_CURVE ( )  B_SPLINE_CURVE ( 2, ( #38186, #34609, #15930, #13042, #26957, #35081, #41988, #41509, #1510 ),
 .UNSPECIFIED., .F., .T. ) 
 B_SPLINE_CURVE_WITH_KNOTS ( ( 3, 2, 2, 2, 3 ),
 ( 0.2300000000000000100, 0.2325000000000000122, 0.2349999999999999867, 0.2374999999999999889, 0.2399999999999999911 ),
 .UNSPECIFIED. ) 
 CURVE ( )  GEOMETRIC_REPRESENTATION_ITEM ( )  RATIONAL_B_SPLINE_CURVE ( ( 1.000000000000000000, 0.9238795325112859613, 1.000000000000000000, 0.9238795325112869605, 1.000000000000000000, 0.9238795325112869605, 1.000000000000000000, 0.9238795325112869605, 1.000000000000000000 ) ) 
 REPRESENTATION_ITEM ( '' )  ) ;
#45546 = LINE ( 'NONE', #5792, #14531 ) ;
#45547 = ORIENTED_EDGE ( 'NONE', *, *, #19179, .F. ) ;
#45548 = ORIENTED_EDGE ( 'NONE', *, *, #44664, .T. ) ;
#45549 = CARTESIAN_POINT ( 'NONE',  ( -0.7185039370078746268, 0.06523048226347956391, 0.2239173228346459099 ) ) ;
#45550 = CARTESIAN_POINT ( 'NONE',  ( 1.002407869896990045, -0.1264236179284866091, 1.163877952702141672 ) ) ;
#45551 = CARTESIAN_POINT ( 'NONE',  ( -0.2333684585041059245, -0.09851385095130453518, 0.05222081355495307442 ) ) ;
#45552 = CARTESIAN_POINT ( 'NONE',  ( -0.2559055118110236116, -0.04346162977120471976, -0.03525533988057330537 ) ) ;
#45553 = CARTESIAN_POINT ( 'NONE',  ( -0.8759842519685039353, -0.1574803149606299191, 1.299212598425196985 ) ) ;
#45554 = CARTESIAN_POINT ( 'NONE',  ( -0.8019270111902717657, 0.1787899950787401604, 0.1919291338045042428 ) ) ;
#45555 = CARTESIAN_POINT ( 'NONE',  ( 0.1264236179284866091, -1.655143653268608572, 0.1264236179284866091 ) ) ;
#45556 = ORIENTED_EDGE ( 'NONE', *, *, #27597, .T. ) ;
#45557 = CARTESIAN_POINT ( 'NONE',  ( -0.9873396505805591694, 0.1113553986120547346, 1.382874015640503940 ) ) ;
#45558 = CARTESIAN_POINT ( 'NONE',  ( -0.1787899950787401604, -0.6279527558517482566, 0.07405724077823318263 ) ) ;
#45559 = CARTESIAN_POINT ( 'NONE',  ( -0.2896766839110013758, -0.1108097609387616589, 1.001812157866037722 ) ) ;
#45560 = ORIENTED_EDGE ( 'NONE', *, *, #7469, .T. ) ;
#45561 = CARTESIAN_POINT ( 'NONE',  ( 0.7495606340400177148, 0.1264236179284866091, 1.296751968450173154 ) ) ;
#45562 = AXIS2_PLACEMENT_3D ( 'NONE', #32077, #33036, #39700 ) ;
#45563 = B_SPLINE_CURVE_WITH_KNOTS ( 'NONE', 3,
 ( #16351, #44364, #12532, #15407, #37673, #15884, #34329, #11571, #15649, #1460, #11812, #26436, #26903, #40999, #44596, #41221, #30054, #26198, #40764, #16119, #4825, #8187, #18970, #7960, #4337, #5069, #37193, #45314, #992, #30287, #37425, #33632, #746, #8425, #4579, #19448, #19214, #30742, #37914, #44839, #27152, #34552, #12049, #23053, #34103, #1230, #30508, #45069, #8907, #12284, #23538, #41463, #8661, #23297, #38139, #19685, #5303, #19920, #46261, #35504, #34806, #2180, #10090, #45541, #5546, #31210, #5788, #2645, #20157, #28086, #1951, #13457, #42648, #27632, #9860, #20627, #24471, #28312, #16802, #38841, #16581, #24701, #13234, #46496, #23763, #38610, #17278, #31441, #42880, #42185, #9391, #31682 ),
 .UNSPECIFIED., .F., .F.,
 ( 4, 2, 2, 2, 1, 1, 1, 1, 2, 2, 2, 2, 2, 1, 1, 1, 2, 2, 2, 2, 2, 1, 1, 1, 1, 1, 2, 2, 2, 2, 2, 1, 1, 2, 2, 2, 2, 1, 1, 2, 2, 2, 2, 2, 1, 1, 1, 1, 2, 2, 2, 2, 2, 2, 2, 4 ),
 ( 0.000000000000000000, 0.06249999999997683797, 0.09374999999996522226, 0.1093749999999593936, 0.1171874999999565209, 0.1210937499999550498, 0.1230468749999542588, 0.1240234374999538702, 0.1245117187499537037, 0.1249999999999535372, 0.1874999999999236167, 0.2187499999999085454, 0.2343749999999009959, 0.2421874999998971656, 0.2460937499998952227, 0.2480468749998942790, 0.2490234374998938072, 0.2499999999998933353, 0.3749999999998249733, 0.4374999999997907230, 0.4687499999997736255, 0.4843749999997650213, 0.4921874999997607469, 0.4960937499997586375, 0.4980468749997575828, 0.4990234374997570832, 0.4995117187497568056, 0.4999999999997565836, 0.5312499999997701838, 0.5468749999997769562, 0.5546874999997801758, 0.5585937499997818412, 0.5605468749997827294, 0.5615234374997831734, 0.5624999999997835065, 0.5937499999997979394, 0.6093749999998051559, 0.6171874999998085976, 0.6210937499998103739, 0.6230468749998112621, 0.6249999999998121503, 0.6874999999998441247, 0.7187499999998601119, 0.7343749999998679945, 0.7421874999998719913, 0.7460937499998739897, 0.7480468749998748779, 0.7490234374998753220, 0.7495117187498755440, 0.7499999999998757660, 0.8124999999999069633, 0.8437499999999225064, 0.8593749999999301670, 0.8749999999999379385, 0.9374999999999690248, 1.000000000000000000 ),
 .UNSPECIFIED. ) ;
#45564 = ( BOUNDED_CURVE ( )  B_SPLINE_CURVE ( 2, ( #42273, #35112, #2257, #18059, #36748, #14246, #28888, #29382, #43448 ),
 .UNSPECIFIED., .F., .F. ) 
 B_SPLINE_CURVE_WITH_KNOTS ( ( 3, 2, 2, 2, 3 ),
 ( 0.7900000000000000355, 0.7924999999999999822, 0.7950000000000000400, 0.7974999999999999867, 0.8000000000000000444 ),
 .UNSPECIFIED. ) 
 CURVE ( )  GEOMETRIC_REPRESENTATION_ITEM ( )  RATIONAL_B_SPLINE_CURVE ( ( 1.000000000000000000, 0.9238795325112899581, 1.000000000000000000, 0.9238795325112869605, 1.000000000000000000, 0.9238795325112869605, 1.000000000000000000, 0.9238795325112869605, 1.000000000000000000 ) ) 
 REPRESENTATION_ITEM ( '' )  ) ;
#45565 = CARTESIAN_POINT ( 'NONE',  ( -0.07405724077823318263, -0.2096456692375751329, -0.1787899950787401604 ) ) ;
#45566 = CYLINDRICAL_SURFACE ( 'NONE', #9623, 0.1574803149606299191 ) ;
#45567 = CIRCLE ( 'NONE', #11183, 0.1864803149606298893 ) ;
#45568 = CIRCLE ( 'NONE', #12618, 0.09842519685039370636 ) ;
#45569 = CARTESIAN_POINT ( 'NONE',  ( -0.1787899950787401604, 0.02546658295186362761, 0.07405724077823318263 ) ) ;
#45570 = CARTESIAN_POINT ( 'NONE',  ( 3.284318927891251994E-17, -1.762303149552535642, 0.1787899950787401882 ) ) ;
#45571 = SHAPE_DEFINITION_REPRESENTATION ( #30345, #40498 ) ;
#45572 = ADVANCED_FACE ( 'NONE', ( #8515 ), #832, .T. ) ;
#45573 = CARTESIAN_POINT ( 'NONE',  ( 0.003168982538894474926, -0.03928607229653706401, -0.1377952867935988979 ) ) ;
#45574 = CARTESIAN_POINT ( 'NONE',  ( -1.054774247047244540, -0.07405724077823318263, 0.7332677164816705506 ) ) ;
#45576 = LINE ( 'NONE', #45350, #22320 ) ;
#45575 = CARTESIAN_POINT ( 'NONE',  ( -0.06523048226347956391, -0.7042322834645671215, -0.1574803149606300301 ) ) ;
#45577 = CARTESIAN_POINT ( 'NONE',  ( 3.301370929368692659E-17, -1.565988691472808947, 0.1797182628040039365 ) ) ;
#45578 = CARTESIAN_POINT ( 'NONE',  ( 0.000000000000000000, 0.1473293504822046074, -0.9532488779249699284 ) ) ;
#45579 = CARTESIAN_POINT ( 'NONE',  ( -0.1264236179284866091, -0.3597440944344256208, -0.1264236179284866091 ) ) ;
#45580 = CARTESIAN_POINT ( 'NONE',  ( 0.2471922904502826257, 0.07695608958885345741, -0.07926021241888737967 ) ) ;
#45581 = CARTESIAN_POINT ( 'NONE',  ( 0.8759842519685039353, 0.1787899950787401882, 1.493602362150960650 ) ) ;
#45582 = CARTESIAN_POINT ( 'NONE',  ( 0.8019270111902716547, -0.1787899950787401604, 1.820866141678520789 ) ) ;
#45583 = CARTESIAN_POINT ( 'NONE',  ( 0.8019270111902716547, 0.1787899950787401604, 0.4675196849856070314 ) ) ;
#45584 = EDGE_CURVE ( 'NONE', #46651, #26985, #26917, .T. ) ;
#45585 = ( REPRESENTATION_RELATIONSHIP ('NONE','NONE', #9609, #30762 ) REPRESENTATION_RELATIONSHIP_WITH_TRANSFORMATION ( #1980 )SHAPE_REPRESENTATION_RELATIONSHIP( ) ) ;
#45586 = ORIENTED_EDGE ( 'NONE', *, *, #23278, .T. ) ;
#45588 = ORIENTED_EDGE ( 'NONE', *, *, #899, .T. ) ;
#45587 = CARTESIAN_POINT ( 'NONE',  ( -0.3161444924769509779, 1.914733266569311532, -0.6843357808987579061 ) ) ;
#45589 = CYLINDRICAL_SURFACE ( 'NONE', #19053, 0.1574803149606299191 ) ;
#45590 = CARTESIAN_POINT ( 'NONE',  ( -0.01585547164981869483, -0.5708661417322835607, 1.025733466389939119 ) ) ;
#45591 = CARTESIAN_POINT ( 'NONE',  ( -0.1787899950787401604, -0.002952755851748290004, 0.07405724077823318263 ) ) ;
#45592 = DIRECTION ( 'NONE',  ( -0.000000000000000000, -0.000000000000000000, -1.000000000000000000 ) ) ;
#45593 = CARTESIAN_POINT ( 'NONE',  ( 1.054774247047244096, 0.000000000000000000, 0.4945866141194645849 ) ) ;
#45594 = CARTESIAN_POINT ( 'NONE',  ( 0.5962569168439626477, 4.766607801171850497E-17, 0.000000000000000000 ) ) ;
#45595 = CARTESIAN_POINT ( 'NONE',  ( -0.8107537697050254399, -0.1574803149606297803, 0.7455708661417325134 ) ) ;
#45596 = CARTESIAN_POINT ( 'NONE',  ( 0.5555748031496099415, 0.6449983665207552619, -0.06082000038405668829 ) ) ;
#45597 = CARTESIAN_POINT ( 'NONE',  ( -1.054774247047244540, 0.07405724077823318263, 1.284448818843874740 ) ) ;
#45598 = CARTESIAN_POINT ( 'NONE',  ( 0.7185039370078746268, -0.06523048226347956391, 0.8489173227271192834 ) ) ;
#45599 = VERTEX_POINT ( 'NONE', #12377 ) ;
#45600 = DIRECTION ( 'NONE',  ( 1.822029033848725028E-16, 0.000000000000000000, 1.000000000000000000 ) ) ;
#45601 = CARTESIAN_POINT ( 'NONE',  ( 0.7495606340400177148, -0.1264236179284866091, 1.075295275536787276 ) ) ;
#45602 = ORIENTED_EDGE ( 'NONE', *, *, #32770, .F. ) ;
#45603 = CARTESIAN_POINT ( 'NONE',  ( -0.1787899950787401882, -1.343996062938362268, 0.000000000000000000 ) ) ;
#45604 = CARTESIAN_POINT ( 'NONE',  ( -0.7646288533564489232, -0.1113553986120547346, 0.6151574802074331050 ) ) ;
#45605 = CARTESIAN_POINT ( 'NONE',  ( 1.033464566929134687, 0.06523048226347956391, 0.09104330708661413640 ) ) ;
#45606 = CARTESIAN_POINT ( 'NONE',  ( -0.8107537697050253289, 0.1574803149606300301, 1.321358267716534751 ) ) ;
#45607 = VECTOR ( 'NONE', #35096, 39.37007874015748143 ) ;
#45608 = CARTESIAN_POINT ( 'NONE',  ( -0.9873396505805591694, -0.1113553986120547346, 1.058070866034204860 ) ) ;
#45610 = CARTESIAN_POINT ( 'NONE',  ( 0.1377952755905509363, 1.687505431895956106E-17, -0.1436967020037460685 ) ) ;
#45609 = FACE_OUTER_BOUND ( 'NONE', #22700, .T. ) ;
#45611 = CARTESIAN_POINT ( 'NONE',  ( 0.7495606340400177148, -0.1264236179284866091, 0.1697834645131657827 ) ) ;
#45612 = CARTESIAN_POINT ( 'NONE',  ( 0.7185039370078739607, 1.928577636452523993E-17, 1.437007873908220601 ) ) ;
#45613 = EDGE_LOOP ( 'NONE', ( #6421, #33174, #45063, #33865 ) ) ;
#45614 = ORIENTED_EDGE ( 'NONE', *, *, #10415, .T. ) ;
#45615 = DIRECTION ( 'NONE',  ( 1.822029033848725028E-16, 0.000000000000000000, 1.000000000000000000 ) ) ;
#45616 = CARTESIAN_POINT ( 'NONE',  ( 0.1574803149606299191, 0.5288907983920094757, -0.7507079620615707549 ) ) ;
#45617 = CARTESIAN_POINT ( 'NONE',  ( 1.054774247047244540, 0.07405724077823318263, 0.6988188975840318173 ) ) ;
#45618 = CARTESIAN_POINT ( 'NONE',  ( -9.642888182262618425E-18, -0.1456692912310557086, -0.1574803149606299191 ) ) ;
#45619 = ORIENTED_EDGE ( 'NONE', *, *, #8435, .F. ) ;
#45620 = ORIENTED_EDGE ( 'NONE', *, *, #28549, .F. ) ;
#45621 = CARTESIAN_POINT ( 'NONE',  ( -0.7185039370078746268, 0.06523048226347956391, 0.2534448817822371192 ) ) ;
#45622 = CARTESIAN_POINT ( 'NONE',  ( 0.7185039370078714072, 0.06523048226347728795, 1.867618110128693720 ) ) ;
#45623 = CARTESIAN_POINT ( 'NONE',  ( -0.9873396505805591694, -0.1113553986120547346, 1.884842519577511810 ) ) ;
#45624 = CARTESIAN_POINT ( 'NONE',  ( -0.1787899950787401604, -1.081816881615065062, -0.07405724077823318263 ) ) ;
#45625 = ORIENTED_EDGE ( 'NONE', *, *, #15382, .T. ) ;
#45626 = CARTESIAN_POINT ( 'NONE',  ( 3.284318927891251994E-17, 0.04872047249470835839, 0.1787899950787401882 ) ) ;
#45627 = EDGE_LOOP ( 'NONE', ( #32827, #18277, #39150, #11510 ) ) ;
#45628 = ORIENTED_EDGE ( 'NONE', *, *, #39100, .F. ) ;
#45629 = DIRECTION ( 'NONE',  ( -1.000000000000000000, 0.000000000000000000, 0.000000000000000000 ) ) ;
#45630 = DIRECTION ( 'NONE',  ( 0.000000000000000000, 0.000000000000000000, 1.000000000000000000 ) ) ;
#45631 = CARTESIAN_POINT ( 'NONE',  ( 0.9873396505805591694, -0.1113553986120547346, 1.894685039370078927 ) ) ;
#45632 = CARTESIAN_POINT ( 'NONE',  ( -0.1787899950787401604, -0.5590551180564723444, -0.07405724077823318263 ) ) ;
#45633 = EDGE_CURVE ( 'NONE', #47216, #40379, #1319, .T. ) ;
#45634 = EDGE_CURVE ( 'NONE', #28525, #9873, #19058, .T. ) ;
#45635 = CARTESIAN_POINT ( 'NONE',  ( -0.8019270111902716547, 0.1787899950787401604, 0.2755905511273391006 ) ) ;
#45636 = CARTESIAN_POINT ( 'NONE',  ( -0.8107537697050253289, 0.1574803149606300301, 1.006397637795276800 ) ) ;
#45637 = CARTESIAN_POINT ( 'NONE',  ( 0.1797182628040039087, -1.120614675724778353, -0.07444174185955065859 ) ) ;
#45638 = CARTESIAN_POINT ( 'NONE',  ( 0.9873396505805591694, -0.1113553986120547346, 1.107283464566929165 ) ) ;
#45639 = CARTESIAN_POINT ( 'NONE',  ( 0.9500414927467378812, 0.1787899950787401604, 1.097440944828127041 ) ) ;
#45640 = CARTESIAN_POINT ( 'NONE',  ( 1.054774247047244096, 0.000000000000000000, 0.2189960629383626012 ) ) ;
#45641 = EDGE_CURVE ( 'NONE', #12253, #29994, #30374, .T. ) ;
#45642 = ADVANCED_FACE ( 'NONE', ( #26288 ), #44680, .T. ) ;
#45643 = CARTESIAN_POINT ( 'NONE',  ( 1.033464566929133799, 0.000000000000000000, 1.624015748031496287 ) ) ;
#45645 = CYLINDRICAL_SURFACE ( 'NONE', #39951, 0.1864803149606299171 ) ;
#45644 = CARTESIAN_POINT ( 'NONE',  ( 0.7617962702031515487, 0.1145390712115343795, 1.980802457175323328 ) ) ;
#45646 = DIRECTION ( 'NONE',  ( -1.000000000000000000, 3.469446951953614189E-15, 1.144917494144692682E-16 ) ) ;
#45647 = CARTESIAN_POINT ( 'NONE',  ( -0.1113553986120547346, -0.7214566928058583350, 0.1113553986120547346 ) ) ;
#45648 = CARTESIAN_POINT ( 'NONE',  ( -0.1264236179284866091, 0.1126968504474643862, -0.1264236179284866091 ) ) ;
#45649 = FACE_OUTER_BOUND ( 'NONE', #20002, .T. ) ;
#45650 = CARTESIAN_POINT ( 'NONE',  ( 1.054774247047244540, -0.07405724077823318263, 1.043307086560409269 ) ) ;
#45651 = CARTESIAN_POINT ( 'NONE',  ( 0.6971942568897648851, -0.07405724077823297447, 1.899606299158834943 ) ) ;
#45652 = CARTESIAN_POINT ( 'NONE',  ( 0.7185039370078746268, 0.06523048226347956391, 0.3321850392625518844 ) ) ;
#45653 = ORIENTED_EDGE ( 'NONE', *, *, #11713, .T. ) ;
#45654 = CARTESIAN_POINT ( 'NONE',  ( 0.000000000000000000, 1.205361022782826802E-17, -0.09842519685039370636 ) ) ;
#45655 = CARTESIAN_POINT ( 'NONE',  ( -0.1113553986120547346, -1.626968503829480328, 0.1113553986120547346 ) ) ;
#45656 = CARTESIAN_POINT ( 'NONE',  ( -0.7185039370078739607, 1.928577636452523993E-17, 0.1771653542231816925 ) ) ;
#45657 = CARTESIAN_POINT ( 'NONE',  ( 0.8759842519685039353, -0.1787899950787401882, 1.311515747977732405 ) ) ;
#45658 = CARTESIAN_POINT ( 'NONE',  ( 0.08392772586502213195, -0.09126532511095285238, 0.2369773207360968970 ) ) ;
#45659 = CARTESIAN_POINT ( 'NONE',  ( -0.1113553986120547346, -1.754921259842519676, 0.1113553986120547346 ) ) ;
#45660 = CONICAL_SURFACE ( 'NONE', #36530, 0.1574803149606299191, 0.9599310885968735940 ) ;
#45661 = CARTESIAN_POINT ( 'NONE',  ( -0.7646288533564489232, 0.1113553986120547346, 1.875000000000000000 ) ) ;
#45662 = CARTESIAN_POINT ( 'NONE',  ( -0.8759842519685039353, -0.1787899950787401882, 0.5634842519147401640 ) ) ;
#45663 = DIRECTION ( 'NONE',  ( 0.000000000000000000, 0.000000000000000000, 1.000000000000000000 ) ) ;
#45664 = FACE_OUTER_BOUND ( 'NONE', #11266, .T. ) ;
#45665 = ORIENTED_EDGE ( 'NONE', *, *, #9973, .T. ) ;
#45667 = CARTESIAN_POINT ( 'NONE',  ( -0.1787899950787401604, -1.543307086560409713, -0.07405724077823318263 ) ) ;
#45666 = CARTESIAN_POINT ( 'NONE',  ( -9.642888182262618425E-18, -0.3818897636720003930, -0.1574803149606299191 ) ) ;
#45668 = CARTESIAN_POINT ( 'NONE',  ( -0.6971942568897626646, -0.07405724077823297447, 0.9547244093950547628 ) ) ;
#45669 = CARTESIAN_POINT ( 'NONE',  ( -0.8759842519685039353, 0.1574803149606299191, 0.01968503937007873988 ) ) ;
#45670 = ORIENTED_EDGE ( 'NONE', *, *, #13172, .F. ) ;
#45671 = CARTESIAN_POINT ( 'NONE',  ( -0.6971942568897626646, -0.07405724077823297447, 0.6791338582139527791 ) ) ;
#45672 = ORIENTED_EDGE ( 'NONE', *, *, #28416, .F. ) ;
#45673 = CARTESIAN_POINT ( 'NONE',  ( 0.000000000000000000, 0.000000000000000000, -0.2357204724409448504 ) ) ;
#45674 = CARTESIAN_POINT ( 'NONE',  ( 0.1519342447269234064, 0.1255575381907582666, -0.05895817643753602233 ) ) ;
#45675 = CARTESIAN_POINT ( 'NONE',  ( 0.1476377952755906220, -0.2274162997038010614, -0.9219983537151217323 ) ) ;
#45676 = CARTESIAN_POINT ( 'NONE',  ( 0.1787899950787401604, -0.7422499524812067317, -0.07405724077823318263 ) ) ;
#45677 = ORIENTED_EDGE ( 'NONE', *, *, #15662, .T. ) ;
#45678 = CARTESIAN_POINT ( 'NONE',  ( -0.09427829952974546568, -0.08956099458637047095, -0.1542373040544813001 ) ) ;
#45679 = CARTESIAN_POINT ( 'NONE',  ( 0.1574803149606299746, 0.4265678656643324129, 0.4783464566929144235 ) ) ;
#45680 = CARTESIAN_POINT ( 'NONE',  ( 0.000000000000000000, 0.000000000000000000, 0.000000000000000000 ) ) ;
#45681 = CARTESIAN_POINT ( 'NONE',  ( -0.9500414927467378812, -0.1787899950787401604, 0.4084645668753704717 ) ) ;
#45682 = ( BOUNDED_CURVE ( )  B_SPLINE_CURVE ( 2, ( #40462, #44071, #18668, #25419, #25168, #39994, #33328, #7186, #21811 ),
 .UNSPECIFIED., .F., .T. ) 
 B_SPLINE_CURVE_WITH_KNOTS ( ( 3, 2, 2, 2, 3 ),
 ( 0.9399999999999999467, 0.9425000000000000044, 0.9449999999999999512, 0.9475000000000000089, 0.9499999999999999556 ),
 .UNSPECIFIED. ) 
 CURVE ( )  GEOMETRIC_REPRESENTATION_ITEM ( )  RATIONAL_B_SPLINE_CURVE ( ( 1.000000000000000000, 0.9238795325112899581, 1.000000000000000000, 0.9238795325112869605, 1.000000000000000000, 0.9238795325112869605, 1.000000000000000000, 0.9238795325112799661, 1.000000000000000000 ) ) 
 REPRESENTATION_ITEM ( '' )  ) ;
#45683 = CARTESIAN_POINT ( 'NONE',  ( -0.8107537697050254399, -0.1574803149606297803, 0.3912401574803148208 ) ) ;
#45684 = ORIENTED_EDGE ( 'NONE', *, *, #16538, .F. ) ;
#45685 = CARTESIAN_POINT ( 'NONE',  ( -1.002407869896990045, -0.1264236179284866091, 1.636318897584031484 ) ) ;
#45686 = CARTESIAN_POINT ( 'NONE',  ( 0.07405724077823318263, -1.528543307032852239, 0.1787899950787401604 ) ) ;
#45687 = CARTESIAN_POINT ( 'NONE',  ( -0.2559057194709206673, 0.06872035568902440383, -0.3097284958882876582 ) ) ;
#45688 = AXIS2_PLACEMENT_3D ( 'NONE', #18791, #21692, #25998 ) ;
#45689 = ADVANCED_FACE ( 'NONE', ( #40847 ), #27240, .T. ) ;
#45690 = DIRECTION ( 'NONE',  ( -1.000000000000000000, 0.000000000000000000, 0.000000000000000000 ) ) ;
#45691 = CARTESIAN_POINT ( 'NONE',  ( 1.033464566929133799, 0.000000000000000000, 0.9547244094488189781 ) ) ;
#45692 = CARTESIAN_POINT ( 'NONE',  ( 1.033464566929134687, -0.06523048226347956391, 0.5585629921259840369 ) ) ;
#45693 = CARTESIAN_POINT ( 'NONE',  ( -0.1797182628040039087, -0.7121501087956446652, -0.07444174185955065859 ) ) ;
#45694 = LINE ( 'NONE', #12914, #43114 ) ;
#45695 = CARTESIAN_POINT ( 'NONE',  ( -1.033464566929134687, 0.06523048226347956391, 1.222933070758614127 ) ) ;
#45696 = EDGE_CURVE ( 'NONE', #22261, #41308, #22904, .T. ) ;
#45698 = CARTESIAN_POINT ( 'NONE',  ( -0.3161444924769509779, 2.177585298233989164, -4.122948637049707266 ) ) ;
#45697 = CARTESIAN_POINT ( 'NONE',  ( 0.1574803149606300301, -0.4827755905511812440, 0.06523048226347956391 ) ) ;
#45699 = CARTESIAN_POINT ( 'NONE',  ( -1.033464566929134687, 0.06523048226347956391, 1.183562992018456272 ) ) ;
#45700 = ORIENTED_EDGE ( 'NONE', *, *, #4497, .T. ) ;
#45701 = EDGE_CURVE ( 'NONE', #3606, #873, #38348, .T. ) ;
#45702 = PLANE ( 'NONE',  #8520 ) ;
#45703 = CARTESIAN_POINT ( 'NONE',  ( -0.6971942568897637749, 2.189545951927499583E-17, 1.070374015694267600 ) ) ;
#45704 = CARTESIAN_POINT ( 'NONE',  ( 0.7185039370078746268, 0.06523048226347956391, 1.050688976377951889 ) ) ;
#45706 = DIRECTION ( 'NONE',  ( 0.000000000000000000, -0.7880107536067216811, 0.6156614753256587358 ) ) ;
#45705 = CARTESIAN_POINT ( 'NONE',  ( -0.1574803149606299191, -0.2142072668875218688, -1.269802121763611291 ) ) ;
#45707 = DIRECTION ( 'NONE',  ( 0.000000000000000000, 0.000000000000000000, 1.000000000000000000 ) ) ;
#45708 = CARTESIAN_POINT ( 'NONE',  ( 0.1574803149606300301, -0.5861220471365676810, -0.06523048226347956391 ) ) ;
#45710 = CARTESIAN_POINT ( 'NONE',  ( -0.8759842519685039353, -0.1574803149606299191, 1.958661417215307177 ) ) ;
#45709 = CARTESIAN_POINT ( 'NONE',  ( 0.4811709046783464450, -3.032960542342102697E-32, 0.09842519685039370636 ) ) ;
#45711 = FACE_BOUND ( 'NONE', #15367, .T. ) ;
#45712 = PRODUCT_DEFINITION_SHAPE ( 'NONE', 'NONE',  #45336 ) ;
#45713 = CARTESIAN_POINT ( 'NONE',  ( -0.1787899950787401604, -0.4753937007336378473, -0.07405724077823318263 ) ) ;
#45714 = ORIENTED_EDGE ( 'NONE', *, *, #28957, .T. ) ;
#45715 = CARTESIAN_POINT ( 'NONE',  ( 0.5538057742782149795, 4.616380251121755931E-17, 0.000000000000000000 ) ) ;
#45716 = CARTESIAN_POINT ( 'NONE',  ( 0.8019270111902717657, 0.1787899950787401604, 0.7824803149068669805 ) ) ;
#45717 = EDGE_LOOP ( 'NONE', ( #40726, #39343, #19930, #1970 ) ) ;
#45718 = CARTESIAN_POINT ( 'NONE',  ( -0.05729443792182730560, 0.07836113345104929462, -0.2523541117089064811 ) ) ;
#45719 = FACE_OUTER_BOUND ( 'NONE', #2546, .T. ) ;
#45720 = CARTESIAN_POINT ( 'NONE',  ( -0.07405724077823318263, -1.646653543253324026, 0.1787899950787401604 ) ) ;
#45721 = CARTESIAN_POINT ( 'NONE',  ( -0.1787899950787401604, -0.8740157479777336258, -0.07405724077823318263 ) ) ;
#45722 = CARTESIAN_POINT ( 'NONE',  ( -0.1574803149606300301, -1.368602362204723866, -0.06523048226347956391 ) ) ;
#45723 = CARTESIAN_POINT ( 'NONE',  ( 0.9873396505805591694, -0.1113553986120547346, 1.254921259734991912 ) ) ;
#45724 = CARTESIAN_POINT ( 'NONE',  ( -1.033464566929133799, 0.000000000000000000, 1.387795275590551158 ) ) ;
#45725 = EDGE_LOOP ( 'NONE', ( #21589, #8915, #26355, #37146 ) ) ;
#45726 = ORIENTED_EDGE ( 'NONE', *, *, #8004, .T. ) ;
#45727 = CARTESIAN_POINT ( 'NONE',  ( -0.8019270111902717657, 0.1787899950787401604, 1.968503936954110189 ) ) ;
#45728 = ORIENTED_EDGE ( 'NONE', *, *, #13640, .F. ) ;
#45729 = CARTESIAN_POINT ( 'NONE',  ( 0.9500414927467378812, 0.1787899950787401604, 1.806102362150961316 ) ) ;
#45730 = VERTEX_POINT ( 'NONE', #45158 ) ;
#45731 = CARTESIAN_POINT ( 'NONE',  ( -0.1113553986120547346, -1.361220472333417364, -0.1113553986120547346 ) ) ;
#45732 = DIRECTION ( 'NONE',  ( 0.000000000000000000, 0.000000000000000000, -1.000000000000000000 ) ) ;
#45733 = CARTESIAN_POINT ( 'NONE',  ( 1.054774247047244096, 0.000000000000000000, 0.3813976377415121966 ) ) ;
#45734 = CARTESIAN_POINT ( 'NONE',  ( -0.8759842519685039353, 0.1787899950787401882, 1.409940944828126153 ) ) ;
#45735 = CARTESIAN_POINT ( 'NONE',  ( -0.8759842519685039353, 0.000000000000000000, 0.000000000000000000 ) ) ;
#45736 = ADVANCED_FACE ( 'NONE', ( #38228 ), #1639, .T. ) ;
#45737 = CARTESIAN_POINT ( 'NONE',  ( -0.9500414927467378812, 0.1787899950787401604, 0.9744094487651340231 ) ) ;
#45738 = CIRCLE ( 'NONE', #10570, 0.09842519685039317900 ) ;
#45739 = CARTESIAN_POINT ( 'NONE',  ( -0.8759842519685039353, -0.1787899950787401882, 0.2928149605761578567 ) ) ;
#45740 = DIRECTION ( 'NONE',  ( 0.5735764363510447161, 0.8191520442889925757, 0.000000000000000000 ) ) ;
#45741 = CARTESIAN_POINT ( 'NONE',  ( -0.8759842519685039353, -0.1787899950787401882, 1.710137795221826851 ) ) ;
#45742 = CARTESIAN_POINT ( 'NONE',  ( -0.7185039370078746268, -0.06523048226347956391, 1.990649606191687404 ) ) ;
#45743 = CARTESIAN_POINT ( 'NONE',  ( -0.1631888523359988907, 0.09129006187719393428, 0.1912159430412066763 ) ) ;
#45744 = CARTESIAN_POINT ( 'NONE',  ( -0.7185039370078739607, 1.928577636452523993E-17, 1.683070866141732402 ) ) ;
#45745 = CARTESIAN_POINT ( 'NONE',  ( -0.7185039370078760701, -0.06523048226348075740, 0.9375000000000002220 ) ) ;
#45746 = CARTESIAN_POINT ( 'NONE',  ( 0.8019270111902716547, -0.1787899950787401604, 1.707677165300568456 ) ) ;
#45747 = CARTESIAN_POINT ( 'NONE',  ( -0.06405282830903208380, -0.09842519685039370636, 0.2182790088969204789 ) ) ;
#45748 = FACE_OUTER_BOUND ( 'NONE', #42438, .T. ) ;
#45749 = DIMENSIONAL_EXPONENTS ( 1.000000000000000000, 0.000000000000000000, 0.000000000000000000, 0.000000000000000000, 0.000000000000000000, 0.000000000000000000, 0.000000000000000000 ) ;
#45750 = VERTEX_POINT ( 'NONE', #34894 ) ;
#45751 = CARTESIAN_POINT ( 'NONE',  ( 0.1787899950787401604, -1.090551181048598606, 0.07405724077823318263 ) ) ;
#45752 = CARTESIAN_POINT ( 'NONE',  ( 0.1264236179284866091, -1.166830708607653477, 0.1264236179284866091 ) ) ;
#45753 = ADVANCED_FACE ( 'NONE', ( #35119 ), #46792, .F. ) ;
#45754 = VECTOR ( 'NONE', #45469, 39.37007874015748143 ) ;
#45755 = DIRECTION ( 'NONE',  ( -1.000000000000000000, 0.000000000000000000, 7.047314121155780399E-15 ) ) ;
#45756 = CARTESIAN_POINT ( 'NONE',  ( 0.1797182628040039087, -0.4513233371421007667, -0.07444174185955065859 ) ) ;
#45757 = CARTESIAN_POINT ( 'NONE',  ( 2.892866454678787531E-17, -1.818897637687747926, 0.1574803149606299191 ) ) ;
#45758 = CARTESIAN_POINT ( 'NONE',  ( -0.8107537697050253289, 0.1574803149606300301, 0.7603346455617647770 ) ) ;
#45759 = CARTESIAN_POINT ( 'NONE',  ( -0.1113553986120547346, -0.07185039370078739884, -0.1113553986120547346 ) ) ;
#45760 = EDGE_CURVE ( 'NONE', #36821, #46851, #2584, .T. ) ;
#45761 = CARTESIAN_POINT ( 'NONE',  ( 1.054774247047244540, -0.07405724077823318263, 0.9645669290800953366 ) ) ;
#45762 = TOROIDAL_SURFACE ( 'NONE', #36624, 0.7874015748031495399, 0.04921259842519685318 ) ;
#45763 = DIRECTION ( 'NONE',  ( 0.000000000000000000, -1.000000000000000000, 0.000000000000000000 ) ) ;
#45764 = CARTESIAN_POINT ( 'NONE',  ( 0.9412147342319837628, 0.1574803149606300301, 0.08612204713656734789 ) ) ;
#45765 = VERTEX_POINT ( 'NONE', #31763 ) ;
#45766 = CARTESIAN_POINT ( 'NONE',  ( 0.9873396505805591694, -0.1113553986120547346, 0.2017716535433070890 ) ) ;
#45768 = CARTESIAN_POINT ( 'NONE',  ( -0.1787899950787401604, -0.3966535432533230265, 0.07405724077823318263 ) ) ;
#45767 = CARTESIAN_POINT ( 'NONE',  ( -9.642888182262618425E-18, -0.9724409447743621593, -0.1574803149606299191 ) ) ;
#45769 = DIRECTION ( 'NONE',  ( -0.5735764363510518216, -0.8191520442889876907, 0.000000000000000000 ) ) ;
#45770 = CARTESIAN_POINT ( 'NONE',  ( 0.1787899950787401604, -1.435039370024976391, -0.07405724077823318263 ) ) ;
#45771 = CARTESIAN_POINT ( 'NONE',  ( 1.054774247047244540, -0.07405724077823318263, 0.3789370078202520253 ) ) ;
#45772 = CARTESIAN_POINT ( 'NONE',  ( 0.1476377952755906220, 1.117014023967196179, -3.442880580079819008 ) ) ;
#45773 = CARTESIAN_POINT ( 'NONE',  ( -0.9500414927467378812, -0.1787899950787401604, 1.865157480261195877 ) ) ;
#45774 = ORIENTED_EDGE ( 'NONE', *, *, #38508, .F. ) ;
#45775 = CARTESIAN_POINT ( 'NONE',  ( -1.054774247047244540, -0.07405724077823318263, 1.520669291284818758 ) ) ;
#45776 = DIRECTION ( 'NONE',  ( 0.000000000000000000, 0.000000000000000000, -1.000000000000000000 ) ) ;
#45777 = CARTESIAN_POINT ( 'NONE',  ( 0.7495606340400177148, 0.1264236179284866091, 1.341043307032850462 ) ) ;
#45778 = CARTESIAN_POINT ( 'NONE',  ( 0.4330708661417322913, 4.616380251121755931E-17, 0.000000000000000000 ) ) ;
#45779 = CARTESIAN_POINT ( 'NONE',  ( -9.642888182262618425E-18, -1.248031495955464365, -0.1574803149606299191 ) ) ;
#45780 = CARTESIAN_POINT ( 'NONE',  ( -0.6971942568897626646, 0.07405724077823318263, 0.6742125983714335469 ) ) ;
#45781 = CARTESIAN_POINT ( 'NONE',  ( 0.7495606340400177148, 0.1264236179284866091, 0.1205708660879689087 ) ) ;
#45782 = CARTESIAN_POINT ( 'NONE',  ( -0.9500414927467378812, 0.1787899950787401604, 1.210629921206079818 ) ) ;
#45783 = DIRECTION ( 'NONE',  ( 1.822029033848725028E-16, 0.000000000000000000, 1.000000000000000000 ) ) ;
#45784 = CARTESIAN_POINT ( 'NONE',  ( 0.7495606340400177148, -0.1264236179284866091, 0.6028543306548976854 ) ) ;
#45785 = CARTESIAN_POINT ( 'NONE',  ( -0.6971942568897648851, -0.07405724077823297447, 0.5167322834108035723 ) ) ;
#45786 = ADVANCED_FACE ( 'NONE', ( #2727 ), #9714, .F. ) ;
#45787 = CARTESIAN_POINT ( 'NONE',  ( 0.1351206911648761555, -0.09842519685039370636, 0.2074211034490122396 ) ) ;
#45788 = AXIS2_PLACEMENT_3D ( 'NONE', #15270, #25823, #26057 ) ;
#45789 = CARTESIAN_POINT ( 'NONE',  ( 0.1574803149606300301, -0.08907480314960623813, 0.06523048226347956391 ) ) ;
#45790 = ORIENTED_EDGE ( 'NONE', *, *, #32933, .T. ) ;
#45791 = CARTESIAN_POINT ( 'NONE',  ( -0.7646288533564489232, -0.1113553986120547346, 0.2312992125984252023 ) ) ;
#45792 = CONICAL_SURFACE ( 'NONE', #5273, 0.1377952755905511861, 1.047197551196598297 ) ;
#45793 = CARTESIAN_POINT ( 'NONE',  ( 0.9500414927467377701, -0.1787899950787401604, 1.240157480261197875 ) ) ;
#45794 = CARTESIAN_POINT ( 'NONE',  ( -0.1637895306277413476, -0.09851385224194922352, 0.1653590908675625915 ) ) ;
#45795 = ORIENTED_EDGE ( 'NONE', *, *, #3786, .F. ) ;
#45796 = CARTESIAN_POINT ( 'NONE',  ( -0.9873396505805591694, -0.1113553986120547346, 0.6348425196850393526 ) ) ;
#45797 = CARTESIAN_POINT ( 'NONE',  ( -0.8759842519685039353, 0.1787899950787401882, 0.9424212597887559051 ) ) ;
#45798 = CARTESIAN_POINT ( 'NONE',  ( -1.094772975963752103E-17, -1.561639716260734279, -0.1787899950787401882 ) ) ;
#45799 = EDGE_LOOP ( 'NONE', ( #45012, #931, #26203, #22478 ) ) ;
#45800 = CARTESIAN_POINT ( 'NONE',  ( -0.7185039370078739607, 1.928577636452523993E-17, 0.1771653542231816925 ) ) ;
#45801 = CARTESIAN_POINT ( 'NONE',  ( 0.1787899950787401604, -0.5688976377415115859, -0.07405724077823318263 ) ) ;
#45802 = FACE_OUTER_BOUND ( 'NONE', #19462, .T. ) ;
#45803 = ORIENTED_EDGE ( 'NONE', *, *, #1941, .F. ) ;
#45804 = CARTESIAN_POINT ( 'NONE',  ( 0.8019270111902717657, -0.1787899950787401604, 1.309055118056472899 ) ) ;
#45805 = CARTESIAN_POINT ( 'NONE',  ( -0.1279527559055118058, 0.2216206741968047289, -0.3149606299212598381 ) ) ;
#45806 = EDGE_CURVE ( 'NONE', #6785, #13130, #2266, .T. ) ;
#45807 = CARTESIAN_POINT ( 'NONE',  ( 0.1264236179284866091, -0.3351377952218271283, -0.1264236179284866091 ) ) ;
#45808 = EDGE_CURVE ( 'NONE', #27525, #41698, #15782, .T. ) ;
#45809 = FACE_OUTER_BOUND ( 'NONE', #44918, .T. ) ;
#45810 = CARTESIAN_POINT ( 'NONE',  ( 0.9873396505805591694, 0.1113553986120547346, 1.815944881782236120 ) ) ;
#45811 = CARTESIAN_POINT ( 'NONE',  ( 0.9500414927467378812, 0.1787899950787401604, 1.604330708607653921 ) ) ;
#45812 = CARTESIAN_POINT ( 'NONE',  ( 0.1787899950787401604, 0.08452170106209991318, -0.07405724077823318263 ) ) ;
#45813 = CARTESIAN_POINT ( 'NONE',  ( 0.1787899950787401604, 0.1299212598962831977, 0.07405724077823318263 ) ) ;
#45814 = FACE_OUTER_BOUND ( 'NONE', #39436, .T. ) ;
#45815 = EDGE_CURVE ( 'NONE', #43027, #38897, #28954, .T. ) ;
#45816 = CARTESIAN_POINT ( 'NONE',  ( 1.002407869896990045, 0.1264236179284866091, 0.4995078739619842612 ) ) ;
#45817 = CARTESIAN_POINT ( 'NONE',  ( -0.7495606340400177148, -0.1264236179284866091, 0.8784448818360000022 ) ) ;
#45818 = CIRCLE ( 'NONE', #27513, 0.09842519685039370636 ) ;
#45820 = DIRECTION ( 'NONE',  ( 0.000000000000000000, -1.000000000000000000, 0.000000000000000000 ) ) ;
#45819 = CARTESIAN_POINT ( 'NONE',  ( -0.1113553986120547346, -0.9675196850393701364, 0.1113553986120547346 ) ) ;
#45822 = CARTESIAN_POINT ( 'NONE',  ( -0.8057660207509481642, -0.1572945814199120107, 1.986871297128391056 ) ) ;
#45821 = CARTESIAN_POINT ( 'NONE',  ( -0.1797182628040039087, -1.652110738716903615, 0.07444174185955065859 ) ) ;
#45823 = CARTESIAN_POINT ( 'NONE',  ( 0.1264236179284866091, -0.3400590550643468601, 0.1264236179284866091 ) ) ;
#45824 = CARTESIAN_POINT ( 'NONE',  ( 0.8759842519685039353, 0.1787899950787401882, 1.572342519631275692 ) ) ;
#45825 = CARTESIAN_POINT ( 'NONE',  ( 0.1574803149606299746, -0.5708661417322835607, 1.057384721142220263 ) ) ;
#45826 = CARTESIAN_POINT ( 'NONE',  ( 0.6971942568897648851, 0.07405724077823318263, 0.3937007873478114983 ) ) ;
#45827 = VECTOR ( 'NONE', #6813, 39.37007874015748143 ) ;
#45828 = VERTEX_POINT ( 'NONE', #39154 ) ;
#45829 = CARTESIAN_POINT ( 'NONE',  ( -0.8759842519685039353, -0.1574803149606299191, 0.1476377951680635792 ) ) ;
#45830 = CARTESIAN_POINT ( 'NONE',  ( 0.7646288533564489232, -0.1113553986120547346, 0.8513779526483780113 ) ) ;
#45831 = DIRECTION ( 'NONE',  ( 0.000000000000000000, 0.000000000000000000, 1.000000000000000000 ) ) ;
#45832 = CARTESIAN_POINT ( 'NONE',  ( -0.1264236179284866091, 0.06840551186478720236, -0.1264236179284866091 ) ) ;
#45833 = AXIS2_PLACEMENT_3D ( 'NONE', #20937, #34885, #13756 ) ;
#45834 = CARTESIAN_POINT ( 'NONE',  ( 0.9500414927467378812, 0.1787899950787401604, 0.3838582676627718127 ) ) ;
#45835 = DIRECTION ( 'NONE',  ( 0.000000000000000000, 1.000000000000000000, 0.000000000000000000 ) ) ;
#45837 = CARTESIAN_POINT ( 'NONE',  ( -0.8107537697050254399, 0.1574803149606300301, 1.715059055118110631 ) ) ;
#45836 = CARTESIAN_POINT ( 'NONE',  ( 1.002407869896990045, -0.1264236179284866091, 1.316437007820252081 ) ) ;
#45838 = CYLINDRICAL_SURFACE ( 'NONE', #47017, 0.6872114956789353579 ) ;
#45839 = CARTESIAN_POINT ( 'NONE',  ( -1.054774247047244540, -0.07405724077823318263, 1.476377952702141449 ) ) ;
#45840 = CARTESIAN_POINT ( 'NONE',  ( 1.033464566929134687, 0.06523048226347956391, 0.7898622046168821687 ) ) ;
#45841 = ORIENTED_EDGE ( 'NONE', *, *, #5516, .T. ) ;
#45843 = VECTOR ( 'NONE', #42419, 39.37007874015748143 ) ;
#45842 = CARTESIAN_POINT ( 'NONE',  ( -1.033464566929134687, 0.06523048226347956391, 0.7898622046168821687 ) ) ;
#45844 = CARTESIAN_POINT ( 'NONE',  ( 0.8759842519685039353, 0.1787899950787401882, 0.9817913385289134265 ) ) ;
#45845 = ORIENTED_EDGE ( 'NONE', *, *, #8215, .F. ) ;
#45846 = CARTESIAN_POINT ( 'NONE',  ( -0.07405724077823318263, -1.351377952702143004, -0.1787899950787401604 ) ) ;
#45847 = CARTESIAN_POINT ( 'NONE',  ( -1.033464566929133799, 0.000000000000000000, 0.5511811022546778682 ) ) ;
#45848 = CARTESIAN_POINT ( 'NONE',  ( -0.8759842519685039353, 0.000000000000000000, 0.000000000000000000 ) ) ;
#45849 = CARTESIAN_POINT ( 'NONE',  ( 0.9500414927467378812, -0.1787899950787401604, 1.668307086560410157 ) ) ;
#45850 = CARTESIAN_POINT ( 'NONE',  ( -0.7646288533564489232, -0.1113553986120547346, 1.412401574803149540 ) ) ;
#45851 = CARTESIAN_POINT ( 'NONE',  ( 0.7185039370078739607, 1.928577636452523993E-17, 1.791338582569637738 ) ) ;
#45852 = DIRECTION ( 'NONE',  ( 0.000000000000000000, 0.7071067811866579289, 0.7071067811864371055 ) ) ;
#45853 = CARTESIAN_POINT ( 'NONE',  ( 1.002407869896990045, -0.1264236179284866091, 0.1008858267178899676 ) ) ;
#45854 = CARTESIAN_POINT ( 'NONE',  ( 0.8759842519685039353, -0.1574803149606299191, 1.486220472333417142 ) ) ;
#45855 = VERTEX_POINT ( 'NONE', #17123 ) ;
#45856 = ORIENTED_EDGE ( 'NONE', *, *, #33481, .F. ) ;
#45857 = CARTESIAN_POINT ( 'NONE',  ( 0.07405724077823318263, 0.1003937008411650705, -0.1787899950787401604 ) ) ;
#45858 = CARTESIAN_POINT ( 'NONE',  ( -0.6971942568897648851, 0.07405724077823318263, 1.692913385773008539 ) ) ;
#45859 = CARTESIAN_POINT ( 'NONE',  ( 2.892866454678787531E-17, -0.2440944880814492068, 0.1574803149606299191 ) ) ;
#45860 = ( BOUNDED_CURVE ( )  B_SPLINE_CURVE ( 2, ( #10238, #29444, #9996, #14541, #21473, #36583, #43756, #39445, #39206 ),
 .UNSPECIFIED., .F., .F. ) 
 B_SPLINE_CURVE_WITH_KNOTS ( ( 3, 2, 2, 2, 3 ),
 ( 0.2600000000000000089, 0.2625000000000000111, 0.2650000000000000133, 0.2675000000000000155, 0.2700000000000000178 ),
 .UNSPECIFIED. ) 
 CURVE ( )  GEOMETRIC_REPRESENTATION_ITEM ( )  RATIONAL_B_SPLINE_CURVE ( ( 1.000000000000000000, 0.9238795325112869605, 1.000000000000000000, 0.9238795325112869605, 1.000000000000000000, 0.9238795325112869605, 1.000000000000000000, 0.9238795325112869605, 1.000000000000000000 ) ) 
 REPRESENTATION_ITEM ( '' )  ) ;
#45861 = CIRCLE ( 'NONE', #32900, 0.1377952755905511861 ) ;
#45862 = DIRECTION ( 'NONE',  ( -2.696301922142131245E-30, 0.6156614753256592909, 0.7880107536067212370 ) ) ;
#45863 = ( BOUNDED_CURVE ( )  B_SPLINE_CURVE ( 2, ( #33685, #18792, #4635, #41278, #23113, #796, #26723, #14990, #19266 ),
 .UNSPECIFIED., .F., .T. ) 
 B_SPLINE_CURVE_WITH_KNOTS ( ( 3, 2, 2, 2, 3 ),
 ( 0.3800000000000000044, 0.3825000000000000067, 0.3850000000000000089, 0.3875000000000000111, 0.3900000000000000133 ),
 .UNSPECIFIED. ) 
 CURVE ( )  GEOMETRIC_REPRESENTATION_ITEM ( )  RATIONAL_B_SPLINE_CURVE ( ( 1.000000000000000000, 0.9238795325112869605, 1.000000000000000000, 0.9238795325112869605, 1.000000000000000000, 0.9238795325112869605, 1.000000000000000000, 0.9238795325112869605, 1.000000000000000000 ) ) 
 REPRESENTATION_ITEM ( '' )  ) ;
#45864 = FACE_OUTER_BOUND ( 'NONE', #5236, .T. ) ;
#45865 = CARTESIAN_POINT ( 'NONE',  ( -0.1787899950787401604, -1.116265700512703907, 0.07405724077823318263 ) ) ;
#45866 = ORIENTED_EDGE ( 'NONE', *, *, #30247, .F. ) ;
#45867 = CARTESIAN_POINT ( 'NONE',  ( 3.284318927891251994E-17, -0.1481299212060791237, 0.1787899950787401882 ) ) ;
#45868 = ORIENTED_EDGE ( 'NONE', *, *, #29496, .T. ) ;
#45869 = EDGE_CURVE ( 'NONE', #157, #30455, #38707, .T. ) ;
#45870 = EDGE_CURVE ( 'NONE', #15025, #37935, #42727, .T. ) ;
#45871 = ORIENTED_EDGE ( 'NONE', *, *, #12795, .T. ) ;
#45872 = CARTESIAN_POINT ( 'NONE',  ( -0.2559051007267882372, -0.06201594832447591965, -0.3107242013313469275 ) ) ;
#45873 = VECTOR ( 'NONE', #18230, 39.37007874015748143 ) ;
#45874 = PLANE ( 'NONE',  #27692 ) ;
#45875 = ADVANCED_FACE ( 'NONE', ( #13763 ), #45874, .F. ) ;
#45876 = CARTESIAN_POINT ( 'NONE',  ( 0.8759842519685039353, -0.1574803149606299191, 1.771653543307086576 ) ) ;
#45877 = CARTESIAN_POINT ( 'NONE',  ( -1.094772975963752103E-17, -0.6058070865604094912, -0.1787899950787401882 ) ) ;
#45878 = ORIENTED_EDGE ( 'NONE', *, *, #8159, .T. ) ;
#45879 = EDGE_CURVE ( 'NONE', #9079, #2757, #10887, .T. ) ;
#45880 = FACE_OUTER_BOUND ( 'NONE', #40132, .T. ) ;
#45881 = CARTESIAN_POINT ( 'NONE',  ( -1.100456976456230270E-17, -1.152602864701155472, -0.1797182628040039365 ) ) ;
#45882 = CARTESIAN_POINT ( 'NONE',  ( -0.8759842519685039353, 0.1574803149606299191, 0.2165354330708661457 ) ) ;
#45883 = CARTESIAN_POINT ( 'NONE',  ( 0.9500414927467378812, 0.1787899950787401604, 1.058070866087969186 ) ) ;
#45884 = CARTESIAN_POINT ( 'NONE',  ( 0.8019270111902716547, -0.1787899950787401604, 0.2460629920722207653 ) ) ;
#45885 = CARTESIAN_POINT ( 'NONE',  ( 0.8759842519685039353, -0.1574803149606299191, 0.2362204724409449064 ) ) ;
#45886 = CARTESIAN_POINT ( 'NONE',  ( 1.033464566929133799, 0.000000000000000000, 1.545275590551181244 ) ) ;
#45888 = CARTESIAN_POINT ( 'NONE',  ( -0.8446276132374470613, 0.1554194282501662749, 1.978957984283404414 ) ) ;
#45887 = CARTESIAN_POINT ( 'NONE',  ( -0.6195511811023656223, 0.1864803149606298893, 1.186023622047243986 ) ) ;
#45889 = LINE ( 'NONE', #5403, #16005 ) ;
#45890 = CARTESIAN_POINT ( 'NONE',  ( -0.7185039370078739607, 1.928577636452523993E-17, 0.6889763778452283605 ) ) ;
#45891 = CARTESIAN_POINT ( 'NONE',  ( 0.8759842519685039353, 0.1787899950787401882, 0.9374999999462362288 ) ) ;
#45892 = CARTESIAN_POINT ( 'NONE',  ( 1.033464566929133799, 0.000000000000000000, 0.3937007872940480047 ) ) ;
#45893 = EDGE_LOOP ( 'NONE', ( #10166, #46632, #45086, #45278 ) ) ;
#45894 = CARTESIAN_POINT ( 'NONE',  ( 1.033464566929133799, 0.000000000000000000, 1.259842519577511810 ) ) ;
#45895 = CARTESIAN_POINT ( 'NONE',  ( 0.9966270878031755487, 0.1135902891731694064, 0.03937007931061534821 ) ) ;
#45896 = CARTESIAN_POINT ( 'NONE',  ( 1.033464566929134687, -0.06523048226347956391, 0.2436023622047244763 ) ) ;
#45897 = CARTESIAN_POINT ( 'NONE',  ( 0.8107537697050254399, -0.1574803149606297803, 1.887303149606298414 ) ) ;
#45898 = CARTESIAN_POINT ( 'NONE',  ( -0.1574803149606300301, -1.634350393593259954, -0.06523048226347956391 ) ) ;
#45899 = CARTESIAN_POINT ( 'NONE',  ( -0.9412147342319837628, -0.1574803149606297803, 0.3075787400499532809 ) ) ;
#45900 = CARTESIAN_POINT ( 'NONE',  ( 0.3161444924769295506, 1.209494567139728360, -1.479906699140346449 ) ) ;
#45901 = CARTESIAN_POINT ( 'NONE',  ( 1.054774247047244096, 0.000000000000000000, 1.321358267662771757 ) ) ;
#45902 = CARTESIAN_POINT ( 'NONE',  ( 0.06175619828060092270, -0.08093302715463278341, 0.2497778431879231764 ) ) ;
#45904 = VECTOR ( 'NONE', #4718, 39.37007874015748143 ) ;
#45903 = CARTESIAN_POINT ( 'NONE',  ( 0.1787899950787401604, 0.06102362210100767403, -0.07405724077823318263 ) ) ;
#45905 = CARTESIAN_POINT ( 'NONE',  ( 0.4811709046783464450, 4.466152701071653354E-17, 0.000000000000000000 ) ) ;
#45906 = CARTESIAN_POINT ( 'NONE',  ( -0.8019270111902717657, 0.1787899950787401604, 0.6643700786863951935 ) ) ;
#45907 = CARTESIAN_POINT ( 'NONE',  ( -0.7185039370078739607, 1.928577636452523993E-17, 0.3444881889763780070 ) ) ;
#45908 = CARTESIAN_POINT ( 'NONE',  ( -0.07975836855958619298, 0.08959396230938611316, 0.2393845553081392907 ) ) ;
#45909 = ORIENTED_EDGE ( 'NONE', *, *, #43336, .F. ) ;
#45910 = DIRECTION ( 'NONE',  ( 0.000000000000000000, 1.000000000000000000, 0.000000000000000000 ) ) ;
#45911 = CIRCLE ( 'NONE', #16114, 0.09842519685039370636 ) ;
#45912 = CARTESIAN_POINT ( 'NONE',  ( -0.1264236179284866091, -1.624507873961984261, -0.1264236179284866091 ) ) ;
#45913 = CARTESIAN_POINT ( 'NONE',  ( -0.9500414927467378812, 0.1787899950787401604, 0.9399606298674970661 ) ) ;
#45914 = CARTESIAN_POINT ( 'NONE',  ( -0.9412147342319837628, 0.1574803149606300301, 0.05659448818897635375 ) ) ;
#45915 = ORIENTED_EDGE ( 'NONE', *, *, #16944, .F. ) ;
#45916 = ADVANCED_FACE ( 'NONE', ( #11362 ), #37637, .F. ) ;
#45917 = CARTESIAN_POINT ( 'NONE',  ( -1.054774247047244540, 0.07405724077823318263, 0.6200787401037165525 ) ) ;
#45918 = ORIENTED_EDGE ( 'NONE', *, *, #786, .T. ) ;
#45919 = CARTESIAN_POINT ( 'NONE',  ( 0.1531955819909203431, 0.1251005666653343951, -0.05420542381351567407 ) ) ;
#45920 = LINE ( 'NONE', #17400, #8316 ) ;
#45921 = CARTESIAN_POINT ( 'NONE',  ( -0.1787899950787401604, -0.6487460154733331041, -0.07405724077823318263 ) ) ;
#45922 = ORIENTED_EDGE ( 'NONE', *, *, #28826, .T. ) ;
#45923 = CARTESIAN_POINT ( 'NONE',  ( 0.1979248385815023659, -0.08956033625505079032, 0.06050146127649999594 ) ) ;
#45924 = PLANE ( 'NONE',  #31058 ) ;
#45925 = EDGE_CURVE ( 'NONE', #8667, #16843, #7748, .T. ) ;
#45926 = ORIENTED_EDGE ( 'NONE', *, *, #3304, .F. ) ;
#45927 = CARTESIAN_POINT ( 'NONE',  ( 0.3108999017613326976, 1.482597719745565090, -0.3467144894627433027 ) ) ;
#45928 = CARTESIAN_POINT ( 'NONE',  ( 0.000000000000000000, 0.000000000000000000, -0.3149606299212598381 ) ) ;
#45929 = CARTESIAN_POINT ( 'NONE',  ( -1.054774247047244540, 0.07405724077823318263, 0.4183070865604097133 ) ) ;
#45930 = DIRECTION ( 'NONE',  ( 0.000000000000000000, 0.7907053606985359195, -0.6121968903568508757 ) ) ;
#45932 = ORIENTED_EDGE ( 'NONE', *, *, #29221, .F. ) ;
#45931 = CIRCLE ( 'NONE', #42858, 0.1624015748031505668 ) ;
#45933 = CARTESIAN_POINT ( 'NONE',  ( -0.8759842519685039353, 0.1787899950787401882, 1.651082677111590513 ) ) ;
#45934 = AXIS2_PLACEMENT_3D ( 'NONE', #36138, #32074, #3294 ) ;
#45935 = AXIS2_PLACEMENT_3D ( 'NONE', #5118, #31499, #38676 ) ;
#45936 = DIRECTION ( 'NONE',  ( 0.000000000000000000, 0.000000000000000000, -1.000000000000000000 ) ) ;
#45937 = DIRECTION ( 'NONE',  ( 0.000000000000000000, 0.000000000000000000, 1.000000000000000000 ) ) ;
#45938 = DIRECTION ( 'NONE',  ( 0.000000000000000000, 0.000000000000000000, -1.000000000000000000 ) ) ;
#45939 = VERTEX_POINT ( 'NONE', #18068 ) ;
#45940 = CARTESIAN_POINT ( 'NONE',  ( 0.7646288533564489232, -0.1113553986120547346, 0.5856299212598424786 ) ) ;
#45941 = CARTESIAN_POINT ( 'NONE',  ( -0.07444174185955065859, -0.7416776678507621678, 0.1797182628040039087 ) ) ;
#45942 = CARTESIAN_POINT ( 'NONE',  ( 0.1574803149606299191, 1.928577636452524918E-17, -0.1966003937007873570 ) ) ;
#45943 = CARTESIAN_POINT ( 'NONE',  ( -0.8759842519685039353, -0.1574803149606299191, 1.210629921152315047 ) ) ;
#45945 = CARTESIAN_POINT ( 'NONE',  ( 1.033464566929133799, 0.000000000000000000, 1.181102362097196989 ) ) ;
#45944 = CARTESIAN_POINT ( 'NONE',  ( -0.1113553986120547346, -0.4557086614173228578, 0.1113553986120547346 ) ) ;
#45946 = ORIENTED_EDGE ( 'NONE', *, *, #28416, .T. ) ;
#45947 = CARTESIAN_POINT ( 'NONE',  ( 0.06523048226347956391, 0.03887795275590551908, -0.1574803149606300301 ) ) ;
#45948 = CARTESIAN_POINT ( 'NONE',  ( 0.7185039370078746268, 0.06523048226347956391, 1.090059055118109965 ) ) ;
#45950 = CARTESIAN_POINT ( 'NONE',  ( -0.7646288533564489232, -0.1113553986120547346, 1.333661417322834719 ) ) ;
#45949 = DIRECTION ( 'NONE',  ( 1.822029033848725028E-16, 0.000000000000000000, 1.000000000000000000 ) ) ;
#45951 = DIRECTION ( 'NONE',  ( -1.000000000000000000, 0.000000000000000000, 0.000000000000000000 ) ) ;
#45953 = CARTESIAN_POINT ( 'NONE',  ( 0.9873396505805591694, -0.1113553986120547346, 1.687992125876724536 ) ) ;
#45952 = DIRECTION ( 'NONE',  ( 1.822029033848725028E-16, 0.000000000000000000, 1.000000000000000000 ) ) ;
#45954 = PLANE ( 'NONE',  #45303 ) ;
#45955 = CARTESIAN_POINT ( 'NONE',  ( 3.284318927891251994E-17, -0.5024606298674960669, 0.1787899950787401882 ) ) ;
#45956 = ORIENTED_EDGE ( 'NONE', *, *, #26743, .F. ) ;
#45957 = CARTESIAN_POINT ( 'NONE',  ( 1.054774247047244540, 0.07405724077823318263, 0.8513779527021426707 ) ) ;
#45958 = CARTESIAN_POINT ( 'NONE',  ( -0.8759842519685039353, 0.000000000000000000, 0.000000000000000000 ) ) ;
#45959 = DIRECTION ( 'NONE',  ( 0.000000000000000000, 0.000000000000000000, 1.000000000000000000 ) ) ;
#45960 = CARTESIAN_POINT ( 'NONE',  ( -0.1264236179284866091, -1.688484251914740275, 0.1264236179284866091 ) ) ;
#45961 = CARTESIAN_POINT ( 'NONE',  ( 0.07405724077823318263, -1.120078740103715997, -0.1787899950787401604 ) ) ;
#45962 = CARTESIAN_POINT ( 'NONE',  ( 0.1574803149606300301, -1.427657480314961091, 0.06523048226347956391 ) ) ;
#45963 = CARTESIAN_POINT ( 'NONE',  ( 0.1567662409572586624, 0.000000000000000000, -0.0004999999999998990712 ) ) ;
#45964 = AXIS2_PLACEMENT_3D ( 'NONE', #3589, #8773, #1098 ) ;
#45965 = ORIENTED_EDGE ( 'NONE', *, *, #46150, .F. ) ;
#45966 = CARTESIAN_POINT ( 'NONE',  ( -1.054774247047244540, 0.07405724077823318263, 1.879921259788756016 ) ) ;
#45967 = CARTESIAN_POINT ( 'NONE',  ( 0.8019270111902717657, -0.1787899950787401604, 1.825787401521040243 ) ) ;
#45968 = ORIENTED_EDGE ( 'NONE', *, *, #26158, .T. ) ;
#45969 = CARTESIAN_POINT ( 'NONE',  ( 0.06523048226347956391, -1.368602362097198322, -0.1574803149606300301 ) ) ;
#45970 = CARTESIAN_POINT ( 'NONE',  ( 1.033464566929133799, 0.000000000000000000, 1.781496062992125928 ) ) ;
#45971 = VECTOR ( 'NONE', #99, 39.37007874015748143 ) ;
#45972 = CARTESIAN_POINT ( 'NONE',  ( -0.8019270111902717657, 0.1787899950787401604, 1.569881889710015299 ) ) ;
#45973 = CARTESIAN_POINT ( 'NONE',  ( 0.2698848154395015464, 4.466152701071653354E-17, 0.000000000000000000 ) ) ;
#45974 = ADVANCED_FACE ( 'NONE', ( #32714 ), #36048, .F. ) ;
#45975 = CIRCLE ( 'NONE', #1601, 0.2952755905511806334 ) ;
#45976 = CARTESIAN_POINT ( 'NONE',  ( -1.054774247047244096, 0.000000000000000000, 0.1845472440407248116 ) ) ;
#45977 = ( BOUNDED_CURVE ( )  B_SPLINE_CURVE ( 2, ( #39891, #14514, #2759, #46848, #42754, #32507, #25053, #7075, #29180 ),
 .UNSPECIFIED., .F., .T. ) 
 B_SPLINE_CURVE_WITH_KNOTS ( ( 3, 2, 2, 2, 3 ),
 ( 0.8900000000000000133, 0.8924999999999999600, 0.8950000000000000178, 0.8974999999999999645, 0.9000000000000000222 ),
 .UNSPECIFIED. ) 
 CURVE ( )  GEOMETRIC_REPRESENTATION_ITEM ( )  RATIONAL_B_SPLINE_CURVE ( ( 1.000000000000000000, 0.9238795325112869605, 1.000000000000000000, 0.9238795325112869605, 1.000000000000000000, 0.9238795325112869605, 1.000000000000000000, 0.9238795325112869605, 1.000000000000000000 ) ) 
 REPRESENTATION_ITEM ( '' )  ) ;
#45978 = EDGE_CURVE ( 'NONE', #32474, #426, #37160, .T. ) ;
#45979 = CARTESIAN_POINT ( 'NONE',  ( -0.2372856289813495834, 0.04209688371797420947, -0.1484361490989300203 ) ) ;
#45980 = CARTESIAN_POINT ( 'NONE',  ( -0.8019270111902717657, 0.1787899950787401604, 1.732283464513166615 ) ) ;
#45981 = CARTESIAN_POINT ( 'NONE',  ( -0.1877875577363922188, 0.07959431159475777173, 0.1770138738565733005 ) ) ;
#45982 = CARTESIAN_POINT ( 'NONE',  ( -0.9873396505805591694, 0.1113553986120547346, 1.747047244094488194 ) ) ;
#45983 = CARTESIAN_POINT ( 'NONE',  ( 0.2559044495549840925, 0.03407473760173215793, -0.03222949210965551231 ) ) ;
#45984 = CARTESIAN_POINT ( 'NONE',  ( -0.1787899950787401604, -0.2501239682292389355, 0.07405724077823318263 ) ) ;
#45985 = CIRCLE ( 'NONE', #46726, 0.04921259842519686706 ) ;
#45986 = CARTESIAN_POINT ( 'NONE',  ( 0.6971942568897648851, -0.07405724077823297447, 1.702755905458047003 ) ) ;
#45987 = CARTESIAN_POINT ( 'NONE',  ( 0.1829792162757791496, -0.09842519685039370636, 0.1095673765095881852 ) ) ;
#45988 = CARTESIAN_POINT ( 'NONE',  ( -0.9412147342319837628, -0.1574803149606297803, 0.7406496061916858498 ) ) ;
#45989 = CARTESIAN_POINT ( 'NONE',  ( 0.3727034120734909473, -0.08090551181102362266, 1.098083891755157578E-17 ) ) ;
#45990 = EDGE_CURVE ( 'NONE', #34176, #33274, #43937, .T. ) ;
#45991 = EDGE_CURVE ( 'NONE', #6659, #8964, #40679, .T. ) ;
#45992 = ORIENTED_EDGE ( 'NONE', *, *, #18307, .F. ) ;
#45993 = CARTESIAN_POINT ( 'NONE',  ( -0.9500414927467377701, 0.1787899950787401604, 1.215551181048599272 ) ) ;
#45994 = CARTESIAN_POINT ( 'NONE',  ( -0.1787899950787401604, -0.9872047243556864027, 0.07405724077823318263 ) ) ;
#45995 = CARTESIAN_POINT ( 'NONE',  ( -0.1264236179284866091, -1.225885826717889815, -0.1264236179284866091 ) ) ;
#45996 = AXIS2_PLACEMENT_3D ( 'NONE', #37953, #1268, #8704 ) ;
#45997 = DIRECTION ( 'NONE',  ( 0.000000000000000000, -1.000000000000000000, -0.000000000000000000 ) ) ;
#45998 = ( LENGTH_UNIT ( ) NAMED_UNIT ( * ) SI_UNIT ( $, .METRE. ) ) ;
#45999 = CARTESIAN_POINT ( 'NONE',  ( 0.6971942568897626646, 0.07405724077823318263, 0.3937007873478115538 ) ) ;
#46000 = CARTESIAN_POINT ( 'NONE',  ( -0.8107537697050253289, -0.1574803149606297803, 0.8538385825696385156 ) ) ;
#46001 = CARTESIAN_POINT ( 'NONE',  ( -0.7646288533564489232, -0.1113553986120547346, 0.7037401574803149318 ) ) ;
#46002 = CARTESIAN_POINT ( 'NONE',  ( -0.1574803149606297803, 0.01427165354330708555, 0.06523048226347956391 ) ) ;
#46003 = AXIS2_PLACEMENT_3D ( 'NONE', #43285, #25581, #22423 ) ;
#46004 = AXIS2_PLACEMENT_3D ( 'NONE', #28445, #7085, #32753 ) ;
#46005 = CARTESIAN_POINT ( 'NONE',  ( 0.6971942568897626646, -0.07405724077823297447, 0.9104330708123776761 ) ) ;
#46006 = CIRCLE ( 'NONE', #33013, 0.2362204724409448231 ) ;
#46007 = B_SPLINE_CURVE_WITH_KNOTS ( 'NONE', 3,
 ( #17657, #46881, #47129, #28718, #39677, #4149, #14317, #1739, #12321, #45573, #12076, #15913, #19245 ),
 .UNSPECIFIED., .F., .F.,
 ( 4, 2, 2, 1, 2, 2, 4 ),
 ( 0.000000000000000000, 0.2499999999999993339, 0.3749999999999990008, 0.4374999999999988343, 0.4687499999999987788, 0.4999999999999987788, 1.000000000000000000 ),
 .UNSPECIFIED. ) ;
#46009 = CARTESIAN_POINT ( 'NONE',  ( 0.2007874015748031815, 0.000000000000000000, 0.000000000000000000 ) ) ;
#46008 = CARTESIAN_POINT ( 'NONE',  ( 0.1432458882846917303, 0.2127911801009324810, -0.02834147079956138293 ) ) ;
#46010 = CARTESIAN_POINT ( 'NONE',  ( 1.054774247047244540, -0.07405724077823318263, 1.914370078686394860 ) ) ;
#46011 = ORIENTED_EDGE ( 'NONE', *, *, #4150, .T. ) ;
#46012 = DIRECTION ( 'NONE',  ( -1.000000000000000000, 0.000000000000000000, 0.000000000000000000 ) ) ;
#46013 = CARTESIAN_POINT ( 'NONE',  ( -0.07405724077823318263, -0.5246062991588343882, -0.1787899950787401604 ) ) ;
#46014 = CARTESIAN_POINT ( 'NONE',  ( -0.1787899950787401882, -1.378444881836000002, 0.000000000000000000 ) ) ;
#46015 = CARTESIAN_POINT ( 'NONE',  ( -0.6971942568897648851, -0.07405724077823297447, 1.894685039316315489 ) ) ;
#46016 = ORIENTED_EDGE ( 'NONE', *, *, #18029, .F. ) ;
#46017 = CARTESIAN_POINT ( 'NONE',  ( -1.054774247047244540, -0.07405724077823318263, 1.402559055064346971 ) ) ;
#46018 = CARTESIAN_POINT ( 'NONE',  ( 1.054774247047244096, 0.000000000000000000, 1.365649606245448844 ) ) ;
#46019 = DIRECTION ( 'NONE',  ( 0.000000000000000000, 0.000000000000000000, 1.000000000000000000 ) ) ;
#46020 = CARTESIAN_POINT ( 'NONE',  ( -0.06523048226347956391, -1.230807086506645387, 0.1574803149606297803 ) ) ;
#46021 = CARTESIAN_POINT ( 'NONE',  ( -0.8019270111902717657, -0.1787899950787401604, 0.6446850393163160442 ) ) ;
#46022 = LINE ( 'NONE', #35736, #2892 ) ;
#46023 = DIRECTION ( 'NONE',  ( 0.000000000000000000, 0.000000000000000000, 1.000000000000000000 ) ) ;
#46024 = CARTESIAN_POINT ( 'NONE',  ( 0.6971942568897648851, -0.07405724077823297447, 0.6791338582139527791 ) ) ;
#46025 = CARTESIAN_POINT ( 'NONE',  ( -0.8019270111902716547, -0.1787899950787401604, 0.5216535432533228045 ) ) ;
#46026 = CARTESIAN_POINT ( 'NONE',  ( 0.1908307771205106085, -0.07780576619185783360, 0.1752568734204135448 ) ) ;
#46027 = EDGE_CURVE ( 'NONE', #31291, #1170, #28493, .T. ) ;
#46028 = CIRCLE ( 'NONE', #43747, 0.1377952755905511861 ) ;
#46029 = CARTESIAN_POINT ( 'NONE',  ( 0.8759842519685039353, 0.1574803149606299191, 1.663385826664125933 ) ) ;
#46030 = ORIENTED_EDGE ( 'NONE', *, *, #8765, .F. ) ;
#46031 = ORIENTED_EDGE ( 'NONE', *, *, #45212, .T. ) ;
#46032 = CARTESIAN_POINT ( 'NONE',  ( -0.9873396505805591694, 0.1113553986120547346, 0.3297244094488189226 ) ) ;
#46033 = CARTESIAN_POINT ( 'NONE',  ( 0.6971942568897648851, 0.07405724077823318263, 1.382874015694267822 ) ) ;
#46034 = CARTESIAN_POINT ( 'NONE',  ( 0.2067241386142287252, -0.09851384623809882057, 0.03057894068402287543 ) ) ;
#46035 = CARTESIAN_POINT ( 'NONE',  ( -0.8759842519685039353, -0.1574803149606299191, 1.840551180994834501 ) ) ;
#46036 = VECTOR ( 'NONE', #21845, 39.37007874015748143 ) ;
#46037 = EDGE_LOOP ( 'NONE', ( #3678, #38920, #40293, #29467 ) ) ;
#46038 = AXIS2_PLACEMENT_3D ( 'NONE', #39469, #10752, #25359 ) ;
#46039 = EDGE_CURVE ( 'NONE', #34797, #30178, #24478, .T. ) ;
#46040 = CARTESIAN_POINT ( 'NONE',  ( 0.07405724077823318263, -1.539494046969397623, 0.1787899950787401604 ) ) ;
#46041 = ORIENTED_EDGE ( 'NONE', *, *, #34067, .F. ) ;
#46042 = CARTESIAN_POINT ( 'NONE',  ( 0.8107537697050254399, 0.1574803149606300301, 1.006397637795276800 ) ) ;
#46043 = CARTESIAN_POINT ( 'NONE',  ( -0.1264236179284866091, -0.6254921259304881964, 0.1264236179284866091 ) ) ;
#46044 = ( LENGTH_UNIT ( ) NAMED_UNIT ( * ) SI_UNIT ( $, .METRE. ) ) ;
#46045 = ORIENTED_EDGE ( 'NONE', *, *, #35455, .T. ) ;
#46046 = CARTESIAN_POINT ( 'NONE',  ( 0.3246033735368759610, -3.032960542342102697E-32, 0.09842519685039370636 ) ) ;
#46047 = CARTESIAN_POINT ( 'NONE',  ( 0.07405724077823318263, -0.3326771653005671237, -0.1787899950787401604 ) ) ;
#46048 = CARTESIAN_POINT ( 'NONE',  ( -0.1264236179284866091, -0.7829724408911181710, 0.1264236179284866091 ) ) ;
#46049 = DIRECTION ( 'NONE',  ( 0.000000000000000000, 1.000000000000000000, 0.000000000000000000 ) ) ;
#46050 = CARTESIAN_POINT ( 'NONE',  ( 0.9873396505805591694, 0.1113553986120547346, 1.422244094380661572 ) ) ;
#46051 = CARTESIAN_POINT ( 'NONE',  ( 1.002407869896990045, 0.1264236179284866091, 1.680610236166708793 ) ) ;
#46052 = CARTESIAN_POINT ( 'NONE',  ( -0.07405724077823318263, 0.01562406326682424552, -0.1787899950787401604 ) ) ;
#46053 = ITEM_DEFINED_TRANSFORMATION ( 'NONE', 'NONE', #28595,  #20860 ) ;
#46054 = CARTESIAN_POINT ( 'NONE',  ( 0.2559055118110236671, -0.07588913166135959065, -0.3086013035114750225 ) ) ;
#46055 = COLOUR_RGB ( '', 0.09019608, 0.27058824, 0.51372549) ;
#46056 = CARTESIAN_POINT ( 'NONE',  ( 1.054774247047244540, 0.07405724077823318263, 0.4970472440407249226 ) ) ;
#46057 = AXIS2_PLACEMENT_3D ( 'NONE', #36336, #3488, #12113 ) ;
#46058 = CARTESIAN_POINT ( 'NONE',  ( -0.7495606340400177148, 0.1264236179284866091, 0.8686023621509606496 ) ) ;
#46060 = CARTESIAN_POINT ( 'NONE',  ( -0.7185039370078739607, 0.000000000000000000, -2.869337061179095023E-17 ) ) ;
#46059 = CARTESIAN_POINT ( 'NONE',  ( -0.06523048226347956391, -0.9404527559055111396, -0.1574803149606300301 ) ) ;
#46062 = CARTESIAN_POINT ( 'NONE',  ( -0.7614880836181143753, -0.1264398804583182212, 1.985866350195779395 ) ) ;
#46061 = CARTESIAN_POINT ( 'NONE',  ( -0.1797182628040039087, -1.612740659976745539, 0.07444174185955065859 ) ) ;
#46063 = CARTESIAN_POINT ( 'NONE',  ( -0.1574803149606299191, -0.4507874014672755836, 0.000000000000000000 ) ) ;
#46064 = CARTESIAN_POINT ( 'NONE',  ( -0.07405724077823318263, -0.3868110235682837295, 0.1787899950787401604 ) ) ;
#46065 = DIRECTION ( 'NONE',  ( 1.000000000000000000, -9.297927578135879519E-16, 0.000000000000000000 ) ) ;
#46066 = CARTESIAN_POINT ( 'NONE',  ( 0.6971942568897648851, 0.07405724077823318263, 1.540354330654897685 ) ) ;
#46068 = CARTESIAN_POINT ( 'NONE',  ( 0.1634876958473884812, 0.1607137227551046210, 3.803501547868341211E-07 ) ) ;
#46067 = LINE ( 'NONE', #24054, #29163 ) ;
#46069 = CARTESIAN_POINT ( 'NONE',  ( 0.9500414927467377701, 0.1787899950787401604, 0.3444881889226146243 ) ) ;
#46070 = CIRCLE ( 'NONE', #40724, 0.009842519685039378616 ) ;
#46071 = DIRECTION ( 'NONE',  ( 0.000000000000000000, 0.000000000000000000, -1.000000000000000000 ) ) ;
#46072 = CARTESIAN_POINT ( 'NONE',  ( -0.7185039370078739607, 1.928577636452523993E-17, 0.1377952754830242266 ) ) ;
#46073 = CYLINDRICAL_SURFACE ( 'NONE', #655, 0.1574803149606299191 ) ;
#46075 = CARTESIAN_POINT ( 'NONE',  ( -1.094772975963752103E-17, -0.05462598419820496182, -0.1787899950787401882 ) ) ;
#46074 = CARTESIAN_POINT ( 'NONE',  ( -0.1574803149606297803, -0.8420275589475905154, 0.06523048226347956391 ) ) ;
#46076 = CARTESIAN_POINT ( 'NONE',  ( 1.054774247047244540, -0.07405724077823318263, 0.4133858267178901480 ) ) ;
#46077 = CARTESIAN_POINT ( 'NONE',  ( -0.1264236179284866091, -0.8617125983714329918, 0.1264236179284866091 ) ) ;
#46078 = CARTESIAN_POINT ( 'NONE',  ( 0.9873396505805591694, -0.1113553986120547346, 0.08366141732283464971 ) ) ;
#46079 = CARTESIAN_POINT ( 'NONE',  ( 0.4632545931758527691, 4.616380251121755931E-17, 0.000000000000000000 ) ) ;
#46080 = CARTESIAN_POINT ( 'NONE',  ( -1.002407869896990045, -0.1264236179284866091, 1.473917322780881722 ) ) ;
#46081 = ORIENTED_EDGE ( 'NONE', *, *, #36171, .T. ) ;
#46082 = CARTESIAN_POINT ( 'NONE',  ( 1.054774247047244540, -0.07405724077823318263, 1.087598425143086578 ) ) ;
#46083 = CARTESIAN_POINT ( 'NONE',  ( -0.1264236179284866091, -1.348917322780881944, -0.1264236179284866091 ) ) ;
#46084 = CARTESIAN_POINT ( 'NONE',  ( -0.7185039370078746268, 0.06523048226347956391, 0.5290354329633386588 ) ) ;
#46085 = CARTESIAN_POINT ( 'NONE',  ( 0.8759842519685039353, 0.1574803149606299191, 0.09842519685039370636 ) ) ;
#46086 = CARTESIAN_POINT ( 'NONE',  ( 0.8019270111902717657, -0.1787899950787401604, 1.702755905458047003 ) ) ;
#46087 = CARTESIAN_POINT ( 'NONE',  ( -0.7185039370078746268, 0.06523048226347956391, 1.405019685039369914 ) ) ;
#46088 = DIRECTION ( 'NONE',  ( 0.000000000000000000, 0.000000000000000000, 1.000000000000000000 ) ) ;
#46089 = CARTESIAN_POINT ( 'NONE',  ( -0.04075098337902038209, -0.2719666410387886479, -0.06815351164855749933 ) ) ;
#46090 = CARTESIAN_POINT ( 'NONE',  ( 1.054774247047244540, -0.07405724077823318263, 0.2214566928596221063 ) ) ;
#46091 = PRODUCT_DEFINITION_CONTEXT ( 'detailed design', #38264, 'design' ) ;
#46092 = CARTESIAN_POINT ( 'NONE',  ( 0.8107537697050253289, -0.1574803149606297803, 1.444389763672000671 ) ) ;
#46093 = ORIENTED_EDGE ( 'NONE', *, *, #11537, .F. ) ;
#46094 = ORIENTED_EDGE ( 'NONE', *, *, #44329, .T. ) ;
#46095 = ADVANCED_FACE ( 'NONE', ( #8212 ), #15195, .T. ) ;
#46096 = DIRECTION ( 'NONE',  ( 0.000000000000000000, -1.000000000000000000, 0.000000000000000000 ) ) ;
#46097 = CARTESIAN_POINT ( 'NONE',  ( 1.033464566929133799, 0.000000000000000000, 1.771653543199558811 ) ) ;
#46098 = VERTEX_POINT ( 'NONE', #11598 ) ;
#46099 = ORIENTED_EDGE ( 'NONE', *, *, #31942, .F. ) ;
#46100 = CARTESIAN_POINT ( 'NONE',  ( -1.054774247047244540, -0.07405724077823318263, 1.673228346402929834 ) ) ;
#46101 = AXIS2_PLACEMENT_3D ( 'NONE', #12050, #1705, #30509 ) ;
#46102 = CARTESIAN_POINT ( 'NONE',  ( 1.033464566929133799, 0.000000000000000000, 0.03937007863263043694 ) ) ;
#46103 = DIRECTION ( 'NONE',  ( 0.000000000000000000, 0.000000000000000000, -1.000000000000000000 ) ) ;
#46104 = CARTESIAN_POINT ( 'NONE',  ( -0.01585547164981869483, -0.5708661417322833387, 1.025733466389939119 ) ) ;
#46105 = CARTESIAN_POINT ( 'NONE',  ( 0.07405724077823318263, -1.185163338307979597, 0.1787899950787401604 ) ) ;
#46106 = ORIENTED_EDGE ( 'NONE', *, *, #19656, .F. ) ;
#46107 = CARTESIAN_POINT ( 'NONE',  ( -0.07405724077823318263, -0.07185039364702387743, 0.1787899950787401604 ) ) ;
#46108 = ORIENTED_EDGE ( 'NONE', *, *, #4104, .T. ) ;
#46109 = ORIENTED_EDGE ( 'NONE', *, *, #34779, .T. ) ;
#46110 = ( GEOMETRIC_REPRESENTATION_CONTEXT ( 3 ) GLOBAL_UNCERTAINTY_ASSIGNED_CONTEXT ( ( #29243 ) ) GLOBAL_UNIT_ASSIGNED_CONTEXT ( ( #30026, #29565, #11787 ) ) REPRESENTATION_CONTEXT ( 'NONE', 'WORKASPACE' ) ) ;
#46111 = AXIS2_PLACEMENT_3D ( 'NONE', #35199, #16740, #38780 ) ;
#46112 = CARTESIAN_POINT ( 'NONE',  ( -0.2559055234657572897, -0.07599696328693686387, -0.3085855680301413106 ) ) ;
#46113 = CARTESIAN_POINT ( 'NONE',  ( -0.7185039370078739607, 1.928577636452523993E-17, 1.446850393700787274 ) ) ;
#46114 = PRODUCT ( 'Link Bar', 'Link Bar', '', ( #11606 ) ) ;
#46115 = CARTESIAN_POINT ( 'NONE',  ( 0.8107537697050253289, 0.1574803149606300301, 1.833169291338582418 ) ) ;
#46116 = AXIS2_PLACEMENT_3D ( 'NONE', #30375, #8041, #4199 ) ;
#46117 = CARTESIAN_POINT ( 'NONE',  ( 0.1264236179284866091, -0.6894685038832439883, -0.1264236179284866091 ) ) ;
#46118 = CARTESIAN_POINT ( 'NONE',  ( -0.8759842519685039353, 0.1787899950787401882, 0.3912401574265515491 ) ) ;
#46119 = CARTESIAN_POINT ( 'NONE',  ( -0.7646288533564489232, -0.1113553986120547346, 1.058070866141732402 ) ) ;
#46120 = CARTESIAN_POINT ( 'NONE',  ( -1.100456976456230270E-17, -1.191972943441313104, -0.1797182628040039365 ) ) ;
#46121 = CARTESIAN_POINT ( 'NONE',  ( -1.033464566929134687, 0.06523048226347956391, 0.2091535433070865757 ) ) ;
#46122 = CARTESIAN_POINT ( 'NONE',  ( 0.8759842519685039353, 0.1787899950787401882, 1.060531496009228247 ) ) ;
#46123 = CARTESIAN_POINT ( 'NONE',  ( 0.9500414927467377701, 0.1787899950787401604, 1.604330708607653921 ) ) ;
#46124 = CYLINDRICAL_SURFACE ( 'NONE', #10068, 0.1574803149606299191 ) ;
#46126 = CARTESIAN_POINT ( 'NONE',  ( -0.8354712756307374200, 0.1536107227041229595, 1.979144599375029623 ) ) ;
#46125 = LINE ( 'NONE', #13325, #18941 ) ;
#46127 = CARTESIAN_POINT ( 'NONE',  ( 0.7185039370078739607, 0.000000000000000000, 4.498031496062992574 ) ) ;
#46128 = CARTESIAN_POINT ( 'NONE',  ( -0.1574803149606297803, -0.7239173227271186173, 0.06523048226347956391 ) ) ;
#46129 = CIRCLE ( 'NONE', #29381, 0.6872114956789353579 ) ;
#46130 = CARTESIAN_POINT ( 'NONE',  ( 0.7185039370078739607, 1.928577636452523993E-17, 1.643700787401574992 ) ) ;
#46131 = CARTESIAN_POINT ( 'NONE',  ( 0.9500414927467377701, 0.1787899950787401604, 0.9744094487651340231 ) ) ;
#46132 = CARTESIAN_POINT ( 'NONE',  ( 0.8759842519685039353, -0.1787899950787401882, 1.985728346402929168 ) ) ;
#46133 = CARTESIAN_POINT ( 'NONE',  ( 0.9412147342319837628, 0.1574803149606300301, 0.3617125983176697201 ) ) ;
#46134 = EDGE_LOOP ( 'NONE', ( #14945, #36932, #45227, #35038 ) ) ;
#46135 = ADVANCED_FACE ( 'NONE', ( #30309 ), #23081, .F. ) ;
#46136 = DIRECTION ( 'NONE',  ( 1.000000000000000000, -3.469446951953626022E-15, -0.000000000000000000 ) ) ;
#46137 = CARTESIAN_POINT ( 'NONE',  ( 1.019390624703269133, 0.07727918952924982265, 0.03937226948580224706 ) ) ;
#46138 = PRODUCT_DEFINITION_FORMATION_WITH_SPECIFIED_SOURCE ( 'ANY', '', #38465, .NOT_KNOWN. ) ;
#46139 = VECTOR ( 'NONE', #14983, 39.37007874015748143 ) ;
#46140 = CARTESIAN_POINT ( 'NONE',  ( -9.642888182262618425E-18, -1.011811023514519681, -0.1574803149606299191 ) ) ;
#46141 = CARTESIAN_POINT ( 'NONE',  ( -0.9873396505805591694, -0.1113553986120547346, 0.3100393699712130080 ) ) ;
#46142 = CARTESIAN_POINT ( 'NONE',  ( 0.1264236179284866091, -0.09399606293836260118, -0.1264236179284866091 ) ) ;
#46143 = CARTESIAN_POINT ( 'NONE',  ( 1.054774247047244540, 0.07405724077823318263, 1.245078740103716886 ) ) ;
#46145 = CARTESIAN_POINT ( 'NONE',  ( 0.1822895153388602307, 0.000000000000000000, -0.2114570894355444486 ) ) ;
#46144 = CARTESIAN_POINT ( 'NONE',  ( 1.033464566929133799, 0.000000000000000000, 1.220472440837354400 ) ) ;
#46146 = CARTESIAN_POINT ( 'NONE',  ( 0.1264236179284866091, 0.1028543307624250058, -0.1264236179284866091 ) ) ;
#46147 = CARTESIAN_POINT ( 'NONE',  ( -0.7185039370078746268, -0.06523048226347956391, 1.006397637687749258 ) ) ;
#46148 = ( BOUNDED_CURVE ( )  B_SPLINE_CURVE ( 2, ( #46454, #20123, #27596, #12730, #16771, #45988, #9112, #42146, #17006 ),
 .UNSPECIFIED., .F., .T. ) 
 B_SPLINE_CURVE_WITH_KNOTS ( ( 3, 2, 2, 2, 3 ),
 ( 0.3499999999999999778, 0.3524999999999999800, 0.3549999999999999822, 0.3574999999999999845, 0.3599999999999999867 ),
 .UNSPECIFIED. ) 
 CURVE ( )  GEOMETRIC_REPRESENTATION_ITEM ( )  RATIONAL_B_SPLINE_CURVE ( ( 1.000000000000000000, 0.9238795325112879597, 1.000000000000000000, 0.9238795325112869605, 1.000000000000000000, 0.9238795325112869605, 1.000000000000000000, 0.9238795325112869605, 1.000000000000000000 ) ) 
 REPRESENTATION_ITEM ( '' )  ) ;
#46149 = AXIS2_PLACEMENT_3D ( 'NONE', #23894, #45910, #5907 ) ;
#46150 = EDGE_CURVE ( 'NONE', #28768, #3799, #37454, .T. ) ;
#46151 = ORIENTED_EDGE ( 'NONE', *, *, #37703, .T. ) ;
#46152 = CARTESIAN_POINT ( 'NONE',  ( 0.9412147342319837628, -0.1574803149606297803, 0.5142716535433068392 ) ) ;
#46153 = CARTESIAN_POINT ( 'NONE',  ( 0.3246033735368759610, 1.205361022782824954E-17, -0.09842519685039370636 ) ) ;
#46154 = ORIENTED_EDGE ( 'NONE', *, *, #7746, .T. ) ;
#46155 = CARTESIAN_POINT ( 'NONE',  ( 0.1264236179284866091, -1.713090551127338657, -0.1264236179284866091 ) ) ;
#46156 = CARTESIAN_POINT ( 'NONE',  ( -0.9500414927467378812, -0.1787899950787401604, 0.9645669290800953366 ) ) ;
#46157 = CARTESIAN_POINT ( 'NONE',  ( -0.6971942568897648851, 0.07405724077823318263, 1.929133858213952335 ) ) ;
#46158 = ORIENTED_EDGE ( 'NONE', *, *, #43810, .F. ) ;
#46159 = EDGE_CURVE ( 'NONE', #29926, #26131, #46955, .T. ) ;
#46160 = CARTESIAN_POINT ( 'NONE',  ( -1.054774247047244540, -0.07405724077823318263, 0.6545275590013545086 ) ) ;
#46161 = CARTESIAN_POINT ( 'NONE',  ( 0.1489248948074351209, 0.1264776978674661545, -0.06844634442982192035 ) ) ;
#46162 = DIRECTION ( 'NONE',  ( 0.000000000000000000, 0.000000000000000000, -1.000000000000000000 ) ) ;
#46163 = CARTESIAN_POINT ( 'NONE',  ( -0.1787899950787401882, -0.6462853855520729329, 0.000000000000000000 ) ) ;
#46164 = ORIENTED_EDGE ( 'NONE', *, *, #42509, .F. ) ;
#46165 = CARTESIAN_POINT ( 'NONE',  ( 0.05163519342973015708, -0.08956075397208444755, -0.1825432363577885742 ) ) ;
#46166 = PLANE ( 'NONE',  #17990 ) ;
#46167 = VERTEX_POINT ( 'NONE', #33896 ) ;
#46168 = LINE ( 'NONE', #21729, #2658 ) ;
#46169 = CARTESIAN_POINT ( 'NONE',  ( -0.8759842519685039353, -0.1574803149606299191, 1.761811023514519459 ) ) ;
#46170 = CARTESIAN_POINT ( 'NONE',  ( -0.7495606340400177148, 0.1264236179284866091, 0.5880905511273386566 ) ) ;
#46171 = CARTESIAN_POINT ( 'NONE',  ( 1.033464566929133799, 1.928577636452524610E-17, 4.498031496062992574 ) ) ;
#46172 = CARTESIAN_POINT ( 'NONE',  ( -0.8759842519685039353, -0.1787899950787401882, 1.710137795221826851 ) ) ;
#46173 = VECTOR ( 'NONE', #7631, 39.37007874015748143 ) ;
#46174 = FACE_OUTER_BOUND ( 'NONE', #34299, .T. ) ;
#46175 = CARTESIAN_POINT ( 'NONE',  ( -0.1574803149606299191, -0.2274162997038010614, -0.9219983537151217323 ) ) ;
#46176 = VERTEX_POINT ( 'NONE', #30775 ) ;
#46177 = CARTESIAN_POINT ( 'NONE',  ( 0.9412147342319837628, -0.1574803149606297803, 0.5536417322834641386 ) ) ;
#46178 = CARTESIAN_POINT ( 'NONE',  ( 0.7185039370078746268, 0.06523048226347956391, 0.6471456691838118891 ) ) ;
#46179 = CARTESIAN_POINT ( 'NONE',  ( -0.7185039370078739607, 1.928577636452523993E-17, 1.279527558947590515 ) ) ;
#46181 = DIRECTION ( 'NONE',  ( 0.000000000000000000, 0.000000000000000000, -1.000000000000000000 ) ) ;
#46180 = CARTESIAN_POINT ( 'NONE',  ( -0.1113553986120547346, -0.5049212598425196763, -0.1113553986120547346 ) ) ;
#46182 = CARTESIAN_POINT ( 'NONE',  ( -0.9412147342319837628, 0.1574803149606300301, 1.188484251860977503 ) ) ;
#46183 = ORIENTED_EDGE ( 'NONE', *, *, #4640, .F. ) ;
#46184 = EDGE_CURVE ( 'NONE', #18361, #24385, #30532, .T. ) ;
#46185 = CARTESIAN_POINT ( 'NONE',  ( 0.3161444924769275522, 1.975221432870720495, -0.9622519263226653186 ) ) ;
#46186 = CARTESIAN_POINT ( 'NONE',  ( 0.9412147342319837628, -0.1574803149606297803, 1.262303149606299746 ) ) ;
#46187 = CARTESIAN_POINT ( 'NONE',  ( 0.06523048226347956391, 0.08809055128862933182, -0.1574803149606297803 ) ) ;
#46189 = CARTESIAN_POINT ( 'NONE',  ( -0.1296641775163207277, 0.1169123912647608288, -2.121729632260068055 ) ) ;
#46188 = CARTESIAN_POINT ( 'NONE',  ( -0.1574803149606299191, -0.2274162997038020051, -0.9219983537151217323 ) ) ;
#46190 = CARTESIAN_POINT ( 'NONE',  ( 0.3604359965418638123, 1.205361022782824954E-17, -0.09842519685039370636 ) ) ;
#46192 = DIRECTION ( 'NONE',  ( 1.822029033848725028E-16, 0.000000000000000000, 1.000000000000000000 ) ) ;
#46191 = FACE_OUTER_BOUND ( 'NONE', #19573, .T. ) ;
#46193 = CARTESIAN_POINT ( 'NONE',  ( -1.033464566929133799, 0.000000000000000000, 0.6791338582677166613 ) ) ;
#46194 = CARTESIAN_POINT ( 'NONE',  ( 0.1264236179284866091, -0.5762795275052914334, 0.1264236179284866091 ) ) ;
#46195 = ORIENTED_EDGE ( 'NONE', *, *, #36911, .F. ) ;
#46196 = ADVANCED_FACE ( 'NONE', ( #37939 ), #38384, .T. ) ;
#46197 = LINE ( 'NONE', #14094, #29220 ) ;
#46198 = CARTESIAN_POINT ( 'NONE',  ( 1.054774247047244096, 0.000000000000000000, 0.8489173227808819444 ) ) ;
#46199 = CARTESIAN_POINT ( 'NONE',  ( -0.06179214533979354718, 0.08095196624129316620, -0.2497573591204075849 ) ) ;
#46200 = LINE ( 'NONE', #39477, #36564 ) ;
#46201 = CARTESIAN_POINT ( 'NONE',  ( 0.07444174185955046430, 0.1047790250626238068, -0.1797182628040039087 ) ) ;
#46202 = CARTESIAN_POINT ( 'NONE',  ( -0.1787899950787401882, -0.9896653542769447975, 0.000000000000000000 ) ) ;
#46203 = CARTESIAN_POINT ( 'NONE',  ( -0.1113553986120547346, -1.361220472440944906, 0.1113553986120547346 ) ) ;
#46204 = CARTESIAN_POINT ( 'NONE',  ( 0.7185039370078746268, -0.06523048226347956391, 1.281988188868851575 ) ) ;
#46205 = ORIENTED_EDGE ( 'NONE', *, *, #33032, .T. ) ;
#46206 = CARTESIAN_POINT ( 'NONE',  ( -1.054774247047244540, -0.07405724077823318263, 1.914370078686394860 ) ) ;
#46207 = CARTESIAN_POINT ( 'NONE',  ( 0.8019270111902717657, -0.1787899950787401604, 1.983267716481667886 ) ) ;
#46208 = ORIENTED_EDGE ( 'NONE', *, *, #18307, .T. ) ;
#46209 = CARTESIAN_POINT ( 'NONE',  ( -1.033464566929133799, 0.000000000000000000, 0.4724409447743622148 ) ) ;
#46210 = CARTESIAN_POINT ( 'NONE',  ( -0.6971942568897637749, 2.189545951927499583E-17, 1.537893700733637736 ) ) ;
#46211 = DIRECTION ( 'NONE',  ( 1.110632647060516814E-14, -0.2432573283306702361, 0.9699617890481173621 ) ) ;
#46212 = CARTESIAN_POINT ( 'NONE',  ( -0.6971942568897648851, 0.07405724077823318263, 1.023622047190330342 ) ) ;
#46213 = CARTESIAN_POINT ( 'NONE',  ( -0.8019270111902717657, -0.1787899950787401604, 0.2903543306548980185 ) ) ;
#46214 = CARTESIAN_POINT ( 'NONE',  ( -0.2471922904502826812, 0.03219022224904098672, -0.1427165354330708902 ) ) ;
#46215 = CARTESIAN_POINT ( 'NONE',  ( -0.6971942568897648851, -0.07405724077823297447, 1.938976377898990799 ) ) ;
#46216 = CARTESIAN_POINT ( 'NONE',  ( -0.7646288533564489232, -0.1113553986120547346, 1.845472440944881942 ) ) ;
#46217 = CIRCLE ( 'NONE', #34787, 0.09940944881889761386 ) ;
#46218 = DIRECTION ( 'NONE',  ( 0.000000000000000000, 0.000000000000000000, -1.000000000000000000 ) ) ;
#46219 = CARTESIAN_POINT ( 'NONE',  ( 0.1787899950787401604, -0.2304389288591599250, -0.07405724077823318263 ) ) ;
#46220 = CARTESIAN_POINT ( 'NONE',  ( 0.2066882016312708570, -0.09842519685039370636, 0.03057550915391468727 ) ) ;
#46221 = CARTESIAN_POINT ( 'NONE',  ( -0.9412147342319837628, -0.1574803149606297803, 1.498523622047243764 ) ) ;
#46222 = CARTESIAN_POINT ( 'NONE',  ( -1.033464566929133799, 0.000000000000000000, 0.8661417321759370402 ) ) ;
#46223 = ORIENTED_EDGE ( 'NONE', *, *, #20772, .T. ) ;
#46224 = VERTEX_POINT ( 'NONE', #27177 ) ;
#46225 = ORIENTED_EDGE ( 'NONE', *, *, #20513, .F. ) ;
#46226 = CARTESIAN_POINT ( 'NONE',  ( -0.1787899950787401604, -1.223425196796630532, -0.07405724077823318263 ) ) ;
#46227 = CARTESIAN_POINT ( 'NONE',  ( -0.8759842519685039353, -0.1574803149606299191, 1.368110236112944911 ) ) ;
#46228 = CARTESIAN_POINT ( 'NONE',  ( 0.07444174185955065859, -0.5005359355672972521, 0.1797182628040039087 ) ) ;
#46229 = DIRECTION ( 'NONE',  ( -1.000000000000000000, 0.000000000000000000, 0.000000000000000000 ) ) ;
#46230 = CARTESIAN_POINT ( 'NONE',  ( -1.033464566929133799, 0.000000000000000000, 0.7874015746956221085 ) ) ;
#46231 = CARTESIAN_POINT ( 'NONE',  ( -0.7185039370078746268, 0.06523048226347956391, 0.7750984251968497940 ) ) ;
#46232 = CARTESIAN_POINT ( 'NONE',  ( 0.1574803149606300301, 0.07332677165354323234, -0.06523048226347956391 ) ) ;
#46233 = VECTOR ( 'NONE', #80, 39.37007874015748143 ) ;
#46234 = EDGE_CURVE ( 'NONE', #9930, #28164, #5090, .T. ) ;
#46235 = CARTESIAN_POINT ( 'NONE',  ( 1.002407869896990045, -0.1264236179284866091, 0.9621062991588346103 ) ) ;
#46236 = CARTESIAN_POINT ( 'NONE',  ( 0.1751023000384251405, -0.1943988721995016100, -0.03960523631944738027 ) ) ;
#46237 = ADVANCED_FACE ( 'NONE', ( #15430 ), #19474, .T. ) ;
#46239 = CYLINDRICAL_SURFACE ( 'NONE', #3204, 0.1574803149606299191 ) ;
#46238 = DIRECTION ( 'NONE',  ( 0.000000000000000000, 0.000000000000000000, 1.000000000000000000 ) ) ;
#46240 = CARTESIAN_POINT ( 'NONE',  ( 0.8759842519685039353, -0.1574803149606299191, 0.2263779526483783444 ) ) ;
#46241 = EDGE_CURVE ( 'NONE', #10953, #1004, #15449, .T. ) ;
#46242 = VERTEX_POINT ( 'NONE', #41483 ) ;
#46243 = ADVANCED_FACE ( 'NONE', ( #18997 ), #36988, .T. ) ;
#46244 = EDGE_LOOP ( 'NONE', ( #4303, #2692, #26163, #35557, #35045 ) ) ;
#46245 = CARTESIAN_POINT ( 'NONE',  ( -0.9412147342319837628, -0.1574803149606297803, 0.7800196849318437042 ) ) ;
#46246 = CARTESIAN_POINT ( 'NONE',  ( -0.9873396505805591694, -0.1113553986120547346, 1.186023622047243986 ) ) ;
#46247 = CARTESIAN_POINT ( 'NONE',  ( -0.07405724077823318263, -0.6279527558517482566, 0.1787899950787401604 ) ) ;
#46248 = CARTESIAN_POINT ( 'NONE',  ( 0.07405724077823318263, -1.366141732229700478, 0.1787899950787401604 ) ) ;
#46249 = CARTESIAN_POINT ( 'NONE',  ( 0.6971942568897637749, 2.189545951927499583E-17, 0.3223425196312759144 ) ) ;
#46250 = ( BOUNDED_CURVE ( )  B_SPLINE_CURVE ( 2, ( #15648, #111, #11173, #8424, #36565, #8660, #41462, #40360, #5068 ),
 .UNSPECIFIED., .F., .T. ) 
 B_SPLINE_CURVE_WITH_KNOTS ( ( 3, 2, 2, 2, 3 ),
 ( 0.3099999999999999978, 0.3125000000000000000, 0.3150000000000000022, 0.3175000000000000044, 0.3200000000000000067 ),
 .UNSPECIFIED. ) 
 CURVE ( )  GEOMETRIC_REPRESENTATION_ITEM ( )  RATIONAL_B_SPLINE_CURVE ( ( 1.000000000000000000, 0.9238795325112869605, 1.000000000000000000, 0.9238795325112869605, 1.000000000000000000, 0.9238795325112869605, 1.000000000000000000, 0.9238795325112869605, 1.000000000000000000 ) ) 
 REPRESENTATION_ITEM ( '' )  ) ;
#46251 = CARTESIAN_POINT ( 'NONE',  ( -0.7495606340400177148, -0.1264236179284866091, 1.975885826717889815 ) ) ;
#46252 = ORIENTED_EDGE ( 'NONE', *, *, #16324, .F. ) ;
#46253 = ORIENTED_EDGE ( 'NONE', *, *, #31671, .T. ) ;
#46254 = CARTESIAN_POINT ( 'NONE',  ( -0.8759842519685039353, 0.1787899950787401882, 1.454232283410803017 ) ) ;
#46255 = CARTESIAN_POINT ( 'NONE',  ( 0.9500414927467378812, 0.1787899950787401604, 1.412401574749386990 ) ) ;
#46256 = VERTEX_POINT ( 'NONE', #33426 ) ;
#46257 = CYLINDRICAL_SURFACE ( 'NONE', #36694, 0.1574803149606299191 ) ;
#46258 = CARTESIAN_POINT ( 'NONE',  ( -0.1574803149606297803, -1.275098425089322696, 0.06523048226347956391 ) ) ;
#46259 = CARTESIAN_POINT ( 'NONE',  ( -0.7495606340400177148, -0.1264236179284866091, 0.6028543306548976854 ) ) ;
#46260 = CARTESIAN_POINT ( 'NONE',  ( -0.7495606340400177148, 0.1264236179284866091, 1.296751968450173154 ) ) ;
#46261 = CARTESIAN_POINT ( 'NONE',  ( 0.08577540572602856961, -0.09842547777292044719, -0.1568821689687208421 ) ) ;
#46262 = CARTESIAN_POINT ( 'NONE',  ( -1.033464566929133799, 0.000000000000000000, 1.614173228238929170 ) ) ;
#46263 = CARTESIAN_POINT ( 'NONE',  ( 1.054774247047244540, -0.07405724077823318263, 0.6938976377415124741 ) ) ;
#46264 = CARTESIAN_POINT ( 'NONE',  ( -0.6971942568897648851, 0.07405724077823318263, 0.4724409448281262636 ) ) ;
#46265 = DIRECTION ( 'NONE',  ( 0.000000000000000000, 0.000000000000000000, 1.000000000000000000 ) ) ;
#46266 = DIRECTION ( 'NONE',  ( 1.822029033848725028E-16, 0.000000000000000000, 1.000000000000000000 ) ) ;
#46267 = VERTEX_POINT ( 'NONE', #539 ) ;
#46268 = CARTESIAN_POINT ( 'NONE',  ( -0.6971942568897637749, 2.189545951927499583E-17, 1.503444881836000002 ) ) ;
#46269 = ORIENTED_EDGE ( 'NONE', *, *, #24553, .T. ) ;
#46270 = FACE_OUTER_BOUND ( 'NONE', #28648, .T. ) ;
#46271 = CARTESIAN_POINT ( 'NONE',  ( -0.8759842519685039353, -0.1574803149606299191, 0.4724409448818898127 ) ) ;
#46272 = CARTESIAN_POINT ( 'NONE',  ( 0.7495606340400177148, -0.1264236179284866091, 1.350885826717889815 ) ) ;
#46273 = CARTESIAN_POINT ( 'NONE',  ( 0.2033951071932515731, -0.09851384550996260259, -0.03145358857524988005 ) ) ;
#46274 = CARTESIAN_POINT ( 'NONE',  ( -0.7646288533564489232, -0.1113553986120547346, 1.835629921152314825 ) ) ;
#46275 = CIRCLE ( 'NONE', #10349, 0.1574803149606299191 ) ;
#46276 = COLOUR_RGB ( '', 0.72549020, 0.75294118, 0.79215686) ;
#46277 = EDGE_LOOP ( 'NONE', ( #11048, #35957, #13240, #33453 ) ) ;
#46278 = CARTESIAN_POINT ( 'NONE',  ( -0.7185039370078739607, 1.928577636452523993E-17, 0.5413385826771653919 ) ) ;
#46279 = CARTESIAN_POINT ( 'NONE',  ( -1.054774247047244096, 0.000000000000000000, 0.9325787401037164415 ) ) ;
#46280 = ( BOUNDED_CURVE ( )  B_SPLINE_CURVE ( 2, ( #15049, #861, #3993, #15519, #44241, #37788, #1105, #22447, #15996 ),
 .UNSPECIFIED., .F., .T. ) 
 B_SPLINE_CURVE_WITH_KNOTS ( ( 3, 2, 2, 2, 3 ),
 ( 0.5400000000000000355, 0.5424999999999999822, 0.5450000000000000400, 0.5474999999999999867, 0.5500000000000000444 ),
 .UNSPECIFIED. ) 
 CURVE ( )  GEOMETRIC_REPRESENTATION_ITEM ( )  RATIONAL_B_SPLINE_CURVE ( ( 1.000000000000000000, 0.9238795325112869605, 1.000000000000000000, 0.9238795325112869605, 1.000000000000000000, 0.9238795325112869605, 1.000000000000000000, 0.9238795325112869605, 1.000000000000000000 ) ) 
 REPRESENTATION_ITEM ( '' )  ) ;
#46281 = ORIENTED_EDGE ( 'NONE', *, *, #11885, .T. ) ;
#46282 = CARTESIAN_POINT ( 'NONE',  ( 0.1787899950787401604, -0.6476377952218281830, -0.07405724077823318263 ) ) ;
#46283 = ( CONVERSION_BASED_UNIT ( 'INCH', #31699 ) LENGTH_UNIT ( ) NAMED_UNIT ( #45749 ) ) ;
#46284 = EDGE_LOOP ( 'NONE', ( #5218, #22585, #11346, #18336 ) ) ;
#46285 = CARTESIAN_POINT ( 'NONE',  ( 1.054774247047244096, 0.000000000000000000, 1.400098425143086800 ) ) ;
#46286 = CARTESIAN_POINT ( 'NONE',  ( -0.07405724077823318263, -0.3129921259304885850, 0.1787899950787401604 ) ) ;
#46287 = CARTESIAN_POINT ( 'NONE',  ( -0.1264236179284866091, -0.7928149605761574126, -0.1264236179284866091 ) ) ;
#46288 = CARTESIAN_POINT ( 'NONE',  ( 0.8759842519685039353, 0.000000000000000000, 4.498031496062992574 ) ) ;
#46289 = DIRECTION ( 'NONE',  ( -5.464378949326941559E-15, -1.000000000000000000, 0.000000000000000000 ) ) ;
#46290 = CARTESIAN_POINT ( 'NONE',  ( 0.6971942568897648851, -0.07405724077823297447, 1.658464566875369472 ) ) ;
#46291 = CARTESIAN_POINT ( 'NONE',  ( 0.1264236179284866091, 0.08698233098335965419, -0.1264236179284866091 ) ) ;
#46292 = CARTESIAN_POINT ( 'NONE',  ( 0.1264236179284866091, 0.01919291343959031448, -0.1264236179284866091 ) ) ;
#46293 = CARTESIAN_POINT ( 'NONE',  ( 0.2559055118110236671, -0.08465028870289853513, -0.3071002465948138305 ) ) ;
#46294 = AXIS2_PLACEMENT_3D ( 'NONE', #25652, #43596, #18211 ) ;
#46295 = CARTESIAN_POINT ( 'NONE',  ( 0.6971942568897637749, 2.189545951927499583E-17, 0.4355314960092284138 ) ) ;
#46296 = ADVANCED_FACE ( 'NONE', ( #44386 ), #17720, .F. ) ;
#46297 = CARTESIAN_POINT ( 'NONE',  ( -1.054774247047244096, 0.000000000000000000, 0.7357283464029290565 ) ) ;
#46299 = CARTESIAN_POINT ( 'NONE',  ( 0.8107537697050254399, 0.1574803149606300301, 0.9965551180027086842 ) ) ;
#46298 = CARTESIAN_POINT ( 'NONE',  ( -0.1574803149606297803, -0.8518700787401587426, 0.06523048226347956391 ) ) ;
#46301 = CARTESIAN_POINT ( 'NONE',  ( -0.7738239533278032933, -0.1371752372774997231, 1.986169549678695079 ) ) ;
#46300 = CARTESIAN_POINT ( 'NONE',  ( -0.07444174185955065859, -1.661953258401944300, -0.1797182628040039087 ) ) ;
#46302 = CARTESIAN_POINT ( 'NONE',  ( -0.1574803149606300301, -0.4926181101286939423, -0.06523048226347956391 ) ) ;
#46303 = AXIS2_PLACEMENT_3D ( 'NONE', #7856, #22474, #33528 ) ;
#46304 = AXIS2_PLACEMENT_3D ( 'NONE', #13421, #6200, #2145 ) ;
#46305 = CARTESIAN_POINT ( 'NONE',  ( 1.054774247047244096, 0.000000000000000000, 1.562499999946236118 ) ) ;
#46307 = LINE ( 'NONE', #10378, #12449 ) ;
#46306 = CARTESIAN_POINT ( 'NONE',  ( 0.1528720448724809056, 0.09445537554013616610, -0.1971723546074463096 ) ) ;
#46308 = CARTESIAN_POINT ( 'NONE',  ( 0.6971942568897648851, 0.07405724077823318263, 0.3543307086076538659 ) ) ;
#46309 = CIRCLE ( 'NONE', #19537, 0.7775590551181102983 ) ;
#46310 = VERTEX_POINT ( 'NONE', #41022 ) ;
#46312 = EDGE_LOOP ( 'NONE', ( #10480, #4360, #26445, #6360 ) ) ;
#46311 = CARTESIAN_POINT ( 'NONE',  ( -0.1235961452251415349, -0.09842519685039370636, -0.2140748031496062798 ) ) ;
#46313 = EDGE_CURVE ( 'NONE', #34404, #32938, #12070, .T. ) ;
#46314 = CARTESIAN_POINT ( 'NONE',  ( 0.5717220857807087109, -0.09842519685039370636, 0.000000000000000000 ) ) ;
#46315 = CARTESIAN_POINT ( 'NONE',  ( -0.7185039370078739607, 0.000000000000000000, -2.869337061179095023E-17 ) ) ;
#46317 = CARTESIAN_POINT ( 'NONE',  ( 0.1264236179284866091, -0.1776574802611972648, -0.1264236179284866091 ) ) ;
#46316 = CARTESIAN_POINT ( 'NONE',  ( -0.1113553986120547346, -0.8887795274515276622, -0.1113553986120547346 ) ) ;
#46318 = CARTESIAN_POINT ( 'NONE',  ( 0.8759842519685039353, -0.1787899950787401882, 0.5634842519147401640 ) ) ;
#46319 = CARTESIAN_POINT ( 'NONE',  ( -0.1787899950787401604, -0.8641732282926931630, 0.07405724077823318263 ) ) ;
#46320 = CARTESIAN_POINT ( 'NONE',  ( 0.7603450666732096686, -0.1189009846179017033, 0.03937015212195697778 ) ) ;
#46321 = CARTESIAN_POINT ( 'NONE',  ( -0.7185039370078739607, 1.928577636452523993E-17, 1.515748031388535200 ) ) ;
#46322 = CARTESIAN_POINT ( 'NONE',  ( -0.8019270111902717657, -0.1787899950787401604, 1.505905511757261284 ) ) ;
#46323 = ORIENTED_EDGE ( 'NONE', *, *, #11700, .F. ) ;
#46324 = CARTESIAN_POINT ( 'NONE',  ( 0.7185039370078739607, 1.928577636452523993E-17, 0.4232283464566928832 ) ) ;
#46325 = CARTESIAN_POINT ( 'NONE',  ( 0.7495606340400177148, 0.1264236179284866091, 0.9867125983714331028 ) ) ;
#46326 = CARTESIAN_POINT ( 'NONE',  ( -0.7646288533564489232, 0.1113553986120547346, 0.7234251967428662056 ) ) ;
#46327 = CARTESIAN_POINT ( 'NONE',  ( 1.002407869896990045, -0.1264236179284866091, 1.670767716481669440 ) ) ;
#46328 = CARTESIAN_POINT ( 'NONE',  ( -0.7646288533564489232, 0.1113553986120547346, 1.363188976377952999 ) ) ;
#46329 = CARTESIAN_POINT ( 'NONE',  ( -1.002407869896990045, -0.1264236179284866091, 0.8833661416785196785 ) ) ;
#46330 = FACE_OUTER_BOUND ( 'NONE', #42961, .T. ) ;
#46331 = CARTESIAN_POINT ( 'NONE',  ( 0.9500414927467377701, 0.1787899950787401604, 0.1525590550643468324 ) ) ;
#46332 = CARTESIAN_POINT ( 'NONE',  ( -1.054774247047244096, 0.000000000000000000, 0.1008858267178899676 ) ) ;
#46333 = CARTESIAN_POINT ( 'NONE',  ( 0.9412147342319837628, 0.1574803149606300301, 1.621555118002709683 ) ) ;
#46334 = VERTEX_POINT ( 'NONE', #8451 ) ;
#46335 = CARTESIAN_POINT ( 'NONE',  ( -1.054774247047244540, 0.07405724077823318263, 1.756889763725764553 ) ) ;
#46336 = CIRCLE ( 'NONE', #30376, 0.1003937007874010356 ) ;
#46337 = CARTESIAN_POINT ( 'NONE',  ( -0.2471922904502826812, 0.09123121687245379363, -0.04590630800384516014 ) ) ;
#46338 = CARTESIAN_POINT ( 'NONE',  ( -1.033464566929133799, 0.000000000000000000, 0.7972440944881890035 ) ) ;
#46339 = CARTESIAN_POINT ( 'NONE',  ( -0.07405724077823318263, -1.111344440670184897, 0.1787899950787401604 ) ) ;
#46340 = VERTEX_POINT ( 'NONE', #28334 ) ;
#46341 = CARTESIAN_POINT ( 'NONE',  ( -0.07405724077823318263, -0.1653543306548978520, -0.1787899950787401604 ) ) ;
#46342 = ORIENTED_EDGE ( 'NONE', *, *, #1198, .F. ) ;
#46343 = CIRCLE ( 'NONE', #29580, 0.1574803149606299191 ) ;
#46344 = CONICAL_SURFACE ( 'NONE', #45539, 0.1003937007874011050, 0.7853981633973787790 ) ;
#46345 = ORIENTED_EDGE ( 'NONE', *, *, #27805, .F. ) ;
#46346 = CARTESIAN_POINT ( 'NONE',  ( 0.7495606340400177148, 0.1264236179284866091, 1.060531496009228247 ) ) ;
#46347 = CARTESIAN_POINT ( 'NONE',  ( -1.033464566929134687, -0.06523048226347956391, 1.218011810916094895 ) ) ;
#46348 = CARTESIAN_POINT ( 'NONE',  ( -1.033464566929133799, 0.000000000000000000, 0.9055118109160944506 ) ) ;
#46349 = CARTESIAN_POINT ( 'NONE',  ( 0.7185039370078746268, 0.06523048226347956391, 1.759350393700787940 ) ) ;
#46350 = CARTESIAN_POINT ( 'NONE',  ( -0.07444174185955065859, -0.1904965654885572290, 0.1797182628040039087 ) ) ;
#46351 = CARTESIAN_POINT ( 'NONE',  ( 0.1264236179284866091, -0.8075787401037164415, -0.1264236179284866091 ) ) ;
#46352 = EDGE_CURVE ( 'NONE', #21958, #6613, #7017, .T. ) ;
#46353 = CARTESIAN_POINT ( 'NONE',  ( -0.9500414927467377701, -0.1787899950787401604, 0.4133858267178901480 ) ) ;
#46354 = CARTESIAN_POINT ( 'NONE',  ( 0.07444174185955065859, -1.327307589110604980, 0.1797182628040039087 ) ) ;
#46355 = CARTESIAN_POINT ( 'NONE',  ( -0.7185039370078692977, 0.06523048226347515077, 1.946358267609008097 ) ) ;
#46356 = CARTESIAN_POINT ( 'NONE',  ( 0.8759842519685039353, -0.1787899950787401882, 1.080216535379306952 ) ) ;
#46357 = CARTESIAN_POINT ( 'NONE',  ( 0.9500414927467377701, 0.1787899950787401604, 1.486220472387181912 ) ) ;
#46358 = CARTESIAN_POINT ( 'NONE',  ( 0.7495606340400177148, 0.1264236179284866091, 0.2337598424659216578 ) ) ;
#46359 = AXIS2_PLACEMENT_3D ( 'NONE', #16096, #18945, #8637 ) ;
#46360 = LINE ( 'NONE', #10192, #12382 ) ;
#46361 = ADVANCED_FACE ( 'NONE', ( #24494 ), #13477, .F. ) ;
#46362 = CARTESIAN_POINT ( 'NONE',  ( 0.8107537697050253289, -0.1574803149606297803, 1.651082677165354839 ) ) ;
#46364 = CARTESIAN_POINT ( 'NONE',  ( -0.8537172869947121656, 0.1566887183902881953, 1.978776088056980464 ) ) ;
#46363 = CARTESIAN_POINT ( 'NONE',  ( 0.7185039370078739607, 0.000000000000000000, 4.498031496062992574 ) ) ;
#46365 = LINE ( 'NONE', #46127, #18275 ) ;
#46366 = CARTESIAN_POINT ( 'NONE',  ( -0.9412147342319837628, 0.1574803149606300301, 1.700295275483023172 ) ) ;
#46367 = CARTESIAN_POINT ( 'NONE',  ( 0.1787899950787401604, -0.01771653537930737918, -0.07405724077823318263 ) ) ;
#46368 = DIRECTION ( 'NONE',  ( 1.000000000000000000, -3.469446951953613794E-15, 0.000000000000000000 ) ) ;
#46370 = DIRECTION ( 'NONE',  ( 0.000000000000000000, 0.000000000000000000, -1.000000000000000000 ) ) ;
#46369 = CARTESIAN_POINT ( 'NONE',  ( 0.7495606340400177148, -0.1264236179284866091, 1.070374015694267600 ) ) ;
#46371 = CARTESIAN_POINT ( 'NONE',  ( 0.9500414927467377701, -0.1787899950787401604, 1.909448818843873186 ) ) ;
#46372 = CARTESIAN_POINT ( 'NONE',  ( 1.033464566929133799, 0.000000000000000000, 0.5511811022546778682 ) ) ;
#46373 = EDGE_LOOP ( 'NONE', ( #16419, #29025 ) ) ;
#46374 = DIRECTION ( 'NONE',  ( 0.000000000000000000, -1.000000000000000000, 0.000000000000000000 ) ) ;
#46375 = CARTESIAN_POINT ( 'NONE',  ( 1.031513553818225626, 0.03767821469943116036, 0.03937002695152881648 ) ) ;
#46376 = AXIS2_PLACEMENT_3D ( 'NONE', #2832, #20591, #46931 ) ;
#46377 = CARTESIAN_POINT ( 'NONE',  ( -0.8107537697050234415, -0.1574803149606297803, 0.1845472439869611236 ) ) ;
#46378 = ORIENTED_EDGE ( 'NONE', *, *, #27582, .T. ) ;
#46379 = CARTESIAN_POINT ( 'NONE',  ( 1.002407869896990045, -0.1264236179284866091, 1.237696850339937038 ) ) ;
#46380 = CARTESIAN_POINT ( 'NONE',  ( 1.033464566929134687, 0.06523048226347956391, 1.222933070758614127 ) ) ;
#46381 = DIMENSIONAL_EXPONENTS ( 1.000000000000000000, 0.000000000000000000, 0.000000000000000000, 0.000000000000000000, 0.000000000000000000, 0.000000000000000000, 0.000000000000000000 ) ;
#46382 = CARTESIAN_POINT ( 'NONE',  ( -0.1264236179284866091, -0.03494094482812625663, 0.1264236179284866091 ) ) ;
#46383 = CARTESIAN_POINT ( 'NONE',  ( 0.7185039370078739607, 1.928577636452523993E-17, 0.7381889763779527769 ) ) ;
#46384 = B_SPLINE_CURVE_WITH_KNOTS ( 'NONE', 3,
 ( #10073, #35258, #24929, #6461, #3102, #39749, #24688, #28071, #21078, #39286, #9843, #35717, #36196, #47204, #39052, #2853, #32377, #39522, #6938, #6222, #21560, #20846 ),
 .UNSPECIFIED., .F., .F.,
 ( 4, 2, 2, 2, 2, 2, 2, 2, 2, 2, 4 ),
 ( 0.000000000000000000, 0.1249999999999998890, 0.1874999999999999167, 0.2187499999999999167, 0.2499999999999999445, 0.4999999999999994449, 0.6249999999999992228, 0.6874999999999991118, 0.7187499999999990008, 0.7499999999999990008, 1.000000000000000000 ),
 .UNSPECIFIED. ) ;
#46385 = ORIENTED_EDGE ( 'NONE', *, *, #6602, .F. ) ;
#46386 = CARTESIAN_POINT ( 'NONE',  ( 0.7185039370078746268, -0.06523048226347956391, 0.5044291338582675976 ) ) ;
#46387 = LINE ( 'NONE', #20046, #14654 ) ;
#46388 = ORIENTED_EDGE ( 'NONE', *, *, #7247, .T. ) ;
#46389 = CARTESIAN_POINT ( 'NONE',  ( -1.054774247047244096, 0.000000000000000000, 1.400098425143086800 ) ) ;
#46391 = CARTESIAN_POINT ( 'NONE',  ( 0.1264236179284866091, -1.762303149552535642, 0.1264236179284866091 ) ) ;
#46390 = CARTESIAN_POINT ( 'NONE',  ( -0.1574803149606297803, -0.4089566928058585571, 0.06523048226347956391 ) ) ;
#46392 = CARTESIAN_POINT ( 'NONE',  ( -0.7495606340400177148, -0.1264236179284866091, 0.9571850393163149340 ) ) ;
#46393 = CARTESIAN_POINT ( 'NONE',  ( -0.8019270111902717657, 0.1787899950787401604, 1.963582677111591401 ) ) ;
#46394 = EDGE_LOOP ( 'NONE', ( #5605, #30728, #17095, #18226 ) ) ;
#46395 = CARTESIAN_POINT ( 'NONE',  ( -0.8759842519685039353, 0.1787899950787401882, 1.055610236166708793 ) ) ;
#46396 = CARTESIAN_POINT ( 'NONE',  ( -1.002407869896990045, -0.1264236179284866091, 0.6914370078202519698 ) ) ;
#46397 = ADVANCED_FACE ( 'NONE', ( #42906 ), #35528, .T. ) ;
#46398 = CARTESIAN_POINT ( 'NONE',  ( -0.1377952755905511861, 1.808041534174241898E-17, -0.1712639279175142137 ) ) ;
#46399 = VERTEX_POINT ( 'NONE', #1732 ) ;
#46400 = CARTESIAN_POINT ( 'NONE',  ( -0.7185039370078739607, 1.928577636452523993E-17, 0.06889763779527559306 ) ) ;
#46401 = CARTESIAN_POINT ( 'NONE',  ( 0.6141732283464567121, 0.000000000000000000, 0.08090551181102362266 ) ) ;
#46402 = VERTEX_POINT ( 'NONE', #9650 ) ;
#46403 = CARTESIAN_POINT ( 'NONE',  ( -0.9873396505805591694, -0.1113553986120547346, 0.3494094487113705294 ) ) ;
#46404 = CARTESIAN_POINT ( 'NONE',  ( -1.002407869896990045, 0.1264236179284866091, 0.6176181101824566033 ) ) ;
#46405 = ORIENTED_EDGE ( 'NONE', *, *, #34779, .F. ) ;
#46406 = CARTESIAN_POINT ( 'NONE',  ( -0.9500414927467377701, -0.1787899950787401604, 1.633858267662771091 ) ) ;
#46407 = LINE ( 'NONE', #9537, #16502 ) ;
#46408 = EDGE_CURVE ( 'NONE', #44045, #36569, #38161, .T. ) ;
#46409 = CARTESIAN_POINT ( 'NONE',  ( -0.8759842519685039353, 0.1574803149606299191, 0.4921259842519685179 ) ) ;
#46410 = ORIENTED_EDGE ( 'NONE', *, *, #36744, .T. ) ;
#46411 = CARTESIAN_POINT ( 'NONE',  ( 0.1270800023317771588, -0.6949256993468247989, 0.1270800023317771588 ) ) ;
#46412 = CARTESIAN_POINT ( 'NONE',  ( 0.2471922904502826257, 0.09379707428445177575, 0.03645092102367950004 ) ) ;
#46413 = CARTESIAN_POINT ( 'NONE',  ( -0.7185039370078746268, 0.06523048226347956391, 1.395177165246804130 ) ) ;
#46414 = CARTESIAN_POINT ( 'NONE',  ( 0.8019270111902717657, 0.1787899950787401604, 0.6692913385289144257 ) ) ;
#46415 = CARTESIAN_POINT ( 'NONE',  ( 0.1574803149606299191, -0.5590551181102362266, -1.928577636452523993E-17 ) ) ;
#46416 = DIRECTION ( 'NONE',  ( -1.000000000000000000, 0.000000000000000000, 0.000000000000000000 ) ) ;
#46417 = ORIENTED_EDGE ( 'NONE', *, *, #42281, .T. ) ;
#46418 = CARTESIAN_POINT ( 'NONE',  ( 0.8107537697050254399, 0.1574803149606300301, 0.1697834644594022058 ) ) ;
#46419 = ADVANCED_FACE ( 'NONE', ( #42211 ), #26194, .T. ) ;
#46420 = CARTESIAN_POINT ( 'NONE',  ( 0.9412147342319837628, 0.1574803149606300301, 1.316437007874015519 ) ) ;
#46422 = CARTESIAN_POINT ( 'NONE',  ( -0.8759842519685039353, -0.1574803149606299191, 1.338582677165354395 ) ) ;
#46421 = DIRECTION ( 'NONE',  ( -0.000000000000000000, 0.000000000000000000, -1.000000000000000000 ) ) ;
#46423 = CARTESIAN_POINT ( 'NONE',  ( 0.9873396505805591694, -0.1113553986120547346, 1.855314960629921295 ) ) ;
#46424 = CARTESIAN_POINT ( 'NONE',  ( -0.1574803149606297803, -0.6058070865066461641, 0.06523048226347956391 ) ) ;
#46426 = FACE_OUTER_BOUND ( 'NONE', #18644, .T. ) ;
#46425 = CARTESIAN_POINT ( 'NONE',  ( 1.054774247047244540, 0.07405724077823318263, 0.6545275590013546196 ) ) ;
#46427 = ORIENTED_EDGE ( 'NONE', *, *, #2320, .F. ) ;
#46428 = CARTESIAN_POINT ( 'NONE',  ( 0.1429759811007342563, 0.1299212598425197041, 0.1098622232965498907 ) ) ;
#46429 = CARTESIAN_POINT ( 'NONE',  ( 0.008396861977877295019, 0.08632935120539782237, -0.1260637287088791914 ) ) ;
#46430 = CARTESIAN_POINT ( 'NONE',  ( 0.9500414927467378812, 0.1787899950787401604, 0.7775590550643479704 ) ) ;
#46431 = CARTESIAN_POINT ( 'NONE',  ( 0.000000000000000000, 0.1102362204724409434, -0.2204724409448818867 ) ) ;
#46432 = CARTESIAN_POINT ( 'NONE',  ( -0.1787899950787401882, -1.811515747977732405, 0.000000000000000000 ) ) ;
#46433 = CARTESIAN_POINT ( 'NONE',  ( -0.1264236179284866091, -1.024114173174582643, 0.1264236179284866091 ) ) ;
#46434 = CARTESIAN_POINT ( 'NONE',  ( -0.1113553986120547346, -1.479330708661417360, 0.1113553986120547346 ) ) ;
#46435 = CARTESIAN_POINT ( 'NONE',  ( 0.7185039370078739607, 1.928577636452523993E-17, 1.240157480207432883 ) ) ;
#46436 = DIRECTION ( 'NONE',  ( -0.000000000000000000, 1.000000000000000000, -0.000000000000000000 ) ) ;
#46437 = UNCERTAINTY_MEASURE_WITH_UNIT (LENGTH_MEASURE( 1.000000000000000082E-05 ), #34333, 'distance_accuracy_value', 'NONE') ;
#46438 = ORIENTED_EDGE ( 'NONE', *, *, #5744, .F. ) ;
#46439 = CARTESIAN_POINT ( 'NONE',  ( -0.9500414927467378812, -0.1787899950787401604, 1.909448818843873186 ) ) ;
#46440 = CYLINDRICAL_SURFACE ( 'NONE', #25227, 0.1574803149606299191 ) ;
#46441 = ORIENTED_EDGE ( 'NONE', *, *, #20710, .T. ) ;
#46442 = CARTESIAN_POINT ( 'NONE',  ( -0.1574803149606299191, -1.435039369971212508, 0.000000000000000000 ) ) ;
#46443 = CARTESIAN_POINT ( 'NONE',  ( -0.8019270111902716547, 0.1787899950787401604, 1.889763779473794481 ) ) ;
#46444 = CARTESIAN_POINT ( 'NONE',  ( -0.9500414927467378812, -0.1787899950787401604, 1.589566929080094448 ) ) ;
#46445 = DIRECTION ( 'NONE',  ( 0.000000000000000000, -1.000000000000000000, 0.000000000000000000 ) ) ;
#46446 = CARTESIAN_POINT ( 'NONE',  ( -1.054774247047244540, -0.07405724077823318263, 1.003937007820251193 ) ) ;
#46447 = CARTESIAN_POINT ( 'NONE',  ( -0.8759842519685039353, 0.1787899950787401882, 0.1943897637257641919 ) ) ;
#46448 = CARTESIAN_POINT ( 'NONE',  ( -0.2471922904502826257, 0.07780974138651210181, 0.07762775726530198039 ) ) ;
#46449 = CARTESIAN_POINT ( 'NONE',  ( -0.8019270111902717657, 0.1787899950787401604, 1.929133858213952335 ) ) ;
#46450 = CARTESIAN_POINT ( 'NONE',  ( -1.033464566929134687, -0.06523048226347956391, 1.936515748031494955 ) ) ;
#46451 = CARTESIAN_POINT ( 'NONE',  ( 0.2559055128465877460, 0.08195185539867717861, -0.05482843030950571711 ) ) ;
#46452 = CARTESIAN_POINT ( 'NONE',  ( -0.1264236179284866091, -0.2870334170481366187, 0.1264236179284866091 ) ) ;
#46453 = CARTESIAN_POINT ( 'NONE',  ( 0.1430309448599517697, -0.09842519685039370636, -0.1381503230155334827 ) ) ;
#46454 = CARTESIAN_POINT ( 'NONE',  ( -0.7185039370078739607, 1.928577636452523993E-17, 0.7283464565853858819 ) ) ;
#46455 = DIRECTION ( 'NONE',  ( 1.000000000000000000, -3.469446951953613794E-15, -0.000000000000000000 ) ) ;
#46456 = CIRCLE ( 'NONE', #38814, 0.1377952755905513804 ) ;
#46457 = CARTESIAN_POINT ( 'NONE',  ( -1.002407869896990045, 0.1264236179284866091, 0.2239173227808822775 ) ) ;
#46458 = ORIENTED_EDGE ( 'NONE', *, *, #46956, .T. ) ;
#46459 = EDGE_CURVE ( 'NONE', #9934, #9904, #5810, .T. ) ;
#46460 = CARTESIAN_POINT ( 'NONE',  ( -0.8759842519685039353, 0.1787899950787401882, 1.257381889710015743 ) ) ;
#46461 = ORIENTED_EDGE ( 'NONE', *, *, #33087, .F. ) ;
#46462 = CARTESIAN_POINT ( 'NONE',  ( 0.07405724077823318263, -1.120078740103715997, -0.1787899950787401604 ) ) ;
#46463 = CARTESIAN_POINT ( 'NONE',  ( -1.094772975963752103E-17, -1.230807086560409269, -0.1787899950787401882 ) ) ;
#46464 = DIRECTION ( 'NONE',  ( 0.000000000000000000, 0.000000000000000000, 1.000000000000000000 ) ) ;
#46465 = LENGTH_MEASURE_WITH_UNIT ( LENGTH_MEASURE( 0.02539999999999999897 ), #45998 ) ;
#46466 = CARTESIAN_POINT ( 'NONE',  ( -0.1797182628040039087, -0.5546697938350136914, -0.07444174185955065859 ) ) ;
#46467 = CARTESIAN_POINT ( 'NONE',  ( -0.7185039370078746268, -0.06523048226347956391, 0.2288385826771655862 ) ) ;
#46468 = CARTESIAN_POINT ( 'NONE',  ( -1.033464566929134687, 0.06523048226347956391, 0.9079724408373542888 ) ) ;
#46469 = CARTESIAN_POINT ( 'NONE',  ( -0.9873396505805591694, -0.1113553986120547346, 0.7529527559055118058 ) ) ;
#46470 = CARTESIAN_POINT ( 'NONE',  ( -0.06523048226347956391, -0.1530511811023622937, -0.1574803149606300301 ) ) ;
#46471 = EDGE_LOOP ( 'NONE', ( #29096, #17028, #26210, #43281 ) ) ;
#46472 = CARTESIAN_POINT ( 'NONE',  ( 0.8759842519685039353, 0.1574803149606299191, 1.860236220364913207 ) ) ;
#46473 = EDGE_CURVE ( 'NONE', #35175, #35809, #9325, .T. ) ;
#46474 = CARTESIAN_POINT ( 'NONE',  ( 0.7646288533564489232, 0.1113553986120547346, 0.7726377952755906220 ) ) ;
#46475 = CARTESIAN_POINT ( 'NONE',  ( 0.09162190804155555257, -0.2425962989909497547, -0.03472289316814022170 ) ) ;
#46476 = CARTESIAN_POINT ( 'NONE',  ( -9.642888182262618425E-18, -0.07677165354330708902, -0.1574803149606299191 ) ) ;
#46477 = EDGE_CURVE ( 'NONE', #18563, #46176, #31464, .T. ) ;
#46479 = DIRECTION ( 'NONE',  ( 0.000000000000000000, 1.000000000000000000, 0.000000000000000000 ) ) ;
#46478 = CARTESIAN_POINT ( 'NONE',  ( -0.2834390116245509850, 0.3740157480314960647, 1.380828817464277991 ) ) ;
#46480 = CARTESIAN_POINT ( 'NONE',  ( 0.8107537697050254399, -0.1574803149606297803, 1.090059055010582423 ) ) ;
#46481 = CARTESIAN_POINT ( 'NONE',  ( 0.7646288533564489232, -0.1113553986120547346, 0.1820866140657015630 ) ) ;
#46482 = ORIENTED_EDGE ( 'NONE', *, *, #38636, .F. ) ;
#46483 = CARTESIAN_POINT ( 'NONE',  ( -0.2066929133858267931, 0.07021257666614935666, -0.1553045758542782318 ) ) ;
#46484 = CARTESIAN_POINT ( 'NONE',  ( 0.1264236179284866091, -0.6107283464029291675, -0.1264236179284866091 ) ) ;
#46486 = CIRCLE ( 'NONE', #33500, 0.1377952755905510474 ) ;
#46485 = CARTESIAN_POINT ( 'NONE',  ( -0.1787899950787401604, -1.420275590497418250, -0.07405724077823318263 ) ) ;
#46487 = CARTESIAN_POINT ( 'NONE',  ( -1.054774247047244096, 0.000000000000000000, 1.911909448765133801 ) ) ;
#46488 = VERTEX_POINT ( 'NONE', #34578 ) ;
#46489 = ORIENTED_EDGE ( 'NONE', *, *, #37438, .F. ) ;
#46490 = CARTESIAN_POINT ( 'NONE',  ( -0.8019270111902717657, 0.1787899950787401604, 1.456692913332062744 ) ) ;
#46491 = ORIENTED_EDGE ( 'NONE', *, *, #5880, .T. ) ;
#46492 = CARTESIAN_POINT ( 'NONE',  ( 0.8107537697050254399, -0.1574803149606297803, 0.9325787400499523372 ) ) ;
#46493 = CARTESIAN_POINT ( 'NONE',  ( -0.1113553986120547346, -1.282480314853102321, -0.1113553986120547346 ) ) ;
#46494 = CARTESIAN_POINT ( 'NONE',  ( -1.002407869896990045, 0.1264236179284866091, 0.7012795275052913224 ) ) ;
#46495 = CARTESIAN_POINT ( 'NONE',  ( 0.7495606340400177148, 0.1264236179284866091, 0.1993110235682838682 ) ) ;
#46496 = CARTESIAN_POINT ( 'NONE',  ( 0.1585082349939047064, -0.09842394368956142170, -0.08275592341139960395 ) ) ;
#46497 = CARTESIAN_POINT ( 'NONE',  ( -1.054774247047244096, 0.000000000000000000, 0.5339566928596221063 ) ) ;
#46498 = CARTESIAN_POINT ( 'NONE',  ( 0.4208034506101054895, 0.09842519685039370636, 1.205361022782828805E-17 ) ) ;
#46499 = CARTESIAN_POINT ( 'NONE',  ( -0.7646288533564489232, -0.1113553986120547346, 0.8612204724409449064 ) ) ;
#46500 = ORIENTED_EDGE ( 'NONE', *, *, #7625, .F. ) ;
#46501 = CARTESIAN_POINT ( 'NONE',  ( -0.6971942568897637749, 2.189545951927499583E-17, 1.424704724355685181 ) ) ;
#46502 = ORIENTED_EDGE ( 'NONE', *, *, #10903, .F. ) ;
#46503 = DIRECTION ( 'NONE',  ( 1.000000000000000000, 0.000000000000000000, 0.000000000000000000 ) ) ;
#46504 = CARTESIAN_POINT ( 'NONE',  ( -0.7646288533564489232, -0.1113553986120547346, 1.491141732283464583 ) ) ;
#46505 = CARTESIAN_POINT ( 'NONE',  ( -0.7185039370078746268, -0.06523048226347956391, 0.4650590551181104093 ) ) ;
#46506 = CARTESIAN_POINT ( 'NONE',  ( 0.7495606340400177148, -0.1264236179284866091, 1.311515747977732405 ) ) ;
#46507 = CARTESIAN_POINT ( 'NONE',  ( 0.1830111034970090533, -0.09851384631394094482, 0.1095843003117216580 ) ) ;
#46508 = APPLICATION_CONTEXT ( 'automotive_design' ) ;
#46509 = VERTEX_POINT ( 'NONE', #46046 ) ;
#46510 = EDGE_CURVE ( 'NONE', #33889, #19863, #25406, .T. ) ;
#46511 = CYLINDRICAL_SURFACE ( 'NONE', #45513, 0.1574803149606299191 ) ;
#46512 = EDGE_CURVE ( 'NONE', #37122, #3623, #29254, .T. ) ;
#46513 = CIRCLE ( 'NONE', #5195, 0.1013779527559055538 ) ;
#46514 = CARTESIAN_POINT ( 'NONE',  ( 0.07405724077823318263, -1.682210582402467791, -0.1787899950787401604 ) ) ;
#46515 = CARTESIAN_POINT ( 'NONE',  ( 3.284318927891251994E-17, -0.6599409448281259305, 0.1787899950787401882 ) ) ;
#46516 = EDGE_CURVE ( 'NONE', #38506, #14850, #26949, .T. ) ;
#46517 = DIRECTION ( 'NONE',  ( 0.000000000000000000, 0.000000000000000000, 1.000000000000000000 ) ) ;
#46518 = VERTEX_POINT ( 'NONE', #43150 ) ;
#46519 = CARTESIAN_POINT ( 'NONE',  ( 1.054774247047244540, 0.07405724077823318263, 1.441929133804504604 ) ) ;
#46520 = CONICAL_SURFACE ( 'NONE', #2135, 0.1377952755905509641, 0.9599310885968941331 ) ;
#46521 = CARTESIAN_POINT ( 'NONE',  ( -0.1787899950787401604, -0.7460629920722210429, 0.07405724077823318263 ) ) ;
#46522 = CARTESIAN_POINT ( 'NONE',  ( 0.3302522695077432791, 0.09842519685039370636, 1.205361022782828805E-17 ) ) ;
#46523 = DIRECTION ( 'NONE',  ( 1.000000000000000000, -0.000000000000000000, -1.144917494144692682E-16 ) ) ;
#46524 = CARTESIAN_POINT ( 'NONE',  ( 0.9500414927467378812, -0.1787899950787401604, 1.668307086560410157 ) ) ;
#46525 = CARTESIAN_POINT ( 'NONE',  ( 1.054774247047244096, 0.000000000000000000, 0.3764763778989925203 ) ) ;
#46526 = CARTESIAN_POINT ( 'NONE',  ( -0.1264236179284866091, -0.01144286586703399666, 0.1264236179284866091 ) ) ;
#46527 = CARTESIAN_POINT ( 'NONE',  ( -0.1787899950787401604, 0.03149606304588949135, -0.07405724077823318263 ) ) ;
#46528 = CARTESIAN_POINT ( 'NONE',  ( 0.2559055118110236116, -0.07522986544523073416, -0.3087092415967106485 ) ) ;
#46529 = CARTESIAN_POINT ( 'NONE',  ( 1.054774247047244096, 0.000000000000000000, 0.5733267715997795166 ) ) ;
#46530 = ( BOUNDED_CURVE ( )  B_SPLINE_CURVE ( 2, ( #27219, #9209, #37496, #1295, #1058, #19754, #26974, #23592, #38205 ),
 .UNSPECIFIED., .F., .T. ) 
 B_SPLINE_CURVE_WITH_KNOTS ( ( 3, 2, 2, 2, 3 ),
 ( 0.9799999999999999822, 0.9825000000000000400, 0.9849999999999999867, 0.9875000000000000444, 0.9899999999999999911 ),
 .UNSPECIFIED. ) 
 CURVE ( )  GEOMETRIC_REPRESENTATION_ITEM ( )  RATIONAL_B_SPLINE_CURVE ( ( 1.000000000000000000, 0.9238795325112869605, 1.000000000000000000, 0.9238795325112869605, 1.000000000000000000, 0.9238795325112869605, 1.000000000000000000, 0.9238795325112869605, 1.000000000000000000 ) ) 
 REPRESENTATION_ITEM ( '' )  ) ;
#46531 = CARTESIAN_POINT ( 'NONE',  ( -0.9500414927467377701, 0.1787899950787401604, 0.8612204723871810241 ) ) ;
#46533 = CARTESIAN_POINT ( 'NONE',  ( 1.033464566929133799, 0.000000000000000000, 1.692913385719244213 ) ) ;
#46532 = CARTESIAN_POINT ( 'NONE',  ( -0.1574803149606297803, -0.8912401574803148208, 0.06523048226347956391 ) ) ;
#46535 = CARTESIAN_POINT ( 'NONE',  ( -0.8433719236205573511, -0.1704368056499333817, 1.987609075866120456 ) ) ;
#46534 = CARTESIAN_POINT ( 'NONE',  ( -0.1797182628040039087, -1.696402077299580702, -0.07444174185955065859 ) ) ;
#46536 = CARTESIAN_POINT ( 'NONE',  ( -0.9412147342319837628, -0.1574803149606297803, 1.252460629813731519 ) ) ;
#46538 = CARTESIAN_POINT ( 'NONE',  ( -9.642888182262618425E-18, 0.001968503937007873988, -0.1574803149606299191 ) ) ;
#46537 = CARTESIAN_POINT ( 'NONE',  ( 0.8019270111902716547, 0.1787899950787401604, 1.924212598371433325 ) ) ;
#46539 = CARTESIAN_POINT ( 'NONE',  ( 1.002407869896990045, -0.1264236179284866091, 0.4502952755367874427 ) ) ;
#46540 = ORIENTED_EDGE ( 'NONE', *, *, #29916, .T. ) ;
#46541 = ORIENTED_EDGE ( 'NONE', *, *, #8331, .T. ) ;
#46542 = CARTESIAN_POINT ( 'NONE',  ( 0.1657973489140633916, -0.1997733981812202797, -0.3128311589625492606 ) ) ;
#46543 = CARTESIAN_POINT ( 'NONE',  ( -0.07405724077823318263, -0.1161417322297011862, 0.1787899950787401604 ) ) ;
#46544 = CARTESIAN_POINT ( 'NONE',  ( 0.6971942568897637749, 2.189545951927499583E-17, 0.5930118109698583329 ) ) ;
#46545 = CARTESIAN_POINT ( 'NONE',  ( -0.1787899950787401604, -0.9478346456155283262, -0.07405724077823318263 ) ) ;
#46546 = CARTESIAN_POINT ( 'NONE',  ( 0.9500414927467378812, -0.1787899950787401604, 0.1377952755367876370 ) ) ;
#46547 = CARTESIAN_POINT ( 'NONE',  ( -0.8759842519685039353, -0.1574803149606299191, 1.525590551073574774 ) ) ;
#46548 = CYLINDRICAL_SURFACE ( 'NONE', #27361, 0.7874015748031496509 ) ;
#46549 = CARTESIAN_POINT ( 'NONE',  ( -0.9500414927467378812, -0.1787899950787401604, 1.392716535379308285 ) ) ;
#46550 = ORIENTED_EDGE ( 'NONE', *, *, #36755, .T. ) ;
#46551 = CARTESIAN_POINT ( 'NONE',  ( -0.2984771744461587328, -0.08441368980803262700, -0.7311049032655659863 ) ) ;
#46552 = CARTESIAN_POINT ( 'NONE',  ( 0.9500414927467378812, 0.1787899950787401604, 1.215551181048599272 ) ) ;
#46553 = CARTESIAN_POINT ( 'NONE',  ( -0.7185039370078739607, 1.928577636452523993E-17, 0.7283464565853858819 ) ) ;
#46554 = CARTESIAN_POINT ( 'NONE',  ( 0.7495606340400177148, 0.1264236179284866091, 1.808562992072220377 ) ) ;
#46555 = CARTESIAN_POINT ( 'NONE',  ( -0.7646288533564489232, -0.1113553986120547346, 1.373031496062992352 ) ) ;
#46556 = CARTESIAN_POINT ( 'NONE',  ( -0.8759842519685039353, -0.1787899950787401882, 0.9571850393163149340 ) ) ;
#46557 = DIRECTION ( 'NONE',  ( 3.469446951953614583E-15, 1.000000000000000000, 0.000000000000000000 ) ) ;
#46558 = DIRECTION ( 'NONE',  ( -0.5735764363510518216, 0.8191520442889876907, 1.003171929053519693E-16 ) ) ;
#46559 = CARTESIAN_POINT ( 'NONE',  ( 0.9500414927467377701, -0.1787899950787401604, 0.1771653542769452416 ) ) ;
#46560 = CARTESIAN_POINT ( 'NONE',  ( -0.6971942568897626646, 0.07405724077823318263, 0.07874015742655143812 ) ) ;
#46561 = CARTESIAN_POINT ( 'NONE',  ( 0.8759842519685039353, -0.1574803149606299191, 1.643700787294047228 ) ) ;
#46562 = EDGE_LOOP ( 'NONE', ( #31926, #32829 ) ) ;
#46563 = VECTOR ( 'NONE', #25683, 39.37007874015748143 ) ;
#46564 = ( BOUNDED_CURVE ( )  B_SPLINE_CURVE ( 2, ( #29541, #11288, #40710, #22283, #7910, #4291, #32401, #46977, #14170 ),
 .UNSPECIFIED., .F., .T. ) 
 B_SPLINE_CURVE_WITH_KNOTS ( ( 3, 2, 2, 2, 3 ),
 ( 0.4400000000000000022, 0.4425000000000000044, 0.4450000000000000067, 0.4475000000000000089, 0.4500000000000000111 ),
 .UNSPECIFIED. ) 
 CURVE ( )  GEOMETRIC_REPRESENTATION_ITEM ( )  RATIONAL_B_SPLINE_CURVE ( ( 1.000000000000000000, 0.9238795325112869605, 1.000000000000000000, 0.9238795325112869605, 1.000000000000000000, 0.9238795325112869605, 1.000000000000000000, 0.9238795325112869605, 1.000000000000000000 ) ) 
 REPRESENTATION_ITEM ( '' )  ) ;
#46565 = CARTESIAN_POINT ( 'NONE',  ( -0.1787899950787401604, 0.1151574803687242243, 0.07405724077823318263 ) ) ;
#46566 = ORIENTED_EDGE ( 'NONE', *, *, #36802, .T. ) ;
#46567 = CARTESIAN_POINT ( 'NONE',  ( 1.054774247047244540, -0.07405724077823318263, 0.7726377952218265177 ) ) ;
#46568 = CARTESIAN_POINT ( 'NONE',  ( -0.6971942568897648851, -0.07405724077823297447, 1.697834645615527771 ) ) ;
#46569 = ADVANCED_FACE ( 'NONE', ( #10360 ), #3625, .T. ) ;
#46570 = CARTESIAN_POINT ( 'NONE',  ( 0.1787899950787401882, -1.476870078686393750, -2.189545951927503898E-17 ) ) ;
#46571 = EDGE_CURVE ( 'NONE', #21208, #33536, #13169, .T. ) ;
#46572 = CYLINDRICAL_SURFACE ( 'NONE', #11549, 0.1574803149606299191 ) ;
#46573 = CARTESIAN_POINT ( 'NONE',  ( -0.4330708661417343452, 3.105646754637359143E-15, 1.186023622047244430 ) ) ;
#46574 = CARTESIAN_POINT ( 'NONE',  ( -0.07405724077823318263, -1.204848377678058524, -0.1787899950787401604 ) ) ;
#46575 = VERTEX_POINT ( 'NONE', #25455 ) ;
#46576 = CARTESIAN_POINT ( 'NONE',  ( 0.07405724077823318263, -0.09153543301710270752, -0.1787899950787401604 ) ) ;
#46577 = EDGE_CURVE ( 'NONE', #44293, #529, #18244, .T. ) ;
#46578 = VERTEX_POINT ( 'NONE', #10603 ) ;
#46579 = CARTESIAN_POINT ( 'NONE',  ( 0.8019270111902717657, -0.1787899950787401604, 1.072834645615528659 ) ) ;
#46580 = EDGE_CURVE ( 'NONE', #5491, #33815, #47239, .T. ) ;
#46581 = CARTESIAN_POINT ( 'NONE',  ( 0.1377952755905509363, 1.687505431895956106E-17, -0.1045766232635885612 ) ) ;
#46582 = CARTESIAN_POINT ( 'NONE',  ( -0.7185039370078746268, -0.06523048226347956391, 0.4158464565853863260 ) ) ;
#46583 = VECTOR ( 'NONE', #18786, 39.37007874015748854 ) ;
#46584 = CARTESIAN_POINT ( 'NONE',  ( 0.6971942568897626646, -0.07405724077823297447, 0.04429133852891373180 ) ) ;
#46585 = CARTESIAN_POINT ( 'NONE',  ( 0.1264236179284866091, -1.555610236166708571, -0.1264236179284866091 ) ) ;
#46586 = EDGE_LOOP ( 'NONE', ( #44443, #12844, #2027, #33750 ) ) ;
#46587 = AXIS2_PLACEMENT_3D ( 'NONE', #39199, #9990, #21232 ) ;
#46588 = CARTESIAN_POINT ( 'NONE',  ( -0.9500414927467377701, 0.1787899950787401604, 0.3100393700249766682 ) ) ;
#46589 = CARTESIAN_POINT ( 'NONE',  ( -0.1751023000383840345, 0.1943988721995235924, -0.03960523631940795347 ) ) ;
#46590 = CARTESIAN_POINT ( 'NONE',  ( 0.8759842519685039353, -0.1787899950787401882, 1.158956692859621995 ) ) ;
#46591 = VECTOR ( 'NONE', #22209, 39.37007874015748143 ) ;
#46592 = CARTESIAN_POINT ( 'NONE',  ( 0.9500414927467377701, -0.1787899950787401604, 1.550196850339938148 ) ) ;
#46593 = CARTESIAN_POINT ( 'NONE',  ( -0.3690944881889767215, 5.424056872940433071E-15, 0.7480314960629921295 ) ) ;
#46595 = CARTESIAN_POINT ( 'NONE',  ( -0.7185039370078739607, 1.928577636452523993E-17, 1.240157480207432883 ) ) ;
#46594 = CARTESIAN_POINT ( 'NONE',  ( 0.7646288533564489232, -0.1113553986120547346, 0.8907480313885355327 ) ) ;
#46596 = CYLINDRICAL_SURFACE ( 'NONE', #22850, 0.04921259842519686706 ) ;
#46597 = CARTESIAN_POINT ( 'NONE',  ( 2.892866454678787531E-17, -0.7559055117034961802, 0.1574803149606299191 ) ) ;
#46598 = CARTESIAN_POINT ( 'NONE',  ( -0.8759842519685039353, 0.1574803149606299191, 1.663385826664125933 ) ) ;
#46599 = CARTESIAN_POINT ( 'NONE',  ( 0.07405724077823318263, 0.01181102367581074800, 0.1787899950787401604 ) ) ;
#46600 = CARTESIAN_POINT ( 'NONE',  ( 0.7495606340400177148, -0.1264236179284866091, 0.2042322834108035723 ) ) ;
#46601 = DIRECTION ( 'NONE',  ( 0.000000000000000000, 0.6156614753256632877, 0.7880107536067181284 ) ) ;
#46603 = FACE_OUTER_BOUND ( 'NONE', #37293, .T. ) ;
#46602 = CARTESIAN_POINT ( 'NONE',  ( 0.9500414927467377701, 0.1787899950787401604, 1.092519684985606032 ) ) ;
#46604 = CARTESIAN_POINT ( 'NONE',  ( 0.1574803149606299191, 0.000000000000000000, -0.2748405511811023438 ) ) ;
#46605 = CARTESIAN_POINT ( 'NONE',  ( 0.9873396505805591694, -0.1113553986120547346, 0.4281496061916850726 ) ) ;
#46606 = EDGE_LOOP ( 'NONE', ( #2665, #10565, #40814, #29351, #39111, #24670, #26034, #2238 ) ) ;
#46607 = CARTESIAN_POINT ( 'NONE',  ( -0.9412147342319837628, 0.1574803149606300301, 1.119586614173229577 ) ) ;
#46608 = CARTESIAN_POINT ( 'NONE',  ( 1.020804986503725420, 0.07407192766898883229, 0.03937343678672019370 ) ) ;
#46609 = VERTEX_POINT ( 'NONE', #46755 ) ;
#46610 = CARTESIAN_POINT ( 'NONE',  ( 1.002407869896990045, 0.1264236179284866091, 1.483759842465921075 ) ) ;
#46611 = DIRECTION ( 'NONE',  ( 0.3420201433256624401, 0.000000000000000000, -0.9396926207859106484 ) ) ;
#46612 = EDGE_CURVE ( 'NONE', #42489, #41232, #21604, .T. ) ;
#46613 = CARTESIAN_POINT ( 'NONE',  ( -0.1787899950787401604, 0.001968503990771383692, 0.07405724077823318263 ) ) ;
#46614 = VERTEX_POINT ( 'NONE', #18001 ) ;
#46615 = CARTESIAN_POINT ( 'NONE',  ( 0.7646288533564489232, 0.1113553986120547346, 0.7332677165354331006 ) ) ;
#46616 = CIRCLE ( 'NONE', #1451, 0.009842519685039369942 ) ;
#46617 = ORIENTED_EDGE ( 'NONE', *, *, #31942, .T. ) ;
#46618 = CARTESIAN_POINT ( 'NONE',  ( 0.9873396505805591694, -0.1113553986120547346, 0.5167322834645668994 ) ) ;
#46619 = CARTESIAN_POINT ( 'NONE',  ( -1.033464566929133799, 1.928577636452524610E-17, 2.869337061179095023E-17 ) ) ;
#46620 = CARTESIAN_POINT ( 'NONE',  ( 1.054774247047244096, 0.000000000000000000, 0.4995078739619842612 ) ) ;
#46621 = ORIENTED_EDGE ( 'NONE', *, *, #17964, .F. ) ;
#46622 = CARTESIAN_POINT ( 'NONE',  ( -0.6971942568897637749, 2.189545951927499583E-17, 1.419783464513165505 ) ) ;
#46623 = CARTESIAN_POINT ( 'NONE',  ( 0.1787899950787401604, -1.676181102308441639, -0.07405724077823318263 ) ) ;
#46624 = CARTESIAN_POINT ( 'NONE',  ( -0.8759842519685039353, 0.1787899950787401882, 1.099901574749385880 ) ) ;
#46625 = CARTESIAN_POINT ( 'NONE',  ( -0.7646288533564489232, -0.1113553986120547346, 0.03444881889763779653 ) ) ;
#46626 = CARTESIAN_POINT ( 'NONE',  ( -1.054774247047244096, 0.000000000000000000, 1.045767716481669440 ) ) ;
#46627 = CIRCLE ( 'NONE', #3773, 0.1003937007874011050 ) ;
#46628 = CARTESIAN_POINT ( 'NONE',  ( -0.9500414927467378812, -0.1787899950787401604, 0.8464566928596233275 ) ) ;
#46629 = EDGE_CURVE ( 'NONE', #33076, #36685, #13942, .T. ) ;
#46630 = CYLINDRICAL_SURFACE ( 'NONE', #19817, 0.1574803149606299191 ) ;
#46631 = CARTESIAN_POINT ( 'NONE',  ( -0.1787899950787401882, -0.7250255430323878647, 0.000000000000000000 ) ) ;
#46632 = ORIENTED_EDGE ( 'NONE', *, *, #35034, .T. ) ;
#46633 = CARTESIAN_POINT ( 'NONE',  ( -0.1570894919835442993, -0.08956159021719448110, 0.05351830911520212564 ) ) ;
#46634 = CONICAL_SURFACE ( 'NONE', #42034, 0.08090551181102362266, 0.9599310885968742602 ) ;
#46635 = CARTESIAN_POINT ( 'NONE',  ( 0.2559055118110236116, 0.1477471161312045311, -0.2921040715117803055 ) ) ;
#46636 = EDGE_CURVE ( 'NONE', #32133, #7349, #2891, .T. ) ;
#46637 = CARTESIAN_POINT ( 'NONE',  ( -1.033464566929133799, 0.000000000000000000, 1.692913385719244213 ) ) ;
#46638 = CARTESIAN_POINT ( 'NONE',  ( -0.6971942568897626646, 0.07405724077823318263, 0.5905511810485987167 ) ) ;
#46639 = DIRECTION ( 'NONE',  ( 1.000000000000000000, -5.411399086424350389E-15, 4.275490733183370330E-15 ) ) ;
#46640 = ORIENTED_EDGE ( 'NONE', *, *, #31033, .F. ) ;
#46641 = CARTESIAN_POINT ( 'NONE',  ( -0.9500414927467377701, 0.1787899950787401604, 1.609251968450173598 ) ) ;
#46642 = DIRECTION ( 'NONE',  ( -1.000000000000000000, 3.469446951953626022E-15, 0.000000000000000000 ) ) ;
#46643 = AXIS2_PLACEMENT_3D ( 'NONE', #44078, #25888, #29044 ) ;
#46644 = EDGE_LOOP ( 'NONE', ( #11525, #41136, #17825, #29195 ) ) ;
#46645 = CARTESIAN_POINT ( 'NONE',  ( -0.1797182628040039365, -0.7884296363546987596, 0.000000000000000000 ) ) ;
#46646 = FACE_BOUND ( 'NONE', #29230, .T. ) ;
#46647 = CARTESIAN_POINT ( 'NONE',  ( -0.8107537697050253289, 0.1574803149606300301, 1.390255905404285119 ) ) ;
#46648 = CARTESIAN_POINT ( 'NONE',  ( 0.8759842519685039353, -0.1787899950787401882, 0.6865157479777322935 ) ) ;
#46649 = CARTESIAN_POINT ( 'NONE',  ( 0.06523048226347956391, -0.5516732283464562681, -0.1574803149606300301 ) ) ;
#46650 = CARTESIAN_POINT ( 'NONE',  ( 0.7646288533564489232, 0.1113553986120547346, 1.628937007766488199 ) ) ;
#46651 = VERTEX_POINT ( 'NONE', #32655 ) ;
#46652 = CARTESIAN_POINT ( 'NONE',  ( -0.2559055118110236116, 0.1477471161312031434, -0.1122047244094468571 ) ) ;
#46653 = CARTESIAN_POINT ( 'NONE',  ( 1.033464566929134687, 0.06523048226347956391, 1.311515748031496509 ) ) ;
#46655 = CARTESIAN_POINT ( 'NONE',  ( -1.033464566929133799, 0.000000000000000000, 1.348425196850393748 ) ) ;
#46654 = DIRECTION ( 'NONE',  ( -1.000000000000000000, 0.000000000000000000, 0.000000000000000000 ) ) ;
#46656 = AXIS2_PLACEMENT_3D ( 'NONE', #32402, #39307, #3612 ) ;
#46657 = DIRECTION ( 'NONE',  ( -1.000000000000000000, 0.000000000000000000, 0.000000000000000000 ) ) ;
#46658 = EDGE_CURVE ( 'NONE', #18113, #43974, #29276, .T. ) ;
#46660 = CARTESIAN_POINT ( 'NONE',  ( 0.7185039370078746268, -0.06523048226347956391, 0.2583661416247562959 ) ) ;
#46659 = CARTESIAN_POINT ( 'NONE',  ( 1.054774247047244096, 0.000000000000000000, 0.7308070865604093802 ) ) ;
#46661 = LINE ( 'NONE', #17438, #27754 ) ;
#46662 = ORIENTED_EDGE ( 'NONE', *, *, #46658, .T. ) ;
#46663 = CARTESIAN_POINT ( 'NONE',  ( -0.7185039370078739607, 0.000000000000000000, -2.869337061179095023E-17 ) ) ;
#46664 = DIRECTION ( 'NONE',  ( 1.000000000000000000, -0.000000000000000000, -0.000000000000000000 ) ) ;
#46665 = CARTESIAN_POINT ( 'NONE',  ( 0.6971942568897626646, 0.07405724077823318263, 0.7874015747493863238 ) ) ;
#46666 = CARTESIAN_POINT ( 'NONE',  ( 0.000000000000000000, 0.000000000000000000, -1.181102362204724310 ) ) ;
#46667 = CYLINDRICAL_SURFACE ( 'NONE', #35021, 0.1574803149606299191 ) ;
#46668 = CARTESIAN_POINT ( 'NONE',  ( -0.1797182628040039087, 0.07525146600750569348, -0.07444174185955065859 ) ) ;
#46669 = CARTESIAN_POINT ( 'NONE',  ( -0.07405724077823318263, -1.061023621993481214, 0.1787899950787401604 ) ) ;
#46670 = CARTESIAN_POINT ( 'NONE',  ( 0.1574803149606300301, -1.580216535433071723, -0.06523048226347956391 ) ) ;
#46671 = CARTESIAN_POINT ( 'NONE',  ( 1.033464566929134687, 0.06523048226347956391, 1.232775590551180134 ) ) ;
#46672 = CARTESIAN_POINT ( 'NONE',  ( -0.8019270111902717657, -0.1787899950787401604, 0.08858267711159097113 ) ) ;
#46673 = ORIENTED_EDGE ( 'NONE', *, *, #26986, .T. ) ;
#46674 = CARTESIAN_POINT ( 'NONE',  ( 0.6971942568897648851, 0.07405724077823318263, 1.973425196796630088 ) ) ;
#46675 = ORIENTED_EDGE ( 'NONE', *, *, #35064, .F. ) ;
#46676 = CARTESIAN_POINT ( 'NONE',  ( 0.7495606340400177148, 0.1264236179284866091, 0.8292322834108031282 ) ) ;
#46677 = EDGE_CURVE ( 'NONE', #37257, #25961, #33074, .T. ) ;
#46678 = CARTESIAN_POINT ( 'NONE',  ( -1.054774247047244096, 0.000000000000000000, 0.2632874015210397434 ) ) ;
#46679 = ADVANCED_FACE ( 'NONE', ( #11075 ), #40263, .T. ) ;
#46680 = AXIS2_PLACEMENT_3D ( 'NONE', #13617, #28258, #42818 ) ;
#46681 = CARTESIAN_POINT ( 'NONE',  ( 0.2362204724409448509, 0.1574803149606299191, 1.186023622047243986 ) ) ;
#46682 = CARTESIAN_POINT ( 'NONE',  ( -1.054774247047244540, 0.07405724077823318263, 1.840551181048599938 ) ) ;
#46683 = CARTESIAN_POINT ( 'NONE',  ( 0.9412147342319837628, 0.1574803149606300301, 0.2928149606299214613 ) ) ;
#46684 = CARTESIAN_POINT ( 'NONE',  ( -0.7185039370078746268, -0.06523048226347956391, 1.882381889763779181 ) ) ;
#46685 = CARTESIAN_POINT ( 'NONE',  ( 0.2759478392031606275, -0.09842519685039370636, 1.555605046820498050 ) ) ;
#46686 = ITEM_DEFINED_TRANSFORMATION ( 'NONE', 'NONE', #46932,  #20860 ) ;
#46687 = CARTESIAN_POINT ( 'NONE',  ( 0.7185039370078739607, 1.928577636452523993E-17, 1.358267716427907779 ) ) ;
#46688 = CARTESIAN_POINT ( 'NONE',  ( -0.7185039370078739607, 1.928577636452523993E-17, 0.05905511800270921846 ) ) ;
#46689 = PRODUCT_DEFINITION_SHAPE ( 'NONE', 'NONE',  #47472 ) ;
#46690 = AXIS2_PLACEMENT_3D ( 'NONE', #39494, #25383, #6432 ) ;
#46691 = CARTESIAN_POINT ( 'NONE',  ( -0.9500414927467378812, 0.1787899950787401604, 0.2263779527021421711 ) ) ;
#46692 = ORIENTED_EDGE ( 'NONE', *, *, #10359, .T. ) ;
#46693 = CARTESIAN_POINT ( 'NONE',  ( -1.054774247047244540, 0.07405724077823318263, 1.210629921206079818 ) ) ;
#46694 = EDGE_LOOP ( 'NONE', ( #45487, #5443, #14297, #23573 ) ) ;
#46695 = CARTESIAN_POINT ( 'NONE',  ( 3.284318927891251994E-17, -1.255413385773007873, 0.1787899950787401882 ) ) ;
#46696 = CARTESIAN_POINT ( 'NONE',  ( -0.1264236179284866091, -1.452263779473795369, 0.1264236179284866091 ) ) ;
#46697 = CARTESIAN_POINT ( 'NONE',  ( 0.000000000000000000, 0.09842519685039370636, 0.000000000000000000 ) ) ;
#46698 = CARTESIAN_POINT ( 'NONE',  ( -0.07444174185955065859, -0.6383312111578482995, -0.1797182628040039087 ) ) ;
#46699 = CARTESIAN_POINT ( 'NONE',  ( 0.1574803149606299746, 0.1473293504822046074, -0.9532488779249699284 ) ) ;
#46700 = CARTESIAN_POINT ( 'NONE',  ( -0.9412147342319837628, 0.1574803149606300301, 0.9128937006798734100 ) ) ;
#46701 = CARTESIAN_POINT ( 'NONE',  ( -0.8759842519685039353, -0.1574803149606299191, 0.6692913385826771977 ) ) ;
#46702 = CARTESIAN_POINT ( 'NONE',  ( 0.1113553986120547346, -0.2096456692913385711, 0.1113553986120547346 ) ) ;
#46703 = CARTESIAN_POINT ( 'NONE',  ( 0.7646288533564489232, -0.1113553986120547346, 1.874999999892472458 ) ) ;
#46704 = ORIENTED_EDGE ( 'NONE', *, *, #14961, .F. ) ;
#46705 = CARTESIAN_POINT ( 'NONE',  ( 1.033464566929134687, -0.06523048226347956391, 0.2337598424121580809 ) ) ;
#46706 = CARTESIAN_POINT ( 'NONE',  ( 0.9412147342319837628, 0.1574803149606300301, 0.7652559055118115516 ) ) ;
#46707 = CYLINDRICAL_SURFACE ( 'NONE', #12280, 0.1377952755905509086 ) ;
#46708 = CARTESIAN_POINT ( 'NONE',  ( 0.06801279071809869514, -0.5708661417322835607, 1.224299699984025658 ) ) ;
#46709 = AXIS2_PLACEMENT_3D ( 'NONE', #29094, #4998, #32436 ) ;
#46711 = CARTESIAN_POINT ( 'NONE',  ( 0.03901279071809810040, -0.09842519685039370636, 1.713085361781127913 ) ) ;
#46710 = CARTESIAN_POINT ( 'NONE',  ( 1.033464566929133799, 0.000000000000000000, 0.8267716534357796299 ) ) ;
#46712 = CARTESIAN_POINT ( 'NONE',  ( 0.9873396505805591694, 0.1113553986120547346, 0.1230314959554651699 ) ) ;
#46713 = AXIS2_PLACEMENT_3D ( 'NONE', #23474, #38076, #18902 ) ;
#46714 = VERTEX_POINT ( 'NONE', #46994 ) ;
#46715 = ORIENTED_EDGE ( 'NONE', *, *, #26648, .F. ) ;
#46716 = CARTESIAN_POINT ( 'NONE',  ( -9.642888182262618425E-18, -0.07677165354330708902, -0.1574803149606299191 ) ) ;
#46717 = FACE_OUTER_BOUND ( 'NONE', #31909, .T. ) ;
#46718 = CARTESIAN_POINT ( 'NONE',  ( 0.1264236179284866091, -0.5418307086076535883, 0.1264236179284866091 ) ) ;
#46719 = VECTOR ( 'NONE', #20473, 39.37007874015748143 ) ;
#46720 = CARTESIAN_POINT ( 'NONE',  ( -0.06523048226347956391, -1.122539370078741827, 0.1574803149606297803 ) ) ;
#46721 = CARTESIAN_POINT ( 'NONE',  ( 0.8759842519685039353, -0.1574803149606299191, 0.8169291337507401662 ) ) ;
#46722 = CARTESIAN_POINT ( 'NONE',  ( 0.1574803149606300023, -0.4950321721878526704, -0.8627979602685659222 ) ) ;
#46723 = CARTESIAN_POINT ( 'NONE',  ( -1.054774247047244096, 0.000000000000000000, 0.4158464566391496531 ) ) ;
#46724 = EDGE_LOOP ( 'NONE', ( #26276, #40016, #8077, #31791 ) ) ;
#46725 = CARTESIAN_POINT ( 'NONE',  ( -0.8019270111902717657, 0.1787899950787401604, 1.496062992072220821 ) ) ;
#46726 = AXIS2_PLACEMENT_3D ( 'NONE', #23230, #18664, #34032 ) ;
#46727 = EDGE_CURVE ( 'NONE', #20308, #39783, #30791, .T. ) ;
#46728 = CARTESIAN_POINT ( 'NONE',  ( 1.002407869896990045, 0.1264236179284866091, 1.567421259788755794 ) ) ;
#46729 = ORIENTED_EDGE ( 'NONE', *, *, #44244, .F. ) ;
#46730 = CARTESIAN_POINT ( 'NONE',  ( 1.033464566929134687, -0.06523048226347956391, 0.9424212597349931331 ) ) ;
#46731 = ADVANCED_FACE ( 'NONE', ( #33128 ), #10114, .T. ) ;
#46732 = CARTESIAN_POINT ( 'NONE',  ( -0.8759842519685039353, -0.1787899950787401882, 0.6471456692375747721 ) ) ;
#46733 = CARTESIAN_POINT ( 'NONE',  ( 0.8019270111902717657, -0.1787899950787401604, 0.1328740156942679607 ) ) ;
#46734 = CARTESIAN_POINT ( 'NONE',  ( -1.033464566929133799, 0.000000000000000000, 1.072834645669291431 ) ) ;
#46735 = CARTESIAN_POINT ( 'NONE',  ( -0.8019270111902716547, -0.1787899950787401604, 0.6791338582139527791 ) ) ;
#46736 = FACE_OUTER_BOUND ( 'NONE', #40665, .T. ) ;
#46737 = EDGE_CURVE ( 'NONE', #10926, #16359, #30899, .T. ) ;
#46738 = CARTESIAN_POINT ( 'NONE',  ( 0.5966535433070866423, 0.000000000000000000, 0.000000000000000000 ) ) ;
#46739 = CARTESIAN_POINT ( 'NONE',  ( -0.1113553986120547346, -0.2194881888688507976, -0.1113553986120547346 ) ) ;
#46740 = CARTESIAN_POINT ( 'NONE',  ( -0.8759842519685039353, 0.1787899950787401882, 1.375492125930488196 ) ) ;
#46741 = CARTESIAN_POINT ( 'NONE',  ( -1.033464566929134687, -0.06523048226347956391, 0.4010826771653545619 ) ) ;
#46742 = CARTESIAN_POINT ( 'NONE',  ( 0.6971942568897648851, -0.07405724077823297447, 1.269685039316314601 ) ) ;
#46743 = CARTESIAN_POINT ( 'NONE',  ( -0.1729752768006175279, -0.09851383664320945144, -0.02639418254170881883 ) ) ;
#46744 = EDGE_LOOP ( 'NONE', ( #16065, #43527, #36349, #13937 ) ) ;
#46745 = EDGE_CURVE ( 'NONE', #20507, #40966, #34245, .T. ) ;
#46746 = AXIS2_PLACEMENT_3D ( 'NONE', #5653, #20263, #34910 ) ;
#46747 = ADVANCED_FACE ( 'NONE', ( #34016 ), #12439, .T. ) ;
#46748 = PRODUCT_RELATED_PRODUCT_CATEGORY ( 'part', '', ( #46114 ) ) ;
#46749 = CARTESIAN_POINT ( 'NONE',  ( -0.1264236179284866091, -1.664986172953647925, 0.1264236179284866091 ) ) ;
#46750 = ORIENTED_EDGE ( 'NONE', *, *, #33255, .T. ) ;
#46751 = EDGE_LOOP ( 'NONE', ( #29531, #2939, #6917, #44307 ) ) ;
#46752 = CARTESIAN_POINT ( 'NONE',  ( 0.8019270111902717657, 0.1787899950787401604, 1.373031496009229135 ) ) ;
#46753 = VECTOR ( 'NONE', #43246, 39.37007874015748143 ) ;
#46754 = AXIS2_PLACEMENT_3D ( 'NONE', #45536, #41933, #5540 ) ;
#46755 = CARTESIAN_POINT ( 'NONE',  ( -9.642888182262618425E-18, 0.08070866141732284393, -0.1574803149606299191 ) ) ;
#46756 = CARTESIAN_POINT ( 'NONE',  ( -0.1787899950787401604, -0.2785433070328505734, 0.07405724077823318263 ) ) ;
#46757 = CARTESIAN_POINT ( 'NONE',  ( 0.1264236179284866091, -0.7731299212060788184, 0.1264236179284866091 ) ) ;
#46758 = DIRECTION ( 'NONE',  ( 0.000000000000000000, 9.251858538542967883E-16, 1.000000000000000000 ) ) ;
#46759 = DIRECTION ( 'NONE',  ( 0.000000000000000000, 1.000000000000000000, 0.000000000000000000 ) ) ;
#46760 = CARTESIAN_POINT ( 'NONE',  ( 0.8759842519685039353, -0.1787899950787401882, 0.3272637794737956463 ) ) ;
#46761 = CARTESIAN_POINT ( 'NONE',  ( 0.1264236179284866091, -0.07049798397727027877, -0.1264236179284866091 ) ) ;
#46762 = CARTESIAN_POINT ( 'NONE',  ( -0.1264236179284866091, -0.2317913385289138151, 0.1264236179284866091 ) ) ;
#46763 = CARTESIAN_POINT ( 'NONE',  ( 0.1787899950787401604, 0.05610236225848794223, -0.07405724077823318263 ) ) ;
#46764 = CARTESIAN_POINT ( 'NONE',  ( 0.02970261290376345273, -0.09842519685039373412, 0.1606413281782796409 ) ) ;
#46765 = DIRECTION ( 'NONE',  ( -1.000000000000000000, 0.000000000000000000, 0.000000000000000000 ) ) ;
#46766 = CARTESIAN_POINT ( 'NONE',  ( 0.9500414927467378812, 0.1787899950787401604, 0.5413385826234012876 ) ) ;
#46767 = CARTESIAN_POINT ( 'NONE',  ( -0.6971942568897648851, -0.07405724077823297447, 0.9940944881352130613 ) ) ;
#46768 = DIRECTION ( 'NONE',  ( -1.000000000000000000, 0.000000000000000000, 0.000000000000000000 ) ) ;
#46769 = CARTESIAN_POINT ( 'NONE',  ( 0.07444174185955065859, -1.760378455252336938, 0.1797182628040039087 ) ) ;
#46770 = CARTESIAN_POINT ( 'NONE',  ( -0.1264236179284866091, -0.4286417322297008115, 0.1264236179284866091 ) ) ;
#46771 = DIRECTION ( 'NONE',  ( -0.7071067811865454633, 8.659560562354952580E-17, -0.7071067811865494601 ) ) ;
#46772 = CARTESIAN_POINT ( 'NONE',  ( 1.054774247047244540, -0.07405724077823318263, 1.678149606245448622 ) ) ;
#46774 = CARTESIAN_POINT ( 'NONE',  ( -0.1673228346456692994, -0.4889725119976395251, -0.8550419489141688478 ) ) ;
#46773 = CARTESIAN_POINT ( 'NONE',  ( 0.1894960330211038768, 0.07859832706092066690, -0.1760274851910411664 ) ) ;
#46775 = ORIENTED_EDGE ( 'NONE', *, *, #45991, .T. ) ;
#46777 = EDGE_CURVE ( 'NONE', #3281, #18202, #4387, .T. ) ;
#46776 = CARTESIAN_POINT ( 'NONE',  ( -0.1675084398163183552, -0.08956740676313401650, -0.1887210895732543414 ) ) ;
#46778 = CARTESIAN_POINT ( 'NONE',  ( 0.7646288533564489232, -0.1113553986120547346, 0.03444881889763779653 ) ) ;
#46780 = CARTESIAN_POINT ( 'NONE',  ( 3.284318927891251994E-17, -0.07431102356828367395, 0.1787899950787401882 ) ) ;
#46779 = CARTESIAN_POINT ( 'NONE',  ( -0.06523048226347956391, -0.8912401573727871673, -0.1574803149606300301 ) ) ;
#46781 = CARTESIAN_POINT ( 'NONE',  ( 0.7495606340400177148, -0.1264236179284866091, 0.6373031495525354195 ) ) ;
#46782 = CARTESIAN_POINT ( 'NONE',  ( -0.1787899950787401882, -1.102854330654897685, 0.000000000000000000 ) ) ;
#46783 = DIRECTION ( 'NONE',  ( -1.000000000000000000, 0.000000000000000000, 0.000000000000000000 ) ) ;
#46784 = CARTESIAN_POINT ( 'NONE',  ( 0.1476377952755906220, 0.05639690512153986562, -0.1570009270184611894 ) ) ;
#46785 = CARTESIAN_POINT ( 'NONE',  ( -0.9873396505805591694, -0.1113553986120547346, 0.9891732283464568232 ) ) ;
#46786 = CARTESIAN_POINT ( 'NONE',  ( -1.002407869896990045, -0.1264236179284866091, 1.434547244040724534 ) ) ;
#46787 = VERTEX_POINT ( 'NONE', #27303 ) ;
#46788 = CARTESIAN_POINT ( 'NONE',  ( -0.2713569170882992876, -0.1500457819031512374, -0.8011292026335117278 ) ) ;
#46789 = EDGE_CURVE ( 'NONE', #4309, #21602, #43785, .T. ) ;
#46790 = CARTESIAN_POINT ( 'NONE',  ( 0.7495606340400177148, -0.1264236179284866091, 1.232775590497417362 ) ) ;
#46791 = CARTESIAN_POINT ( 'NONE',  ( -0.8107537697050253289, 0.1574803149606300301, 0.7209645668216065895 ) ) ;
#46792 = CONICAL_SURFACE ( 'NONE', #14653, 0.09842519685039310962, 0.7853981633972314524 ) ;
#46793 = CIRCLE ( 'NONE', #83, 0.2559055118110236116 ) ;
#46794 = CARTESIAN_POINT ( 'NONE',  ( 0.8107537697050254399, -0.1574803149606297803, 1.493602362204724754 ) ) ;
#46795 = CARTESIAN_POINT ( 'NONE',  ( 0.7495606340400177148, 0.1264236179284866091, 1.847933070812378009 ) ) ;
#46796 = CARTESIAN_POINT ( 'NONE',  ( -0.9412147342319837628, 0.1574803149606300301, 1.434547244094487972 ) ) ;
#46797 = CARTESIAN_POINT ( 'NONE',  ( -0.6971942568897626646, 0.07405724077823318263, 0.9448818897100165204 ) ) ;
#46798 = CARTESIAN_POINT ( 'NONE',  ( 0.000000000000000000, 0.000000000000000000, 0.000000000000000000 ) ) ;
#46799 = LINE ( 'NONE', #13514, #13256 ) ;
#46800 = CARTESIAN_POINT ( 'NONE',  ( 0.6971942568897648851, 0.07405724077823318263, 0.3592519684501735422 ) ) ;
#46801 = CARTESIAN_POINT ( 'NONE',  ( -1.054774247047244540, -0.07405724077823318263, 0.5708661416785201226 ) ) ;
#46802 = AXIS2_PLACEMENT_3D ( 'NONE', #7300, #33437, #14731 ) ;
#46803 = CARTESIAN_POINT ( 'NONE',  ( 0.9412147342319837628, 0.1574803149606300301, 1.542814960522393308 ) ) ;
#46804 = ORIENTED_EDGE ( 'NONE', *, *, #22284, .F. ) ;
#46805 = CARTESIAN_POINT ( 'NONE',  ( 0.1264236179284866091, 0.04872047249470835839, 0.1264236179284866091 ) ) ;
#46806 = CARTESIAN_POINT ( 'NONE',  ( 0.9412147342319837628, 0.1574803149606300301, 1.779035432963339769 ) ) ;
#46807 = CARTESIAN_POINT ( 'NONE',  ( 0.8019270111902717657, -0.1787899950787401604, 0.8415354330171019859 ) ) ;
#46808 = CARTESIAN_POINT ( 'NONE',  ( -1.054774247047244096, 0.000000000000000000, 1.911909448765133801 ) ) ;
#46809 = DIRECTION ( 'NONE',  ( 0.000000000000000000, 0.000000000000000000, -1.000000000000000000 ) ) ;
#46810 = DIRECTION ( 'NONE',  ( 1.000000000000000000, 0.000000000000000000, 0.000000000000000000 ) ) ;
#46811 = CARTESIAN_POINT ( 'NONE',  ( 0.1787899950787401604, -1.293431054843413142, -0.07405724077823318263 ) ) ;
#46812 = EDGE_LOOP ( 'NONE', ( #11452, #8247, #16632, #17185, #23142, #15733 ) ) ;
#46813 = CARTESIAN_POINT ( 'NONE',  ( -0.07405724077823318263, -0.2687007873478113318, 0.1787899950787401604 ) ) ;
#46814 = ORIENTED_EDGE ( 'NONE', *, *, #23177, .F. ) ;
#46815 = CARTESIAN_POINT ( 'NONE',  ( 0.0005737749932938826774, -0.1277779173642346333, -0.05427780112423363085 ) ) ;
#46816 = DIRECTION ( 'NONE',  ( 0.000000000000000000, 0.000000000000000000, 1.000000000000000000 ) ) ;
#46817 = ( BOUNDED_CURVE ( )  B_SPLINE_CURVE ( 2, ( #34473, #45699, #41618, #46182, #27548, #35188, #27070, #42100, #9305 ),
 .UNSPECIFIED., .F., .T. ) 
 B_SPLINE_CURVE_WITH_KNOTS ( ( 3, 2, 2, 2, 3 ),
 ( 0.5799999999999999600, 0.5825000000000000178, 0.5849999999999999645, 0.5875000000000000222, 0.5899999999999999689 ),
 .UNSPECIFIED. ) 
 CURVE ( )  GEOMETRIC_REPRESENTATION_ITEM ( )  RATIONAL_B_SPLINE_CURVE ( ( 1.000000000000000000, 0.9238795325112869605, 1.000000000000000000, 0.9238795325112869605, 1.000000000000000000, 0.9238795325112869605, 1.000000000000000000, 0.9238795325112869605, 1.000000000000000000 ) ) 
 REPRESENTATION_ITEM ( '' )  ) ;
#46818 = VECTOR ( 'NONE', #47391, 39.37007874015748143 ) ;
#46819 = VECTOR ( 'NONE', #41963, 39.37007874015748143 ) ;
#46820 = AXIS2_PLACEMENT_3D ( 'NONE', #37064, #8294, #23166 ) ;
#46821 = CARTESIAN_POINT ( 'NONE',  ( -0.1787899950787401604, -1.503937007820251637, -0.07405724077823318263 ) ) ;
#46822 = CARTESIAN_POINT ( 'NONE',  ( -0.1264236179284866091, -0.7878937007336378473, 0.1264236179284866091 ) ) ;
#46823 = CARTESIAN_POINT ( 'NONE',  ( -0.8759842519685039353, 0.1787899950787401882, 0.4306102361667086820 ) ) ;
#46824 = CARTESIAN_POINT ( 'NONE',  ( -0.1797182628040039087, -1.297780030055485589, 0.07444174185955065859 ) ) ;
#46825 = CARTESIAN_POINT ( 'NONE',  ( -0.08530144295877870042, 0.2462454212078929172, -0.03730110279446391397 ) ) ;
#46826 = CARTESIAN_POINT ( 'NONE',  ( 0.7495606340400177148, 0.1264236179284866091, 1.222933070812378009 ) ) ;
#46827 = CARTESIAN_POINT ( 'NONE',  ( 0.7495606340400177148, -0.1264236179284866091, 1.542814960576157413 ) ) ;
#46828 = ADVANCED_FACE ( 'NONE', ( #19362 ), #34645, .F. ) ;
#46829 = CARTESIAN_POINT ( 'NONE',  ( 0.7185039370078739607, 1.928577636452523993E-17, 1.683070866141732402 ) ) ;
#46831 = CARTESIAN_POINT ( 'NONE',  ( 0.8759842519685039353, -0.1574803149606299191, 1.525590551073574774 ) ) ;
#46830 = CARTESIAN_POINT ( 'NONE',  ( 0.1559668151880143627, -0.05603484930530078928, 0.1377952755905511861 ) ) ;
#46832 = CARTESIAN_POINT ( 'NONE',  ( 0.9412147342319837628, 0.1574803149606300301, 0.6766732282389295028 ) ) ;
#46833 = CARTESIAN_POINT ( 'NONE',  ( -0.7646288533564489232, 0.1113553986120547346, 1.786417322727117840 ) ) ;
#46835 = ( BOUNDED_SURFACE ( )  B_SPLINE_SURFACE ( 1, 2, ( 
 ( #11707, #32817, #4014, #176, #33293, #47410, #33056, #416, #33524, #18865, #18407, #22709, #29715, #43802, #4235, #37315, #14823, #640, #11002, #25619, #40654, #22002, #36627, #44034, #7851, #3790, #22469, #37087, #43473, #36319, #32257, #6343, #28670, #46834, #17371, #14024, #43716, #40113, #32008, #43238, #47326, #25543, #10679, #3474, #14498, #7306, #28909, #6585, #21926, #18330, #21197, #10920, #25039, #32495, #3220, #18086, #24571, #13778, #32732, #25287, #39171, #13548, #35832, #42990, #35604, #9959, #20958, #21689, #2743, #29159, #17611, #2978, #39402, #32967, #46600, #10441, #28185, #6816, #28424, #36546, #7062, #42744, #3707, #10198, #24804, #39634, #21436, #39876, #36063, #17849, #47077, #14270, #15699, #36776, #44179, #29409, #18789, #33443, #11150, #11383, #4386, #44883, #40341, #8239, #559, #26720, #43953, #3934, #14985, #22383, #19264, #18555, #11855, #33212, #30108, #12096, #41274, #40575, #11624, #26481, #25771, #26243, #37480, #19502, #8473, #29638, #25995, #7531, #22630, #19017, #7767, #37007, #33680, #23108, #793, #22866, #15457, #37723, #41045, #33918, #1041, #4874, #38668, #8715, #31256, #37962, #16626, #45834, #30799, #13043, #23810, #27679, #31491, #5346, #41990, #19735, #42242, #9192, #9445, #46076, #20445, #38891, #1759, #45364, #19970, #24293, #5113, #12577, #24061, #5837, #34371, #35083, #34610, #6054, #20203, #2231, #1511, #16850, #13277, #27910, #41754, #42473, #9678, #41510, #38188, #34146, #38429, #16401, #1276, #15931, #31026, #26958, #45593, #12814, #16164, #27444, #30560, #45121, #27205, #5595, #12338, #23351, #8958, #23578, #34855, #2000, #36010, #13727, #32679, #26119, #28365, #18033, #32194, #39587, #10386, #25228, #31725, #20912, #10625, #17797, #46318, #20680, #42934, #2696, #42691, #17087, #28134, #28857, #13502, #21632, #24753, #10144, #46544, #40690, #9909, #2921, #35320, #13968, #24518, #7005, #14217, #2460, #39816, #47267, #39116, #6768, #14447, #29103, #24992, #36266, #46781, #39348, #6530, #11498, #6292, #35552, #21144, #35779, #28618, #17323, #44294, #43178, #21385, #3167, #32444, #47022, #43417, #19383, #23476, #41635, #23234, #8841, #4503, #45477, #677, #26604, #18903, #12704, #16286, #33559, #19140, #12214, #33805, #34037, #22986, #38078, #5234, #37597, #27329, #4757, #7885, #15819, #45001, #41397, #8596, #19623, #10023, #34742, #2116, #13608, #27807, #39238, #5719, #20334, #42585, #42113, #9327, #46430, #9566, #45716, #5481, #46665, #13850, #24643, #12932, #35208, #13396, #31851, #41876, #13171, #28249, #23946, #38553, #24407, #34972, #16746, #38787, #27566, #9081, #23700, #42812, #42367, #6412, #21028, #31387, #38309, #46198, #45957, #24185, #5944, #20565, #35674, #20096, #2346, #1883, #9798, #39009, #32076, #16979, #31617, #6176, #16518, #28026, #20799, #35440, #2811, #17442, #2577, #17216, #31146, #3770, #14339, #14569, #6886, #17676, #10757, #32326, #29470, #18392, #39946, #43064, #43543, #33035, #402, #44015, #46905, #25110, #10267, #32570, #28984, #39473, #39699, #32799, #11217, #21268, #36611, #47155, #7596, #24878, #3047, #28743, #3296, #161, #14095, #25604, #43307, #10987, #40178, #21505, #7378, #18159, #21989, #25830, #25364, #36392, #10511, #14809, #3547, #40408, #22210, #36840, #33277, #7136, #36142, #21757, #18616, #17916, #47394, #3996, #28496, #29237, #6651, #43788, #35893, #1108, #4945, #619, #12159, #1345, #41342, #22692, #26783, #19572, #22448, #19082, #15051, #4701, #15524, #44948, #37793, #33753, #7835, #30166, #864, #18850, #44706, #45188, #41581, #33507, #11929, #16000, #27030, #8543, #34216, #30623, #8783, #30399, #8069, #23419, #19802, #37296, #12410, #26548, #33981, #19332, #38022, #26064, #15278, #5181, #23176, #40633, #29700, #4447, #44474, #37068, #11447, #4222, #34434, #29929, #44243, #41108, #8300, #40871, #11690, #26314, #22931, #37541, #15767, #23643, #35383, #42534, #16231, #20741, #31795, #46379, #42060, #20272, #46143, #30866, #41820, #9265, #2528, #34920, #28195, #12875, #27509, #2290, #1824, #16460, #6116, #16695, #5418, #12645, #6354, #20969, #17154, #20037, #42313, #20512, #38951, #1581, #2064, #42753, #31096, #45657, #31560, #23882, #38494, #45901, #34678, #45427, #27271, #9972, #31324, #24584, #39181, #5664, #9021, #5900, #9506, #24128, #38732, #35148, #38255, #16920, #13339, #27968, #9737, #24353, #25781, #21447, #3233, #47340, #28437, #43486, #32267, #32744, #7320, #3719, #43728, #14513, #10693, #10931, #36076, #21700, #14037, #24815, #17863, #39414, #36559, #25552, #47088, #2758, #104, #6596, #7073, #32981, #14750, #25300, #21939, #32505, #39646, #43251, #40351, #7544, #35615, #6827, #14282, #28922, #32019, #40123, #17381, #18340, #36333, #46610, #28683, #29421, #39888, #43966, #29177, #3485, #11164, #21209, #13791, #43001, #18100, #10212, #35841, #2990, #17622, #46846, #10452, #25052, #807, #18570, #44896, #15713, #37024, #41287, #19030, #37735, #4175, #8015, #11394, #1291, #44652, #4891, #44421, #22396, #11869, #15946, #3944, #40590, #15001, #4649, #19275, #12350, #22646, #26494, #33932, #29652, #41056, #18800, #1054, #8487, #19513, #30348, #12109, #8254, #23122, #34161, #30572, #574, #26010, #45133, #7781, #26969, #22155, #33226, #352, #44194, #33457, #15232, #29878, #11637, #26257, #40820, #16640, #31270, #45849, #46327, #8728, #23364, #13056, #27694, #24074, #19750, #13289, #37972, #42484, #38683, #34385, #1772, #46086, #5850, #38903, #16860, #20459, #2471, #8970, #31739, #1524, #35093, #16178, #45378, #23589, #38201, #5363, #31503, #19983, #34622, #39128, #18043, #36277, #10156, #14456, #39598, #10877, #24765, #28629, #31970, #21884, #6777, #25497, #35564, #2930, #29114, #43187, #40064, #6543, #21154, #43427, #42948, #39363, #47278, #10399, #46554, #6299, #44, #14692, #7265, #13738, #36020, #14227, #32687, #42702, #13980, #43666, #35789, #17567, #25241, #32206, #46795, #21395, #28380, #9921, #24528, #36504, #3180, #3659, #18282, #17809, #20922, #47036, #32457, #28869, #2707, #10636, #39828, #32925, #7020, #21644, #3429, #17335, #4335, #25950, #26433, #989, #44835, #37421, #8184, #33630, #4576, #15173, #15405, #7718, #18513, #11569, #33166, #30284, #19211, #40762, #43906, #41218, #288, #30052, #26668, #8421, #44594, #15646, #26196, #33398, #36963, #1227, #29366, #11107, #514, #44362, #7957, #40299, #33871 ),
 ( #22577, #7482, #12046, #22808, #11338, #23050, #11810, #4822, #40529, #29817, #14935, #22101, #3888, #22335, #4117, #18740, #2178, #27392, #13232, #19918, #34550, #16579, #16116, #41936, #20390, #9143, #23760, #8658, #30505, #45066, #31440, #38370, #34803, #1949, #5785, #23294, #31208, #16801, #45781, #27630, #38608, #6006, #2643, #46733, #20862, #7203, #21825, #39767, #35735, #14404, #21578, #35503, #31680, #6717, #28311, #39302, #17277, #13917, #25434, #28085, #9859, #6958, #32139, #29053, #36221, #31912, #24470, #21332, #42879, #6477, #46495, #28564, #6235, #43132, #10336, #39544, #17748, #46973, #35963, #32396, #14166, #43372, #3372, #17981, #32634, #693, #8137, #19157, #11762, #15347, #44313, #26382, #22279, #22521, #14877, #25671, #18683, #40246, #33820, #22760, #466, #32868, #937, #7433, #7905, #15597, #30233, #26138, #44783, #33342, #40478, #44088, #38523, #14635, #29304, #7662, #4070, #15119, #11055, #11997, #22052, #36677, #37137, #3836, #29537, #18458, #29765, #33107, #231, #4287, #25896, #36915, #11515, #40706, #18918, #37614, #28446, #17391, #4773, #26854, #27346, #8611, #1657, #19401, #45733, #16534, #37866, #42130, #5254, #6363, #5020, #8858, #12231, #2767, #34503, #20978, #15838, #30695, #9980, #23492, #35625, #34283, #1409, #23718, #23250, #19639, #27579, #38092, #41414, #34052, #43012, #23002, #32029, #16070, #16303, #41889, #12946, #1177, #41654, #24591, #45259, #12480, #5497, #27105, #30931, #45492, #12719, #30460, #45018, #9097, #38324, #20109, #46620, #34757, #1897, #31163, #13803, #36343, #6606, #32992, #3728, #25062, #29431, #39899, #25792, #39653, #10706, #46858, #36801, #7086, #40363, #2999, #17872, #43975, #25311, #7553, #21457, #36088, #10942, #10462, #6837, #14761, #21711, #14045, #21221, #15010, #29663, #22162, #28692, #3497, #29191, #114, #10221, #28935, #11177, #3245, #32516, #40133, #47101, #14291, #18112, #43261, #24825, #39427, #3954, #32755, #18577, #33234, #47351, #17633, #14525, #43738, #25561, #7331, #21947, #361, #32277, #36568, #18347, #41298, #1303, #11647, #44663, #22887, #12362, #40832, #1063, #8025, #8739, #5135, #15479, #1782, #31050, #45617, #27466, #13069, #42013, #9220, #23838, #2023, #6556, #18294, #7276, #28881, #31979, #29377, #21166, #36289, #14702, #43917, #7030, #36516, #47047, #21406, #25013, #7495, #36740, #17347, #36033, #32468, #43442, #13749, #21894, #46567, #3671, #18053, #22115, #10411, #32935, #10647, #56, #10889, #32700, #11121, #35800, #40312, #10167, #39611, #25739, #3194, #28391, #28642, #43200, #47290, #17580, #32222, #42959, #14240, #2945, #24775, #39372, #46807, #13992, #6788, #25252, #3441, #17822, #39841, #21656, #14470, #29126, #43680, #25509, #40078, #4127, #44602, #22346, #8670, #33178, #41228, #37201, #1238, #23062, #18750, #299, #8197, #29828, #18978, #33408, #41006, #45077, #40540, #22820, #7730, #1001, #12055, #41467, #37435, #8433, #15892, #41762, #42250, #31034, #31500, #6060, #2467, #42481, #13285, #9454, #9684, #20212, #20454, #12820, #23585, #16634, #38196, #35328, #38900, #45844, #1519, #46325, #5357, #5845, #31732, #13508, #24068, #20688, #31265, #38437, #41996, #24525, #6297, #34380, #5604, #2008, #13052, #30806, #17094, #16172, #28142, #35089, #39126, #27453, #42699, #27688, #9917, #27916, #2237, #45373, #19978, #12587, #8966, #34862, #34617, #1766, #16408, #45601, #9200, #38677, #23818, #16856, #46082, #10874, #14455, #35788, #40062, #3176, #36503, #2927, #6776, #10154, #42, #17806, #3658, #24761, #7262, #39595, #11105, #7014, #25495, #6539, #18041, #21883, #47276, #28628, #32686, #18281, #28376, #24999, #20920, #10632, #21392, #3426, #32923, #36017, #13735, #32455, #47032, #39358, #14223, #14690, #29364, #17565, #28866, #25728, #40296, #29113, #35560, #2704, #17331, #36275, #13977, #31967, #46552, #43185, #42944, #43424, #39825, #25237, #32203, #46790, #10395, #44833, #4575, #18509, #36728, #29815, #36962, #29596, #286, #14932, #37667, #44138, #4821, #11568, #44360, #33397, #12281, #11337, #37190, #40528, #743, #7717, #19445, #986, #22332, #34097, #1225, #15879, #513, #26193, #33868, #18738, #22573, #45065, #26899, #15171, #7956, #4334, #33629, #15404, #30048, #37418, #38137, #45777, #9622, #34325, #2175, #12760, #20623, #8657, #16115, #41702, #30971, #46018, #30738, #38604, #12528, #5780, #20387, #5299, #35027, #31205, #16798, #38838, #27390, #1942, #27149, #31437, #16575, #13228, #6003, #42418, #46255, #9141, #19917, #41934, #31677, #8903, #34548, #24240, #35270, #1699, #2405, #20153, #17038, #13452, #9387, #41457, #23535, #23293, #1455, #23758, #37909, #5065, #45537, #38367, #34800, #12986, #27627, #42179, #24465, #3368, #21576, #42875, #47219, #10332, #43608, #10086, #13914, #17272, #7201, #24943, #25431, #20856, #35731, #40006, #28559, #21822, #39298, #6472, #28806, #28308, #24698, #32631, #43128, #31908, #39063, #32865, #43852, #36451, #13670, #21329, #14163, #17978, #28082, #46728, #3605, #2869, #17504, #10581, #32135, #39540, #6714, #35961, #42644, #9855, #18225, #3118, #6232, #35499, #17745, #2640, #32392, #43369, #25179, #39763, #6955, #36216, #43850, #33103, #7431, #15344, #11757, #4770, #463, #29762, #26380, #22049, #22518, #11281, #40938, #33818, #30231, #22758, #8134, #37133, #37363, #15116, #691, #40475, #3833, #44309, #18455, #15593, #4517, #26134, #29302, #26616, #225, #33574, #11995, #41169, #4284, #934, #11512, #18679, #22276, #19397, #34049, #14632, #33339, #40703, #7902, #11053, #19154, #25667, #44780, #29997, #40242, #18915, #8372, #36675, #22999, #14874, #25893, #29534, #44541, #37611, #44085, #7659, #36912, #4065, #41410, #9340, #34500, #42377, #15834, #23247, #1406, #23489, #5730, #37861, #45729, #5015, #31159, #12944, #45256, #27576, #38321, #42127, #45967, #1654, #9093, #34279, #23959, #23715, #38565, #13182, #2129, #5956, #16299, #12476, #30927, #38796, #19635, #27099, #16758, #31397, #16066, #9576, #45489, #20576, #16531, #24194, #30692, #1173, #45014, #12226, #8854, #8608, #41651, #38090, #5251, #12716, #5494, #27342, #41886, #20107, #6422, #28037, #2819, #21042, #39019, #35683, #17924, #14345, #6185, #17452, #21514, #47162, #17686, #10521, #36153, #28994, #3059, #28261, #43552, #39952, #42822, #32577, #46674, #6662, #24889, #39711, #46207, #35448, #25119, #32337, #13408, #35218 ) ),
 .UNSPECIFIED., .F., .F., .F. ) 
 B_SPLINE_SURFACE_WITH_KNOTS ( ( 2, 2 ),
 ( 3, 2, 2, 2, 2, 2, 2, 2, 2, 2, 2, 2, 2, 2, 2, 2, 2, 2, 2, 2, 2, 2, 2, 2, 2, 2, 2, 2, 2, 2, 2, 2, 2, 2, 2, 2, 2, 2, 2, 2, 2, 2, 2, 2, 2, 2, 2, 2, 2, 2, 2, 2, 2, 2, 2, 2, 2, 2, 2, 2, 2, 2, 2, 2, 2, 2, 2, 2, 2, 2, 2, 2, 2, 2, 2, 2, 2, 2, 2, 2, 2, 2, 2, 2, 2, 2, 2, 2, 2, 2, 2, 2, 2, 2, 2, 2, 2, 2, 2, 2, 2, 2, 2, 2, 2, 2, 2, 2, 2, 2, 2, 2, 2, 2, 2, 2, 2, 2, 2, 2, 2, 2, 2, 2, 2, 2, 2, 2, 2, 2, 2, 2, 2, 2, 2, 2, 2, 2, 2, 2, 2, 2, 2, 2, 2, 2, 2, 2, 2, 2, 2, 2, 2, 2, 2, 2, 2, 2, 2, 2, 2, 2, 2, 2, 2, 2, 2, 2, 2, 2, 2, 2, 2, 2, 2, 2, 2, 2, 2, 2, 2, 2, 2, 2, 2, 2, 2, 2, 2, 2, 2, 2, 2, 2, 2, 2, 2, 2, 2, 2, 2, 2, 2, 2, 2, 2, 2, 2, 2, 2, 2, 2, 2, 2, 2, 2, 2, 2, 2, 2, 2, 2, 2, 2, 2, 2, 2, 2, 2, 2, 2, 2, 2, 2, 2, 2, 2, 2, 2, 2, 2, 2, 2, 2, 2, 2, 2, 2, 2, 2, 2, 2, 2, 2, 2, 2, 2, 2, 2, 2, 2, 2, 2, 2, 2, 2, 2, 2, 2, 2, 2, 2, 2, 2, 2, 2, 2, 2, 2, 2, 2, 2, 2, 2, 2, 2, 2, 2, 2, 2, 2, 2, 2, 2, 2, 2, 2, 2, 2, 2, 2, 2, 2, 2, 2, 2, 2, 2, 2, 2, 2, 2, 2, 2, 2, 2, 2, 2, 2, 2, 2, 2, 2, 2, 2, 2, 2, 2, 2, 2, 2, 2, 2, 2, 2, 2, 2, 2, 2, 2, 2, 2, 2, 2, 2, 2, 2, 2, 2, 2, 2, 2, 2, 2, 2, 2, 2, 2, 2, 2, 2, 2, 2, 2, 2, 2, 2, 2, 2, 2, 2, 2, 2, 2, 2, 2, 2, 2, 2, 2, 2, 2, 2, 2, 2, 2, 2, 2, 2, 2, 2, 2, 2, 2, 2, 2, 2, 2, 2, 2, 3 ),
 ( 0.000000000000000000, 1.000000000000000000 ),
 ( 0.000000000000000000, 0.002500000000000000052, 0.005000000000000000104, 0.007499999999999999722, 0.01000000000000000021, 0.01250000000000000069, 0.01499999999999999944, 0.01750000000000000167, 0.02000000000000000042, 0.02249999999999999917, 0.02500000000000000139, 0.02750000000000000014, 0.02999999999999999889, 0.03250000000000000111, 0.03500000000000000333, 0.03749999999999999861, 0.04000000000000000083, 0.04250000000000000305, 0.04499999999999999833, 0.04750000000000000056, 0.05000000000000000278, 0.05249999999999999806, 0.05500000000000000028, 0.05750000000000000250, 0.05999999999999999778, 0.06250000000000000000, 0.06500000000000000222, 0.06750000000000000444, 0.07000000000000000666, 0.07249999999999999500, 0.07499999999999999722, 0.07749999999999999944, 0.08000000000000000167, 0.08250000000000000389, 0.08500000000000000611, 0.08749999999999999445, 0.08999999999999999667, 0.09249999999999999889, 0.09500000000000000111, 0.09750000000000000333, 0.1000000000000000056, 0.1024999999999999939, 0.1049999999999999961, 0.1074999999999999983, 0.1100000000000000006, 0.1125000000000000028, 0.1150000000000000050, 0.1174999999999999933, 0.1199999999999999956, 0.1224999999999999978, 0.1250000000000000000, 0.1275000000000000022, 0.1300000000000000044, 0.1325000000000000067, 0.1350000000000000089, 0.1375000000000000111, 0.1400000000000000133, 0.1424999999999999878, 0.1449999999999999900, 0.1474999999999999922, 0.1499999999999999944, 0.1524999999999999967, 0.1549999999999999989, 0.1575000000000000011, 0.1600000000000000033, 0.1625000000000000056, 0.1650000000000000078, 0.1675000000000000100, 0.1700000000000000122, 0.1724999999999999867, 0.1749999999999999889, 0.1774999999999999911, 0.1799999999999999933, 0.1824999999999999956, 0.1849999999999999978, 0.1875000000000000000, 0.1900000000000000022, 0.1925000000000000044, 0.1950000000000000067, 0.1975000000000000089, 0.2000000000000000111, 0.2025000000000000133, 0.2049999999999999878, 0.2074999999999999900, 0.2099999999999999922, 0.2124999999999999944, 0.2149999999999999967, 0.2174999999999999989, 0.2200000000000000011, 0.2225000000000000033, 0.2250000000000000056, 0.2275000000000000078, 0.2300000000000000100, 0.2325000000000000122, 0.2349999999999999867, 0.2374999999999999889, 0.2399999999999999911, 0.2424999999999999933, 0.2449999999999999956, 0.2474999999999999978, 0.2500000000000000000, 0.2525000000000000022, 0.2550000000000000044, 0.2575000000000000067, 0.2600000000000000089, 0.2625000000000000111, 0.2650000000000000133, 0.2675000000000000155, 0.2700000000000000178, 0.2725000000000000200, 0.2750000000000000222, 0.2775000000000000244, 0.2800000000000000266, 0.2824999999999999734, 0.2849999999999999756, 0.2874999999999999778, 0.2899999999999999800, 0.2924999999999999822, 0.2949999999999999845, 0.2974999999999999867, 0.2999999999999999889, 0.3024999999999999911, 0.3049999999999999933, 0.3074999999999999956, 0.3099999999999999978, 0.3125000000000000000, 0.3150000000000000022, 0.3175000000000000044, 0.3200000000000000067, 0.3225000000000000089, 0.3250000000000000111, 0.3275000000000000133, 0.3300000000000000155, 0.3325000000000000178, 0.3350000000000000200, 0.3375000000000000222, 0.3400000000000000244, 0.3425000000000000266, 0.3449999999999999734, 0.3474999999999999756, 0.3499999999999999778, 0.3524999999999999800, 0.3549999999999999822, 0.3574999999999999845, 0.3599999999999999867, 0.3624999999999999889, 0.3649999999999999911, 0.3674999999999999933, 0.3699999999999999956, 0.3724999999999999978, 0.3750000000000000000, 0.3775000000000000022, 0.3800000000000000044, 0.3825000000000000067, 0.3850000000000000089, 0.3875000000000000111, 0.3900000000000000133, 0.3925000000000000155, 0.3950000000000000178, 0.3975000000000000200, 0.4000000000000000222, 0.4025000000000000244, 0.4050000000000000266, 0.4074999999999999734, 0.4099999999999999756, 0.4124999999999999778, 0.4149999999999999800, 0.4174999999999999822, 0.4199999999999999845, 0.4224999999999999867, 0.4249999999999999889, 0.4274999999999999911, 0.4299999999999999933, 0.4324999999999999956, 0.4349999999999999978, 0.4375000000000000000, 0.4400000000000000022, 0.4425000000000000044, 0.4450000000000000067, 0.4475000000000000089, 0.4500000000000000111, 0.4525000000000000133, 0.4550000000000000155, 0.4575000000000000178, 0.4600000000000000200, 0.4625000000000000222, 0.4650000000000000244, 0.4675000000000000266, 0.4699999999999999734, 0.4724999999999999756, 0.4749999999999999778, 0.4774999999999999800, 0.4799999999999999822, 0.4824999999999999845, 0.4849999999999999867, 0.4874999999999999889, 0.4899999999999999911, 0.4924999999999999933, 0.4949999999999999956, 0.4974999999999999978, 0.5000000000000000000, 0.5024999999999999467, 0.5050000000000000044, 0.5074999999999999512, 0.5100000000000000089, 0.5124999999999999556, 0.5150000000000000133, 0.5174999999999999600, 0.5200000000000000178, 0.5224999999999999645, 0.5250000000000000222, 0.5274999999999999689, 0.5300000000000000266, 0.5324999999999999734, 0.5350000000000000311, 0.5374999999999999778, 0.5400000000000000355, 0.5424999999999999822, 0.5450000000000000400, 0.5474999999999999867, 0.5500000000000000444, 0.5524999999999999911, 0.5550000000000000488, 0.5574999999999999956, 0.5600000000000000533, 0.5625000000000000000, 0.5649999999999999467, 0.5675000000000000044, 0.5699999999999999512, 0.5725000000000000089, 0.5749999999999999556, 0.5775000000000000133, 0.5799999999999999600, 0.5825000000000000178, 0.5849999999999999645, 0.5875000000000000222, 0.5899999999999999689, 0.5925000000000000266, 0.5949999999999999734, 0.5975000000000000311, 0.5999999999999999778, 0.6025000000000000355, 0.6049999999999999822, 0.6075000000000000400, 0.6099999999999999867, 0.6125000000000000444, 0.6149999999999999911, 0.6175000000000000488, 0.6199999999999999956, 0.6225000000000000533, 0.6250000000000000000, 0.6274999999999999467, 0.6300000000000000044, 0.6324999999999999512, 0.6350000000000000089, 0.6374999999999999556, 0.6400000000000000133, 0.6424999999999999600, 0.6450000000000000178, 0.6474999999999999645, 0.6500000000000000222, 0.6524999999999999689, 0.6550000000000000266, 0.6574999999999999734, 0.6600000000000000311, 0.6624999999999999778, 0.6650000000000000355, 0.6674999999999999822, 0.6700000000000000400, 0.6724999999999999867, 0.6750000000000000444, 0.6774999999999999911, 0.6800000000000000488, 0.6824999999999999956, 0.6850000000000000533, 0.6875000000000000000, 0.6899999999999999467, 0.6925000000000000044, 0.6949999999999999512, 0.6975000000000000089, 0.6999999999999999556, 0.7025000000000000133, 0.7049999999999999600, 0.7075000000000000178, 0.7099999999999999645, 0.7125000000000000222, 0.7149999999999999689, 0.7175000000000000266, 0.7199999999999999734, 0.7225000000000000311, 0.7249999999999999778, 0.7275000000000000355, 0.7299999999999999822, 0.7325000000000000400, 0.7349999999999999867, 0.7375000000000000444, 0.7399999999999999911, 0.7425000000000000488, 0.7449999999999999956, 0.7475000000000000533, 0.7500000000000000000, 0.7524999999999999467, 0.7550000000000000044, 0.7574999999999999512, 0.7600000000000000089, 0.7624999999999999556, 0.7650000000000000133, 0.7674999999999999600, 0.7700000000000000178, 0.7724999999999999645, 0.7750000000000000222, 0.7774999999999999689, 0.7800000000000000266, 0.7824999999999999734, 0.7850000000000000311, 0.7874999999999999778, 0.7900000000000000355, 0.7924999999999999822, 0.7950000000000000400, 0.7974999999999999867, 0.8000000000000000444, 0.8024999999999999911, 0.8050000000000000488, 0.8074999999999999956, 0.8100000000000000533, 0.8125000000000000000, 0.8149999999999999467, 0.8175000000000000044, 0.8199999999999999512, 0.8225000000000000089, 0.8249999999999999556, 0.8275000000000000133, 0.8299999999999999600, 0.8325000000000000178, 0.8349999999999999645, 0.8375000000000000222, 0.8399999999999999689, 0.8425000000000000266, 0.8449999999999999734, 0.8475000000000000311, 0.8499999999999999778, 0.8525000000000000355, 0.8549999999999999822, 0.8575000000000000400, 0.8599999999999999867, 0.8625000000000000444, 0.8649999999999999911, 0.8675000000000000488, 0.8699999999999999956, 0.8725000000000000533, 0.8750000000000000000, 0.8774999999999999467, 0.8800000000000000044, 0.8824999999999999512, 0.8850000000000000089, 0.8874999999999999556, 0.8900000000000000133, 0.8924999999999999600, 0.8950000000000000178, 0.8974999999999999645, 0.9000000000000000222, 0.9024999999999999689, 0.9050000000000000266, 0.9074999999999999734, 0.9100000000000000311, 0.9124999999999999778, 0.9150000000000000355, 0.9174999999999999822, 0.9200000000000000400, 0.9224999999999999867, 0.9250000000000000444, 0.9274999999999999911, 0.9300000000000000488, 0.9324999999999999956, 0.9350000000000000533, 0.9375000000000000000, 0.9399999999999999467, 0.9425000000000000044, 0.9449999999999999512, 0.9475000000000000089, 0.9499999999999999556, 0.9525000000000000133, 0.9549999999999999600, 0.9575000000000000178, 0.9599999999999999645, 0.9625000000000000222, 0.9649999999999999689, 0.9675000000000000266, 0.9699999999999999734, 0.9725000000000000311, 0.9749999999999999778, 0.9775000000000000355, 0.9799999999999999822, 0.9825000000000000400, 0.9849999999999999867, 0.9875000000000000444, 0.9899999999999999911, 0.9925000000000000488, 0.9949999999999999956, 0.9975000000000000533, 1.000000000000000000 ),
 .UNSPECIFIED. ) 
 GEOMETRIC_REPRESENTATION_ITEM ( )  RATIONAL_B_SPLINE_SURFACE ( (
 ( 1.000000000000000000, 0.9238795325112869605, 1.000000000000000000, 0.9238795325112869605, 1.000000000000000000, 0.9238795325112869605, 1.000000000000000000, 0.9238795325112869605, 1.000000000000000000, 0.9238795325112869605, 1.000000000000000000, 0.9238795325112869605, 1.000000000000000000, 0.9238795325112869605, 1.000000000000000000, 0.9238795325112869605, 1.000000000000000000, 0.9238795325112869605, 1.000000000000000000, 0.9238795325112869605, 1.000000000000000000, 0.9238795325112869605, 1.000000000000000000, 0.9238795325112869605, 1.000000000000000000, 0.9238795325112869605, 1.000000000000000000, 0.9238795325112869605, 1.000000000000000000, 0.9238795325112869605, 1.000000000000000000, 0.9238795325112869605, 1.000000000000000000, 0.9238795325112869605, 1.000000000000000000, 0.9238795325112869605, 1.000000000000000000, 0.9238795325112869605, 1.000000000000000000, 0.9238795325112869605, 1.000000000000000000, 0.9238795325112869605, 1.000000000000000000, 0.9238795325112869605, 1.000000000000000000, 0.9238795325112869605, 1.000000000000000000, 0.9238795325112869605, 1.000000000000000000, 0.9238795325112869605, 1.000000000000000000, 0.9238795325112869605, 1.000000000000000000, 0.9238795325112869605, 1.000000000000000000, 0.9238795325112869605, 1.000000000000000000, 0.9238795325112869605, 1.000000000000000000, 0.9238795325112869605, 1.000000000000000000, 0.9238795325112869605, 1.000000000000000000, 0.9238795325112869605, 1.000000000000000000, 0.9238795325112869605, 1.000000000000000000, 0.9238795325112869605, 1.000000000000000000, 0.9238795325112869605, 1.000000000000000000, 0.9238795325112869605, 1.000000000000000000, 0.9238795325112869605, 1.000000000000000000, 0.9238795325112869605, 1.000000000000000000, 0.9238795325112869605, 1.000000000000000000, 0.9238795325112869605, 1.000000000000000000, 0.9238795325112869605, 1.000000000000000000, 0.9238795325112869605, 1.000000000000000000, 0.9238795325112869605, 1.000000000000000000, 0.9238795325112869605, 1.000000000000000000, 0.9238795325112869605, 1.000000000000000000, 0.9238795325112869605, 1.000000000000000000, 0.9238795325112869605, 1.000000000000000000, 0.9238795325112869605, 1.000000000000000000, 0.9238795325112869605, 1.000000000000000000, 0.9238795325112869605, 1.000000000000000000, 0.9238795325112869605, 1.000000000000000000, 0.9238795325112869605, 1.000000000000000000, 0.9238795325112869605, 1.000000000000000000, 0.9238795325112869605, 1.000000000000000000, 0.9238795325112869605, 1.000000000000000000, 0.9238795325112869605, 1.000000000000000000, 0.9238795325112869605, 1.000000000000000000, 0.9238795325112869605, 1.000000000000000000, 0.9238795325112869605, 1.000000000000000000, 0.9238795325112869605, 1.000000000000000000, 0.9238795325112869605, 1.000000000000000000, 0.9238795325112869605, 1.000000000000000000, 0.9238795325112869605, 1.000000000000000000, 0.9238795325112869605, 1.000000000000000000, 0.9238795325112869605, 1.000000000000000000, 0.9238795325112869605, 1.000000000000000000, 0.9238795325112869605, 1.000000000000000000, 0.9238795325112869605, 1.000000000000000000, 0.9238795325112869605, 1.000000000000000000, 0.9238795325112869605, 1.000000000000000000, 0.9238795325112869605, 1.000000000000000000, 0.9238795325112869605, 1.000000000000000000, 0.9238795325112869605, 1.000000000000000000, 0.9238795325112869605, 1.000000000000000000, 0.9238795325112869605, 1.000000000000000000, 0.9238795325112869605, 1.000000000000000000, 0.9238795325112869605, 1.000000000000000000, 0.9238795325112869605, 1.000000000000000000, 0.9238795325112869605, 1.000000000000000000, 0.9238795325112869605, 1.000000000000000000, 0.9238795325112869605, 1.000000000000000000, 0.9238795325112869605, 1.000000000000000000, 0.9238795325112869605, 1.000000000000000000, 0.9238795325112869605, 1.000000000000000000, 0.9238795325112869605, 1.000000000000000000, 0.9238795325112869605, 1.000000000000000000, 0.9238795325112869605, 1.000000000000000000, 0.9238795325112869605, 1.000000000000000000, 0.9238795325112869605, 1.000000000000000000, 0.9238795325112869605, 1.000000000000000000, 0.9238795325112869605, 1.000000000000000000, 0.9238795325112869605, 1.000000000000000000, 0.9238795325112869605, 1.000000000000000000, 0.9238795325112869605, 1.000000000000000000, 0.9238795325112869605, 1.000000000000000000, 0.9238795325112869605, 1.000000000000000000, 0.9238795325112869605, 1.000000000000000000, 0.9238795325112869605, 1.000000000000000000, 0.9238795325112869605, 1.000000000000000000, 0.9238795325112869605, 1.000000000000000000, 0.9238795325112869605, 1.000000000000000000, 0.9238795325112869605, 1.000000000000000000, 0.9238795325112869605, 1.000000000000000000, 0.9238795325112869605, 1.000000000000000000, 0.9238795325112869605, 1.000000000000000000, 0.9238795325112869605, 1.000000000000000000, 0.9238795325112869605, 1.000000000000000000, 0.9238795325112869605, 1.000000000000000000, 0.9238795325112869605, 1.000000000000000000, 0.9238795325112869605, 1.000000000000000000, 0.9238795325112869605, 1.000000000000000000, 0.9238795325112869605, 1.000000000000000000, 0.9238795325112869605, 1.000000000000000000, 0.9238795325112869605, 1.000000000000000000, 0.9238795325112869605, 1.000000000000000000, 0.9238795325112869605, 1.000000000000000000, 0.9238795325112869605, 1.000000000000000000, 0.9238795325112869605, 1.000000000000000000, 0.9238795325112869605, 1.000000000000000000, 0.9238795325112869605, 1.000000000000000000, 0.9238795325112869605, 1.000000000000000000, 0.9238795325112869605, 1.000000000000000000, 0.9238795325112869605, 1.000000000000000000, 0.9238795325112869605, 1.000000000000000000, 0.9238795325112869605, 1.000000000000000000, 0.9238795325112869605, 1.000000000000000000, 0.9238795325112869605, 1.000000000000000000, 0.9238795325112869605, 1.000000000000000000, 0.9238795325112869605, 1.000000000000000000, 0.9238795325112869605, 1.000000000000000000, 0.9238795325112869605, 1.000000000000000000, 0.9238795325112869605, 1.000000000000000000, 0.9238795325112869605, 1.000000000000000000, 0.9238795325112869605, 1.000000000000000000, 0.9238795325112869605, 1.000000000000000000, 0.9238795325112869605, 1.000000000000000000, 0.9238795325112869605, 1.000000000000000000, 0.9238795325112869605, 1.000000000000000000, 0.9238795325112869605, 1.000000000000000000, 0.9238795325112869605, 1.000000000000000000, 0.9238795325112869605, 1.000000000000000000, 0.9238795325112869605, 1.000000000000000000, 0.9238795325112869605, 1.000000000000000000, 0.9238795325112869605, 1.000000000000000000, 0.9238795325112869605, 1.000000000000000000, 0.9238795325112869605, 1.000000000000000000, 0.9238795325112869605, 1.000000000000000000, 0.9238795325112869605, 1.000000000000000000, 0.9238795325112869605, 1.000000000000000000, 0.9238795325112869605, 1.000000000000000000, 0.9238795325112869605, 1.000000000000000000, 0.9238795325112869605, 1.000000000000000000, 0.9238795325112869605, 1.000000000000000000, 0.9238795325112869605, 1.000000000000000000, 0.9238795325112869605, 1.000000000000000000, 0.9238795325112869605, 1.000000000000000000, 0.9238795325112869605, 1.000000000000000000, 0.9238795325112869605, 1.000000000000000000, 0.9238795325112869605, 1.000000000000000000, 0.9238795325112869605, 1.000000000000000000, 0.9238795325112869605, 1.000000000000000000, 0.9238795325112869605, 1.000000000000000000, 0.9238795325112869605, 1.000000000000000000, 0.9238795325112869605, 1.000000000000000000, 0.9238795325112869605, 1.000000000000000000, 0.9238795325112869605, 1.000000000000000000, 0.9238795325112869605, 1.000000000000000000, 0.9238795325112869605, 1.000000000000000000, 0.9238795325112869605, 1.000000000000000000, 0.9238795325112869605, 1.000000000000000000, 0.9238795325112869605, 1.000000000000000000, 0.9238795325112869605, 1.000000000000000000, 0.9238795325112869605, 1.000000000000000000, 0.9238795325112869605, 1.000000000000000000, 0.9238795325112869605, 1.000000000000000000, 0.9238795325112869605, 1.000000000000000000, 0.9238795325112869605, 1.000000000000000000, 0.9238795325112869605, 1.000000000000000000, 0.9238795325112869605, 1.000000000000000000, 0.9238795325112869605, 1.000000000000000000, 0.9238795325112869605, 1.000000000000000000, 0.9238795325112869605, 1.000000000000000000, 0.9238795325112869605, 1.000000000000000000, 0.9238795325112869605, 1.000000000000000000, 0.9238795325112869605, 1.000000000000000000, 0.9238795325112869605, 1.000000000000000000, 0.9238795325112869605, 1.000000000000000000, 0.9238795325112869605, 1.000000000000000000, 0.9238795325112869605, 1.000000000000000000, 0.9238795325112869605, 1.000000000000000000, 0.9238795325112869605, 1.000000000000000000, 0.9238795325112869605, 1.000000000000000000, 0.9238795325112869605, 1.000000000000000000, 0.9238795325112869605, 1.000000000000000000, 0.9238795325112869605, 1.000000000000000000, 0.9238795325112869605, 1.000000000000000000, 0.9238795325112869605, 1.000000000000000000, 0.9238795325112869605, 1.000000000000000000, 0.9238795325112869605, 1.000000000000000000, 0.9238795325112869605, 1.000000000000000000, 0.9238795325112869605, 1.000000000000000000, 0.9238795325112869605, 1.000000000000000000, 0.9238795325112869605, 1.000000000000000000, 0.9238795325112869605, 1.000000000000000000, 0.9238795325112869605, 1.000000000000000000, 0.9238795325112869605, 1.000000000000000000, 0.9238795325112869605, 1.000000000000000000, 0.9238795325112869605, 1.000000000000000000, 0.9238795325112869605, 1.000000000000000000, 0.9238795325112869605, 1.000000000000000000, 0.9238795325112869605, 1.000000000000000000, 0.9238795325112869605, 1.000000000000000000, 0.9238795325112869605, 1.000000000000000000, 0.9238795325112869605, 1.000000000000000000, 0.9238795325112869605, 1.000000000000000000, 0.9238795325112869605, 1.000000000000000000, 0.9238795325112869605, 1.000000000000000000, 0.9238795325112869605, 1.000000000000000000, 0.9238795325112869605, 1.000000000000000000, 0.9238795325112869605, 1.000000000000000000, 0.9238795325112869605, 1.000000000000000000, 0.9238795325112869605, 1.000000000000000000, 0.9238795325112869605, 1.000000000000000000, 0.9238795325112869605, 1.000000000000000000, 0.9238795325112869605, 1.000000000000000000, 0.9238795325112869605, 1.000000000000000000, 0.9238795325112869605, 1.000000000000000000, 0.9238795325112869605, 1.000000000000000000, 0.9238795325112869605, 1.000000000000000000, 0.9238795325112869605, 1.000000000000000000, 0.9238795325112869605, 1.000000000000000000, 0.9238795325112869605, 1.000000000000000000, 0.9238795325112869605, 1.000000000000000000, 0.9238795325112869605, 1.000000000000000000, 0.9238795325112869605, 1.000000000000000000, 0.9238795325112869605, 1.000000000000000000, 0.9238795325112869605, 1.000000000000000000, 0.9238795325112869605, 1.000000000000000000, 0.9238795325112869605, 1.000000000000000000, 0.9238795325112869605, 1.000000000000000000, 0.9238795325112869605, 1.000000000000000000, 0.9238795325112869605, 1.000000000000000000, 0.9238795325112869605, 1.000000000000000000, 0.9238795325112869605, 1.000000000000000000, 0.9238795325112869605, 1.000000000000000000, 0.9238795325112869605, 1.000000000000000000, 0.9238795325112869605, 1.000000000000000000, 0.9238795325112869605, 1.000000000000000000, 0.9238795325112869605, 1.000000000000000000, 0.9238795325112869605, 1.000000000000000000, 0.9238795325112869605, 1.000000000000000000, 0.9238795325112869605, 1.000000000000000000, 0.9238795325112869605, 1.000000000000000000, 0.9238795325112869605, 1.000000000000000000, 0.9238795325112869605, 1.000000000000000000, 0.9238795325112869605, 1.000000000000000000, 0.9238795325112869605, 1.000000000000000000, 0.9238795325112869605, 1.000000000000000000, 0.9238795325112869605, 1.000000000000000000, 0.9238795325112869605, 1.000000000000000000, 0.9238795325112869605, 1.000000000000000000, 0.9238795325112869605, 1.000000000000000000, 0.9238795325112869605, 1.000000000000000000, 0.9238795325112869605, 1.000000000000000000, 0.9238795325112869605, 1.000000000000000000, 0.9238795325112869605, 1.000000000000000000, 0.9238795325112869605, 1.000000000000000000, 0.9238795325112869605, 1.000000000000000000, 0.9238795325112869605, 1.000000000000000000, 0.9238795325112869605, 1.000000000000000000, 0.9238795325112869605, 1.000000000000000000, 0.9238795325112869605, 1.000000000000000000, 0.9238795325112869605, 1.000000000000000000, 0.9238795325112869605, 1.000000000000000000, 0.9238795325112869605, 1.000000000000000000, 0.9238795325112869605, 1.000000000000000000, 0.9238795325112869605, 1.000000000000000000, 0.9238795325112869605, 1.000000000000000000, 0.9238795325112869605, 1.000000000000000000, 0.9238795325112869605, 1.000000000000000000, 0.9238795325112869605, 1.000000000000000000, 0.9238795325112869605, 1.000000000000000000, 0.9238795325112869605, 1.000000000000000000, 0.9238795325112869605, 1.000000000000000000, 0.9238795325112869605, 1.000000000000000000, 0.9238795325112869605, 1.000000000000000000, 0.9238795325112869605, 1.000000000000000000, 0.9238795325112869605, 1.000000000000000000, 0.9238795325112869605, 1.000000000000000000, 0.9238795325112869605, 1.000000000000000000, 0.9238795325112869605, 1.000000000000000000, 0.9238795325112869605, 1.000000000000000000, 0.9238795325112869605, 1.000000000000000000, 0.9238795325112869605, 1.000000000000000000, 0.9238795325112869605, 1.000000000000000000, 0.9238795325112869605, 1.000000000000000000, 0.9238795325112869605, 1.000000000000000000, 0.9238795325112869605, 1.000000000000000000, 0.9238795325112869605, 1.000000000000000000, 0.9238795325112869605, 1.000000000000000000, 0.9238795325112869605, 1.000000000000000000, 0.9238795325112869605, 1.000000000000000000, 0.9238795325112869605, 1.000000000000000000, 0.9238795325112869605, 1.000000000000000000, 0.9238795325112869605, 1.000000000000000000, 0.9238795325112869605, 1.000000000000000000, 0.9238795325112869605, 1.000000000000000000, 0.9238795325112869605, 1.000000000000000000, 0.9238795325112869605, 1.000000000000000000, 0.9238795325112869605, 1.000000000000000000, 0.9238795325112869605, 1.000000000000000000, 0.9238795325112869605, 1.000000000000000000, 0.9238795325112869605, 1.000000000000000000, 0.9238795325112869605, 1.000000000000000000, 0.9238795325112869605, 1.000000000000000000, 0.9238795325112869605, 1.000000000000000000, 0.9238795325112869605, 1.000000000000000000, 0.9238795325112869605, 1.000000000000000000, 0.9238795325112869605, 1.000000000000000000, 0.9238795325112869605, 1.000000000000000000, 0.9238795325112869605, 1.000000000000000000, 0.9238795325112869605, 1.000000000000000000, 0.9238795325112869605, 1.000000000000000000, 0.9238795325112869605, 1.000000000000000000, 0.9238795325112869605, 1.000000000000000000, 0.9238795325112869605, 1.000000000000000000, 0.9238795325112869605, 1.000000000000000000, 0.9238795325112869605, 1.000000000000000000, 0.9238795325112869605, 1.000000000000000000, 0.9238795325112869605, 1.000000000000000000, 0.9238795325112869605, 1.000000000000000000, 0.9238795325112869605, 1.000000000000000000, 0.9238795325112869605, 1.000000000000000000, 0.9238795325112869605, 1.000000000000000000, 0.9238795325112869605, 1.000000000000000000, 0.9238795325112869605, 1.000000000000000000, 0.9238795325112869605, 1.000000000000000000, 0.9238795325112869605, 1.000000000000000000, 0.9238795325112869605, 1.000000000000000000, 0.9238795325112869605, 1.000000000000000000, 0.9238795325112869605, 1.000000000000000000, 0.9238795325112869605, 1.000000000000000000, 0.9238795325112869605, 1.000000000000000000, 0.9238795325112869605, 1.000000000000000000, 0.9238795325112869605, 1.000000000000000000, 0.9238795325112869605, 1.000000000000000000, 0.9238795325112869605, 1.000000000000000000, 0.9238795325112869605, 1.000000000000000000, 0.9238795325112869605, 1.000000000000000000, 0.9238795325112869605, 1.000000000000000000, 0.9238795325112869605, 1.000000000000000000, 0.9238795325112869605, 1.000000000000000000, 0.9238795325112869605, 1.000000000000000000, 0.9238795325112869605, 1.000000000000000000, 0.9238795325112869605, 1.000000000000000000, 0.9238795325112869605, 1.000000000000000000, 0.9238795325112869605, 1.000000000000000000, 0.9238795325112869605, 1.000000000000000000, 0.9238795325112869605, 1.000000000000000000, 0.9238795325112869605, 1.000000000000000000, 0.9238795325112869605, 1.000000000000000000, 0.9238795325112869605, 1.000000000000000000, 0.9238795325112869605, 1.000000000000000000, 0.9238795325112869605, 1.000000000000000000, 0.9238795325112869605, 1.000000000000000000, 0.9238795325112869605, 1.000000000000000000, 0.9238795325112869605, 1.000000000000000000, 0.9238795325112869605, 1.000000000000000000, 0.9238795325112869605, 1.000000000000000000, 0.9238795325112869605, 1.000000000000000000, 0.9238795325112869605, 1.000000000000000000, 0.9238795325112869605, 1.000000000000000000, 0.9238795325112869605, 1.000000000000000000, 0.9238795325112869605, 1.000000000000000000, 0.9238795325112869605, 1.000000000000000000, 0.9238795325112869605, 1.000000000000000000, 0.9238795325112869605, 1.000000000000000000, 0.9238795325112869605, 1.000000000000000000, 0.9238795325112869605, 1.000000000000000000, 0.9238795325112869605, 1.000000000000000000, 0.9238795325112869605, 1.000000000000000000, 0.9238795325112869605, 1.000000000000000000, 0.9238795325112869605, 1.000000000000000000, 0.9238795325112869605, 1.000000000000000000, 0.9238795325112869605, 1.000000000000000000, 0.9238795325112869605, 1.000000000000000000, 0.9238795325112869605, 1.000000000000000000, 0.9238795325112869605, 1.000000000000000000, 0.9238795325112869605, 1.000000000000000000, 0.9238795325112869605, 1.000000000000000000, 0.9238795325112869605, 1.000000000000000000, 0.9238795325112869605, 1.000000000000000000, 0.9238795325112869605, 1.000000000000000000, 0.9238795325112869605, 1.000000000000000000, 0.9238795325112869605, 1.000000000000000000, 0.9238795325112869605, 1.000000000000000000, 0.9238795325112869605, 1.000000000000000000, 0.9238795325112869605, 1.000000000000000000, 0.9238795325112869605, 1.000000000000000000, 0.9238795325112869605, 1.000000000000000000),
 ( 1.000000000000000000, 0.9238795325112869605, 1.000000000000000000, 0.9238795325112869605, 1.000000000000000000, 0.9238795325112869605, 1.000000000000000000, 0.9238795325112869605, 1.000000000000000000, 0.9238795325112869605, 1.000000000000000000, 0.9238795325112869605, 1.000000000000000000, 0.9238795325112869605, 1.000000000000000000, 0.9238795325112869605, 1.000000000000000000, 0.9238795325112869605, 1.000000000000000000, 0.9238795325112869605, 1.000000000000000000, 0.9238795325112869605, 1.000000000000000000, 0.9238795325112869605, 1.000000000000000000, 0.9238795325112869605, 1.000000000000000000, 0.9238795325112869605, 1.000000000000000000, 0.9238795325112869605, 1.000000000000000000, 0.9238795325112869605, 1.000000000000000000, 0.9238795325112869605, 1.000000000000000000, 0.9238795325112869605, 1.000000000000000000, 0.9238795325112869605, 1.000000000000000000, 0.9238795325112869605, 1.000000000000000000, 0.9238795325112869605, 1.000000000000000000, 0.9238795325112869605, 1.000000000000000000, 0.9238795325112869605, 1.000000000000000000, 0.9238795325112869605, 1.000000000000000000, 0.9238795325112869605, 1.000000000000000000, 0.9238795325112869605, 1.000000000000000000, 0.9238795325112869605, 1.000000000000000000, 0.9238795325112869605, 1.000000000000000000, 0.9238795325112869605, 1.000000000000000000, 0.9238795325112869605, 1.000000000000000000, 0.9238795325112869605, 1.000000000000000000, 0.9238795325112869605, 1.000000000000000000, 0.9238795325112869605, 1.000000000000000000, 0.9238795325112869605, 1.000000000000000000, 0.9238795325112869605, 1.000000000000000000, 0.9238795325112869605, 1.000000000000000000, 0.9238795325112869605, 1.000000000000000000, 0.9238795325112869605, 1.000000000000000000, 0.9238795325112869605, 1.000000000000000000, 0.9238795325112869605, 1.000000000000000000, 0.9238795325112869605, 1.000000000000000000, 0.9238795325112869605, 1.000000000000000000, 0.9238795325112869605, 1.000000000000000000, 0.9238795325112869605, 1.000000000000000000, 0.9238795325112869605, 1.000000000000000000, 0.9238795325112869605, 1.000000000000000000, 0.9238795325112869605, 1.000000000000000000, 0.9238795325112869605, 1.000000000000000000, 0.9238795325112869605, 1.000000000000000000, 0.9238795325112869605, 1.000000000000000000, 0.9238795325112869605, 1.000000000000000000, 0.9238795325112869605, 1.000000000000000000, 0.9238795325112869605, 1.000000000000000000, 0.9238795325112869605, 1.000000000000000000, 0.9238795325112869605, 1.000000000000000000, 0.9238795325112869605, 1.000000000000000000, 0.9238795325112869605, 1.000000000000000000, 0.9238795325112869605, 1.000000000000000000, 0.9238795325112869605, 1.000000000000000000, 0.9238795325112869605, 1.000000000000000000, 0.9238795325112869605, 1.000000000000000000, 0.9238795325112869605, 1.000000000000000000, 0.9238795325112869605, 1.000000000000000000, 0.9238795325112869605, 1.000000000000000000, 0.9238795325112869605, 1.000000000000000000, 0.9238795325112869605, 1.000000000000000000, 0.9238795325112869605, 1.000000000000000000, 0.9238795325112869605, 1.000000000000000000, 0.9238795325112869605, 1.000000000000000000, 0.9238795325112869605, 1.000000000000000000, 0.9238795325112869605, 1.000000000000000000, 0.9238795325112869605, 1.000000000000000000, 0.9238795325112869605, 1.000000000000000000, 0.9238795325112869605, 1.000000000000000000, 0.9238795325112869605, 1.000000000000000000, 0.9238795325112869605, 1.000000000000000000, 0.9238795325112869605, 1.000000000000000000, 0.9238795325112869605, 1.000000000000000000, 0.9238795325112869605, 1.000000000000000000, 0.9238795325112869605, 1.000000000000000000, 0.9238795325112869605, 1.000000000000000000, 0.9238795325112869605, 1.000000000000000000, 0.9238795325112869605, 1.000000000000000000, 0.9238795325112869605, 1.000000000000000000, 0.9238795325112869605, 1.000000000000000000, 0.9238795325112869605, 1.000000000000000000, 0.9238795325112869605, 1.000000000000000000, 0.9238795325112869605, 1.000000000000000000, 0.9238795325112869605, 1.000000000000000000, 0.9238795325112869605, 1.000000000000000000, 0.9238795325112869605, 1.000000000000000000, 0.9238795325112869605, 1.000000000000000000, 0.9238795325112869605, 1.000000000000000000, 0.9238795325112869605, 1.000000000000000000, 0.9238795325112869605, 1.000000000000000000, 0.9238795325112869605, 1.000000000000000000, 0.9238795325112869605, 1.000000000000000000, 0.9238795325112869605, 1.000000000000000000, 0.9238795325112869605, 1.000000000000000000, 0.9238795325112869605, 1.000000000000000000, 0.9238795325112869605, 1.000000000000000000, 0.9238795325112869605, 1.000000000000000000, 0.9238795325112869605, 1.000000000000000000, 0.9238795325112869605, 1.000000000000000000, 0.9238795325112869605, 1.000000000000000000, 0.9238795325112869605, 1.000000000000000000, 0.9238795325112869605, 1.000000000000000000, 0.9238795325112869605, 1.000000000000000000, 0.9238795325112869605, 1.000000000000000000, 0.9238795325112869605, 1.000000000000000000, 0.9238795325112869605, 1.000000000000000000, 0.9238795325112869605, 1.000000000000000000, 0.9238795325112869605, 1.000000000000000000, 0.9238795325112869605, 1.000000000000000000, 0.9238795325112869605, 1.000000000000000000, 0.9238795325112869605, 1.000000000000000000, 0.9238795325112869605, 1.000000000000000000, 0.9238795325112869605, 1.000000000000000000, 0.9238795325112869605, 1.000000000000000000, 0.9238795325112869605, 1.000000000000000000, 0.9238795325112869605, 1.000000000000000000, 0.9238795325112869605, 1.000000000000000000, 0.9238795325112869605, 1.000000000000000000, 0.9238795325112869605, 1.000000000000000000, 0.9238795325112869605, 1.000000000000000000, 0.9238795325112869605, 1.000000000000000000, 0.9238795325112869605, 1.000000000000000000, 0.9238795325112869605, 1.000000000000000000, 0.9238795325112869605, 1.000000000000000000, 0.9238795325112869605, 1.000000000000000000, 0.9238795325112869605, 1.000000000000000000, 0.9238795325112869605, 1.000000000000000000, 0.9238795325112869605, 1.000000000000000000, 0.9238795325112869605, 1.000000000000000000, 0.9238795325112869605, 1.000000000000000000, 0.9238795325112869605, 1.000000000000000000, 0.9238795325112869605, 1.000000000000000000, 0.9238795325112869605, 1.000000000000000000, 0.9238795325112869605, 1.000000000000000000, 0.9238795325112869605, 1.000000000000000000, 0.9238795325112869605, 1.000000000000000000, 0.9238795325112869605, 1.000000000000000000, 0.9238795325112869605, 1.000000000000000000, 0.9238795325112869605, 1.000000000000000000, 0.9238795325112869605, 1.000000000000000000, 0.9238795325112869605, 1.000000000000000000, 0.9238795325112869605, 1.000000000000000000, 0.9238795325112869605, 1.000000000000000000, 0.9238795325112869605, 1.000000000000000000, 0.9238795325112869605, 1.000000000000000000, 0.9238795325112869605, 1.000000000000000000, 0.9238795325112869605, 1.000000000000000000, 0.9238795325112869605, 1.000000000000000000, 0.9238795325112869605, 1.000000000000000000, 0.9238795325112869605, 1.000000000000000000, 0.9238795325112869605, 1.000000000000000000, 0.9238795325112869605, 1.000000000000000000, 0.9238795325112869605, 1.000000000000000000, 0.9238795325112869605, 1.000000000000000000, 0.9238795325112869605, 1.000000000000000000, 0.9238795325112869605, 1.000000000000000000, 0.9238795325112869605, 1.000000000000000000, 0.9238795325112869605, 1.000000000000000000, 0.9238795325112869605, 1.000000000000000000, 0.9238795325112869605, 1.000000000000000000, 0.9238795325112869605, 1.000000000000000000, 0.9238795325112869605, 1.000000000000000000, 0.9238795325112869605, 1.000000000000000000, 0.9238795325112869605, 1.000000000000000000, 0.9238795325112869605, 1.000000000000000000, 0.9238795325112869605, 1.000000000000000000, 0.9238795325112869605, 1.000000000000000000, 0.9238795325112869605, 1.000000000000000000, 0.9238795325112869605, 1.000000000000000000, 0.9238795325112869605, 1.000000000000000000, 0.9238795325112869605, 1.000000000000000000, 0.9238795325112869605, 1.000000000000000000, 0.9238795325112869605, 1.000000000000000000, 0.9238795325112869605, 1.000000000000000000, 0.9238795325112869605, 1.000000000000000000, 0.9238795325112869605, 1.000000000000000000, 0.9238795325112869605, 1.000000000000000000, 0.9238795325112869605, 1.000000000000000000, 0.9238795325112869605, 1.000000000000000000, 0.9238795325112869605, 1.000000000000000000, 0.9238795325112869605, 1.000000000000000000, 0.9238795325112869605, 1.000000000000000000, 0.9238795325112869605, 1.000000000000000000, 0.9238795325112869605, 1.000000000000000000, 0.9238795325112869605, 1.000000000000000000, 0.9238795325112869605, 1.000000000000000000, 0.9238795325112869605, 1.000000000000000000, 0.9238795325112869605, 1.000000000000000000, 0.9238795325112869605, 1.000000000000000000, 0.9238795325112869605, 1.000000000000000000, 0.9238795325112869605, 1.000000000000000000, 0.9238795325112869605, 1.000000000000000000, 0.9238795325112869605, 1.000000000000000000, 0.9238795325112869605, 1.000000000000000000, 0.9238795325112869605, 1.000000000000000000, 0.9238795325112869605, 1.000000000000000000, 0.9238795325112869605, 1.000000000000000000, 0.9238795325112869605, 1.000000000000000000, 0.9238795325112869605, 1.000000000000000000, 0.9238795325112869605, 1.000000000000000000, 0.9238795325112869605, 1.000000000000000000, 0.9238795325112869605, 1.000000000000000000, 0.9238795325112869605, 1.000000000000000000, 0.9238795325112869605, 1.000000000000000000, 0.9238795325112869605, 1.000000000000000000, 0.9238795325112869605, 1.000000000000000000, 0.9238795325112869605, 1.000000000000000000, 0.9238795325112869605, 1.000000000000000000, 0.9238795325112869605, 1.000000000000000000, 0.9238795325112869605, 1.000000000000000000, 0.9238795325112869605, 1.000000000000000000, 0.9238795325112869605, 1.000000000000000000, 0.9238795325112869605, 1.000000000000000000, 0.9238795325112869605, 1.000000000000000000, 0.9238795325112869605, 1.000000000000000000, 0.9238795325112869605, 1.000000000000000000, 0.9238795325112869605, 1.000000000000000000, 0.9238795325112869605, 1.000000000000000000, 0.9238795325112869605, 1.000000000000000000, 0.9238795325112869605, 1.000000000000000000, 0.9238795325112869605, 1.000000000000000000, 0.9238795325112869605, 1.000000000000000000, 0.9238795325112869605, 1.000000000000000000, 0.9238795325112869605, 1.000000000000000000, 0.9238795325112869605, 1.000000000000000000, 0.9238795325112869605, 1.000000000000000000, 0.9238795325112869605, 1.000000000000000000, 0.9238795325112869605, 1.000000000000000000, 0.9238795325112869605, 1.000000000000000000, 0.9238795325112869605, 1.000000000000000000, 0.9238795325112869605, 1.000000000000000000, 0.9238795325112869605, 1.000000000000000000, 0.9238795325112869605, 1.000000000000000000, 0.9238795325112869605, 1.000000000000000000, 0.9238795325112869605, 1.000000000000000000, 0.9238795325112869605, 1.000000000000000000, 0.9238795325112869605, 1.000000000000000000, 0.9238795325112869605, 1.000000000000000000, 0.9238795325112869605, 1.000000000000000000, 0.9238795325112869605, 1.000000000000000000, 0.9238795325112869605, 1.000000000000000000, 0.9238795325112869605, 1.000000000000000000, 0.9238795325112869605, 1.000000000000000000, 0.9238795325112869605, 1.000000000000000000, 0.9238795325112869605, 1.000000000000000000, 0.9238795325112869605, 1.000000000000000000, 0.9238795325112869605, 1.000000000000000000, 0.9238795325112869605, 1.000000000000000000, 0.9238795325112869605, 1.000000000000000000, 0.9238795325112869605, 1.000000000000000000, 0.9238795325112869605, 1.000000000000000000, 0.9238795325112869605, 1.000000000000000000, 0.9238795325112869605, 1.000000000000000000, 0.9238795325112869605, 1.000000000000000000, 0.9238795325112869605, 1.000000000000000000, 0.9238795325112869605, 1.000000000000000000, 0.9238795325112869605, 1.000000000000000000, 0.9238795325112869605, 1.000000000000000000, 0.9238795325112869605, 1.000000000000000000, 0.9238795325112869605, 1.000000000000000000, 0.9238795325112869605, 1.000000000000000000, 0.9238795325112869605, 1.000000000000000000, 0.9238795325112869605, 1.000000000000000000, 0.9238795325112869605, 1.000000000000000000, 0.9238795325112869605, 1.000000000000000000, 0.9238795325112869605, 1.000000000000000000, 0.9238795325112869605, 1.000000000000000000, 0.9238795325112869605, 1.000000000000000000, 0.9238795325112869605, 1.000000000000000000, 0.9238795325112869605, 1.000000000000000000, 0.9238795325112869605, 1.000000000000000000, 0.9238795325112869605, 1.000000000000000000, 0.9238795325112869605, 1.000000000000000000, 0.9238795325112869605, 1.000000000000000000, 0.9238795325112869605, 1.000000000000000000, 0.9238795325112869605, 1.000000000000000000, 0.9238795325112869605, 1.000000000000000000, 0.9238795325112869605, 1.000000000000000000, 0.9238795325112869605, 1.000000000000000000, 0.9238795325112869605, 1.000000000000000000, 0.9238795325112869605, 1.000000000000000000, 0.9238795325112869605, 1.000000000000000000, 0.9238795325112869605, 1.000000000000000000, 0.9238795325112869605, 1.000000000000000000, 0.9238795325112869605, 1.000000000000000000, 0.9238795325112869605, 1.000000000000000000, 0.9238795325112869605, 1.000000000000000000, 0.9238795325112869605, 1.000000000000000000, 0.9238795325112869605, 1.000000000000000000, 0.9238795325112869605, 1.000000000000000000, 0.9238795325112869605, 1.000000000000000000, 0.9238795325112869605, 1.000000000000000000, 0.9238795325112869605, 1.000000000000000000, 0.9238795325112869605, 1.000000000000000000, 0.9238795325112869605, 1.000000000000000000, 0.9238795325112869605, 1.000000000000000000, 0.9238795325112869605, 1.000000000000000000, 0.9238795325112869605, 1.000000000000000000, 0.9238795325112869605, 1.000000000000000000, 0.9238795325112869605, 1.000000000000000000, 0.9238795325112869605, 1.000000000000000000, 0.9238795325112869605, 1.000000000000000000, 0.9238795325112869605, 1.000000000000000000, 0.9238795325112869605, 1.000000000000000000, 0.9238795325112869605, 1.000000000000000000, 0.9238795325112869605, 1.000000000000000000, 0.9238795325112869605, 1.000000000000000000, 0.9238795325112869605, 1.000000000000000000, 0.9238795325112869605, 1.000000000000000000, 0.9238795325112869605, 1.000000000000000000, 0.9238795325112869605, 1.000000000000000000, 0.9238795325112869605, 1.000000000000000000, 0.9238795325112869605, 1.000000000000000000, 0.9238795325112869605, 1.000000000000000000, 0.9238795325112869605, 1.000000000000000000, 0.9238795325112869605, 1.000000000000000000, 0.9238795325112869605, 1.000000000000000000, 0.9238795325112869605, 1.000000000000000000, 0.9238795325112869605, 1.000000000000000000, 0.9238795325112869605, 1.000000000000000000, 0.9238795325112869605, 1.000000000000000000, 0.9238795325112869605, 1.000000000000000000, 0.9238795325112869605, 1.000000000000000000, 0.9238795325112869605, 1.000000000000000000, 0.9238795325112869605, 1.000000000000000000, 0.9238795325112869605, 1.000000000000000000, 0.9238795325112869605, 1.000000000000000000, 0.9238795325112869605, 1.000000000000000000, 0.9238795325112869605, 1.000000000000000000, 0.9238795325112869605, 1.000000000000000000, 0.9238795325112869605, 1.000000000000000000, 0.9238795325112869605, 1.000000000000000000, 0.9238795325112869605, 1.000000000000000000, 0.9238795325112869605, 1.000000000000000000, 0.9238795325112869605, 1.000000000000000000, 0.9238795325112869605, 1.000000000000000000, 0.9238795325112869605, 1.000000000000000000, 0.9238795325112869605, 1.000000000000000000, 0.9238795325112869605, 1.000000000000000000, 0.9238795325112869605, 1.000000000000000000, 0.9238795325112869605, 1.000000000000000000, 0.9238795325112869605, 1.000000000000000000, 0.9238795325112869605, 1.000000000000000000, 0.9238795325112869605, 1.000000000000000000, 0.9238795325112869605, 1.000000000000000000, 0.9238795325112869605, 1.000000000000000000, 0.9238795325112869605, 1.000000000000000000, 0.9238795325112869605, 1.000000000000000000, 0.9238795325112869605, 1.000000000000000000, 0.9238795325112869605, 1.000000000000000000, 0.9238795325112869605, 1.000000000000000000, 0.9238795325112869605, 1.000000000000000000, 0.9238795325112869605, 1.000000000000000000, 0.9238795325112869605, 1.000000000000000000, 0.9238795325112869605, 1.000000000000000000, 0.9238795325112869605, 1.000000000000000000, 0.9238795325112869605, 1.000000000000000000, 0.9238795325112869605, 1.000000000000000000, 0.9238795325112869605, 1.000000000000000000, 0.9238795325112869605, 1.000000000000000000, 0.9238795325112869605, 1.000000000000000000, 0.9238795325112869605, 1.000000000000000000, 0.9238795325112869605, 1.000000000000000000, 0.9238795325112869605, 1.000000000000000000, 0.9238795325112869605, 1.000000000000000000, 0.9238795325112869605, 1.000000000000000000, 0.9238795325112869605, 1.000000000000000000, 0.9238795325112869605, 1.000000000000000000, 0.9238795325112869605, 1.000000000000000000, 0.9238795325112869605, 1.000000000000000000, 0.9238795325112869605, 1.000000000000000000, 0.9238795325112869605, 1.000000000000000000, 0.9238795325112869605, 1.000000000000000000, 0.9238795325112869605, 1.000000000000000000, 0.9238795325112869605, 1.000000000000000000, 0.9238795325112869605, 1.000000000000000000, 0.9238795325112869605, 1.000000000000000000, 0.9238795325112869605, 1.000000000000000000, 0.9238795325112869605, 1.000000000000000000, 0.9238795325112869605, 1.000000000000000000, 0.9238795325112869605, 1.000000000000000000, 0.9238795325112869605, 1.000000000000000000, 0.9238795325112869605, 1.000000000000000000, 0.9238795325112869605, 1.000000000000000000, 0.9238795325112869605, 1.000000000000000000, 0.9238795325112869605, 1.000000000000000000, 0.9238795325112869605, 1.000000000000000000, 0.9238795325112869605, 1.000000000000000000, 0.9238795325112869605, 1.000000000000000000, 0.9238795325112869605, 1.000000000000000000, 0.9238795325112869605, 1.000000000000000000, 0.9238795325112869605, 1.000000000000000000, 0.9238795325112869605, 1.000000000000000000, 0.9238795325112869605, 1.000000000000000000, 0.9238795325112869605, 1.000000000000000000) ) ) 
 REPRESENTATION_ITEM ( '' )  SURFACE ( )  ) ;
#46834 = CARTESIAN_POINT ( 'NONE',  ( 1.054774247047244540, 0.07405724077823318263, 0.1033464566391498751 ) ) ;
#46836 = EDGE_CURVE ( 'NONE', #35869, #39913, #16273, .T. ) ;
#46838 = CARTESIAN_POINT ( 'NONE',  ( -0.8107537697050254399, 0.1574803149606300301, 1.951279527559056870 ) ) ;
#46837 = CARTESIAN_POINT ( 'NONE',  ( 0.9500414927467377701, 0.1787899950787401604, 1.210629921206079818 ) ) ;
#46839 = CARTESIAN_POINT ( 'NONE',  ( 1.033464566929134687, -0.06523048226347956391, 0.4306102361129448552 ) ) ;
#46840 = ORIENTED_EDGE ( 'NONE', *, *, #8935, .T. ) ;
#46841 = CARTESIAN_POINT ( 'NONE',  ( -0.6195511811023656223, 0.9842519685039370358, -1.186023622047243986 ) ) ;
#46842 = EDGE_CURVE ( 'NONE', #36286, #5716, #22967, .T. ) ;
#46843 = CARTESIAN_POINT ( 'NONE',  ( 0.8700650591850297433, 0.1747820667289631535, 0.03936860327882610311 ) ) ;
#46844 = CARTESIAN_POINT ( 'NONE',  ( -0.8759842519685039353, -0.1574803149606299191, 0.3444881888688507976 ) ) ;
#46845 = CARTESIAN_POINT ( 'NONE',  ( -0.7646288533564489232, -0.1113553986120547346, 1.530511811023621993 ) ) ;
#46846 = CARTESIAN_POINT ( 'NONE',  ( 1.002407869896990045, 0.1264236179284866091, 1.523129921206078707 ) ) ;
#46847 = EDGE_CURVE ( 'NONE', #8667, #40494, #35929, .T. ) ;
#46848 = CARTESIAN_POINT ( 'NONE',  ( -0.8107537697050254399, -0.1574803149606297803, 1.769192913385826404 ) ) ;
#46849 = CARTESIAN_POINT ( 'NONE',  ( 0.9412147342319837628, -0.1574803149606297803, 1.183562992125983593 ) ) ;
#46850 = CARTESIAN_POINT ( 'NONE',  ( -0.07405724077823318263, -0.07185039364702387743, 0.1787899950787401604 ) ) ;
#46851 = VERTEX_POINT ( 'NONE', #9058 ) ;
#46852 = DIRECTION ( 'NONE',  ( 0.000000000000000000, 0.000000000000000000, 1.000000000000000000 ) ) ;
#46853 = VECTOR ( 'NONE', #8492, 39.37007874015748143 ) ;
#46854 = ORIENTED_EDGE ( 'NONE', *, *, #20886, .T. ) ;
#46855 = CARTESIAN_POINT ( 'NONE',  ( 0.1944374611862057511, 0.07559918600398417288, 0.1731745503097384398 ) ) ;
#46856 = ORIENTED_EDGE ( 'NONE', *, *, #35297, .F. ) ;
#46857 = DIRECTION ( 'NONE',  ( 0.000000000000000000, 0.000000000000000000, 1.000000000000000000 ) ) ;
#46858 = CARTESIAN_POINT ( 'NONE',  ( 1.054774247047244540, -0.07405724077823318263, 0.5364173227808821665 ) ) ;
#46859 = ORIENTED_EDGE ( 'NONE', *, *, #15932, .F. ) ;
#46860 = CARTESIAN_POINT ( 'NONE',  ( -0.1787899950787401604, -1.661417322780881500, -0.07405724077823318263 ) ) ;
#46861 = CARTESIAN_POINT ( 'NONE',  ( -1.054774247047244096, 0.000000000000000000, 1.090059055064346527 ) ) ;
#46862 = AXIS2_PLACEMENT_3D ( 'NONE', #3681, #766, #310 ) ;
#46863 = CIRCLE ( 'NONE', #22366, 0.1574803149606299191 ) ;
#46864 = CARTESIAN_POINT ( 'NONE',  ( -0.9412147342319837628, -0.1574803149606297803, 0.1993110236220472509 ) ) ;
#46865 = EDGE_LOOP ( 'NONE', ( #20224, #42965, #6652, #33504 ) ) ;
#46866 = CARTESIAN_POINT ( 'NONE',  ( -0.7495606340400177148, 0.1264236179284866091, 0.8292322834108031282 ) ) ;
#46867 = CARTESIAN_POINT ( 'NONE',  ( -0.6971942568897626646, 0.07405724077823318263, 0.2017716534895435399 ) ) ;
#46868 = CARTESIAN_POINT ( 'NONE',  ( 4.801428276353606495E-17, 0.03219022224904102836, 0.2854330708661417804 ) ) ;
#46869 = LINE ( 'NONE', #14054, #31298 ) ;
#46870 = CARTESIAN_POINT ( 'NONE',  ( -0.1787899950787401604, -0.7619349918512856590, 0.07405724077823318263 ) ) ;
#46871 = ORIENTED_EDGE ( 'NONE', *, *, #27399, .T. ) ;
#46872 = CARTESIAN_POINT ( 'NONE',  ( -0.7185039370078746268, 0.06523048226347956391, 0.06643700787401589369 ) ) ;
#46873 = CARTESIAN_POINT ( 'NONE',  ( 0.1574803149606299191, -0.5708661417322835607, -6.991093932140394160E-17 ) ) ;
#46874 = ORIENTED_EDGE ( 'NONE', *, *, #36744, .F. ) ;
#46875 = ORIENTED_EDGE ( 'NONE', *, *, #17489, .T. ) ;
#46876 = DIRECTION ( 'NONE',  ( 1.000000000000000000, 0.000000000000000000, -1.822029033848725275E-16 ) ) ;
#46877 = CARTESIAN_POINT ( 'NONE',  ( -0.8019270111902717657, -0.1787899950787401604, 0.6003937007336380693 ) ) ;
#46878 = DIRECTION ( 'NONE',  ( 0.000000000000000000, 0.000000000000000000, -1.000000000000000000 ) ) ;
#46879 = ORIENTED_EDGE ( 'NONE', *, *, #36036, .T. ) ;
#46880 = CARTESIAN_POINT ( 'NONE',  ( -0.6971942568897637749, 2.189545951927499583E-17, 1.779035433017102319 ) ) ;
#46881 = CARTESIAN_POINT ( 'NONE',  ( -9.829250441071060444E-18, -0.006719043512062446329, -0.1377952755905511861 ) ) ;
#46882 = TOROIDAL_SURFACE ( 'NONE', #45340, 0.01968503937007873988, 0.009842519685039369942 ) ;
#46883 = CARTESIAN_POINT ( 'NONE',  ( -0.9873396505805591694, 0.1113553986120547346, 0.4872047244094488416 ) ) ;
#46884 = ORIENTED_EDGE ( 'NONE', *, *, #1721, .F. ) ;
#46885 = CARTESIAN_POINT ( 'NONE',  ( 0.8759842519685039353, -0.1574803149606299191, 0.6299212598425196763 ) ) ;
#46886 = CARTESIAN_POINT ( 'NONE',  ( -0.07444174185955065859, -0.7810477465909202444, 0.1797182628040039087 ) ) ;
#46887 = CARTESIAN_POINT ( 'NONE',  ( -0.9412147342319837628, 0.1574803149606300301, 0.9621062992125994917 ) ) ;
#46888 = CARTESIAN_POINT ( 'NONE',  ( -0.9873396505805591694, 0.1113553986120547346, 1.422244094380661572 ) ) ;
#46889 = CARTESIAN_POINT ( 'NONE',  ( 1.002407869896990045, 0.1264236179284866091, 0.7800196849856062542 ) ) ;
#46890 = CARTESIAN_POINT ( 'NONE',  ( 0.1113553986120547346, -0.6328740157480314821, -0.1113553986120547346 ) ) ;
#46891 = CIRCLE ( 'NONE', #3279, 0.09842519685039370636 ) ;
#46892 = LINE ( 'NONE', #21975, #14655 ) ;
#46893 = CARTESIAN_POINT ( 'NONE',  ( 0.7185039370078746268, -0.06523048226347956391, 1.213090551181103427 ) ) ;
#46895 = SURFACE_STYLE_USAGE ( .BOTH. , #35195 ) ;
#46894 = CARTESIAN_POINT ( 'NONE',  ( 0.9325001150361308389, -0.1669857002805301138, 1.989206133734520154 ) ) ;
#46896 = DIRECTION ( 'NONE',  ( 0.000000000000000000, 0.000000000000000000, -1.000000000000000000 ) ) ;
#46897 = ADVANCED_FACE ( 'NONE', ( #22727 ), #31126, .T. ) ;
#46899 = LINE ( 'NONE', #6879, #30019 ) ;
#46898 = CARTESIAN_POINT ( 'NONE',  ( 0.9500414927467377701, 0.1787899950787401604, 0.6594488188438737408 ) ) ;
#46900 = DIRECTION ( 'NONE',  ( -4.336808689942014285E-16, 0.000000000000000000, -1.000000000000000000 ) ) ;
#46901 = DIRECTION ( 'NONE',  ( -1.000000000000000000, -0.000000000000000000, 0.000000000000000000 ) ) ;
#46902 = CARTESIAN_POINT ( 'NONE',  ( 0.1636882031745370836, 0.08048648106634784249, 0.1394067746907973471 ) ) ;
#46903 = CARTESIAN_POINT ( 'NONE',  ( 0.9412147342319837628, -0.1574803149606297803, 1.734744094488190003 ) ) ;
#46904 = CARTESIAN_POINT ( 'NONE',  ( 0.8107537697050254399, -0.1574803149606297803, 0.7062007874015745479 ) ) ;
#46905 = CARTESIAN_POINT ( 'NONE',  ( 0.6971942568897626646, 0.07405724077823318263, 0.9448818897100165204 ) ) ;
#46906 = EDGE_CURVE ( 'NONE', #32919, #30008, #14812, .T. ) ;
#46907 = EDGE_LOOP ( 'NONE', ( #2807, #47053, #6321, #26738 ) ) ;
#46908 = CARTESIAN_POINT ( 'NONE',  ( 0.7185039370078746268, 0.06523048226347956391, 1.483759842519686067 ) ) ;
#46909 = DIRECTION ( 'NONE',  ( 0.000000000000000000, 0.000000000000000000, 1.000000000000000000 ) ) ;
#46910 = CARTESIAN_POINT ( 'NONE',  ( -0.1270800023317771588, 0.07279083608624586921, -0.1270800023317771588 ) ) ;
#46911 = CARTESIAN_POINT ( 'NONE',  ( -1.094772975963752103E-17, -1.275098425143086578, -0.1787899950787401882 ) ) ;
#46912 = CARTESIAN_POINT ( 'NONE',  ( -0.1574803149606299191, -1.484251968503937036, 0.000000000000000000 ) ) ;
#46913 = CARTESIAN_POINT ( 'NONE',  ( 1.033464566929133799, 0.000000000000000000, 1.230314960629921295 ) ) ;
#46914 = EDGE_LOOP ( 'NONE', ( #42375, #18352, #16917, #24488, #38858 ) ) ;
#46915 = CARTESIAN_POINT ( 'NONE',  ( -1.002407869896990045, -0.1264236179284866091, 0.1353346456155277433 ) ) ;
#46916 = ORIENTED_EDGE ( 'NONE', *, *, #27637, .F. ) ;
#46917 = ORIENTED_EDGE ( 'NONE', *, *, #38636, .T. ) ;
#46918 = DIRECTION ( 'NONE',  ( 0.000000000000000000, 0.000000000000000000, 1.000000000000000000 ) ) ;
#46919 = ORIENTED_EDGE ( 'NONE', *, *, #36697, .T. ) ;
#46920 = CARTESIAN_POINT ( 'NONE',  ( -1.002407869896990045, 0.1264236179284866091, 1.961122047190330786 ) ) ;
#46921 = CARTESIAN_POINT ( 'NONE',  ( -0.7495606340400177148, -0.1264236179284866091, 1.582185039316315045 ) ) ;
#46922 = CARTESIAN_POINT ( 'NONE',  ( 0.7495606340400177148, -0.1264236179284866091, 0.8784448818360000022 ) ) ;
#46923 = CARTESIAN_POINT ( 'NONE',  ( -0.6971942568897637749, 2.189545951927499583E-17, 0.8292322834108031282 ) ) ;
#46924 = CARTESIAN_POINT ( 'NONE',  ( -1.054774247047244540, -0.07405724077823318263, 0.3789370078202520253 ) ) ;
#46925 = AXIS2_PLACEMENT_3D ( 'NONE', #17194, #18074, #20316 ) ;
#46926 = CARTESIAN_POINT ( 'NONE',  ( -0.1908328281150615813, 0.07780450164205222896, -0.1752556861836934432 ) ) ;
#46927 = CARTESIAN_POINT ( 'NONE',  ( -1.002407869896990045, 0.1264236179284866091, 1.882381889710015743 ) ) ;
#46928 = CARTESIAN_POINT ( 'NONE',  ( -0.7646288533564489232, 0.1113553986120547346, 1.914370078740157632 ) ) ;
#46929 = CARTESIAN_POINT ( 'NONE',  ( -0.07405724077823318263, -0.3239428658670340799, 0.1787899950787401604 ) ) ;
#46930 = DIRECTION ( 'NONE',  ( 0.000000000000000000, 0.000000000000000000, 1.000000000000000000 ) ) ;
#46931 = DIRECTION ( 'NONE',  ( -1.000000000000000000, 0.000000000000000000, 0.000000000000000000 ) ) ;
#46932 = AXIS2_PLACEMENT_3D ( 'NONE', #4370, #15679, #22369 ) ;
#46933 = CIRCLE ( 'NONE', #31648, 0.09842519685039370636 ) ;
#46934 = ADVANCED_FACE ( 'NONE', ( #28472 ), #6152, .T. ) ;
#46935 = CARTESIAN_POINT ( 'NONE',  ( -0.8759842519685039353, -0.1787899950787401882, 0.09104330703285078152 ) ) ;
#46936 = ORIENTED_EDGE ( 'NONE', *, *, #5061, .T. ) ;
#46937 = ORIENTED_EDGE ( 'NONE', *, *, #28652, .F. ) ;
#46938 = CARTESIAN_POINT ( 'NONE',  ( -0.8019270111902716547, 0.1787899950787401604, 1.220472440891118504 ) ) ;
#46939 = EDGE_LOOP ( 'NONE', ( #5063, #8152, #13528, #17390 ) ) ;
#46940 = CARTESIAN_POINT ( 'NONE',  ( -0.1787899950787401882, -1.147145669237574772, 0.000000000000000000 ) ) ;
#46941 = CARTESIAN_POINT ( 'NONE',  ( 3.284318927891251994E-17, -1.368602362150960650, 0.1787899950787401882 ) ) ;
#46942 = DIRECTION ( 'NONE',  ( 1.822029033848725028E-16, 0.000000000000000000, 1.000000000000000000 ) ) ;
#46943 = CARTESIAN_POINT ( 'NONE',  ( 0.7646288533564489232, -0.1113553986120547346, 0.3494094488188976277 ) ) ;
#46944 = DIRECTION ( 'NONE',  ( 1.000000000000000000, 0.000000000000000000, 0.000000000000000000 ) ) ;
#46945 = CARTESIAN_POINT ( 'NONE',  ( -0.8759842519685039353, -0.1574803149606299191, 0.8956692912310552090 ) ) ;
#46946 = CARTESIAN_POINT ( 'NONE',  ( -0.8759842519685039353, 0.1574803149606299191, 0.7677165354330708347 ) ) ;
#46947 = CARTESIAN_POINT ( 'NONE',  ( 2.892866454678787531E-17, -0.1358267716535433156, 0.1574803149606299191 ) ) ;
#46948 = CARTESIAN_POINT ( 'NONE',  ( 1.033464566929133799, 0.000000000000000000, 1.811023621939716444 ) ) ;
#46949 = ORIENTED_EDGE ( 'NONE', *, *, #35619, .F. ) ;
#46950 = CARTESIAN_POINT ( 'NONE',  ( 0.000000000000000000, 0.000000000000000000, -0.1045766232635885612 ) ) ;
#46951 = CARTESIAN_POINT ( 'NONE',  ( 0.7185039370078746268, -0.06523048226347956391, 0.8587598425196850682 ) ) ;
#46952 = DIRECTION ( 'NONE',  ( -1.000000000000000000, 0.000000000000000000, 0.000000000000000000 ) ) ;
#46953 = B_SPLINE_CURVE_WITH_KNOTS ( 'NONE', 3,
 ( #21266, #17914, #39471, #40406, #21024, #25602, #21503, #29468, #21987, #6649, #35671, #25362, #46902, #10508, #35891, #32566, #44013 ),
 .UNSPECIFIED., .F., .F.,
 ( 4, 2, 2, 2, 2, 1, 2, 2, 4 ),
 ( 0.000000000000000000, 0.2500000000000179301, 0.3750000000000189293, 0.5000000000000199840, 0.6250000000000210942, 0.6875000000000186517, 0.7187500000000174305, 0.7500000000000162093, 1.000000000000000000 ),
 .UNSPECIFIED. ) ;
#46954 = CARTESIAN_POINT ( 'NONE',  ( -0.06523048226347956391, -0.07431102362204729250, -0.1574803149606300301 ) ) ;
#46955 = ( BOUNDED_CURVE ( )  B_SPLINE_CURVE ( 2, ( #22604, #4605, #19712, #16142, #37216, #19238, #4849, #37696, #23323 ),
 .UNSPECIFIED., .F., .F. ) 
 B_SPLINE_CURVE_WITH_KNOTS ( ( 3, 2, 2, 2, 3 ),
 ( 0.3499999999999999778, 0.3524999999999999800, 0.3549999999999999822, 0.3574999999999999845, 0.3599999999999999867 ),
 .UNSPECIFIED. ) 
 CURVE ( )  GEOMETRIC_REPRESENTATION_ITEM ( )  RATIONAL_B_SPLINE_CURVE ( ( 1.000000000000000000, 0.9238795325112879597, 1.000000000000000000, 0.9238795325112869605, 1.000000000000000000, 0.9238795325112869605, 1.000000000000000000, 0.9238795325112869605, 1.000000000000000000 ) ) 
 REPRESENTATION_ITEM ( '' )  ) ;
#46956 = EDGE_CURVE ( 'NONE', #23930, #19760, #5926, .T. ) ;
#46958 = PRESENTATION_STYLE_ASSIGNMENT (( #35487 ) ) ;
#46957 = DIRECTION ( 'NONE',  ( 0.000000000000000000, -0.7880107536067206819, 0.6156614753256598460 ) ) ;
#46959 = CARTESIAN_POINT ( 'NONE',  ( 0.7185039370078746268, -0.06523048226347956391, 0.1402559054042841202 ) ) ;
#46960 = AXIS2_PLACEMENT_3D ( 'NONE', #37576, #41613, #8819 ) ;
#46961 = EDGE_CURVE ( 'NONE', #1272, #39970, #23897, .T. ) ;
#46962 = CARTESIAN_POINT ( 'NONE',  ( -0.1113553986120547346, 0.1053149607374482266, 0.1113553986120547346 ) ) ;
#46963 = CARTESIAN_POINT ( 'NONE',  ( 2.892866454678787531E-17, -1.503937007766488199, 0.1574803149606299191 ) ) ;
#46964 = CARTESIAN_POINT ( 'NONE',  ( -0.1264236179284866091, -0.6304133857730078727, 0.1264236179284866091 ) ) ;
#46965 = CARTESIAN_POINT ( 'NONE',  ( 0.1113553986120547346, -1.115157480314960647, 0.1113553986120547346 ) ) ;
#46966 = CARTESIAN_POINT ( 'NONE',  ( 0.7185039370078746268, -0.06523048226347956391, 0.9276574802074333270 ) ) ;
#46967 = PLANE ( 'NONE',  #26776 ) ;
#46968 = CARTESIAN_POINT ( 'NONE',  ( -0.6971942568897626646, -0.07405724077823297447, 0.4379921259304882519 ) ) ;
#46969 = ORIENTED_EDGE ( 'NONE', *, *, #24032, .T. ) ;
#46970 = ORIENTED_EDGE ( 'NONE', *, *, #18776, .F. ) ;
#46971 = CARTESIAN_POINT ( 'NONE',  ( -0.8019270111902717657, -0.1787899950787401604, 1.628937007820252303 ) ) ;
#46972 = CARTESIAN_POINT ( 'NONE',  ( -0.8019270111902717657, -0.1787899950787401604, 0.8021653542769460188 ) ) ;
#46973 = CARTESIAN_POINT ( 'NONE',  ( 0.9500414927467378812, -0.1787899950787401604, 0.2165354330171024577 ) ) ;
#46974 = CARTESIAN_POINT ( 'NONE',  ( -0.9873396505805591694, -0.1113553986120547346, 1.687992125876724536 ) ) ;
#46975 = CARTESIAN_POINT ( 'NONE',  ( 0.6971942568897648851, -0.07405724077823297447, 0.7578740156942688211 ) ) ;
#46976 = CARTESIAN_POINT ( 'NONE',  ( -1.002407869896990045, -0.1264236179284866091, 0.7652559054580472253 ) ) ;
#46977 = CARTESIAN_POINT ( 'NONE',  ( 0.7185039370078746268, 0.06523048226347956391, 0.9227362203649142058 ) ) ;
#46978 = CARTESIAN_POINT ( 'NONE',  ( 0.7185039370078739607, 1.928577636452523993E-17, 1.131889763779527547 ) ) ;
#46979 = CARTESIAN_POINT ( 'NONE',  ( 0.1574803149606299191, -0.2736220471365672924, -1.928577636452523993E-17 ) ) ;
#46980 = CARTESIAN_POINT ( 'NONE',  ( -0.7495606340400177148, 0.1264236179284866091, 1.419783464513165505 ) ) ;
#46981 = DIRECTION ( 'NONE',  ( 0.000000000000000000, 1.000000000000000000, 0.000000000000000000 ) ) ;
#46982 = CARTESIAN_POINT ( 'NONE',  ( -0.8759842519685039353, 0.1574803149606299191, 1.515748031496062964 ) ) ;
#46983 = CARTESIAN_POINT ( 'NONE',  ( -0.9412147342319837628, 0.1574803149606300301, 0.4109251968503938590 ) ) ;
#46984 = CARTESIAN_POINT ( 'NONE',  ( 1.054774247047244540, -0.07405724077823318263, 1.481299212544662902 ) ) ;
#46985 = CARTESIAN_POINT ( 'NONE',  ( -0.1604542604227535418, -0.09851383291672559384, 0.05492199793948401854 ) ) ;
#46986 = CARTESIAN_POINT ( 'NONE',  ( 0.7185039370078739607, 1.928577636452523993E-17, 1.958661417322834719 ) ) ;
#46987 = ORIENTED_EDGE ( 'NONE', *, *, #18826, .T. ) ;
#46988 = CIRCLE ( 'NONE', #7177, 0.1377952755905511861 ) ;
#46989 = ADVANCED_FACE ( 'NONE', ( #43041 ), #23143, .F. ) ;
#46990 = CARTESIAN_POINT ( 'NONE',  ( 3.284318927891251994E-17, -1.738805070591442847, 0.1787899950787401882 ) ) ;
#46991 = VERTEX_POINT ( 'NONE', #24383 ) ;
#46992 = CARTESIAN_POINT ( 'NONE',  ( 1.033464566929134687, -0.06523048226347956391, 0.4010826771653545619 ) ) ;
#46993 = ORIENTED_EDGE ( 'NONE', *, *, #23757, .T. ) ;
#46994 = CARTESIAN_POINT ( 'NONE',  ( 0.5415383587465882886, 0.09842519685039370636, 1.205361022782828805E-17 ) ) ;
#46995 = CARTESIAN_POINT ( 'NONE',  ( -0.07405724077823318263, -0.8346456692375755493, -0.1787899950787401604 ) ) ;
#46996 = CARTESIAN_POINT ( 'NONE',  ( -0.2471915046496347967, -0.08339338023411900502, -0.06619788746946630997 ) ) ;
#46997 = CARTESIAN_POINT ( 'NONE',  ( 0.1640397255806962662, -0.1615187269478208787, -1.214557857170256269E-06 ) ) ;
#46998 = CIRCLE ( 'NONE', #307, 0.4724409448818896462 ) ;
#46999 = ADVANCED_FACE ( 'NONE', ( #21247 ), #17190, .T. ) ;
#47000 = CARTESIAN_POINT ( 'NONE',  ( 0.1787899950787401604, -0.07787987374104976546, 0.07405724077823318263 ) ) ;
#47001 = CARTESIAN_POINT ( 'NONE',  ( -0.1787899950787401882, -0.2760826771115909573, 0.000000000000000000 ) ) ;
#47002 = CARTESIAN_POINT ( 'NONE',  ( -0.1264236179284866091, -0.0004921259304884456750, 0.1264236179284866091 ) ) ;
#47003 = CONTEXT_DEPENDENT_SHAPE_REPRESENTATION ( #43142, #46689 ) ;
#47004 = CARTESIAN_POINT ( 'NONE',  ( 0.2471904733175533664, -0.07069887449118136824, -0.09042980707038553168 ) ) ;
#47005 = CARTESIAN_POINT ( 'NONE',  ( -0.9412147342319837628, -0.1574803149606297803, 1.695374015748031926 ) ) ;
#47006 = CARTESIAN_POINT ( 'NONE',  ( 0.7495606340400177148, -0.1264236179284866091, 0.6766732282926929409 ) ) ;
#47007 = CARTESIAN_POINT ( 'NONE',  ( -0.9500414927467377701, 0.1787899950787401604, 0.9793307086076531442 ) ) ;
#47008 = EDGE_CURVE ( 'NONE', #27709, #44763, #6220, .T. ) ;
#47009 = CARTESIAN_POINT ( 'NONE',  ( -0.8617263095615074198, 0.1748397955725940756, 0.03937007874015843734 ) ) ;
#47010 = CARTESIAN_POINT ( 'NONE',  ( 0.1270800023317771588, -1.748075305646037414, -0.1270800023317771588 ) ) ;
#47011 = CYLINDRICAL_SURFACE ( 'NONE', #24599, 0.1574803149606299191 ) ;
#47012 = CARTESIAN_POINT ( 'NONE',  ( 0.9500414927467378812, 0.1787899950787401604, 1.687992125930489307 ) ) ;
#47014 = CARTESIAN_POINT ( 'NONE',  ( 0.1642909309817496277, 0.1618381351750143859, 1.491082269536694323E-08 ) ) ;
#47013 = FACE_OUTER_BOUND ( 'NONE', #30578, .T. ) ;
#47015 = ORIENTED_EDGE ( 'NONE', *, *, #27301, .F. ) ;
#47016 = VERTEX_POINT ( 'NONE', #44457 ) ;
#47017 = AXIS2_PLACEMENT_3D ( 'NONE', #45596, #42864, #27683 ) ;
#47018 = EDGE_CURVE ( 'NONE', #32014, #31452, #27006, .T. ) ;
#47019 = CARTESIAN_POINT ( 'NONE',  ( 1.033464566929133799, 0.000000000000000000, 1.338582677057826853 ) ) ;
#47020 = CARTESIAN_POINT ( 'NONE',  ( 0.07405724077823318263, -0.1358267715997797664, -0.1787899950787401604 ) ) ;
#47021 = CARTESIAN_POINT ( 'NONE',  ( -1.002407869896990045, -0.1264236179284866091, 0.4158464566391496531 ) ) ;
#47022 = CARTESIAN_POINT ( 'NONE',  ( 0.6971942568897626646, -0.07405724077823297447, 0.6742125983714335469 ) ) ;
#47023 = CARTESIAN_POINT ( 'NONE',  ( -0.1264236179284866091, -1.068405511757259951, -0.1264236179284866091 ) ) ;
#47024 = CARTESIAN_POINT ( 'NONE',  ( 0.9500414927467378812, 0.1787899950787401604, 0.07381889758403178958 ) ) ;
#47025 = FACE_BOUND ( 'NONE', #15365, .T. ) ;
#47026 = EDGE_CURVE ( 'NONE', #39516, #11282, #8046, .T. ) ;
#47027 = CARTESIAN_POINT ( 'NONE',  ( -0.9500414927467378812, 0.1787899950787401604, 1.564960629867495845 ) ) ;
#47028 = ORIENTED_EDGE ( 'NONE', *, *, #45879, .T. ) ;
#47029 = VECTOR ( 'NONE', #8750, 39.37007874015748143 ) ;
#47030 = CARTESIAN_POINT ( 'NONE',  ( -0.8019270111902717657, -0.1787899950787401604, 1.117125984198206412 ) ) ;
#47031 = CARTESIAN_POINT ( 'NONE',  ( -0.3076751137723114371, -0.03860885780051061950, -0.7130813053422531134 ) ) ;
#47032 = CARTESIAN_POINT ( 'NONE',  ( 0.9500414927467378812, 0.1787899950787401604, 1.176181102308441417 ) ) ;
#47033 = AXIS2_PLACEMENT_3D ( 'NONE', #549, #21917, #28903 ) ;
#47034 = CARTESIAN_POINT ( 'NONE',  ( -0.1574803149606300301, -1.161909448711369919, -0.06523048226347956391 ) ) ;
#47035 = CARTESIAN_POINT ( 'NONE',  ( -0.7185039370078746268, 0.06523048226347956391, 0.6865157479239701876 ) ) ;
#47036 = CARTESIAN_POINT ( 'NONE',  ( 1.054774247047244540, 0.07405724077823318263, 1.874999999946236784 ) ) ;
#47037 = CARTESIAN_POINT ( 'NONE',  ( -0.8019270111902717657, -0.1787899950787401604, 0.8759842519147408302 ) ) ;
#47038 = CARTESIAN_POINT ( 'NONE',  ( -0.9873396505805591694, -0.1113553986120547346, 1.619094488188976388 ) ) ;
#47039 = CARTESIAN_POINT ( 'NONE',  ( 0.3246033735368759610, 4.766607801171850497E-17, 0.000000000000000000 ) ) ;
#47040 = CARTESIAN_POINT ( 'NONE',  ( 0.6971942568897626646, 0.07405724077823318263, 0.2805118109698587214 ) ) ;
#47041 = CARTESIAN_POINT ( 'NONE',  ( -0.8759842519685039353, -0.1787899950787401882, 0.2485236219934806867 ) ) ;
#47042 = CARTESIAN_POINT ( 'NONE',  ( -0.8019270111902717657, -0.1787899950787401604, 0.7185039369541108556 ) ) ;
#47043 = CARTESIAN_POINT ( 'NONE',  ( 1.033464566929133799, 0.000000000000000000, 1.574803149498771537 ) ) ;
#47044 = ORIENTED_EDGE ( 'NONE', *, *, #43935, .T. ) ;
#47045 = CARTESIAN_POINT ( 'NONE',  ( -0.07405724077823318263, -0.07677165348954355373, 0.1787899950787401604 ) ) ;
#47046 = ORIENTED_EDGE ( 'NONE', *, *, #9491, .T. ) ;
#47047 = CARTESIAN_POINT ( 'NONE',  ( 0.8759842519685039353, 0.1787899950787401882, 0.7455708660879684091 ) ) ;
#47048 = CARTESIAN_POINT ( 'NONE',  ( 1.054774247047244540, 0.07405724077823318263, 1.013779527505291878 ) ) ;
#47049 = CARTESIAN_POINT ( 'NONE',  ( -0.8019270111902716547, -0.1787899950787401604, 1.860236220418677089 ) ) ;
#47050 = FACE_OUTER_BOUND ( 'NONE', #8655, .T. ) ;
#47051 = CARTESIAN_POINT ( 'NONE',  ( 0.9873396505805591694, 0.1113553986120547346, 1.313976377952756014 ) ) ;
#47052 = CARTESIAN_POINT ( 'NONE',  ( 3.284318927891251994E-17, -1.226994046969395624, 0.1787899950787401882 ) ) ;
#47053 = ORIENTED_EDGE ( 'NONE', *, *, #38544, .F. ) ;
#47054 = CARTESIAN_POINT ( 'NONE',  ( 0.1264236179284866091, -0.2908464566391499861, -0.1264236179284866091 ) ) ;
#47055 = ORIENTED_EDGE ( 'NONE', *, *, #34521, .F. ) ;
#47056 = CARTESIAN_POINT ( 'NONE',  ( 1.002407869896990045, -0.1264236179284866091, 1.119586614119464585 ) ) ;
#47057 = EDGE_CURVE ( 'NONE', #23980, #13081, #36139, .T. ) ;
#47058 = DIRECTION ( 'NONE',  ( 0.000000000000000000, 0.000000000000000000, 1.000000000000000000 ) ) ;
#47059 = CARTESIAN_POINT ( 'NONE',  ( -0.2471922711061399491, -0.07744971747242616888, 0.07831899213450065067 ) ) ;
#47060 = CARTESIAN_POINT ( 'NONE',  ( 0.7646288533564489232, -0.1113553986120547346, 1.963582677165354395 ) ) ;
#47061 = CIRCLE ( 'NONE', #38653, 0.09842519685039370636 ) ;
#47062 = ADVANCED_FACE ( 'NONE', ( #14001 ), #28650, .F. ) ;
#47063 = VECTOR ( 'NONE', #34128, 39.37007874015748143 ) ;
#47064 = PRESENTATION_LAYER_ASSIGNMENT (  '', '', ( #6491 ) ) ;
#47065 = CARTESIAN_POINT ( 'NONE',  ( 0.1264236179284866091, -1.644192913332062966, 0.1264236179284866091 ) ) ;
#47066 = CARTESIAN_POINT ( 'NONE',  ( -0.1787899950787401604, -0.7165354330171036512, -0.07405724077823318263 ) ) ;
#47067 = CARTESIAN_POINT ( 'NONE',  ( -0.8759842519685039353, -0.1787899950787401882, 0.4896653542769449086 ) ) ;
#47068 = CARTESIAN_POINT ( 'NONE',  ( -0.1181206562389580106, -0.09842519685039372024, 0.1154461398689740764 ) ) ;
#47069 = CARTESIAN_POINT ( 'NONE',  ( 0.1864803149606299171, 0.5288907983920102529, -0.7507079620615728643 ) ) ;
#47070 = CARTESIAN_POINT ( 'NONE',  ( 1.054774247047244540, 0.07405724077823318263, 1.210629921206079818 ) ) ;
#47071 = CARTESIAN_POINT ( 'NONE',  ( 1.002407869896990045, 0.1264236179284866091, 1.562499999946236118 ) ) ;
#47072 = DIRECTION ( 'NONE',  ( 0.000000000000000000, 1.000000000000000000, 0.000000000000000000 ) ) ;
#47073 = CARTESIAN_POINT ( 'NONE',  ( 0.7185039370078746268, 0.06523048226347956391, 1.719980314960629864 ) ) ;
#47074 = CARTESIAN_POINT ( 'NONE',  ( 0.1588152253974371431, -0.05589252443383686819, 0.1377952755905511029 ) ) ;
#47075 = FACE_OUTER_BOUND ( 'NONE', #16434, .T. ) ;
#47076 = CARTESIAN_POINT ( 'NONE',  ( -0.8759842519685039353, 0.1574803149606299191, 1.742125984144440975 ) ) ;
#47077 = CARTESIAN_POINT ( 'NONE',  ( 0.7495606340400177148, -0.1264236179284866091, 0.2436023621509610382 ) ) ;
#47079 = CARTESIAN_POINT ( 'NONE',  ( 0.3649999999999999911, -0.2362204724409449064, 0.000000000000000000 ) ) ;
#47078 = CARTESIAN_POINT ( 'NONE',  ( 0.9500414927467377701, 0.1787899950787401604, 1.131889763725763887 ) ) ;
#47080 = EDGE_CURVE ( 'NONE', #34914, #8746, #33186, .T. ) ;
#47081 = LINE ( 'NONE', #3478, #2094 ) ;
#47082 = CARTESIAN_POINT ( 'NONE',  ( 1.033464566929133799, 0.000000000000000000, 0.4330708660342047489 ) ) ;
#47083 = VERTEX_POINT ( 'NONE', #40320 ) ;
#47084 = DIRECTION ( 'NONE',  ( 1.000000000000000000, -0.000000000000000000, -0.000000000000000000 ) ) ;
#47085 = CARTESIAN_POINT ( 'NONE',  ( 0.8729137959494666088, 0.1746894649194470073, 0.03936731548249973456 ) ) ;
#47086 = CARTESIAN_POINT ( 'NONE',  ( -0.9873396505805591694, -0.1113553986120547346, 0.4675196849318432601 ) ) ;
#47087 = ORIENTED_EDGE ( 'NONE', *, *, #40660, .F. ) ;
#47088 = CARTESIAN_POINT ( 'NONE',  ( 0.8019270111902717657, -0.1787899950787401604, 1.427165354276944687 ) ) ;
#47089 = CARTESIAN_POINT ( 'NONE',  ( -0.7185039370078739607, 1.928577636452523993E-17, 1.131889763779527547 ) ) ;
#47091 = CARTESIAN_POINT ( 'NONE',  ( 0.9412147342319837628, -0.1574803149606297803, 0.07135826760900840227 ) ) ;
#47090 = CARTESIAN_POINT ( 'NONE',  ( -0.8759842519685039353, 0.000000000000000000, 0.000000000000000000 ) ) ;
#47092 = CARTESIAN_POINT ( 'NONE',  ( -0.1787899950787401882, -0.03986220467064590517, 0.000000000000000000 ) ) ;
#47093 = VERTEX_POINT ( 'NONE', #14711 ) ;
#47094 = CARTESIAN_POINT ( 'NONE',  ( 2.892866454678787531E-17, -0.08661417312081949593, 0.1574803149606299191 ) ) ;
#47095 = EDGE_LOOP ( 'NONE', ( #41283, #19509, #273, #4421, #25597 ) ) ;
#47097 = DIRECTION ( 'NONE',  ( 0.000000000000000000, 0.000000000000000000, -1.000000000000000000 ) ) ;
#47096 = VECTOR ( 'NONE', #14123, 39.37007874015748143 ) ;
#47098 = CARTESIAN_POINT ( 'NONE',  ( 0.1528784791660942888, -0.09445537554013612447, -0.1971681403756167517 ) ) ;
#47099 = VERTEX_POINT ( 'NONE', #22357 ) ;
#47100 = LINE ( 'NONE', #14524, #25529 ) ;
#47101 = CARTESIAN_POINT ( 'NONE',  ( 1.002407869896990045, -0.1264236179284866091, 0.6126968503399370380 ) ) ;
#47102 = ORIENTED_EDGE ( 'NONE', *, *, #9607, .T. ) ;
#47103 = CARTESIAN_POINT ( 'NONE',  ( -0.8759842519685039353, 0.1787899950787401882, 1.449311023568283341 ) ) ;
#47104 = CARTESIAN_POINT ( 'NONE',  ( -9.642888182262618425E-18, 0.1299212599500466636, -0.1574803149606299191 ) ) ;
#47105 = CARTESIAN_POINT ( 'NONE',  ( -0.6971942568897648851, 0.07405724077823318263, 1.146653543253323582 ) ) ;
#47106 = VECTOR ( 'NONE', #13702, 39.37007874015748143 ) ;
#47107 = VECTOR ( 'NONE', #8798, 39.37007874015748143 ) ;
#47108 = CARTESIAN_POINT ( 'NONE',  ( -0.7185039370078746268, -0.06523048226347956391, 0.1894685039370080093 ) ) ;
#47109 = CARTESIAN_POINT ( 'NONE',  ( -0.9500414927467377701, -0.1787899950787401604, 1.038385826717890259 ) ) ;
#47110 = CARTESIAN_POINT ( 'NONE',  ( -0.6971942568897637749, 2.189545951927499583E-17, 0.7554133857730077617 ) ) ;
#47111 = ( BOUNDED_CURVE ( )  B_SPLINE_CURVE ( 2, ( #24456, #13664, #34790, #31430, #27381, #31668, #27852, #9846, #2632 ),
 .UNSPECIFIED., .F., .F. ) 
 B_SPLINE_CURVE_WITH_KNOTS ( ( 3, 2, 2, 2, 3 ),
 ( 0.1700000000000000122, 0.1724999999999999867, 0.1749999999999999889, 0.1774999999999999911, 0.1799999999999999933 ),
 .UNSPECIFIED. ) 
 CURVE ( )  GEOMETRIC_REPRESENTATION_ITEM ( )  RATIONAL_B_SPLINE_CURVE ( ( 1.000000000000000000, 0.9238795325112849621, 1.000000000000000000, 0.9238795325112869605, 1.000000000000000000, 0.9238795325112869605, 1.000000000000000000, 0.9238795325112869605, 1.000000000000000000 ) ) 
 REPRESENTATION_ITEM ( '' )  ) ;
#47112 = DIRECTION ( 'NONE',  ( -1.000000000000000000, 0.000000000000000000, 0.000000000000000000 ) ) ;
#47113 = CARTESIAN_POINT ( 'NONE',  ( -0.1264236179284866091, -0.7988444406701832312, 0.1264236179284866091 ) ) ;
#47114 = CARTESIAN_POINT ( 'NONE',  ( -0.004948818435039661207, -0.08956172228597282514, 0.1527134704424525646 ) ) ;
#47115 = CARTESIAN_POINT ( 'NONE',  ( 0.7554274433290401047, 0.1321208994424742933, 0.03937161865901335489 ) ) ;
#47116 = ORIENTED_EDGE ( 'NONE', *, *, #39382, .F. ) ;
#47117 = CARTESIAN_POINT ( 'NONE',  ( -0.7185039370078746268, -0.06523048226347956391, 0.3371062991050715607 ) ) ;
#47118 = EDGE_CURVE ( 'NONE', #7162, #33937, #18993, .T. ) ;
#47119 = DIRECTION ( 'NONE',  ( 0.000000000000000000, 0.000000000000000000, 1.000000000000000000 ) ) ;
#47120 = CARTESIAN_POINT ( 'NONE',  ( -1.054774247047244096, 0.000000000000000000, 0.6126968503399370380 ) ) ;
#47121 = CARTESIAN_POINT ( 'NONE',  ( 0.5839895013123354017, -0.08090551181102362266, 1.098083891755157578E-17 ) ) ;
#47122 = ADVANCED_FACE ( 'NONE', ( #37450 ), #22836, .T. ) ;
#47123 = ORIENTED_EDGE ( 'NONE', *, *, #13186, .T. ) ;
#47124 = ADVANCED_FACE ( 'NONE', ( #4140 ), #159, .F. ) ;
#47125 = CARTESIAN_POINT ( 'NONE',  ( -0.7495606340400177148, -0.1264236179284866091, 1.823326771599779406 ) ) ;
#47126 = AXIS2_PLACEMENT_3D ( 'NONE', #40179, #39947, #18394 ) ;
#47127 = EDGE_CURVE ( 'NONE', #44436, #22067, #13936, .T. ) ;
#47128 = VERTEX_POINT ( 'NONE', #18304 ) ;
#47129 = CARTESIAN_POINT ( 'NONE',  ( 0.0002749165346187715567, -0.01333023677889469405, -0.1377841106655355030 ) ) ;
#47130 = ( BOUNDED_CURVE ( )  B_SPLINE_CURVE ( 2, ( #16537, #15130, #44556, #7674, #29548, #33119, #15606, #44795, #25444 ),
 .UNSPECIFIED., .F., .F. ) 
 B_SPLINE_CURVE_WITH_KNOTS ( ( 3, 2, 2, 2, 3 ),
 ( 0.8199999999999999512, 0.8225000000000000089, 0.8249999999999999556, 0.8275000000000000133, 0.8299999999999999600 ),
 .UNSPECIFIED. ) 
 CURVE ( )  GEOMETRIC_REPRESENTATION_ITEM ( )  RATIONAL_B_SPLINE_CURVE ( ( 1.000000000000000000, 0.9238795325112899581, 1.000000000000000000, 0.9238795325112869605, 1.000000000000000000, 0.9238795325112869605, 1.000000000000000000, 0.9238795325112829637, 1.000000000000000000 ) ) 
 REPRESENTATION_ITEM ( '' )  ) ;
#47131 = CARTESIAN_POINT ( 'NONE',  ( -1.002407869896990045, -0.1264236179284866091, 0.1008858267178899676 ) ) ;
#47132 = ORIENTED_EDGE ( 'NONE', *, *, #5795, .T. ) ;
#47133 = CARTESIAN_POINT ( 'NONE',  ( 0.7185039370078746268, 0.06523048226347956391, 0.6963582677165359724 ) ) ;
#47134 = CARTESIAN_POINT ( 'NONE',  ( -1.100456976456230270E-17, -0.9163823922602106764, -0.1797182628040039365 ) ) ;
#47135 = CARTESIAN_POINT ( 'NONE',  ( -1.033464566929133799, 0.000000000000000000, 0.3937007872940476716 ) ) ;
#47136 = CARTESIAN_POINT ( 'NONE',  ( -0.9873396505805591694, 0.1113553986120547346, 1.343503936900346529 ) ) ;
#47137 = CARTESIAN_POINT ( 'NONE',  ( 0.6971942568897626646, -0.07405724077823297447, 0.8366141731745828647 ) ) ;
#47138 = CARTESIAN_POINT ( 'NONE',  ( -0.1113553986120547346, -0.6624015748031496509, -0.1113553986120547346 ) ) ;
#47139 = VECTOR ( 'NONE', #9591, 39.37007874015748143 ) ;
#47140 = CARTESIAN_POINT ( 'NONE',  ( -0.1626266311456144864, 0.1259158391802847055, -0.01719266890941318487 ) ) ;
#47141 = VERTEX_POINT ( 'NONE', #25967 ) ;
#47142 = CARTESIAN_POINT ( 'NONE',  ( -0.2559055118110236116, 0.07057771752877874116, -0.04780316061551689866 ) ) ;
#47143 = CARTESIAN_POINT ( 'NONE',  ( 0.9873396505805591694, -0.1113553986120547346, 1.225393700787401619 ) ) ;
#47145 = CARTESIAN_POINT ( 'NONE',  ( -0.1235961452251413406, 0.09842519685039370636, -0.2140748031496062798 ) ) ;
#47144 = CARTESIAN_POINT ( 'NONE',  ( 0.8435002617486037080, -0.1706024796764649409, 1.987610845726340392 ) ) ;
#47146 = CARTESIAN_POINT ( 'NONE',  ( 1.033464566929134687, -0.06523048226347956391, 1.975885826771653475 ) ) ;
#47147 = CARTESIAN_POINT ( 'NONE',  ( 0.06523048226347956391, -0.6353346455617642219, 0.1574803149606297803 ) ) ;
#47149 = FACE_OUTER_BOUND ( 'NONE', #26061, .T. ) ;
#47148 = CARTESIAN_POINT ( 'NONE',  ( 0.7495606340400177148, 0.1264236179284866091, 0.7062007873478109987 ) ) ;
#47150 = CARTESIAN_POINT ( 'NONE',  ( -0.1787899950787401604, -0.6722440944344262315, -0.07405724077823318263 ) ) ;
#47151 = LINE ( 'NONE', #13604, #46818 ) ;
#47152 = EDGE_LOOP ( 'NONE', ( #45845, #9273, #10215, #35182 ) ) ;
#47153 = LINE ( 'NONE', #14337, #31428 ) ;
#47154 = CYLINDRICAL_SURFACE ( 'NONE', #32232, 0.1377952755905510751 ) ;
#47155 = CARTESIAN_POINT ( 'NONE',  ( 1.002407869896990045, 0.1264236179284866091, 0.9719488188438739629 ) ) ;
#47156 = DIRECTION ( 'NONE',  ( 0.000000000000000000, 0.000000000000000000, 1.000000000000000000 ) ) ;
#47157 = CARTESIAN_POINT ( 'NONE',  ( -0.07405724077823318263, -1.272637795221826629, -0.1787899950787401604 ) ) ;
#47158 = CARTESIAN_POINT ( 'NONE',  ( -0.06523048226347956391, -1.516240157480315709, 0.1574803149606297803 ) ) ;
#47159 = CARTESIAN_POINT ( 'NONE',  ( -0.2471922904502826812, -0.09842519685039370636, 5.914624404477007554E-17 ) ) ;
#47160 = CARTESIAN_POINT ( 'NONE',  ( -1.054774247047244096, 0.000000000000000000, 0.06151574797773248782 ) ) ;
#47161 = ORIENTED_EDGE ( 'NONE', *, *, #12634, .T. ) ;
#47162 = CARTESIAN_POINT ( 'NONE',  ( 0.8759842519685039353, -0.1787899950787401882, 1.946358267662771757 ) ) ;
#47163 = ORIENTED_EDGE ( 'NONE', *, *, #16538, .T. ) ;
#47164 = CARTESIAN_POINT ( 'NONE',  ( 0.1264236179284866091, -1.407972440891118282, 0.1264236179284866091 ) ) ;
#47165 = CARTESIAN_POINT ( 'NONE',  ( -0.9500414927467377701, 0.1787899950787401604, 1.924212598371433325 ) ) ;
#47166 = CARTESIAN_POINT ( 'NONE',  ( -1.002407869896990045, 0.1264236179284866091, 1.601870078686393750 ) ) ;
#47167 = CIRCLE ( 'NONE', #18079, 0.4724409448818900348 ) ;
#47168 = CARTESIAN_POINT ( 'NONE',  ( -0.9500414927467378812, -0.1787899950787401604, 1.077755905458048113 ) ) ;
#47169 = CARTESIAN_POINT ( 'NONE',  ( -1.054774247047244540, -0.07405724077823318263, 0.3395669290800945039 ) ) ;
#47170 = CARTESIAN_POINT ( 'NONE',  ( -0.1627568843983587810, 0.09133345722617068618, -0.1914653398462846101 ) ) ;
#47171 = CARTESIAN_POINT ( 'NONE',  ( -0.8759842519685039353, -0.1787899950787401882, 1.946358267662771757 ) ) ;
#47172 = CARTESIAN_POINT ( 'NONE',  ( -0.7185039370078746268, 0.06523048226347956391, 1.483759842519686067 ) ) ;
#47173 = CARTESIAN_POINT ( 'NONE',  ( -0.7185039370078746268, 0.06523048226347956391, 1.838090551181102539 ) ) ;
#47174 = LINE ( 'NONE', #29946, #38187 ) ;
#47175 = CARTESIAN_POINT ( 'NONE',  ( -0.1787899950787401604, -0.3337853855520734325, -0.07405724077823318263 ) ) ;
#47176 = CARTESIAN_POINT ( 'NONE',  ( -0.1459546509031376116, -0.09842519685039370636, 0.08266691343448798190 ) ) ;
#47177 = ITEM_DEFINED_TRANSFORMATION ( 'NONE', 'NONE', #3326,  #20860 ) ;
#47178 = CARTESIAN_POINT ( 'NONE',  ( -0.8759842519685039353, 0.000000000000000000, 1.990649606245448844 ) ) ;
#47179 = CARTESIAN_POINT ( 'NONE',  ( -1.002407869896990045, -0.1264236179284866091, 0.1353346456155277433 ) ) ;
#47180 = EDGE_CURVE ( 'NONE', #6785, #42193, #38710, .T. ) ;
#47181 = DIRECTION ( 'NONE',  ( 1.267059173938978811E-30, 3.652049423109077687E-16, -1.000000000000000000 ) ) ;
#47182 = ORIENTED_EDGE ( 'NONE', *, *, #6804, .T. ) ;
#47183 = EDGE_LOOP ( 'NONE', ( #38450, #20736, #14848, #22745 ) ) ;
#47184 = EDGE_CURVE ( 'NONE', #28387, #24360, #26224, .T. ) ;
#47185 = CARTESIAN_POINT ( 'NONE',  ( -0.8019270111902716547, 0.1787899950787401604, 1.456692913332062522 ) ) ;
#47186 = EDGE_LOOP ( 'NONE', ( #43847, #44044, #17576 ) ) ;
#47187 = EDGE_CURVE ( 'NONE', #19692, #33511, #34257, .T. ) ;
#47188 = CARTESIAN_POINT ( 'NONE',  ( 0.1264236179284866091, -1.161909448765133801, -0.1264236179284866091 ) ) ;
#47189 = CARTESIAN_POINT ( 'NONE',  ( 0.07405724077823318263, -1.366141732229700478, 0.1787899950787401604 ) ) ;
#47190 = DIRECTION ( 'NONE',  ( 7.000000000000000150E-15, -2.999999999999999839E-15, 1.000000000000000000 ) ) ;
#47191 = CARTESIAN_POINT ( 'NONE',  ( 0.8107537697050253289, 0.1574803149606300301, 0.3371062992125987146 ) ) ;
#47192 = CARTESIAN_POINT ( 'NONE',  ( -0.07444174185955065859, -0.5989611324176910001, -0.1797182628040039087 ) ) ;
#47193 = CARTESIAN_POINT ( 'NONE',  ( -0.8107537697050234415, -0.1574803149606297803, 0.2337598425196851515 ) ) ;
#47194 = CARTESIAN_POINT ( 'NONE',  ( -0.8759842519685039353, 0.1574803149606299191, 0.9940944880814488460 ) ) ;
#47195 = CARTESIAN_POINT ( 'NONE',  ( 0.6971942568897626646, -0.07405724077823297447, 0.4429133857730075952 ) ) ;
#47196 = CARTESIAN_POINT ( 'NONE',  ( 0.06523048226347956391, -0.1186023622047245596, -0.1574803149606300301 ) ) ;
#47197 = CARTESIAN_POINT ( 'NONE',  ( 1.033464566929134687, 0.06523048226347956391, 1.892224409341292546 ) ) ;
#47198 = EDGE_LOOP ( 'NONE', ( #37042, #31157, #45450, #32063 ) ) ;
#47199 = DIRECTION ( 'NONE',  ( 0.000000000000000000, 0.000000000000000000, 1.000000000000000000 ) ) ;
#47200 = CARTESIAN_POINT ( 'NONE',  ( 0.9873396505805591694, 0.1113553986120547346, 0.8021653543307086798 ) ) ;
#47201 = CARTESIAN_POINT ( 'NONE',  ( 0.05949606008254617467, -0.2611441659580287511, -0.05295753290290579340 ) ) ;
#47202 = CARTESIAN_POINT ( 'NONE',  ( -0.7185039370078746268, 0.06523048226347956391, 1.090059055118109965 ) ) ;
#47204 = CARTESIAN_POINT ( 'NONE',  ( 0.1571385178022482731, -0.1097099440836124123, -0.09077329659535897377 ) ) ;
#47203 = CARTESIAN_POINT ( 'NONE',  ( 0.000000000000000000, 0.000000000000000000, -0.1436967020037460685 ) ) ;
#47205 = CARTESIAN_POINT ( 'NONE',  ( 1.033464566929134687, -0.06523048226347956391, 0.1156496061916856694 ) ) ;
#47206 = VERTEX_POINT ( 'NONE', #23781 ) ;
#47207 = DIRECTION ( 'NONE',  ( 1.000000000000000000, 0.000000000000000000, 0.000000000000000000 ) ) ;
#47208 = CARTESIAN_POINT ( 'NONE',  ( -0.1574803149606299191, -1.513779527451527329, 0.000000000000000000 ) ) ;
#47209 = CARTESIAN_POINT ( 'NONE',  ( 0.1264236179284866091, -0.8075787401037164415, -0.1264236179284866091 ) ) ;
#47210 = DIRECTION ( 'NONE',  ( -1.000000000000000000, 0.000000000000000000, 0.000000000000000000 ) ) ;
#47211 = CARTESIAN_POINT ( 'NONE',  ( 0.1574803149606299191, -1.070866141732283339, -1.928577636452523993E-17 ) ) ;
#47212 = CARTESIAN_POINT ( 'NONE',  ( 1.033464566929134687, 0.06523048226347956391, 0.9079724408373542888 ) ) ;
#47213 = CARTESIAN_POINT ( 'NONE',  ( 0.3302522695077432791, 1.205361022782824954E-17, -0.09842519685039370636 ) ) ;
#47214 = CARTESIAN_POINT ( 'NONE',  ( -0.9500414927467378812, 0.1787899950787401604, 0.3444881889226146243 ) ) ;
#47215 = VERTEX_POINT ( 'NONE', #34123 ) ;
#47216 = VERTEX_POINT ( 'NONE', #19235 ) ;
#47217 = CARTESIAN_POINT ( 'NONE',  ( -0.8759842519685039353, -0.1787899950787401882, 1.670767716481669440 ) ) ;
#47218 = VERTEX_POINT ( 'NONE', #16138 ) ;
#47219 = CARTESIAN_POINT ( 'NONE',  ( 0.9500414927467378812, 0.1787899950787401604, 1.491141732229701367 ) ) ;
#47220 = ORIENTED_EDGE ( 'NONE', *, *, #41846, .F. ) ;
#47221 = CARTESIAN_POINT ( 'NONE',  ( -0.8759842519685039353, -0.1787899950787401882, 0.8439960629383622681 ) ) ;
#47222 = CARTESIAN_POINT ( 'NONE',  ( -0.9873396505805591694, 0.1113553986120547346, 0.2509842519685039353 ) ) ;
#47223 = CARTESIAN_POINT ( 'NONE',  ( 0.8019270111902716547, -0.1787899950787401604, 0.8021653542769462408 ) ) ;
#47224 = CARTESIAN_POINT ( 'NONE',  ( -0.8019270111902716547, 0.1787899950787401604, 0.6643700786863951935 ) ) ;
#47225 = CIRCLE ( 'NONE', #20429, 0.07874015748031495954 ) ;
#47226 = CARTESIAN_POINT ( 'NONE',  ( 0.9873396505805591694, -0.1113553986120547346, 1.146653543307086798 ) ) ;
#47227 = CARTESIAN_POINT ( 'NONE',  ( -0.06523048226347956391, -0.2219488187901106635, -0.1574803149606300301 ) ) ;
#47228 = CARTESIAN_POINT ( 'NONE',  ( -1.033464566929133799, 0.000000000000000000, 1.850393700679873854 ) ) ;
#47229 = VERTEX_POINT ( 'NONE', #1481 ) ;
#47230 = CARTESIAN_POINT ( 'NONE',  ( -1.033464566929134687, 0.06523048226347956391, 0.4847440944881890590 ) ) ;
#47231 = CARTESIAN_POINT ( 'NONE',  ( 0.6971942568897648851, -0.07405724077823297447, 1.427165354276944687 ) ) ;
#47232 = CARTESIAN_POINT ( 'NONE',  ( -0.1623731327614419684, -0.09851383322942126874, 0.05011340600964842712 ) ) ;
#47233 = CARTESIAN_POINT ( 'NONE',  ( -0.8107537697050254399, -0.1574803149606297803, 1.572342519685040907 ) ) ;
#47234 = ORIENTED_EDGE ( 'NONE', *, *, #22625, .T. ) ;
#47235 = ADVANCED_FACE ( 'NONE', ( #45802 ), #39193, .T. ) ;
#47236 = VERTEX_POINT ( 'NONE', #41479 ) ;
#47237 = VERTEX_POINT ( 'NONE', #34826 ) ;
#47238 = EDGE_CURVE ( 'NONE', #29873, #27278, #12448, .T. ) ;
#47239 = LINE ( 'NONE', #252, #4713 ) ;
#47240 = CARTESIAN_POINT ( 'NONE',  ( 0.07405724077823318263, -0.3868110235682837295, 0.1787899950787401604 ) ) ;
#47241 = ( BOUNDED_CURVE ( )  B_SPLINE_CURVE ( 2, ( #32049, #39447, #2317, #27995, #6386, #10240, #38518, #42559, #13581 ),
 .UNSPECIFIED., .F., .T. ) 
 B_SPLINE_CURVE_WITH_KNOTS ( ( 3, 2, 2, 2, 3 ),
 ( 0.04499999999999999833, 0.04750000000000000056, 0.05000000000000000278, 0.05249999999999999806, 0.05500000000000000028 ),
 .UNSPECIFIED. ) 
 CURVE ( )  GEOMETRIC_REPRESENTATION_ITEM ( )  RATIONAL_B_SPLINE_CURVE ( ( 1.000000000000000000, 0.9238795325112869605, 1.000000000000000000, 0.9238795325112869605, 1.000000000000000000, 0.9238795325112869605, 1.000000000000000000, 0.9238795325112869605, 1.000000000000000000 ) ) 
 REPRESENTATION_ITEM ( '' )  ) ;
#47242 = CARTESIAN_POINT ( 'NONE',  ( 0.1787899950787401604, -0.8838582676627719792, -0.07405724077823318263 ) ) ;
#47243 = CARTESIAN_POINT ( 'NONE',  ( 0.9873396505805591694, 0.1113553986120547346, 1.038385826771653475 ) ) ;
#47244 = CARTESIAN_POINT ( 'NONE',  ( 0.1642211665447064484, -0.1618716989613354917, -2.141082140707521260E-06 ) ) ;
#47245 = CARTESIAN_POINT ( 'NONE',  ( 0.9500414927467378812, 0.1787899950787401604, 1.722440944828125930 ) ) ;
#47246 = CARTESIAN_POINT ( 'NONE',  ( 0.6971942568897626646, 0.07405724077823318263, 0.2755905511273391006 ) ) ;
#47247 = CARTESIAN_POINT ( 'NONE',  ( -0.1270800023317771588, -0.1535871166696596291, 0.1270800023317771588 ) ) ;
#47248 = CARTESIAN_POINT ( 'NONE',  ( -1.094772975963752103E-17, -0.06557672413475058859, -0.1787899950787401882 ) ) ;
#47249 = CARTESIAN_POINT ( 'NONE',  ( 0.1264236179284866091, -0.2908464566391499861, -0.1264236179284866091 ) ) ;
#47250 = CARTESIAN_POINT ( 'NONE',  ( -0.07405724077823318263, -0.09153543301710270752, -0.1787899950787401604 ) ) ;
#47251 = CARTESIAN_POINT ( 'NONE',  ( 0.7646288533564489232, -0.1113553986120547346, 0.1427165353255439029 ) ) ;
#47252 = CARTESIAN_POINT ( 'NONE',  ( 0.8759842519685039353, -0.1787899950787401882, 0.6028543306548976854 ) ) ;
#47253 = VECTOR ( 'NONE', #30811, 39.37007874015748854 ) ;
#47254 = CARTESIAN_POINT ( 'NONE',  ( -1.002407869896990045, -0.1264236179284866091, 1.006397637741511808 ) ) ;
#47256 = CARTESIAN_POINT ( 'NONE',  ( 0.9412147342319837628, 0.1574803149606300301, 1.700295275483023172 ) ) ;
#47255 = CARTESIAN_POINT ( 'NONE',  ( -0.8759842519685039353, 0.000000000000000000, 0.000000000000000000 ) ) ;
#47257 = CARTESIAN_POINT ( 'NONE',  ( -0.1797182628040039087, -1.770220974937375402, 0.07444174185955065859 ) ) ;
#47258 = DIRECTION ( 'NONE',  ( 1.000000000000000000, 0.000000000000000000, 0.000000000000000000 ) ) ;
#47259 = CARTESIAN_POINT ( 'NONE',  ( 0.7495606340400177148, -0.1264236179284866091, 1.626476377898992132 ) ) ;
#47260 = CARTESIAN_POINT ( 'NONE',  ( 0.7646288533564489232, 0.1113553986120547346, 0.1328740156405045225 ) ) ;
#47261 = VERTEX_POINT ( 'NONE', #19471 ) ;
#47262 = CARTESIAN_POINT ( 'NONE',  ( -0.7185039370078739607, 1.928577636452523993E-17, 1.407480314960629864 ) ) ;
#47263 = PLANE ( 'NONE',  #45061 ) ;
#47264 = CARTESIAN_POINT ( 'NONE',  ( 0.07405724077823318263, -0.2687007873478113318, 0.1787899950787401604 ) ) ;
#47266 = CARTESIAN_POINT ( 'NONE',  ( 0.1564256176496356399, 0.1180751491311807649, 0.07625914551937829078 ) ) ;
#47265 = CARTESIAN_POINT ( 'NONE',  ( -0.9500414927467378812, -0.1787899950787401604, 0.4527559054580477249 ) ) ;
#47267 = CARTESIAN_POINT ( 'NONE',  ( 0.9500414927467378812, 0.1787899950787401604, 0.6200787401037165525 ) ) ;
#47268 = EDGE_CURVE ( 'NONE', #29740, #18622, #2851, .T. ) ;
#47269 = CARTESIAN_POINT ( 'NONE',  ( 0.1787899950787401882, -1.004429133804503937, -2.189545951927503898E-17 ) ) ;
#47270 = CARTESIAN_POINT ( 'NONE',  ( 0.8019270111902717657, 0.1787899950787401604, 0.1574803149068664809 ) ) ;
#47271 = CARTESIAN_POINT ( 'NONE',  ( 0.9412147342319837628, 0.1574803149606300301, 1.109744094380661350 ) ) ;
#47272 = CARTESIAN_POINT ( 'NONE',  ( -0.7495606340400177148, -0.1264236179284866091, 1.660925196796630088 ) ) ;
#47273 = ORIENTED_EDGE ( 'NONE', *, *, #46745, .F. ) ;
#47274 = CARTESIAN_POINT ( 'NONE',  ( -0.8759842519685039353, -0.1787899950787401882, 1.198326771599779628 ) ) ;
#47275 = CARTESIAN_POINT ( 'NONE',  ( -0.2611872605799127056, -0.1670510767787601047, -0.8649260808424121816 ) ) ;
#47276 = CARTESIAN_POINT ( 'NONE',  ( 0.8019270111902717657, 0.1787899950787401604, 1.141732283410804349 ) ) ;
#47277 = CARTESIAN_POINT ( 'NONE',  ( 0.1574803149606300301, -1.137303149498771537, -0.06523048226347956391 ) ) ;
#47278 = CARTESIAN_POINT ( 'NONE',  ( 0.8759842519685039353, 0.1787899950787401882, 1.803641732229700700 ) ) ;
#47279 = CARTESIAN_POINT ( 'NONE',  ( -0.7185039370078739607, 1.928577636452523993E-17, 0.6200787401574803237 ) ) ;
#47280 = CARTESIAN_POINT ( 'NONE',  ( -0.9500414927467378812, -0.1787899950787401604, 0.8415354330171019859 ) ) ;
#47281 = DIRECTION ( 'NONE',  ( -0.5735764363510518216, -0.8191520442889876907, 0.000000000000000000 ) ) ;
#47282 = CARTESIAN_POINT ( 'NONE',  ( -1.033464566929133799, 0.000000000000000000, 1.338582677057826853 ) ) ;
#47283 = CARTESIAN_POINT ( 'NONE',  ( 0.6971942568897637749, 2.189545951927499583E-17, 0.3617125983714334359 ) ) ;
#47284 = CARTESIAN_POINT ( 'NONE',  ( -0.6971942568897637749, 2.189545951927499583E-17, 0.1599409448281264023 ) ) ;
#47285 = CARTESIAN_POINT ( 'NONE',  ( -0.6971942568897626646, -0.07405724077823297447, 0.7923228345919055560 ) ) ;
#47286 = CARTESIAN_POINT ( 'NONE',  ( 0.8107537697050253289, 0.1574803149606300301, 1.587106299105073060 ) ) ;
#47287 = ORIENTED_EDGE ( 'NONE', *, *, #1075, .T. ) ;
#47288 = VECTOR ( 'NONE', #33914, 39.37007874015748143 ) ;
#47289 = CARTESIAN_POINT ( 'NONE',  ( 0.07405724077823318263, 0.02165354336085014916, -0.1787899950787401604 ) ) ;
#47290 = CARTESIAN_POINT ( 'NONE',  ( 0.9500414927467378812, 0.1787899950787401604, 0.8218503936470251681 ) ) ;
#47291 = CARTESIAN_POINT ( 'NONE',  ( 0.7495606340400177148, 0.1264236179284866091, 1.104822834591905556 ) ) ;
#47292 = CARTESIAN_POINT ( 'NONE',  ( -0.6971942568897637749, 2.189545951927499583E-17, 1.892224409395055096 ) ) ;
#47293 = ADVANCED_FACE ( 'NONE', ( #33891 ), #1013, .F. ) ;
#47294 = CARTESIAN_POINT ( 'NONE',  ( 0.8759842519685039353, 0.1787899950787401882, 1.961122047190330786 ) ) ;
#47295 = EDGE_CURVE ( 'NONE', #42894, #34892, #45309, .T. ) ;
#47296 = CIRCLE ( 'NONE', #32778, 0.2362204724409448231 ) ;
#47297 = EDGE_CURVE ( 'NONE', #1535, #5296, #30529, .T. ) ;
#47298 = CARTESIAN_POINT ( 'NONE',  ( 0.1864803149606299171, 0.5288907983920102529, -0.7507079620615728643 ) ) ;
#47299 = CARTESIAN_POINT ( 'NONE',  ( 0.1787899950787401882, -1.374631842244986357, -2.189545951927503898E-17 ) ) ;
#47300 = ORIENTED_EDGE ( 'NONE', *, *, #5182, .F. ) ;
#47301 = CARTESIAN_POINT ( 'NONE',  ( 0.1787899950787401882, -0.2563976377415121966, -2.189545951927503898E-17 ) ) ;
#47302 = CARTESIAN_POINT ( 'NONE',  ( -0.1113553986120547346, 0.01673228357209397693, -0.1113553986120547346 ) ) ;
#47303 = VERTEX_POINT ( 'NONE', #23321 ) ;
#47304 = CARTESIAN_POINT ( 'NONE',  ( 0.6971942568897637749, 2.189545951927499583E-17, 1.144192913332062966 ) ) ;
#47305 = ADVANCED_FACE ( 'NONE', ( #13251 ), #39084, .T. ) ;
#47306 = CARTESIAN_POINT ( 'NONE',  ( 0.5555748031496086092, 0.2597269656108935343, 0.5511811023622046335 ) ) ;
#47307 = CARTESIAN_POINT ( 'NONE',  ( 1.033464566929133799, 0.000000000000000000, 1.377952755797984263 ) ) ;
#47308 = ADVANCED_BREP_SHAPE_REPRESENTATION ( 'ISO 4162 M5x10 Hex Flange Bolt', ( #5351, #20860 ), #30086 ) ;
#47309 = CARTESIAN_POINT ( 'NONE',  ( 0.7185039370078739607, 1.928577636452523993E-17, 1.919291338582677309 ) ) ;
#47310 = CARTESIAN_POINT ( 'NONE',  ( -0.07405724077823318263, -1.666338582623402953, -0.1787899950787401604 ) ) ;
#47311 = CARTESIAN_POINT ( 'NONE',  ( 3.284318927891251994E-17, -1.722933070812378009, 0.1787899950787401882 ) ) ;
#47312 = CARTESIAN_POINT ( 'NONE',  ( -0.6971942568897637749, 2.189545951927499583E-17, 0.5191929133320630774 ) ) ;
#47313 = AXIS2_PLACEMENT_3D ( 'NONE', #3286, #28017, #10015 ) ;
#47314 = CARTESIAN_POINT ( 'NONE',  ( 0.3161444924769295506, 1.209494567139728360, -1.479906699140346449 ) ) ;
#47315 = CARTESIAN_POINT ( 'NONE',  ( -0.1270800023317771588, -1.265791841079108027, -0.1270800023317771588 ) ) ;
#47316 = CARTESIAN_POINT ( 'NONE',  ( 0.6971942568897637749, 2.189545951927502049E-17, 1.990649606245448844 ) ) ;
#47317 = CARTESIAN_POINT ( 'NONE',  ( 1.054774247047244540, -0.07405724077823318263, 1.205708661363558365 ) ) ;
#47318 = CARTESIAN_POINT ( 'NONE',  ( 1.054774247047244096, 0.000000000000000000, 1.675688976324189117 ) ) ;
#47319 = CARTESIAN_POINT ( 'NONE',  ( -0.7185039370078746268, 0.06523048226347956391, 0.6077755904436539236 ) ) ;
#47321 = CARTESIAN_POINT ( 'NONE',  ( -0.7579867284075441081, 0.1110391951864165283, 1.980897914036486407 ) ) ;
#47320 = CARTESIAN_POINT ( 'NONE',  ( 0.1596653045507425150, -0.05551344951183716930, 0.1404739663221734325 ) ) ;
#47322 = DIRECTION ( 'NONE',  ( 5.553163235302570029E-14, 0.2432573283306915246, -0.9699617890481121441 ) ) ;
#47323 = CARTESIAN_POINT ( 'NONE',  ( -0.1113553986120547346, -0.8001968502861731558, 0.1113553986120547346 ) ) ;
#47324 = CARTESIAN_POINT ( 'NONE',  ( -0.9873396505805591694, -0.1113553986120547346, 1.766732283357039135 ) ) ;
#47325 = VECTOR ( 'NONE', #4078, 39.37007874015748854 ) ;
#47326 = CARTESIAN_POINT ( 'NONE',  ( 0.6971942568897637749, 2.189545951927499583E-17, 0.1205708660879689087 ) ) ;
#47327 = EDGE_CURVE ( 'NONE', #14162, #44831, #5806, .T. ) ;
#47328 = CARTESIAN_POINT ( 'NONE',  ( 0.7027460018079232373, -0.01315211221934205719, 0.03936999329196508302 ) ) ;
#47330 = CARTESIAN_POINT ( 'NONE',  ( -0.7185039370078739607, 1.928577636452523993E-17, 0.5314960628845992741 ) ) ;
#47329 = CARTESIAN_POINT ( 'NONE',  ( 0.6971942568897648851, -0.07405724077823297447, 1.264763779473795813 ) ) ;
#47331 = DIRECTION ( 'NONE',  ( 1.541976423090495042E-15, 0.4344452574044144755, -0.9006982393225890782 ) ) ;
#47332 = CARTESIAN_POINT ( 'NONE',  ( -0.7495606340400177148, -0.1264236179284866091, 1.188484251914740275 ) ) ;
#47333 = CARTESIAN_POINT ( 'NONE',  ( 0.8759842519685039353, 0.1574803149606299191, 0.5216535431995598104 ) ) ;
#47334 = EDGE_LOOP ( 'NONE', ( #43031, #42540, #40500, #18667 ) ) ;
#47335 = CARTESIAN_POINT ( 'NONE',  ( -0.8759842519685039353, 0.1787899950787401882, 1.060531496009228247 ) ) ;
#47336 = PRESENTATION_STYLE_ASSIGNMENT (( #28432 ) ) ;
#47337 = CARTESIAN_POINT ( 'NONE',  ( 0.8584509703022565885, 0.1747054016738197046, 0.03937131093437663820 ) ) ;
#47338 = CARTESIAN_POINT ( 'NONE',  ( -0.8759842519685039353, -0.1574803149606299191, 0.4232283463491653963 ) ) ;
#47339 = ORIENTED_EDGE ( 'NONE', *, *, #40067, .F. ) ;
#47340 = CARTESIAN_POINT ( 'NONE',  ( 0.6971942568897637749, 2.189545951927499583E-17, 1.380413385773007873 ) ) ;
#47341 = CARTESIAN_POINT ( 'NONE',  ( -0.7185039370078739607, 1.928577636452523993E-17, 1.082677165246803241 ) ) ;
#47343 = CARTESIAN_POINT ( 'NONE',  ( -0.9873396505805591694, -0.1113553986120547346, 0.1230314960629921295 ) ) ;
#47342 = DIRECTION ( 'NONE',  ( 0.000000000000000000, 0.000000000000000000, -1.000000000000000000 ) ) ;
#47344 = CARTESIAN_POINT ( 'NONE',  ( 0.7185039370078739607, 1.928577636452523993E-17, 1.171259842519684957 ) ) ;
#47345 = CARTESIAN_POINT ( 'NONE',  ( 0.07405724077823318263, -0.05216535427694517224, -0.1787899950787401604 ) ) ;
#47346 = ORIENTED_EDGE ( 'NONE', *, *, #21354, .F. ) ;
#47347 = DIRECTION ( 'NONE',  ( 1.822029033848725028E-16, 0.000000000000000000, 1.000000000000000000 ) ) ;
#47348 = DIRECTION ( 'NONE',  ( 0.5735764363510447161, -0.8191520442889925757, 1.003171929053525486E-16 ) ) ;
#47349 = FACE_OUTER_BOUND ( 'NONE', #40876, .T. ) ;
#47350 = EDGE_LOOP ( 'NONE', ( #25715, #11830, #21880, #40153 ) ) ;
#47351 = CARTESIAN_POINT ( 'NONE',  ( 0.6971942568897637749, 2.189545951927499583E-17, 0.6373031495525354195 ) ) ;
#47352 = EDGE_CURVE ( 'NONE', #9783, #740, #38978, .T. ) ;
#47353 = EDGE_LOOP ( 'NONE', ( #47234, #27238, #37787, #43809 ) ) ;
#47354 = CARTESIAN_POINT ( 'NONE',  ( -0.07405724077823318263, -1.784448818843874962, -0.1787899950787401604 ) ) ;
#47355 = CARTESIAN_POINT ( 'NONE',  ( -0.8759842519685039353, 0.1787899950787401882, 1.139271653489543290 ) ) ;
#47356 = ORIENTED_EDGE ( 'NONE', *, *, #1300, .T. ) ;
#47357 = CARTESIAN_POINT ( 'NONE',  ( -1.054774247047244096, 0.000000000000000000, 1.085137795221826629 ) ) ;
#47358 = EDGE_CURVE ( 'NONE', #45939, #31965, #6734, .T. ) ;
#47359 = VECTOR ( 'NONE', #9957, 39.37007874015748143 ) ;
#47360 = CARTESIAN_POINT ( 'NONE',  ( -0.7495606340400177148, -0.1264236179284866091, 0.2091535432533232486 ) ) ;
#47361 = CARTESIAN_POINT ( 'NONE',  ( 1.033464566929133799, 0.000000000000000000, 1.269685039370078705 ) ) ;
#47362 = CARTESIAN_POINT ( 'NONE',  ( 0.9412147342319837628, -0.1574803149606297803, 1.646161417215307843 ) ) ;
#47363 = CARTESIAN_POINT ( 'NONE',  ( -0.07405724077823318263, -0.8898877477567983529, -0.1787899950787401604 ) ) ;
#47364 = ORIENTED_EDGE ( 'NONE', *, *, #3268, .T. ) ;
#47365 = CARTESIAN_POINT ( 'NONE',  ( 3.284318927891251994E-17, 0.1274606299750234428, 0.1787899950787401882 ) ) ;
#47366 = AXIS2_PLACEMENT_3D ( 'NONE', #15152, #18489, #724 ) ;
#47367 = ORIENTED_EDGE ( 'NONE', *, *, #30541, .F. ) ;
#47368 = CARTESIAN_POINT ( 'NONE',  ( 1.002407869896990045, 0.1264236179284866091, 1.011318897584031484 ) ) ;
#47369 = LINE ( 'NONE', #39671, #23415 ) ;
#47370 = AXIS2_PLACEMENT_3D ( 'NONE', #882, #34232, #23664 ) ;
#47371 = CARTESIAN_POINT ( 'NONE',  ( -1.054774247047244096, 0.000000000000000000, 0.7308070865604093802 ) ) ;
#47372 = CARTESIAN_POINT ( 'NONE',  ( -0.8759842519685039353, 0.1787899950787401882, 1.769192913332062966 ) ) ;
#47373 = CARTESIAN_POINT ( 'NONE',  ( -0.9500414927467377701, 0.1787899950787401604, 0.1131889763241892000 ) ) ;
#47374 = CARTESIAN_POINT ( 'NONE',  ( 0.7185039370078746268, 0.06523048226347956391, 0.6569881889763781180 ) ) ;
#47375 = CARTESIAN_POINT ( 'NONE',  ( 3.301370929368692659E-17, -0.8966973528901319712, 0.1797182628040039365 ) ) ;
#47376 = CYLINDRICAL_SURFACE ( 'NONE', #45446, 0.1574803149606299191 ) ;
#47377 = CARTESIAN_POINT ( 'NONE',  ( -0.7646288533564489232, 0.1113553986120547346, 1.432086614065700925 ) ) ;
#47378 = CARTESIAN_POINT ( 'NONE',  ( 0.9500414927467378812, -0.1787899950787401604, 0.7677165353793073965 ) ) ;
#47379 = CARTESIAN_POINT ( 'NONE',  ( 0.9500414927467377701, 0.1787899950787401604, 1.368110236166710125 ) ) ;
#47380 = CARTESIAN_POINT ( 'NONE',  ( -0.1113553986120547346, -0.6230314960629921295, -0.1113553986120547346 ) ) ;
#47381 = FACE_OUTER_BOUND ( 'NONE', #46394, .T. ) ;
#47382 = CARTESIAN_POINT ( 'NONE',  ( -0.2559055118110236116, 0.05914120415906069794, -0.04157189868441935748 ) ) ;
#47383 = CARTESIAN_POINT ( 'NONE',  ( 0.7185039370078746268, -0.06523048226347956391, 1.449311023622047445 ) ) ;
#47385 = CARTESIAN_POINT ( 'NONE',  ( 1.033464566929134687, -0.06523048226347956391, 1.572342519577513142 ) ) ;
#47384 = CARTESIAN_POINT ( 'NONE',  ( 0.9537752801991592477, -0.1590467385219253571, 1.989622353916787878 ) ) ;
#47386 = CARTESIAN_POINT ( 'NONE',  ( 0.9873396505805591694, -0.1113553986120547346, 1.727362204616881947 ) ) ;
#47388 = DIRECTION ( 'NONE',  ( 0.000000000000000000, -0.2432573283306645462, 0.9699617890481188054 ) ) ;
#47387 = CARTESIAN_POINT ( 'NONE',  ( 0.8759842519685039353, -0.1787899950787401882, 0.7209645668753701386 ) ) ;
#47389 = VECTOR ( 'NONE', #34607, 39.37007874015748143 ) ;
#47390 = CARTESIAN_POINT ( 'NONE',  ( 0.1787899950787401882, -0.6894685038832439883, -2.189545951927503898E-17 ) ) ;
#47391 = DIRECTION ( 'NONE',  ( 5.934354299241488461E-32, 1.000000000000000000, 8.673617379884034486E-16 ) ) ;
#47392 = CARTESIAN_POINT ( 'NONE',  ( 1.033464566929134687, -0.06523048226347956391, 0.6274606298137325178 ) ) ;
#47393 = FACE_OUTER_BOUND ( 'NONE', #28931, .T. ) ;
#47394 = CARTESIAN_POINT ( 'NONE',  ( 1.054774247047244540, 0.07405724077823318263, 1.048228346402928723 ) ) ;
#47395 = EDGE_CURVE ( 'NONE', #1767, #32266, #43146, .T. ) ;
#47396 = DIRECTION ( 'NONE',  ( 0.000000000000000000, -1.000000000000000000, 0.000000000000000000 ) ) ;
#47397 = CARTESIAN_POINT ( 'NONE',  ( -0.1574803149606300301, -1.526082677165353951, -0.06523048226347956391 ) ) ;
#47398 = CARTESIAN_POINT ( 'NONE',  ( 0.7185039370078746268, 0.06523048226347956391, 1.247539370078740273 ) ) ;
#47399 = ( BOUNDED_CURVE ( )  B_SPLINE_CURVE ( 2, ( #33614, #25476, #40515, #18954, #728, #11322, #40745, #3876, #25711 ),
 .UNSPECIFIED., .F., .T. ) 
 B_SPLINE_CURVE_WITH_KNOTS ( ( 3, 2, 2, 2, 3 ),
 ( 0.9300000000000000488, 0.9324999999999999956, 0.9350000000000000533, 0.9375000000000000000, 0.9399999999999999467 ),
 .UNSPECIFIED. ) 
 CURVE ( )  GEOMETRIC_REPRESENTATION_ITEM ( )  RATIONAL_B_SPLINE_CURVE ( ( 1.000000000000000000, 0.9238795325112899581, 1.000000000000000000, 0.9238795325112869605, 1.000000000000000000, 0.9238795325112869605, 1.000000000000000000, 0.9238795325112829637, 1.000000000000000000 ) ) 
 REPRESENTATION_ITEM ( '' )  ) ;
#47400 = CARTESIAN_POINT ( 'NONE',  ( -0.8759842519685039353, -0.1787899950787401882, 0.05167322829269314910 ) ) ;
#47401 = AXIS2_PLACEMENT_3D ( 'NONE', #20388, #6004, #20624 ) ;
#47402 = EDGE_CURVE ( 'NONE', #17877, #10554, #4742, .T. ) ;
#47403 = VERTEX_POINT ( 'NONE', #9647 ) ;
#47404 = CARTESIAN_POINT ( 'NONE',  ( -0.1574803149606299191, -0.3326771652468035745, 0.000000000000000000 ) ) ;
#47405 = CARTESIAN_POINT ( 'NONE',  ( -0.8019270111902716547, -0.1787899950787401604, 1.943897637741510254 ) ) ;
#47406 = CARTESIAN_POINT ( 'NONE',  ( -0.8759842519685039353, -0.1787899950787401882, 1.744586614119464807 ) ) ;
#47407 = CARTESIAN_POINT ( 'NONE',  ( -0.7495606340400177148, 0.1264236179284866091, 0.4355314960092284138 ) ) ;
#47408 = CARTESIAN_POINT ( 'NONE',  ( -0.8759842519685039353, -0.1574803149606299191, 1.801181102254677091 ) ) ;
#47409 = CARTESIAN_POINT ( 'NONE',  ( 0.8070866141732283561, -0.3937007874015746034, -0.6590551181102368705 ) ) ;
#47410 = CARTESIAN_POINT ( 'NONE',  ( 0.8019270111902717657, 0.1787899950787401604, 0.03444881884387430981 ) ) ;
#47411 = CARTESIAN_POINT ( 'NONE',  ( -0.3100393700787401619, -2.714815113292586694E-26, -0.7086614173228351632 ) ) ;
#47412 = CARTESIAN_POINT ( 'NONE',  ( -0.1787899950787401882, -0.4100649131111284151, 0.000000000000000000 ) ) ;
#47413 = CARTESIAN_POINT ( 'NONE',  ( -0.1399992916321618208, -0.09842519685039370636, 0.09114338793869390665 ) ) ;
#47414 = FACE_OUTER_BOUND ( 'NONE', #30406, .T. ) ;
#47415 = DIRECTION ( 'NONE',  ( 0.000000000000000000, 1.000000000000000000, 0.000000000000000000 ) ) ;
#47416 = ( BOUNDED_CURVE ( )  B_SPLINE_CURVE ( 2, ( #22714, #4471, #30419, #11466, #11954 ),
 .UNSPECIFIED., .F., .T. ) 
 B_SPLINE_CURVE_WITH_KNOTS ( ( 3, 2, 3 ),
 ( 0.9799999999999999822, 0.9825000000000000400, 0.9850000000591240257 ),
 .UNSPECIFIED. ) 
 CURVE ( )  GEOMETRIC_REPRESENTATION_ITEM ( )  RATIONAL_B_SPLINE_CURVE ( ( 1.000000000000000000, 0.9238795325112869605, 1.000000000000000000, 0.9238795325112869605, 1.000000000000000000 ) ) 
 REPRESENTATION_ITEM ( '' )  ) ;
#47417 = CARTESIAN_POINT ( 'NONE',  ( -0.8759842519685039353, -0.1787899950787401882, 0.3272637794737956463 ) ) ;
#47418 = CARTESIAN_POINT ( 'NONE',  ( -0.7108038343253642033, 0.06841996760810098444, 0.03937007874015843040 ) ) ;
#47419 = AXIS2_PLACEMENT_3D ( 'NONE', #25173, #3827, #40237 ) ;
#47420 = CARTESIAN_POINT ( 'NONE',  ( 0.7185039370078746268, -0.06523048226347956391, 1.606791338582677309 ) ) ;
#47421 = ORIENTED_EDGE ( 'NONE', *, *, #16063, .T. ) ;
#47422 = ( BOUNDED_CURVE ( )  B_SPLINE_CURVE ( 2, ( #22683, #25594, #22440, #44006, #15269 ),
 .UNSPECIFIED., .F., .F. ) 
 B_SPLINE_CURVE_WITH_KNOTS ( ( 3, 2, 3 ),
 ( 0.01000000005912435840, 0.01250000000000000069, 0.01499999999999999944 ),
 .UNSPECIFIED. ) 
 CURVE ( )  GEOMETRIC_REPRESENTATION_ITEM ( )  RATIONAL_B_SPLINE_CURVE ( ( 1.000000000000000000, 0.9238795325112869605, 1.000000000000000000, 0.9238795325112869605, 1.000000000000000000 ) ) 
 REPRESENTATION_ITEM ( '' )  ) ;
#47423 = CARTESIAN_POINT ( 'NONE',  ( -1.002407869896990045, 0.1264236179284866091, 1.370570866087968520 ) ) ;
#47424 = ORIENTED_EDGE ( 'NONE', *, *, #26869, .T. ) ;
#47425 = CARTESIAN_POINT ( 'NONE',  ( -0.07405724077823318263, -1.233267716481668774, -0.1787899950787401604 ) ) ;
#47426 = AXIS2_PLACEMENT_3D ( 'NONE', #19454, #41005, #45075 ) ;
#47427 = CARTESIAN_POINT ( 'NONE',  ( 0.07405724077823318263, -1.430118110182456714, -0.1787899950787401604 ) ) ;
#47428 = CARTESIAN_POINT ( 'NONE',  ( 0.000000000000000000, -0.09842519685039370636, 0.000000000000000000 ) ) ;
#47429 = DIRECTION ( 'NONE',  ( 7.000000000000000150E-15, -4.999999999999999994E-15, 1.000000000000000000 ) ) ;
#47430 = CARTESIAN_POINT ( 'NONE',  ( 0.9873396505805591694, -0.1113553986120547346, 0.3198818897637795700 ) ) ;
#47431 = CARTESIAN_POINT ( 'NONE',  ( 0.4620708661417324281, 7.036468458233680972E-30, 1.186023622047243986 ) ) ;
#47432 = CARTESIAN_POINT ( 'NONE',  ( -0.8107537697050253289, -0.1574803149606297803, 0.9719488187901104137 ) ) ;
#47433 = AXIS2_PLACEMENT_3D ( 'NONE', #11645, #11401, #26739 ) ;
#47434 = CARTESIAN_POINT ( 'NONE',  ( 0.6971942568897637749, 2.189545951927499583E-17, 0.4798228345919055560 ) ) ;
#47435 = ( REPRESENTATION_RELATIONSHIP ('NONE','NONE', #9609, #20643 ) REPRESENTATION_RELATIONSHIP_WITH_TRANSFORMATION ( #46686 )SHAPE_REPRESENTATION_RELATIONSHIP( ) ) ;
#47436 = CARTESIAN_POINT ( 'NONE',  ( -0.1574803149606297803, -0.1432086614173227745, 0.06523048226347956391 ) ) ;
#47437 = CARTESIAN_POINT ( 'NONE',  ( 1.033464566929134687, -0.06523048226347956391, 1.808562992018457383 ) ) ;
#47438 = ORIENTED_EDGE ( 'NONE', *, *, #17864, .F. ) ;
#47439 = DIRECTION ( 'NONE',  ( 0.000000000000000000, 0.000000000000000000, -1.000000000000000000 ) ) ;
#47440 = CARTESIAN_POINT ( 'NONE',  ( 1.033464566929134687, -0.06523048226347956391, 0.8341535433070870198 ) ) ;
#47441 = DIRECTION ( 'NONE',  ( 3.469446951953614978E-15, 1.000000000000000000, -3.995705278811693553E-31 ) ) ;
#47443 = CARTESIAN_POINT ( 'NONE',  ( -1.033464566929134687, -0.06523048226347956391, 0.8341535433070870198 ) ) ;
#47442 = CARTESIAN_POINT ( 'NONE',  ( 0.8070866141732283561, 0.000000000000000000, -0.6580708661417323802 ) ) ;
#47444 = CARTESIAN_POINT ( 'NONE',  ( 1.614954907737318939E-16, 0.1564960629921311464, 0.4940944881889759444 ) ) ;
#47445 = ORIENTED_EDGE ( 'NONE', *, *, #25974, .T. ) ;
#47446 = ADVANCED_FACE ( 'NONE', ( #39559 ), #6026, .T. ) ;
#47447 = CARTESIAN_POINT ( 'NONE',  ( -0.9873396505805591694, -0.1113553986120547346, 0.6249999998924724576 ) ) ;
#47448 = CARTESIAN_POINT ( 'NONE',  ( 0.1787899950787401604, -1.636811023568283341, 0.07405724077823318263 ) ) ;
#47449 = CARTESIAN_POINT ( 'NONE',  ( -0.1574803149606297803, -1.590059055010582645, 0.06523048226347956391 ) ) ;
#47450 = CARTESIAN_POINT ( 'NONE',  ( 0.07405724077823318263, -0.7657480314423001921, -0.1787899950787401604 ) ) ;
#47451 = CARTESIAN_POINT ( 'NONE',  ( -1.033464566929134687, 0.06523048226347956391, 0.1205708660342053040 ) ) ;
#47452 = CARTESIAN_POINT ( 'NONE',  ( -0.06523048226347956391, -0.9798228346456692162, -0.1574803149606300301 ) ) ;
#47453 = CARTESIAN_POINT ( 'NONE',  ( 0.8759842519685039353, -0.1574803149606299191, 0.8956692912310552090 ) ) ;
#47454 = EDGE_CURVE ( 'NONE', #2356, #47099, #34115, .T. ) ;
#47455 = DIRECTION ( 'NONE',  ( 0.000000000000000000, -0.2432573283306645462, 0.9699617890481188054 ) ) ;
#47456 = VECTOR ( 'NONE', #36148, 39.37007874015748143 ) ;
#47457 = CARTESIAN_POINT ( 'NONE',  ( -1.054774247047244540, 0.07405724077823318263, 0.3789370078202520253 ) ) ;
#47458 = VERTEX_POINT ( 'NONE', #20416 ) ;
#47459 = CARTESIAN_POINT ( 'NONE',  ( -1.002407869896990045, -0.1264236179284866091, 1.675688976324189117 ) ) ;
#47460 = ORIENTED_EDGE ( 'NONE', *, *, #23617, .F. ) ;
#47461 = NEXT_ASSEMBLY_USAGE_OCCURRENCE ( 'Base Plate:1', ' ', ' ', #23955, #36823, $ ) ;
#47462 = NEXT_ASSEMBLY_USAGE_OCCURRENCE ( 'Catch Plate:1', ' ', ' ', #23955, #6332, $ ) ;
#47463 = NEXT_ASSEMBLY_USAGE_OCCURRENCE ( 'Hook Bracket:1', ' ', ' ', #23955, #6390, $ ) ;
#47464 = NEXT_ASSEMBLY_USAGE_OCCURRENCE ( 'Side Bracket:1', ' ', ' ', #23955, #11944, $ ) ;
#47465 = NEXT_ASSEMBLY_USAGE_OCCURRENCE ( 'Side Bracket:1', ' ', ' ', #23955, #14855, $ ) ;
#47466 = NEXT_ASSEMBLY_USAGE_OCCURRENCE ( 'Handle Arm Left:1', ' ', ' ', #23955, #754, $ ) ;
#47467 = NEXT_ASSEMBLY_USAGE_OCCURRENCE ( 'Handle Arm Right:1', ' ', ' ', #23955, #20410, $ ) ;
#47468 = NEXT_ASSEMBLY_USAGE_OCCURRENCE ( 'Pivot Pin:1', ' ', ' ', #23955, #18369, $ ) ;
#47469 = NEXT_ASSEMBLY_USAGE_OCCURRENCE ( 'Link Bar:1', ' ', ' ', #23955, #7809, $ ) ;
#47470 = NEXT_ASSEMBLY_USAGE_OCCURRENCE ( 'Pivot Shaft:1', ' ', ' ', #23955, #33920, $ ) ;
#47471 = NEXT_ASSEMBLY_USAGE_OCCURRENCE ( 'U-Bolt:1', ' ', ' ', #23955, #45336, $ ) ;
#47472 = NEXT_ASSEMBLY_USAGE_OCCURRENCE ( 'ISO 10513 M8 Lock Nut:1', ' ', ' ', #23955, #24794, $ ) ;
#47473 = NEXT_ASSEMBLY_USAGE_OCCURRENCE ( 'ISO 10513 M8 Lock Nut:2', ' ', ' ', #23955, #24794, $ ) ;
#47474 = NEXT_ASSEMBLY_USAGE_OCCURRENCE ( 'Threaded Bushing:1', ' ', ' ', #23955, #16326, $ ) ;
#47475 = NEXT_ASSEMBLY_USAGE_OCCURRENCE ( 'Threaded Bushing:2', ' ', ' ', #23955, #16326, $ ) ;
#47476 = NEXT_ASSEMBLY_USAGE_OCCURRENCE ( 'ISO 4162 M5x10 Hex Flange Bolt:1', ' ', ' ', #23955, #1359, $ ) ;
#47477 = NEXT_ASSEMBLY_USAGE_OCCURRENCE ( 'ISO 4162 M5x10 Hex Flange Bolt:2', ' ', ' ', #23955, #1359, $ ) ;
#47478 = NEXT_ASSEMBLY_USAGE_OCCURRENCE ( 'ISO 4162 M5x10 Hex Flange Bolt:3', ' ', ' ', #23955, #1359, $ ) ;
#47479 = NEXT_ASSEMBLY_USAGE_OCCURRENCE ( 'ISO 4162 M5x10 Hex Flange Bolt:4', ' ', ' ', #23955, #1359, $ ) ;
ENDSEC;
END-ISO-10303-21;
